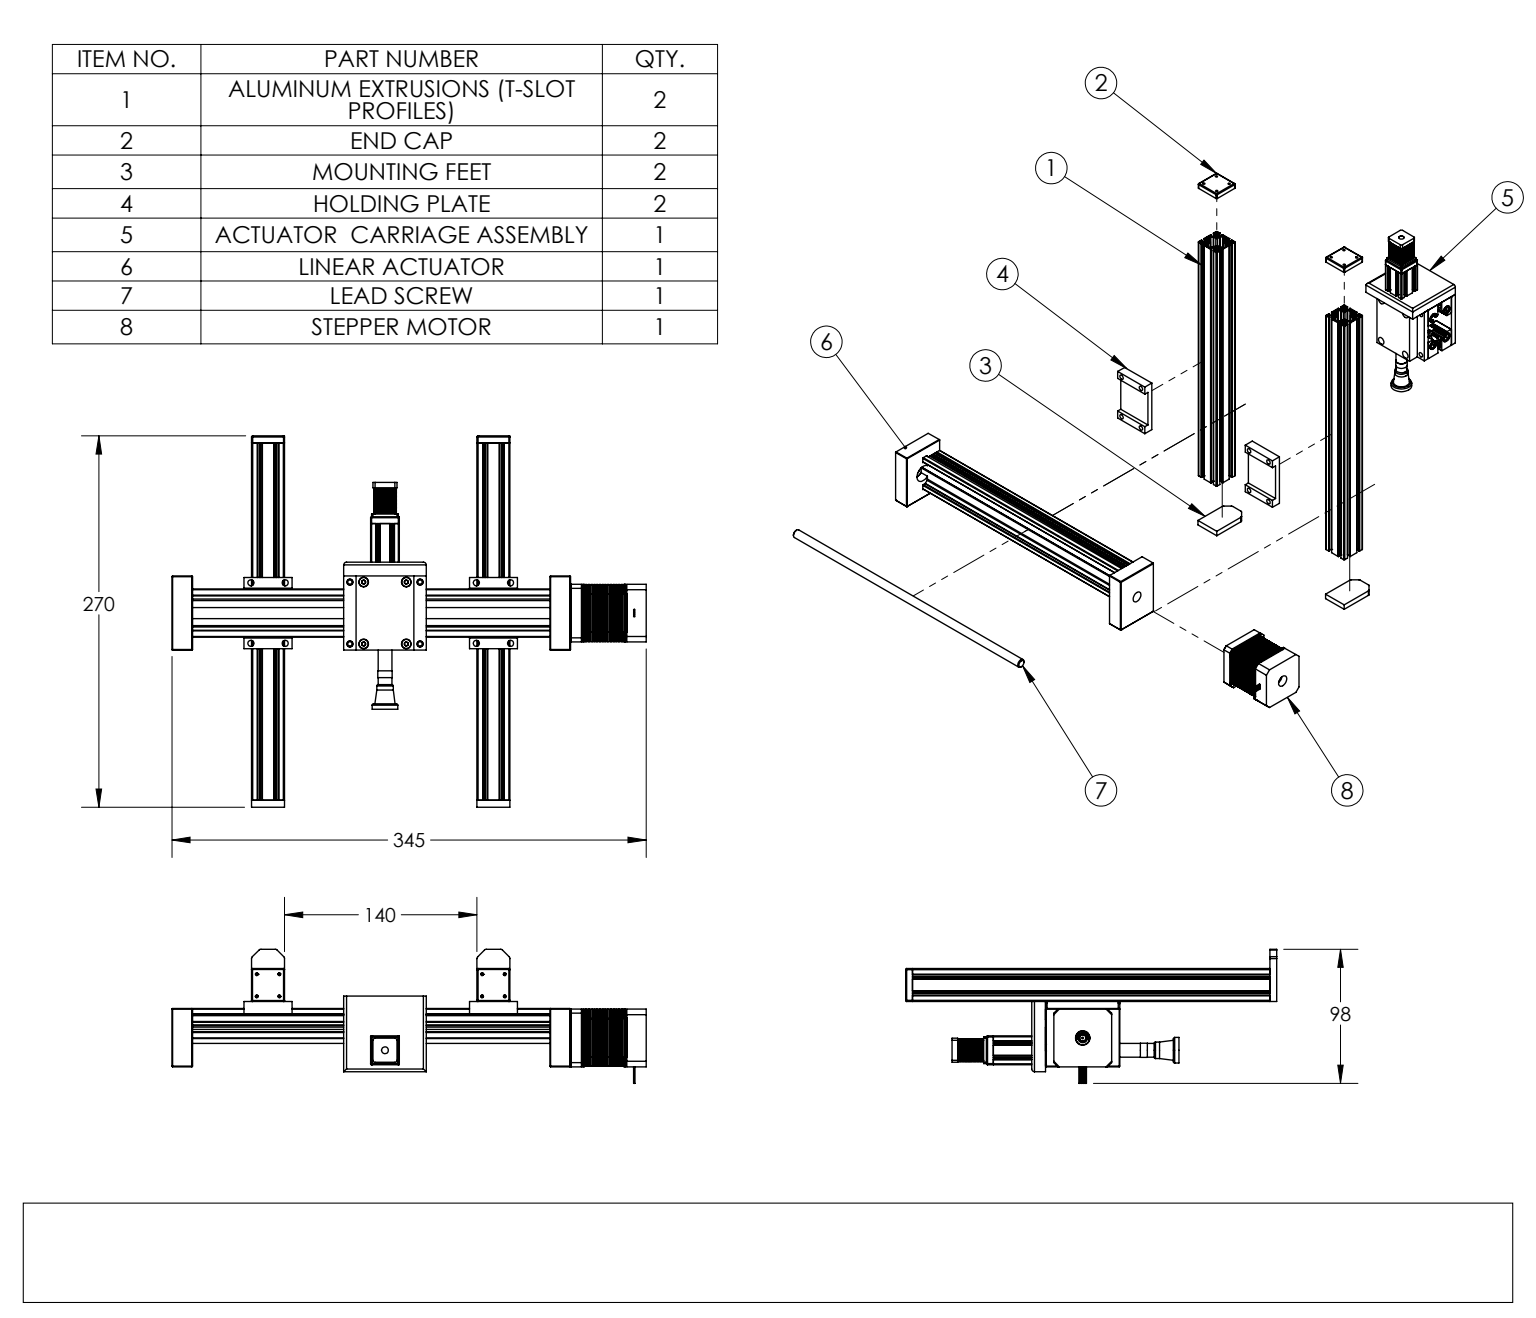
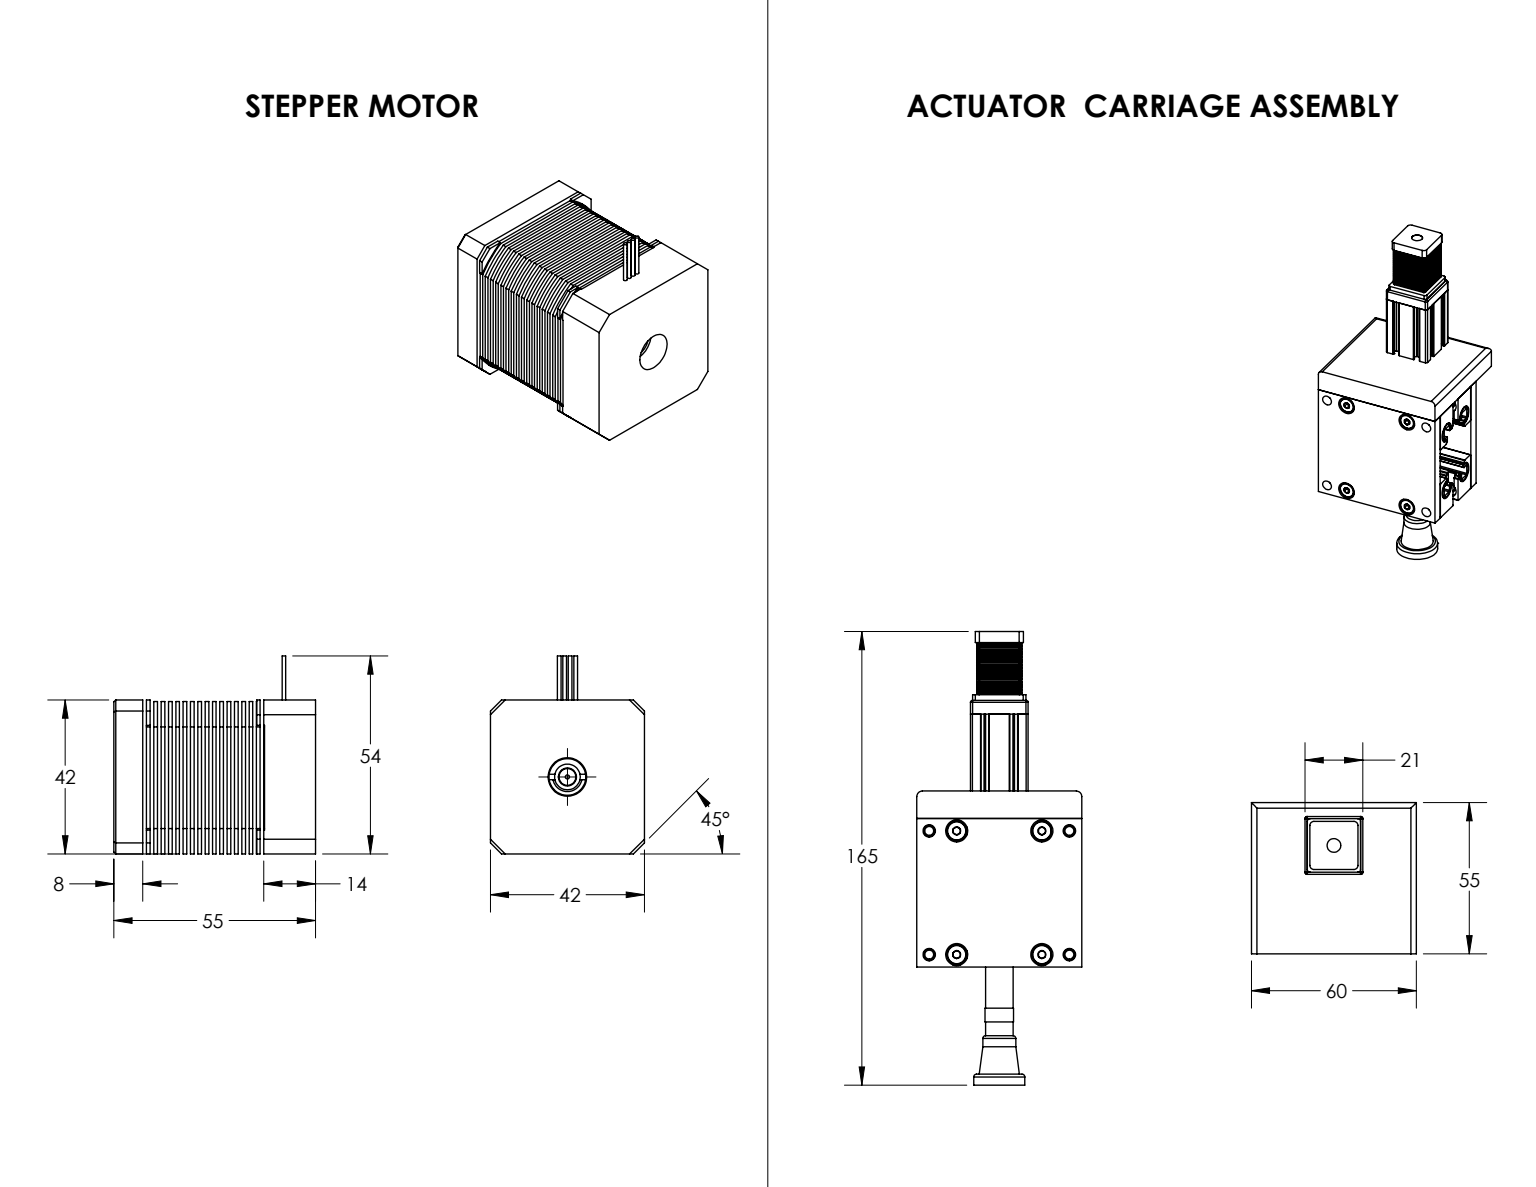
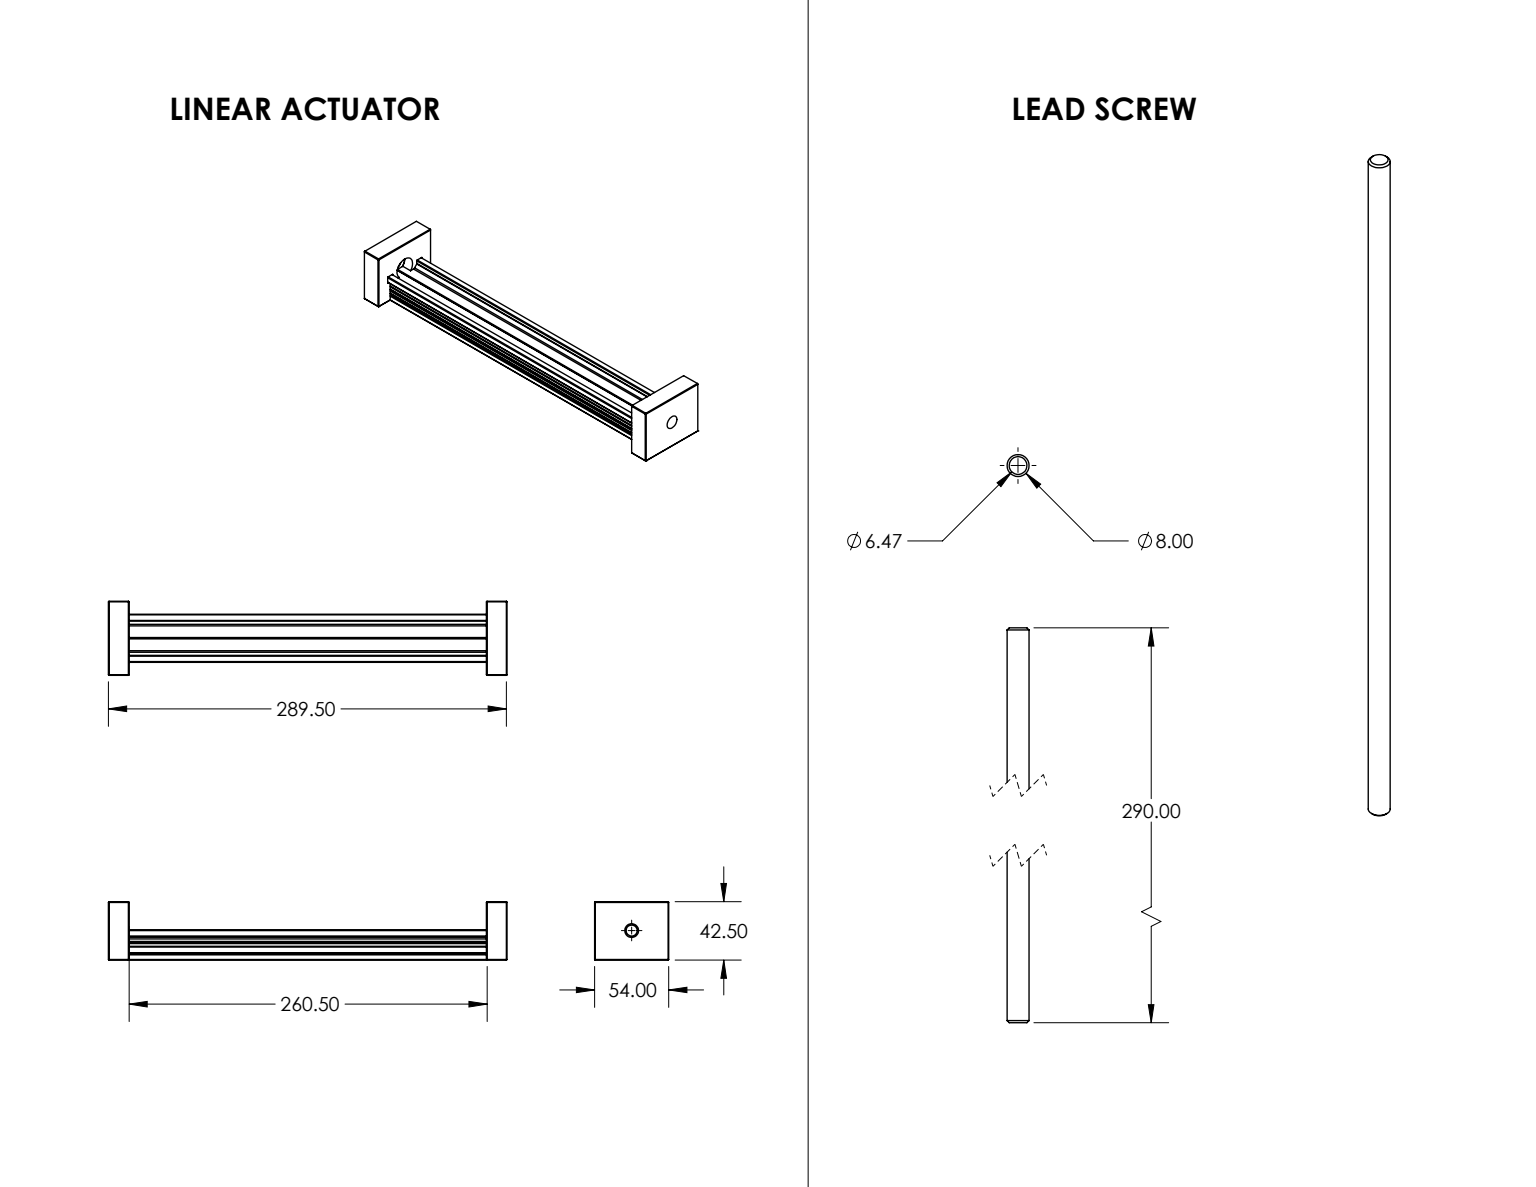
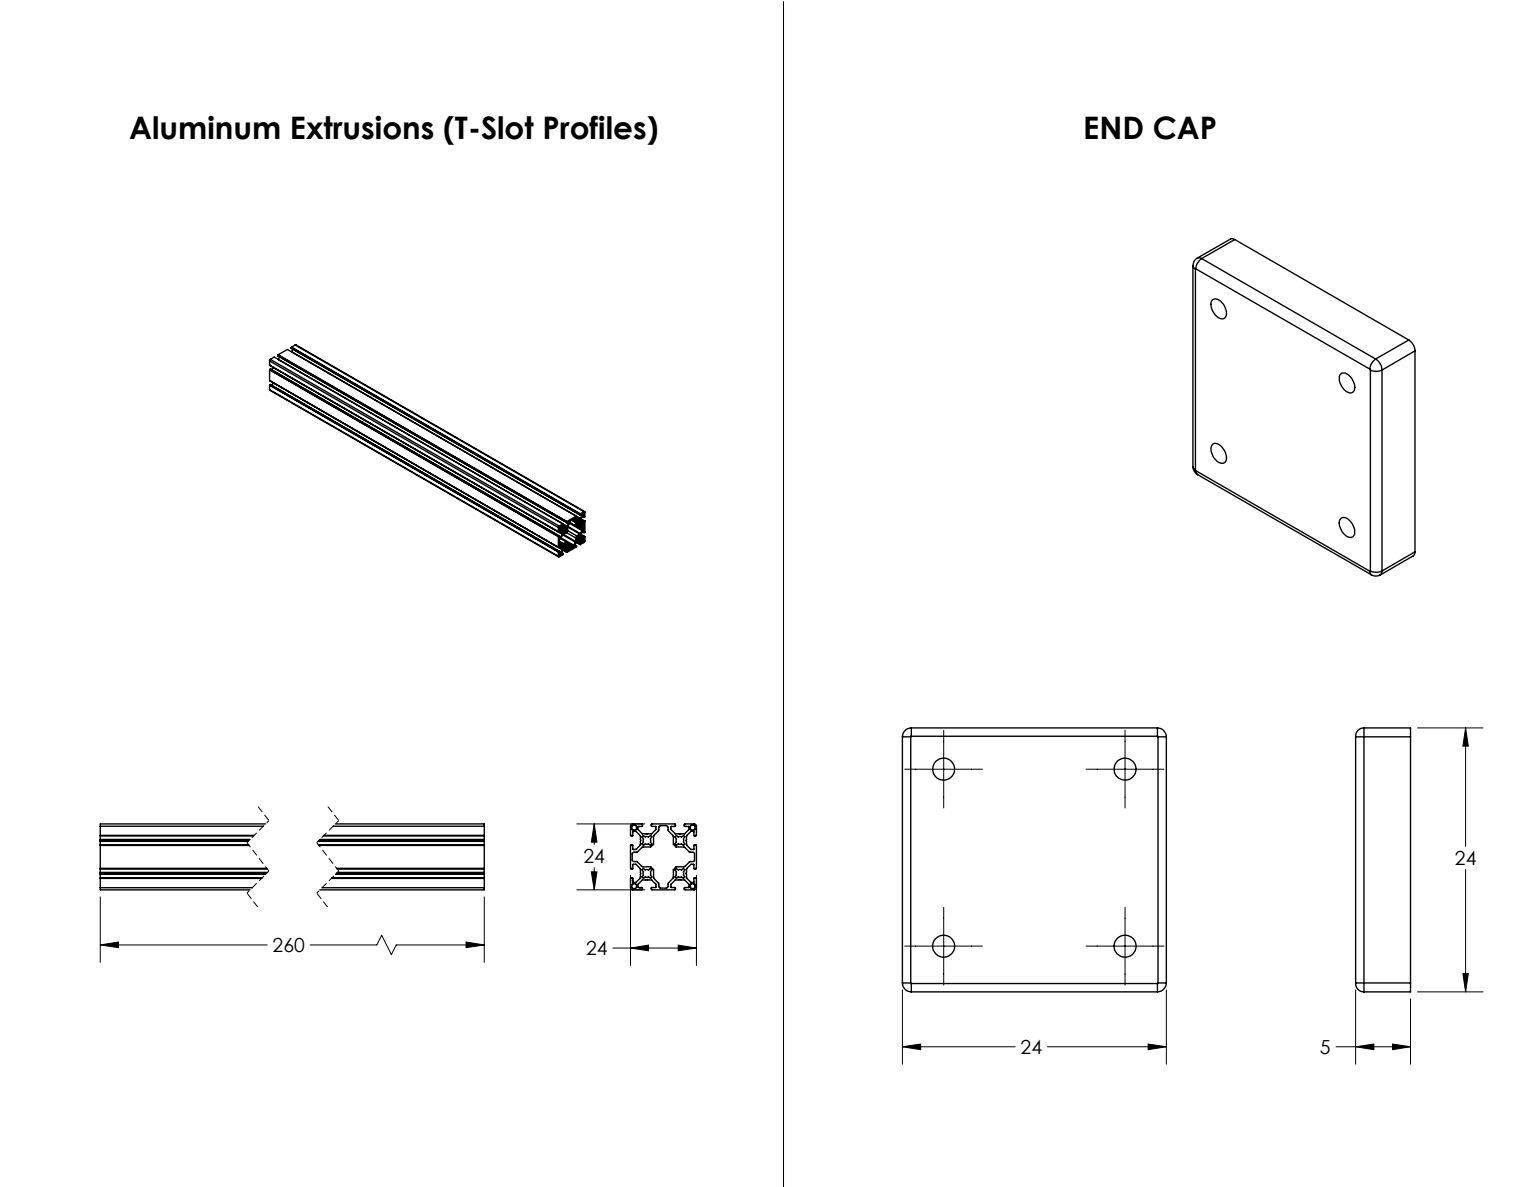
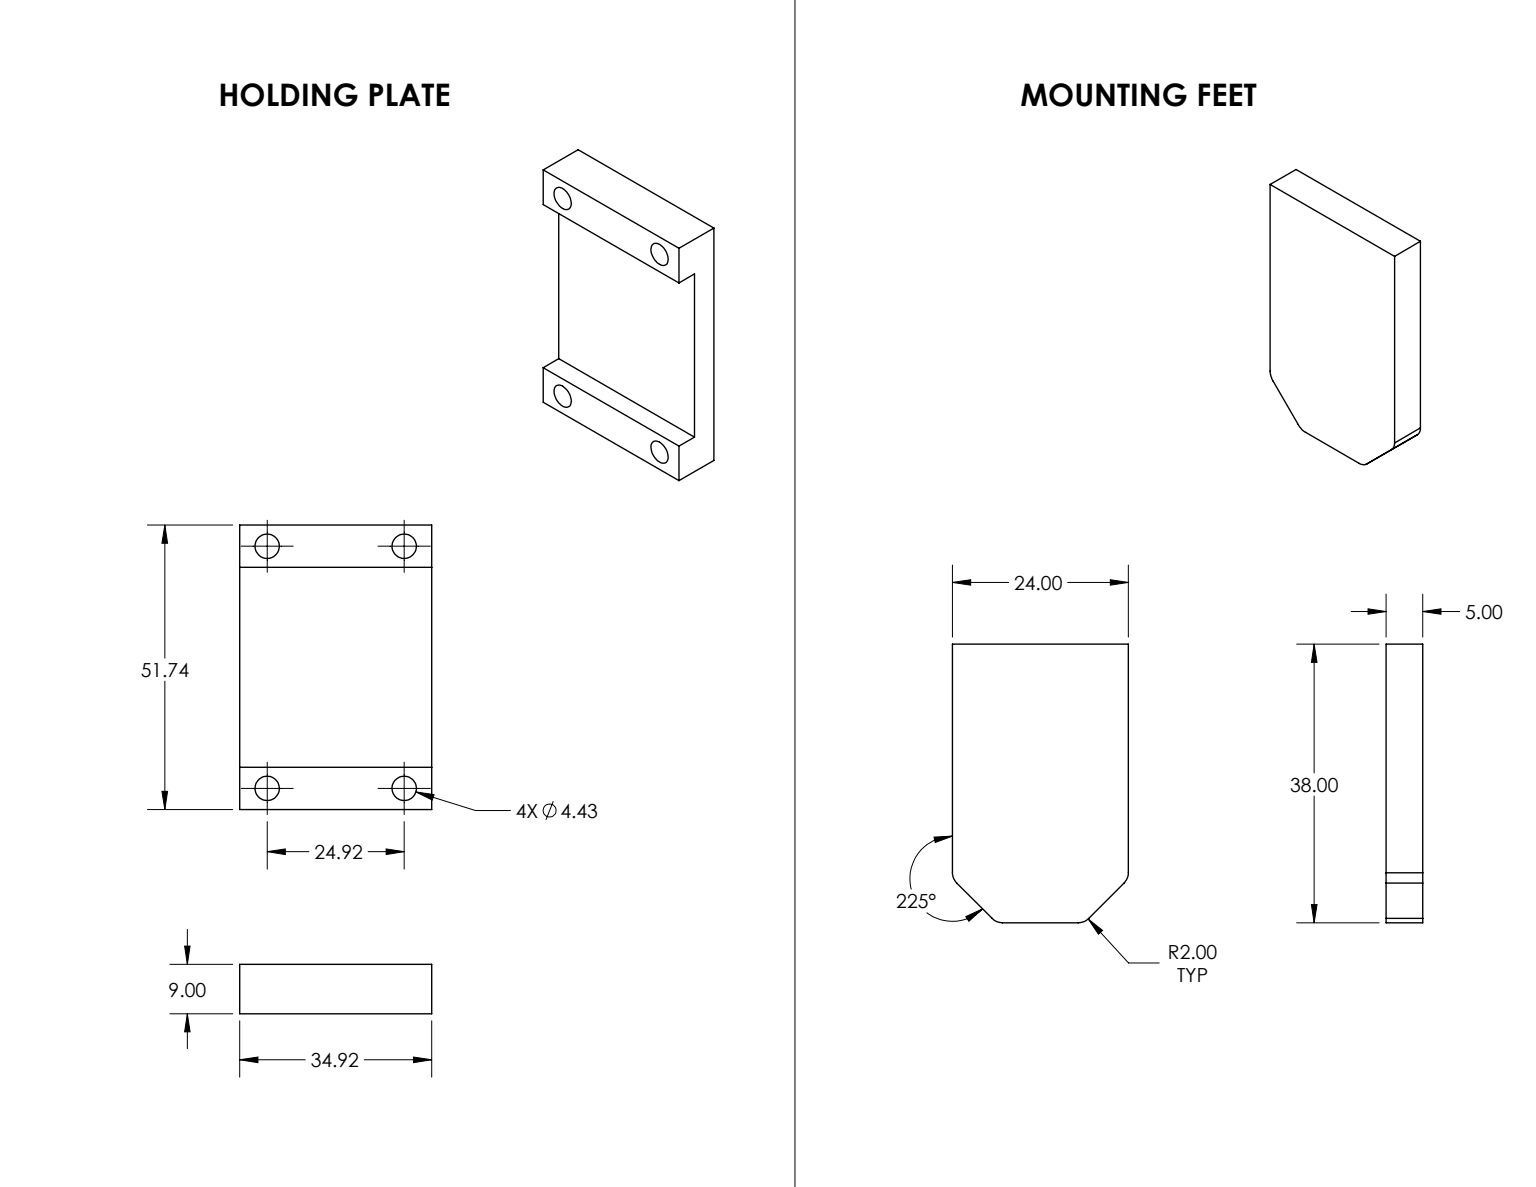
ISO-10303-21;
HEADER;
FILE_DESCRIPTION (('STEP AP214'),
    '1' );
FILE_NAME ('BR-Y-111',
    '2026-10-09T16:01:55',
    ( '' ),
    ( '' ),
    'SwSTEP 2.0',
    'SolidWorks 2024',
    '' );
FILE_SCHEMA (( 'AUTOMOTIVE_DESIGN' ));
ENDSEC;

DATA;
#1 = DIRECTION ( 'NONE',  ( 1.836970198721029934E-16, 1.836970198721010706E-16, -1.000000000000000000 ) ) ;
#3 = PLANE ( 'NONE',  #28714 ) ;
#2 = AXIS2_PLACEMENT_3D ( 'NONE', #65024, #57963, #9532 ) ;
#4 = ORIENTED_EDGE ( 'NONE', *, *, #679, .F. ) ;
#5 = CIRCLE ( 'NONE', #64414, 24.99999999998794920 ) ;
#6 = DIRECTION ( 'NONE',  ( -1.000000000000000000, 0.000000000000000000, 0.000000000000000000 ) ) ;
#8 = LINE ( 'NONE', #43125, #47900 ) ;
#7 = DIRECTION ( 'NONE',  ( 0.7071067811865422437, -0.7071067811865527908, 0.000000000000000000 ) ) ;
#9 = ORIENTED_EDGE ( 'NONE', *, *, #69803, .T. ) ;
#10 = VERTEX_POINT ( 'NONE', #4255 ) ;
#12 = VERTEX_POINT ( 'NONE', #25817 ) ;
#11 = LINE ( 'NONE', #65402, #38696 ) ;
#13 = ORIENTED_EDGE ( 'NONE', *, *, #42356, .F. ) ;
#14 = AXIS2_PLACEMENT_3D ( 'NONE', #25100, #35689, #34989 ) ;
#15 = ADVANCED_FACE ( 'NONE', ( #41711 ), #19784, .T. ) ;
#17 = AXIS2_PLACEMENT_3D ( 'NONE', #56008, #906, #7566 ) ;
#16 = FACE_OUTER_BOUND ( 'NONE', #57290, .T. ) ;
#18 = CIRCLE ( 'NONE', #40620, 8.300000000000002487 ) ;
#19 = ADVANCED_FACE ( 'NONE', ( #47367 ), #45971, .F. ) ;
#20 = CARTESIAN_POINT ( 'NONE',  ( 7.000000000000000000, -26.50000000000000000, 9.080000000000000071 ) ) ;
#21 = ORIENTED_EDGE ( 'NONE', *, *, #32727, .F. ) ;
#22 = EDGE_CURVE ( 'NONE', #35164, #51205, #22753, .T. ) ;
#23 = AXIS2_PLACEMENT_3D ( 'NONE', #22038, #43598, #28713 ) ;
#24 = VECTOR ( 'NONE', #20692, 1000.000000000000000 ) ;
#25 = FACE_OUTER_BOUND ( 'NONE', #67171, .T. ) ;
#26 = EDGE_CURVE ( 'NONE', #33489, #6963, #35337, .T. ) ;
#27 = DIRECTION ( 'NONE',  ( -1.000000000000000000, 1.794541526872559352E-16, 0.000000000000000000 ) ) ;
#28 = VERTEX_POINT ( 'NONE', #47018 ) ;
#29 = ORIENTED_EDGE ( 'NONE', *, *, #35649, .T. ) ;
#30 = PLANE ( 'NONE',  #1467 ) ;
#31 = LINE ( 'NONE', #62705, #60565 ) ;
#32 = ADVANCED_FACE ( 'NONE', ( #68598 ), #51631, .F. ) ;
#33 = CARTESIAN_POINT ( 'NONE',  ( 32.89999999999999858, -21.00000000000001421, -13.86939075806900945 ) ) ;
#34 = ORIENTED_EDGE ( 'NONE', *, *, #62391, .F. ) ;
#35 = SHAPE_REPRESENTATION ( 'Aluminum Extrusions (T-Slot Profiles)_5537T808', ( #45918 ), #47199 ) ;
#36 = CARTESIAN_POINT ( 'NONE',  ( -11.99351654964679526, -7.826483450353362237, 455.0000000000000568 ) ) ;
#37 = FACE_OUTER_BOUND ( 'NONE', #4535, .T. ) ;
#39 = ORIENTED_EDGE ( 'NONE', *, *, #40166, .F. ) ;
#38 = CARTESIAN_POINT ( 'NONE',  ( 4.201500623656003519, -4.740315990920191069, 195.0000000000000284 ) ) ;
#41 = ORIENTED_EDGE ( 'NONE', *, *, #17643, .F. ) ;
#40 = CARTESIAN_POINT ( 'NONE',  ( -12.00000000000000000, -11.18999999999999950, -4.250000000000000000 ) ) ;
#42 = EDGE_CURVE ( 'NONE', #51075, #15946, #66798, .T. ) ;
#43 = FACE_OUTER_BOUND ( 'NONE', #36731, .T. ) ;
#44 = DIRECTION ( 'NONE',  ( -1.000000000000000000, 0.000000000000000000, 0.000000000000000000 ) ) ;
#45 = CARTESIAN_POINT ( 'NONE',  ( 6.006483450353353959, 5.993516549646629166, 195.0000000000000284 ) ) ;
#46 = LINE ( 'NONE', #38894, #69673 ) ;
#47 = ADVANCED_FACE ( 'NONE', ( #64337 ), #37812, .F. ) ;
#48 = CARTESIAN_POINT ( 'NONE',  ( 11.08848345035334404, -11.08848345035339733, 195.0000000000000284 ) ) ;
#49 = FACE_OUTER_BOUND ( 'NONE', #48947, .T. ) ;
#50 = VERTEX_POINT ( 'NONE', #59375 ) ;
#51 = DIRECTION ( 'NONE',  ( 1.000000000000000000, 0.000000000000000000, 0.000000000000000000 ) ) ;
#52 = VECTOR ( 'NONE', #54469, 1000.000000000000000 ) ;
#54 = ORIENTED_EDGE ( 'NONE', *, *, #29068, .T. ) ;
#53 = DIRECTION ( 'NONE',  ( 0.000000000000000000, -1.000000000000000000, 0.000000000000000000 ) ) ;
#56 = ORIENTED_EDGE ( 'NONE', *, *, #20714, .T. ) ;
#55 = LINE ( 'NONE', #58414, #51365 ) ;
#57 = CIRCLE ( 'NONE', #62089, 0.3999999999999993006 ) ;
#58 = DIRECTION ( 'NONE',  ( 0.000000000000000000, 0.7096009616570518874, -0.7046037717862339012 ) ) ;
#59 = DIRECTION ( 'NONE',  ( -0.000000000000000000, -0.000000000000000000, -1.000000000000000000 ) ) ;
#60 = VECTOR ( 'NONE', #58581, 1000.000000000000000 ) ;
#61 = ORIENTED_EDGE ( 'NONE', *, *, #49040, .T. ) ;
#62 = CARTESIAN_POINT ( 'NONE',  ( 30.00000000000000000, -14.04000000000000092, 17.04524521594300523 ) ) ;
#63 = CARTESIAN_POINT ( 'NONE',  ( -7.605476262117258024, 9.722976262117178692, 54.00000000000000711 ) ) ;
#64 = VERTEX_POINT ( 'NONE', #42415 ) ;
#65 = VECTOR ( 'NONE', #47625, 1000.000000000000114 ) ;
#66 = DIRECTION ( 'NONE',  ( -1.000000000000000000, 0.000000000000000000, 0.000000000000000000 ) ) ;
#67 = DIRECTION ( 'NONE',  ( 2.478176394252584099E-15, 1.000000000000000000, 0.000000000000000000 ) ) ;
#68 =( LENGTH_UNIT ( ) NAMED_UNIT ( * ) SI_UNIT ( .MILLI., .METRE. ) );
#69 = AXIS2_PLACEMENT_3D ( 'NONE', #9677, #37599, #64471 ) ;
#70 = EDGE_CURVE ( 'NONE', #46124, #11076, #48766, .T. ) ;
#71 = ADVANCED_FACE ( 'NONE', ( #55074 ), #31476, .T. ) ;
#72 = ORIENTED_EDGE ( 'NONE', *, *, #39303, .F. ) ;
#73 = DIRECTION ( 'NONE',  ( 0.000000000000000000, 0.000000000000000000, 1.000000000000000000 ) ) ;
#74 = ORIENTED_EDGE ( 'NONE', *, *, #13941, .F. ) ;
#75 = ORIENTED_EDGE ( 'NONE', *, *, #18728, .F. ) ;
#76 = CARTESIAN_POINT ( 'NONE',  ( 11.00000000000000000, -17.14999999999900027, 26.64999999999900027 ) ) ;
#77 = AXIS2_PLACEMENT_3D ( 'NONE', #40976, #13759, #8096 ) ;
#78 = CARTESIAN_POINT ( 'NONE',  ( 11.48848345035341900, 10.19191654964656202, 455.0000000000000568 ) ) ;
#79 = VECTOR ( 'NONE', #901, 1000.000000000000000 ) ;
#80 = PLANE ( 'NONE',  #21958 ) ;
#81 = PLANE ( 'NONE',  #14890 ) ;
#82 = EDGE_LOOP ( 'NONE', ( #52627, #35376, #11266, #26532 ) ) ;
#83 = ORIENTED_EDGE ( 'NONE', *, *, #7597, .F. ) ;
#85 = ORIENTED_EDGE ( 'NONE', *, *, #57080, .T. ) ;
#84 = CARTESIAN_POINT ( 'NONE',  ( 30.00000000000000000, -5.599999999999999645, -9.400000000000000355 ) ) ;
#86 = VERTEX_POINT ( 'NONE', #37468 ) ;
#87 = DIRECTION ( 'NONE',  ( 0.000000000000000000, -3.673940397442059868E-16, 1.000000000000000000 ) ) ;
#88 = PLANE ( 'NONE',  #65914 ) ;
#89 = CARTESIAN_POINT ( 'NONE',  ( 6.006483450353353959, 5.993516549646629166, 195.0000000000000284 ) ) ;
#90 = LINE ( 'NONE', #39288, #28849 ) ;
#92 = FACE_OUTER_BOUND ( 'NONE', #31226, .T. ) ;
#91 = DIRECTION ( 'NONE',  ( 0.000000000000000000, -0.9938079899998859545, 0.1111111111112941946 ) ) ;
#93 = ORIENTED_EDGE ( 'NONE', *, *, #1630, .F. ) ;
#95 = ORIENTED_EDGE ( 'NONE', *, *, #37069, .T. ) ;
#94 = LINE ( 'NONE', #53844, #47687 ) ;
#96 = VERTEX_POINT ( 'NONE', #36776 ) ;
#97 = VERTEX_POINT ( 'NONE', #64001 ) ;
#98 = CARTESIAN_POINT ( 'NONE',  ( 275.0000000000000000, -0.5000000000000000000, -26.50000000000000000 ) ) ;
#99 = LINE ( 'NONE', #17046, #62617 ) ;
#100 = AXIS2_PLACEMENT_3D ( 'NONE', #13229, #2981, #46110 ) ;
#101 = DIRECTION ( 'NONE',  ( 1.000000000000000000, 0.000000000000000000, 0.000000000000000000 ) ) ;
#102 = EDGE_CURVE ( 'NONE', #33046, #57965, #58906, .T. ) ;
#103 = CARTESIAN_POINT ( 'NONE',  ( 0.000000000000000000, -8.249999999999998224, -13.50000000000000178 ) ) ;
#104 = EDGE_LOOP ( 'NONE', ( #32156, #26137, #19889, #8846 ) ) ;
#105 = ORIENTED_EDGE ( 'NONE', *, *, #55339, .T. ) ;
#106 = ORIENTED_EDGE ( 'NONE', *, *, #31966, .F. ) ;
#108 = ADVANCED_FACE ( 'NONE', ( #69649 ), #9907, .T. ) ;
#107 = VECTOR ( 'NONE', #53809, 1000.000000000000000 ) ;
#109 = CARTESIAN_POINT ( 'NONE',  ( 11.00000000000000000, -17.00000000000000000, 15.70499999999969809 ) ) ;
#110 = CARTESIAN_POINT ( 'NONE',  ( 14.89999999999999680, 13.66939075806899240, -20.79999999999999361 ) ) ;
#111 = EDGE_CURVE ( 'NONE', #61998, #6695, #11268, .T. ) ;
#112 = CARTESIAN_POINT ( 'NONE',  ( 8.249999999999996447, -7.848062532927998269, 0.000000000000000000 ) ) ;
#113 = EDGE_CURVE ( 'NONE', #43177, #7725, #15895, .T. ) ;
#114 = VERTEX_POINT ( 'NONE', #53041 ) ;
#115 = CIRCLE ( 'NONE', #62160, 1.620999999999997332 ) ;
#116 = VECTOR ( 'NONE', #2061, 1000.000000000000000 ) ;
#117 = ORIENTED_EDGE ( 'NONE', *, *, #12680, .F. ) ;
#118 = DIRECTION ( 'NONE',  ( -1.836970198721029934E-16, 1.836970198721036344E-16, -1.000000000000000000 ) ) ;
#119 = ADVANCED_FACE ( 'NONE', ( #37125 ), #15567, .T. ) ;
#120 = EDGE_CURVE ( 'NONE', #5167, #67654, #58950, .T. ) ;
#121 = FACE_OUTER_BOUND ( 'NONE', #43409, .T. ) ;
#122 = VERTEX_POINT ( 'NONE', #47717 ) ;
#123 = AXIS2_PLACEMENT_3D ( 'NONE', #35895, #68773, #47212 ) ;
#124 = EDGE_CURVE ( 'NONE', #2059, #46953, #44248, .T. ) ;
#125 = CARTESIAN_POINT ( 'NONE',  ( -11.00000000000000000, -9.200000000000120082, 17.64999999999993108 ) ) ;
#127 = VERTEX_POINT ( 'NONE', #32847 ) ;
#126 = LINE ( 'NONE', #53521, #21596 ) ;
#128 = ORIENTED_EDGE ( 'NONE', *, *, #65488, .T. ) ;
#130 = CARTESIAN_POINT ( 'NONE',  ( -7.793516549646827940, -11.12648345035340647, 455.0000000000000568 ) ) ;
#129 = AXIS2_PLACEMENT_3D ( 'NONE', #11576, #55092, #50108 ) ;
#131 = DIRECTION ( 'NONE',  ( 0.8660254037844482555, 0.000000000000000000, -0.4999999999999831801 ) ) ;
#132 = DIRECTION ( 'NONE',  ( 0.000000000000000000, 0.000000000000000000, 1.000000000000000000 ) ) ;
#133 = CARTESIAN_POINT ( 'NONE',  ( 1.480523737882788238, -9.404523737882794165, 54.00000000000000711 ) ) ;
#134 = DIRECTION ( 'NONE',  ( 0.000000000000000000, 0.000000000000000000, 1.000000000000000000 ) ) ;
#135 = VERTEX_POINT ( 'NONE', #54425 ) ;
#136 = DIRECTION ( 'NONE',  ( -1.836970198721029934E-16, 1.836970198721036344E-16, -1.000000000000000000 ) ) ;
#137 = ORIENTED_EDGE ( 'NONE', *, *, #53122, .T. ) ;
#138 = DIRECTION ( 'NONE',  ( 1.000000000000000000, -0.000000000000000000, -0.000000000000000000 ) ) ;
#139 = CARTESIAN_POINT ( 'NONE',  ( 29.50000000000000355, -12.00000000000000000, 10.69999999999999929 ) ) ;
#140 = VECTOR ( 'NONE', #32792, 1000.000000000000000 ) ;
#141 = CARTESIAN_POINT ( 'NONE',  ( 275.0000000000000000, -21.00000000000000000, 12.50000000000000000 ) ) ;
#142 = DIRECTION ( 'NONE',  ( 1.836970198721029934E-16, 1.836970198721010706E-16, -1.000000000000000000 ) ) ;
#143 = DIRECTION ( 'NONE',  ( 1.047444401652939849E-14, 1.000000000000000000, 1.836970198721029934E-16 ) ) ;
#144 = VERTEX_POINT ( 'NONE', #43447 ) ;
#145 = DIRECTION ( 'NONE',  ( 1.000000000000000000, 0.000000000000000000, 0.000000000000000000 ) ) ;
#146 = CIRCLE ( 'NONE', #27251, 2.000000000000001776 ) ;
#147 = DIRECTION ( 'NONE',  ( 1.000000000000000000, 0.000000000000000000, 0.000000000000000000 ) ) ;
#148 = EDGE_CURVE ( 'NONE', #32098, #68514, #65034, .T. ) ;
#149 = VECTOR ( 'NONE', #1157, 1000.000000000000000 ) ;
#150 = EDGE_LOOP ( 'NONE', ( #65077, #13580, #38197, #52160, #31394, #37304, #41041, #48083 ) ) ;
#151 = DIRECTION ( 'NONE',  ( 1.000000000000000000, 0.000000000000000000, 0.000000000000000000 ) ) ;
#152 = CARTESIAN_POINT ( 'NONE',  ( 47.00000000000000000, 0.000000000000000000, 0.000000000000000000 ) ) ;
#153 = ADVANCED_FACE ( 'NONE', ( #5637 ), #10243, .T. ) ;
#154 = AXIS2_PLACEMENT_3D ( 'NONE', #15103, #20746, #47621 ) ;
#155 = ORIENTED_EDGE ( 'NONE', *, *, #10566, .T. ) ;
#156 = EDGE_CURVE ( 'NONE', #48024, #52249, #59027, .T. ) ;
#157 = DIRECTION ( 'NONE',  ( 1.000000000000000000, 0.000000000000000000, 0.000000000000000000 ) ) ;
#158 = CARTESIAN_POINT ( 'NONE',  ( 31.89999999999999858, -0.2000000000089119934, -8.913009219568841313E-12 ) ) ;
#159 = ORIENTED_EDGE ( 'NONE', *, *, #8792, .F. ) ;
#160 = CARTESIAN_POINT ( 'NONE',  ( 12.00648345035338060, -7.826483450353491023, 455.0000000000000568 ) ) ;
#161 = DIRECTION ( 'NONE',  ( -1.000000000000000000, 4.121462285523434458E-16, 1.514200678731842937E-31 ) ) ;
#162 = EDGE_CURVE ( 'NONE', #51028, #19307, #65708, .T. ) ;
#163 = CIRCLE ( 'NONE', #63398, 0.1999999999999987899 ) ;
#164 = VECTOR ( 'NONE', #31402, 1000.000000000000000 ) ;
#165 = LINE ( 'NONE', #32674, #35413 ) ;
#166 = CARTESIAN_POINT ( 'NONE',  ( 275.2500000000000000, -42.25000000000000000, 26.75000000000000000 ) ) ;
#167 = VERTEX_POINT ( 'NONE', #1968 ) ;
#169 = EDGE_LOOP ( 'NONE', ( #39486, #29430, #2363, #22947 ) ) ;
#168 = DIRECTION ( 'NONE',  ( 1.000000000000000000, -0.000000000000000000, 0.000000000000000000 ) ) ;
#170 = AXIS2_PLACEMENT_3D ( 'NONE', #9286, #3635, #67983 ) ;
#171 = CIRCLE ( 'NONE', #58872, 0.4999999999991850963 ) ;
#172 = DIRECTION ( 'NONE',  ( 1.356437060717831815E-15, 1.000000000000000000, 0.000000000000000000 ) ) ;
#173 = CYLINDRICAL_SURFACE ( 'NONE', #39140, 3.499999999999850342 ) ;
#174 = LINE ( 'NONE', #65556, #3686 ) ;
#175 = ORIENTED_EDGE ( 'NONE', *, *, #63248, .F. ) ;
#176 = AXIS2_PLACEMENT_3D ( 'NONE', #44626, #60208, #34021 ) ;
#177 = PLANE ( 'NONE',  #17503 ) ;
#178 = CARTESIAN_POINT ( 'NONE',  ( -7.250000000000000888, 7.250000000000001776, -18.00000000000000000 ) ) ;
#179 = ORIENTED_EDGE ( 'NONE', *, *, #39700, .T. ) ;
#180 = ORIENTED_EDGE ( 'NONE', *, *, #26893, .F. ) ;
#181 = ORIENTED_EDGE ( 'NONE', *, *, #42792, .T. ) ;
#182 = DIRECTION ( 'NONE',  ( -0.000000000000000000, 3.673940397442059868E-16, -1.000000000000000000 ) ) ;
#183 = CARTESIAN_POINT ( 'NONE',  ( 11.50000000000000000, -11.50000000000100009, -10.50000000000065903 ) ) ;
#184 =( LENGTH_UNIT ( ) NAMED_UNIT ( * ) SI_UNIT ( .MILLI., .METRE. ) );
#185 = EDGE_CURVE ( 'NONE', #36958, #12401, #20004, .T. ) ;
#186 = ORIENTED_EDGE ( 'NONE', *, *, #14388, .F. ) ;
#187 = VERTEX_POINT ( 'NONE', #23532 ) ;
#188 = ORIENTED_EDGE ( 'NONE', *, *, #41288, .T. ) ;
#189 = DIRECTION ( 'NONE',  ( -1.813998472013049506E-14, -1.000000000000000000, -1.836970198721043986E-16 ) ) ;
#190 = VERTEX_POINT ( 'NONE', #61701 ) ;
#191 = VERTEX_POINT ( 'NONE', #61342 ) ;
#192 = ORIENTED_EDGE ( 'NONE', *, *, #64535, .T. ) ;
#193 = ORIENTED_EDGE ( 'NONE', *, *, #5564, .T. ) ;
#194 = DIRECTION ( 'NONE',  ( 1.000000000000000000, 0.000000000000000000, 0.000000000000000000 ) ) ;
#195 = EDGE_CURVE ( 'NONE', #57192, #24019, #50407, .T. ) ;
#196 = EDGE_CURVE ( 'NONE', #13160, #36733, #7955, .T. ) ;
#197 = CIRCLE ( 'NONE', #57770, 2.204799999999999205 ) ;
#199 = ORIENTED_EDGE ( 'NONE', *, *, #12386, .F. ) ;
#198 = DIRECTION ( 'NONE',  ( 1.000000000000000000, 0.000000000000000000, 0.000000000000000000 ) ) ;
#200 = CARTESIAN_POINT ( 'NONE',  ( 7.000000000000000000, -42.00000000000000000, -7.000000000000000000 ) ) ;
#201 = AXIS2_PLACEMENT_3D ( 'NONE', #59073, #10628, #38219 ) ;
#202 = DIRECTION ( 'NONE',  ( -0.7071067811865480168, -0.7071067811865470176, 0.000000000000000000 ) ) ;
#203 = EDGE_CURVE ( 'NONE', #26279, #24611, #49905, .T. ) ;
#204 = CARTESIAN_POINT ( 'NONE',  ( 7.000000000000000000, -26.50000000000000000, -0.5000000000000000000 ) ) ;
#205 = ORIENTED_EDGE ( 'NONE', *, *, #6943, .T. ) ;
#206 = VECTOR ( 'NONE', #26081, 1000.000000000000000 ) ;
#207 = AXIS2_PLACEMENT_3D ( 'NONE', #51978, #16234, #48423 ) ;
#208 = DIRECTION ( 'NONE',  ( -1.000000000000000000, 3.491481338843133355E-15, 1.836970198721036344E-16 ) ) ;
#209 = CARTESIAN_POINT ( 'NONE',  ( -7.450000000000001954, 0.000000000000000000, -18.00000000000000000 ) ) ;
#210 = ORIENTED_EDGE ( 'NONE', *, *, #15362, .F. ) ;
#211 = AXIS2_PLACEMENT_3D ( 'NONE', #34304, #7442, #6750 ) ;
#212 = DIRECTION ( 'NONE',  ( 0.000000000000000000, -0.1249999999999996531, -0.9921567416492215186 ) ) ;
#213 = CARTESIAN_POINT ( 'NONE',  ( 32.89999999999999858, 20.60000000000000142, 13.86939075806900057 ) ) ;
#214 = LINE ( 'NONE', #16474, #66351 ) ;
#215 = ORIENTED_EDGE ( 'NONE', *, *, #61304, .T. ) ;
#216 = DIRECTION ( 'NONE',  ( 0.000000000000000000, -0.7071067811865474617, -0.7071067811865474617 ) ) ;
#217 = DIRECTION ( 'NONE',  ( -1.047444401652940164E-14, -1.000000000000000000, -1.836970198721030181E-16 ) ) ;
#218 = DIRECTION ( 'NONE',  ( 0.000000000000000000, 0.000000000000000000, 1.000000000000000000 ) ) ;
#219 = DIRECTION ( 'NONE',  ( 0.000000000000000000, 0.000000000000000000, -1.000000000000000000 ) ) ;
#220 = PLANE ( 'NONE',  #66350 ) ;
#221 = LINE ( 'NONE', #21784, #62152 ) ;
#222 = DIRECTION ( 'NONE',  ( -0.000000000000000000, -0.000000000000000000, -1.000000000000000000 ) ) ;
#223 = PLANE ( 'NONE',  #58243 ) ;
#224 = ORIENTED_EDGE ( 'NONE', *, *, #41153, .T. ) ;
#225 = CARTESIAN_POINT ( 'NONE',  ( -29.50000000000000355, -15.46862696659690073, 14.50000000000000000 ) ) ;
#226 = LINE ( 'NONE', #22825, #12692 ) ;
#227 = EDGE_CURVE ( 'NONE', #15964, #12532, #53311, .T. ) ;
#228 = ADVANCED_FACE ( 'NONE', ( #56750 ), #13963, .T. ) ;
#229 = EDGE_CURVE ( 'NONE', #49648, #8082, #14853, .T. ) ;
#230 = DIRECTION ( 'NONE',  ( 0.000000000000000000, 0.000000000000000000, -1.000000000000000000 ) ) ;
#231 = CARTESIAN_POINT ( 'NONE',  ( 0.000000000000000000, -42.00000000000000000, 26.50000000000000000 ) ) ;
#232 = ORIENTED_EDGE ( 'NONE', *, *, #38318, .F. ) ;
#233 = CARTESIAN_POINT ( 'NONE',  ( 30.00000000000000000, -5.599999999999999645, 9.400000000000000355 ) ) ;
#234 = DIRECTION ( 'NONE',  ( -1.000000000000000000, 0.000000000000000000, 0.000000000000000000 ) ) ;
#235 = AXIS2_PLACEMENT_3D ( 'NONE', #32460, #32097, #54031 ) ;
#236 = LINE ( 'NONE', #68848, #62717 ) ;
#237 = ADVANCED_FACE ( 'NONE', ( #40838 ), #18219, .F. ) ;
#238 = CARTESIAN_POINT ( 'NONE',  ( -11.00000000000000000, -9.199999999999999289, -12.34999999999989839 ) ) ;
#239 = LINE ( 'NONE', #1275, #59908 ) ;
#240 = VECTOR ( 'NONE', #33249, 1000.000000000000000 ) ;
#241 = ORIENTED_EDGE ( 'NONE', *, *, #54639, .T. ) ;
#242 = ORIENTED_EDGE ( 'NONE', *, *, #68755, .F. ) ;
#243 = FACE_OUTER_BOUND ( 'NONE', #8510, .T. ) ;
#244 = CARTESIAN_POINT ( 'NONE',  ( 7.450000000000004619, -1.336933437520057563E-15, -23.00000000000000000 ) ) ;
#245 = VERTEX_POINT ( 'NONE', #54763 ) ;
#246 = CARTESIAN_POINT ( 'NONE',  ( 7.250000000000005329, -8.249999999999998224, -20.00000000000000000 ) ) ;
#247 = DIRECTION ( 'NONE',  ( 0.000000000000000000, 0.000000000000000000, -1.000000000000000000 ) ) ;
#248 = ORIENTED_EDGE ( 'NONE', *, *, #20850, .F. ) ;
#249 = AXIS2_PLACEMENT_3D ( 'NONE', #24240, #50751, #62765 ) ;
#250 = ADVANCED_FACE ( 'NONE', ( #56401 ), #28821, .T. ) ;
#251 = CARTESIAN_POINT ( 'NONE',  ( -11.00000000000000000, -11.50000000000000000, -11.00000000000000000 ) ) ;
#252 = ORIENTED_EDGE ( 'NONE', *, *, #3134, .T. ) ;
#253 = ORIENTED_EDGE ( 'NONE', *, *, #15197, .T. ) ;
#254 = CARTESIAN_POINT ( 'NONE',  ( -6.775514141871385121, 7.394232575409538377, 26.00000000000000711 ) ) ;
#255 = ORIENTED_EDGE ( 'NONE', *, *, #43723, .F. ) ;
#256 = CIRCLE ( 'NONE', #3484, 0.3499999999999996447 ) ;
#257 = DIRECTION ( 'NONE',  ( -1.836970198721029934E-16, 1.836970198721036590E-16, -1.000000000000000000 ) ) ;
#258 = DIRECTION ( 'NONE',  ( 0.000000000000000000, 0.000000000000000000, -1.000000000000000000 ) ) ;
#259 = DIRECTION ( 'NONE',  ( -0.000000000000000000, -0.7071067811865474617, 0.7071067811865474617 ) ) ;
#260 = VECTOR ( 'NONE', #28913, 1000.000000000000000 ) ;
#261 = ORIENTED_EDGE ( 'NONE', *, *, #56801, .T. ) ;
#262 = ORIENTED_EDGE ( 'NONE', *, *, #61325, .F. ) ;
#263 = DIRECTION ( 'NONE',  ( 0.000000000000000000, 0.000000000000000000, -1.000000000000000000 ) ) ;
#265 = DIRECTION ( 'NONE',  ( -1.000000000000000000, 0.000000000000000000, 0.000000000000000000 ) ) ;
#264 = CARTESIAN_POINT ( 'NONE',  ( 8.711985858128686644, 8.079219948824833963, 54.00000000000000711 ) ) ;
#266 = ORIENTED_EDGE ( 'NONE', *, *, #48155, .T. ) ;
#267 = EDGE_LOOP ( 'NONE', ( #46441, #3343, #16944, #35181, #20767, #32717, #56095, #39421 ) ) ;
#268 = VERTEX_POINT ( 'NONE', #57103 ) ;
#269 = LINE ( 'NONE', #54368, #39000 ) ;
#271 = EDGE_LOOP ( 'NONE', ( #35321, #22155, #8372, #56356 ) ) ;
#270 = FACE_OUTER_BOUND ( 'NONE', #3892, .T. ) ;
#272 = ADVANCED_FACE ( 'NONE', ( #34467 ), #50744, .F. ) ;
#273 = FACE_OUTER_BOUND ( 'NONE', #58305, .T. ) ;
#274 = CARTESIAN_POINT ( 'NONE',  ( -8.593516549646745162, -4.396432944014545541, 455.0000000000000568 ) ) ;
#275 = EDGE_CURVE ( 'NONE', #16443, #31143, #40125, .T. ) ;
#276 = ORIENTED_EDGE ( 'NONE', *, *, #51497, .T. ) ;
#277 = ADVANCED_FACE ( 'NONE', ( #51453 ), #24234, .T. ) ;
#278 = VERTEX_POINT ( 'NONE', #3022 ) ;
#279 = FACE_OUTER_BOUND ( 'NONE', #56428, .T. ) ;
#280 = ADVANCED_FACE ( 'NONE', ( #45792 ), #62049, .F. ) ;
#281 = ORIENTED_EDGE ( 'NONE', *, *, #951, .F. ) ;
#282 = EDGE_CURVE ( 'NONE', #46458, #1557, #680, .T. ) ;
#283 = CARTESIAN_POINT ( 'NONE',  ( -8.000000000000000000, 8.000000000000000000, -1.000000000000000000 ) ) ;
#284 = CARTESIAN_POINT ( 'NONE',  ( -11.33351654964671162, 1.077516549646603483, 455.0000000000000568 ) ) ;
#285 = EDGE_CURVE ( 'NONE', #49229, #23467, #8668, .T. ) ;
#286 = EDGE_CURVE ( 'NONE', #67917, #37432, #33951, .T. ) ;
#287 = VECTOR ( 'NONE', #16206, 1000.000000000000000 ) ;
#288 = VERTEX_POINT ( 'NONE', #14671 ) ;
#289 = EDGE_CURVE ( 'NONE', #31751, #6775, #9008, .T. ) ;
#290 = DIRECTION ( 'NONE',  ( 1.000000000000000000, -0.000000000000000000, 0.000000000000000000 ) ) ;
#291 = CARTESIAN_POINT ( 'NONE',  ( -9.722976262117237312, 7.605476262117214503, 54.00000000000000711 ) ) ;
#293 = ORIENTED_EDGE ( 'NONE', *, *, #42329, .T. ) ;
#292 = FACE_OUTER_BOUND ( 'NONE', #58833, .T. ) ;
#294 = ORIENTED_EDGE ( 'NONE', *, *, #44456, .F. ) ;
#295 = AXIS2_PLACEMENT_3D ( 'NONE', #54190, #47225, #5411 ) ;
#296 = DIRECTION ( 'NONE',  ( 1.000000000000000000, -0.000000000000000000, 0.000000000000000000 ) ) ;
#297 = CARTESIAN_POINT ( 'NONE',  ( -6.651770455163783957, -7.532023737882790115, 54.00000000000000711 ) ) ;
#298 = FACE_OUTER_BOUND ( 'NONE', #42957, .T. ) ;
#299 = DIRECTION ( 'NONE',  ( 0.000000000000000000, -1.000000000000000000, 0.000000000000000000 ) ) ;
#300 = LINE ( 'NONE', #16908, #68047 ) ;
#301 = ORIENTED_EDGE ( 'NONE', *, *, #36059, .F. ) ;
#302 = LINE ( 'NONE', #38144, #67419 ) ;
#303 = CARTESIAN_POINT ( 'NONE',  ( 0.9555237378828163042, 9.390476262117214645, 54.00000000000000711 ) ) ;
#304 = CARTESIAN_POINT ( 'NONE',  ( 11.18999999999999950, 11.25000000000000178, -5.000000000000000000 ) ) ;
#306 = ORIENTED_EDGE ( 'NONE', *, *, #47365, .T. ) ;
#305 = DIRECTION ( 'NONE',  ( -1.000000000000000000, -0.000000000000000000, -0.000000000000000000 ) ) ;
#307 = CYLINDRICAL_SURFACE ( 'NONE', #50491, 0.5000000000079367624 ) ;
#308 = VECTOR ( 'NONE', #40044, 1000.000000000000000 ) ;
#309 = DIRECTION ( 'NONE',  ( 1.000000000000000000, 0.000000000000000000, 0.000000000000000000 ) ) ;
#310 = CARTESIAN_POINT ( 'NONE',  ( -7.250000000000000888, 8.250000000000001776, -19.50000000000000000 ) ) ;
#311 = VECTOR ( 'NONE', #59625, 1000.000000000000000 ) ;
#312 = DIRECTION ( 'NONE',  ( 1.000000000000000000, 0.000000000000000000, 0.000000000000000000 ) ) ;
#313 = AXIS2_PLACEMENT_3D ( 'NONE', #44992, #2555, #62301 ) ;
#314 = ORIENTED_EDGE ( 'NONE', *, *, #49490, .T. ) ;
#315 = CARTESIAN_POINT ( 'NONE',  ( -14.25000000000000000, -0.2038245569916330158, 21.77831216351300014 ) ) ;
#316 = CARTESIAN_POINT ( 'NONE',  ( 5.257023737882819070, -4.032023737882826531, 54.00000000000000711 ) ) ;
#317 = ORIENTED_EDGE ( 'NONE', *, *, #26344, .F. ) ;
#318 = LINE ( 'NONE', #15885, #62736 ) ;
#319 = PLANE ( 'NONE',  #6241 ) ;
#320 = CARTESIAN_POINT ( 'NONE',  ( 8.250000000000005329, -7.249999999999998224, -19.50000000000000000 ) ) ;
#321 = VECTOR ( 'NONE', #3166, 1000.000000000000000 ) ;
#322 = CARTESIAN_POINT ( 'NONE',  ( 4.186483450353422953, 11.77351654964658501, 455.0000000000000568 ) ) ;
#323 = CARTESIAN_POINT ( 'NONE',  ( 275.5000000000000000, -42.50000000000000000, -30.09999999999999787 ) ) ;
#324 = VECTOR ( 'NONE', #38964, 1000.000000000000000 ) ;
#325 = VERTEX_POINT ( 'NONE', #15027 ) ;
#326 = ORIENTED_EDGE ( 'NONE', *, *, #36665, .T. ) ;
#327 = CARTESIAN_POINT ( 'NONE',  ( -9.689999999999999503, -9.750000000000001776, -5.000000000000000000 ) ) ;
#328 = ORIENTED_EDGE ( 'NONE', *, *, #56971, .F. ) ;
#329 = CYLINDRICAL_SURFACE ( 'NONE', #52589, 2.458500000000000796 ) ;
#330 = VERTEX_POINT ( 'NONE', #52509 ) ;
#331 = DIRECTION ( 'NONE',  ( 0.000000000000000000, 0.000000000000000000, 1.000000000000000000 ) ) ;
#332 = EDGE_CURVE ( 'NONE', #67879, #12341, #4078, .T. ) ;
#333 = DIRECTION ( 'NONE',  ( -1.836970198721029934E-16, -1.836970198721010706E-16, 1.000000000000000000 ) ) ;
#334 = EDGE_CURVE ( 'NONE', #43309, #34406, #4773, .T. ) ;
#335 = PLANE ( 'NONE',  #53647 ) ;
#336 = ORIENTED_EDGE ( 'NONE', *, *, #64829, .F. ) ;
#337 = EDGE_LOOP ( 'NONE', ( #22411, #3438, #18951, #7458 ) ) ;
#338 = VECTOR ( 'NONE', #2632, 1000.000000000000000 ) ;
#339 = CARTESIAN_POINT ( 'NONE',  ( -6.331612867284244217, -8.406483450353421816, 455.0000000000000568 ) ) ;
#340 = ORIENTED_EDGE ( 'NONE', *, *, #61679, .T. ) ;
#341 = VERTEX_POINT ( 'NONE', #10421 ) ;
#342 = CARTESIAN_POINT ( 'NONE',  ( 11.75000000000000000, -5.000000000000000000, 23.89194109070750471 ) ) ;
#343 = LINE ( 'NONE', #58702, #21159 ) ;
#344 = CARTESIAN_POINT ( 'NONE',  ( 7.000000000000000000, -28.94999999999999929, -13.50000000000000000 ) ) ;
#345 = EDGE_CURVE ( 'NONE', #14752, #26669, #26112, .T. ) ;
#346 = ORIENTED_EDGE ( 'NONE', *, *, #49780, .F. ) ;
#347 = AXIS2_PLACEMENT_3D ( 'NONE', #37839, #1052, #32875 ) ;
#348 = DIRECTION ( 'NONE',  ( -0.000000000000000000, 3.673940397442059868E-16, -1.000000000000000000 ) ) ;
#350 = DIRECTION ( 'NONE',  ( -1.000000000000000000, 0.000000000000000000, 0.000000000000000000 ) ) ;
#349 = DIRECTION ( 'NONE',  ( -0.000000000000000000, 0.000000000000000000, -1.000000000000000000 ) ) ;
#351 = ORIENTED_EDGE ( 'NONE', *, *, #10046, .F. ) ;
#352 = ORIENTED_EDGE ( 'NONE', *, *, #34899, .F. ) ;
#354 = VERTEX_POINT ( 'NONE', #52877 ) ;
#353 = DIRECTION ( 'NONE',  ( 1.047444401652940007E-14, 1.000000000000000000, 1.836970198721029934E-16 ) ) ;
#355 = VERTEX_POINT ( 'NONE', #24929 ) ;
#356 = EDGE_CURVE ( 'NONE', #64205, #63555, #57452, .T. ) ;
#357 = PLANE ( 'NONE',  #20890 ) ;
#358 = VECTOR ( 'NONE', #51370, 1000.000000000000000 ) ;
#359 = ADVANCED_FACE ( 'NONE', ( #19615 ), #63466, .F. ) ;
#360 = ORIENTED_EDGE ( 'NONE', *, *, #15360, .T. ) ;
#361 = VERTEX_POINT ( 'NONE', #69466 ) ;
#362 = AXIS2_PLACEMENT_3D ( 'NONE', #29002, #49877, #27973 ) ;
#364 = CARTESIAN_POINT ( 'NONE',  ( 3.682023737882785586, -9.912023737882801555, 26.00000000000000000 ) ) ;
#363 = VECTOR ( 'NONE', #30317, 1000.000000000000000 ) ;
#365 = CARTESIAN_POINT ( 'NONE',  ( 39.00000000000000000, -21.00000000000000000, -16.96999999999999886 ) ) ;
#366 = ORIENTED_EDGE ( 'NONE', *, *, #51811, .T. ) ;
#367 = CARTESIAN_POINT ( 'NONE',  ( 39.00000000000000000, 4.286263797015736595E-16, -3.500000000000000000 ) ) ;
#368 = CARTESIAN_POINT ( 'NONE',  ( 8.612468434717177601, 1.466476262117168972, 26.00000000000000711 ) ) ;
#369 = VECTOR ( 'NONE', #9157, 1000.000000000000000 ) ;
#370 = AXIS2_PLACEMENT_3D ( 'NONE', #47263, #51866, #52935 ) ;
#371 = EDGE_CURVE ( 'NONE', #42134, #10117, #15730, .T. ) ;
#372 = LINE ( 'NONE', #65080, #9063 ) ;
#373 = VERTEX_POINT ( 'NONE', #52152 ) ;
#374 = EDGE_CURVE ( 'NONE', #1632, #1811, #9368, .T. ) ;
#375 = AXIS2_PLACEMENT_3D ( 'NONE', #48813, #22962, #60097 ) ;
#376 = FACE_OUTER_BOUND ( 'NONE', #48764, .T. ) ;
#377 = CARTESIAN_POINT ( 'NONE',  ( 25.90000000000000213, 13.66939075806899240, 20.79999999999999361 ) ) ;
#379 = ORIENTED_EDGE ( 'NONE', *, *, #51031, .F. ) ;
#378 = DIRECTION ( 'NONE',  ( -1.000000000000000000, 0.000000000000000000, 0.000000000000000000 ) ) ;
#381 = VERTEX_POINT ( 'NONE', #68418 ) ;
#380 = CARTESIAN_POINT ( 'NONE',  ( 6.500000000000000888, -6.500000000000002665, -1.000000000000000000 ) ) ;
#382 = FACE_OUTER_BOUND ( 'NONE', #42466, .T. ) ;
#383 = CARTESIAN_POINT ( 'NONE',  ( -4.141586236041100655, 5.779227145995200488, 26.00000000000000711 ) ) ;
#384 = AXIS2_PLACEMENT_3D ( 'NONE', #58436, #19880, #25191 ) ;
#385 = EDGE_CURVE ( 'NONE', #21656, #53653, #49808, .T. ) ;
#386 = PLANE ( 'NONE',  #21114 ) ;
#387 = CARTESIAN_POINT ( 'NONE',  ( 7.811466277050736373, -4.740315990920159095, 195.0000000000000284 ) ) ;
#388 = DIRECTION ( 'NONE',  ( 1.836970198721029934E-16, 1.836970198721010706E-16, -1.000000000000000000 ) ) ;
#389 = PLANE ( 'NONE',  #20249 ) ;
#390 = CIRCLE ( 'NONE', #36469, 1.224999999999998757 ) ;
#391 = VERTEX_POINT ( 'NONE', #36234 ) ;
#392 = CARTESIAN_POINT ( 'NONE',  ( 7.000000000000000000, -20.40000000000000213, 12.40000000000000213 ) ) ;
#394 = ORIENTED_EDGE ( 'NONE', *, *, #68255, .T. ) ;
#393 = LINE ( 'NONE', #21950, #33380 ) ;
#396 = ORIENTED_EDGE ( 'NONE', *, *, #62344, .F. ) ;
#395 = DIRECTION ( 'NONE',  ( 0.5001543609659999667, 1.060466075314215496E-16, 0.8659362650950080953 ) ) ;
#397 =( LENGTH_UNIT ( ) NAMED_UNIT ( * ) SI_UNIT ( .MILLI., .METRE. ) );
#398 = FACE_OUTER_BOUND ( 'NONE', #65165, .T. ) ;
#399 = ORIENTED_EDGE ( 'NONE', *, *, #14387, .F. ) ;
#400 = CARTESIAN_POINT ( 'NONE',  ( 0.000000000000000000, -17.79289321881345032, 20.50000000000000000 ) ) ;
#401 = CARTESIAN_POINT ( 'NONE',  ( -11.00000000000000000, -12.00000000000000000, -12.20000000000000107 ) ) ;
#402 = ORIENTED_EDGE ( 'NONE', *, *, #57864, .T. ) ;
#403 = ADVANCED_FACE ( 'NONE', ( #57802 ), #20668, .T. ) ;
#404 = CARTESIAN_POINT ( 'NONE',  ( -11.00000000000000000, -17.14999999999999858, -27.00000000000000000 ) ) ;
#405 = DIRECTION ( 'NONE',  ( -0.000000000000000000, -0.000000000000000000, -1.000000000000000000 ) ) ;
#406 = CARTESIAN_POINT ( 'NONE',  ( -11.50000000000000000, -11.50000000000100009, 15.00000000000084910 ) ) ;
#407 = EDGE_CURVE ( 'NONE', #41205, #12761, #63817, .T. ) ;
#408 = CIRCLE ( 'NONE', #10596, 6.000000000000005329 ) ;
#409 = AXIS2_PLACEMENT_3D ( 'NONE', #62583, #37393, #19457 ) ;
#410 = ORIENTED_EDGE ( 'NONE', *, *, #40798, .T. ) ;
#411 = CYLINDRICAL_SURFACE ( 'NONE', #53076, 0.1999999999999987899 ) ;
#412 = ORIENTED_EDGE ( 'NONE', *, *, #18461, .T. ) ;
#413 = EDGE_CURVE ( 'NONE', #57464, #29889, #25280, .T. ) ;
#414 = VERTEX_POINT ( 'NONE', #10075 ) ;
#415 = VECTOR ( 'NONE', #51891, 1000.000000000000000 ) ;
#416 = PLANE ( 'NONE',  #61814 ) ;
#417 = CARTESIAN_POINT ( 'NONE',  ( 18.89999999999999858, -21.00000000000001421, -13.86939075806900945 ) ) ;
#418 = VECTOR ( 'NONE', #29526, 1000.000000000000000 ) ;
#419 = VECTOR ( 'NONE', #6445, 1000.000000000000000 ) ;
#420 = EDGE_CURVE ( 'NONE', #60080, #69579, #58869, .T. ) ;
#421 = PLANE ( 'NONE',  #68238 ) ;
#422 = VECTOR ( 'NONE', #20592, 1000.000000000000000 ) ;
#423 = VECTOR ( 'NONE', #48895, 1000.000000000000000 ) ;
#424 = EDGE_CURVE ( 'NONE', #60302, #2392, #26333, .T. ) ;
#425 = PLANE ( 'NONE',  #31811 ) ;
#426 = ORIENTED_EDGE ( 'NONE', *, *, #27573, .F. ) ;
#427 = VERTEX_POINT ( 'NONE', #21020 ) ;
#429 = ORIENTED_EDGE ( 'NONE', *, *, #55499, .F. ) ;
#428 = LINE ( 'NONE', #32247, #49859 ) ;
#430 = ORIENTED_EDGE ( 'NONE', *, *, #65625, .F. ) ;
#431 = DIRECTION ( 'NONE',  ( 1.901462112903059913E-14, 1.000000000000000000, 1.836970198721045958E-16 ) ) ;
#432 = DIRECTION ( 'NONE',  ( 8.673617379884068604E-15, 1.000000000000000000, 0.000000000000000000 ) ) ;
#433 = CARTESIAN_POINT ( 'NONE',  ( -2.993516549646791258, -7.428221114745081621, 455.0000000000000568 ) ) ;
#434 = EDGE_CURVE ( 'NONE', #62987, #48159, #64181, .T. ) ;
#435 = ADVANCED_FACE ( 'NONE', ( #60581 ), #22758, .F. ) ;
#436 = DIRECTION ( 'NONE',  ( 1.000000000000000000, 0.000000000000000000, 0.000000000000000000 ) ) ;
#438 = PLANE ( 'NONE',  #6363 ) ;
#437 = DIRECTION ( 'NONE',  ( -1.000000000000000000, 0.000000000000000000, -0.000000000000000000 ) ) ;
#439 = EDGE_LOOP ( 'NONE', ( #63217, #45203, #8235, #44713 ) ) ;
#441 = ORIENTED_EDGE ( 'NONE', *, *, #10741, .T. ) ;
#440 = CARTESIAN_POINT ( 'NONE',  ( 9.404523737882817258, -1.480523737882825985, 54.00000000000000711 ) ) ;
#442 = EDGE_LOOP ( 'NONE', ( #22286, #68727, #54112, #64195 ) ) ;
#443 = EDGE_LOOP ( 'NONE', ( #42999, #49146, #19104, #67733 ) ) ;
#444 = EDGE_CURVE ( 'NONE', #43479, #36887, #64517, .T. ) ;
#445 = EDGE_CURVE ( 'NONE', #15497, #55902, #11786, .T. ) ;
#446 = DIRECTION ( 'NONE',  ( 0.000000000000000000, -0.7046037717859445770, 0.7096009616573392131 ) ) ;
#447 = CARTESIAN_POINT ( 'NONE',  ( 7.450000000000006395, 7.250000000000000888, -13.00000000000000178 ) ) ;
#448 = EDGE_CURVE ( 'NONE', #36079, #28576, #31997, .T. ) ;
#449 = FACE_OUTER_BOUND ( 'NONE', #18243, .T. ) ;
#450 = ORIENTED_EDGE ( 'NONE', *, *, #43002, .T. ) ;
#451 = ORIENTED_EDGE ( 'NONE', *, *, #36674, .F. ) ;
#452 = ORIENTED_EDGE ( 'NONE', *, *, #12447, .F. ) ;
#453 = VECTOR ( 'NONE', #50729, 1000.000000000000000 ) ;
#454 = CARTESIAN_POINT ( 'NONE',  ( 8.250000000000005329, -8.249999999999998224, -26.00000000000001066 ) ) ;
#455 = DIRECTION ( 'NONE',  ( -1.000000000000000000, 0.000000000000000000, 0.000000000000000000 ) ) ;
#456 = DIRECTION ( 'NONE',  ( 0.000000000000000000, 0.000000000000000000, -1.000000000000000000 ) ) ;
#457 = ORIENTED_EDGE ( 'NONE', *, *, #46961, .T. ) ;
#458 = ORIENTED_EDGE ( 'NONE', *, *, #13082, .T. ) ;
#459 = CARTESIAN_POINT ( 'NONE',  ( 39.00000000000000000, -0.2000000000000000111, 0.000000000000000000 ) ) ;
#460 = ADVANCED_FACE ( 'NONE', ( #5816 ), #59558, .F. ) ;
#461 = DIRECTION ( 'NONE',  ( 1.836970198721029934E-16, -1.836970198721036344E-16, 1.000000000000000000 ) ) ;
#462 = ORIENTED_EDGE ( 'NONE', *, *, #49079, .T. ) ;
#463 = EDGE_CURVE ( 'NONE', #56608, #65774, #59207, .T. ) ;
#464 = AXIS2_PLACEMENT_3D ( 'NONE', #42051, #41699, #8826 ) ;
#465 = AXIS2_PLACEMENT_3D ( 'NONE', #49320, #22091, #59913 ) ;
#466 = DIRECTION ( 'NONE',  ( 0.000000000000000000, 0.000000000000000000, 1.000000000000000000 ) ) ;
#468 = ORIENTED_EDGE ( 'NONE', *, *, #39229, .F. ) ;
#467 = DIRECTION ( 'NONE',  ( 0.000000000000000000, 0.000000000000000000, -1.000000000000000000 ) ) ;
#469 = ORIENTED_EDGE ( 'NONE', *, *, #18723, .T. ) ;
#470 = CARTESIAN_POINT ( 'NONE',  ( -9.093516549646711411, 11.11351654964659730, 195.0000000000000284 ) ) ;
#471 = CARTESIAN_POINT ( 'NONE',  ( -8.250000000000001776, 7.250000000000000888, -18.50000000000000000 ) ) ;
#472 = VECTOR ( 'NONE', #25072, 1000.000000000000000 ) ;
#473 = LINE ( 'NONE', #6118, #22739 ) ;
#474 = DIRECTION ( 'NONE',  ( -0.6414496315691494699, -0.7671651518153064231, -0.000000000000000000 ) ) ;
#475 = DIRECTION ( 'NONE',  ( 0.000000000000000000, -0.8188976377952758012, -0.5739395950910839428 ) ) ;
#476 = VECTOR ( 'NONE', #4566, 1000.000000000000000 ) ;
#477 = VECTOR ( 'NONE', #26958, 1000.000000000000000 ) ;
#478 = ORIENTED_EDGE ( 'NONE', *, *, #7168, .T. ) ;
#479 = LINE ( 'NONE', #69082, #25901 ) ;
#480 = ORIENTED_EDGE ( 'NONE', *, *, #45337, .T. ) ;
#481 = CARTESIAN_POINT ( 'NONE',  ( -9.093516549646711411, 10.08346604330776941, 195.0000000000000284 ) ) ;
#482 = FACE_OUTER_BOUND ( 'NONE', #63046, .T. ) ;
#483 = CARTESIAN_POINT ( 'NONE',  ( -8.198316549646712303, 5.993516549646603409, 455.0000000000000568 ) ) ;
#484 = CIRCLE ( 'NONE', #15171, 0.1999999999999996503 ) ;
#485 = DIRECTION ( 'NONE',  ( 0.8660254037844435926, 0.4999999999999913958, 2.509347957447859069E-16 ) ) ;
#486 = FACE_OUTER_BOUND ( 'NONE', #18940, .T. ) ;
#487 = ORIENTED_EDGE ( 'NONE', *, *, #5618, .F. ) ;
#488 = CARTESIAN_POINT ( 'NONE',  ( 5.668387132715918320, -8.406483450353393394, 195.0000000000000284 ) ) ;
#489 = CARTESIAN_POINT ( 'NONE',  ( 283.0000000000000568, -23.70411739045900390, 12.50000000000000000 ) ) ;
#490 = EDGE_CURVE ( 'NONE', #33868, #48285, #12497, .T. ) ;
#491 = ORIENTED_EDGE ( 'NONE', *, *, #68790, .F. ) ;
#492 = DIRECTION ( 'NONE',  ( -0.000000000000000000, 3.673940397442059868E-16, -1.000000000000000000 ) ) ;
#493 = DIRECTION ( 'NONE',  ( -1.000000000000000000, 0.000000000000000000, 0.000000000000000000 ) ) ;
#494 = AXIS2_PLACEMENT_3D ( 'NONE', #5103, #65205, #17093 ) ;
#495 = EDGE_CURVE ( 'NONE', #42963, #28954, #53915, .T. ) ;
#496 = ORIENTED_EDGE ( 'NONE', *, *, #56762, .T. ) ;
#497 = CARTESIAN_POINT ( 'NONE',  ( 8.250000000000005329, -8.249999999999998224, -26.00000000000001066 ) ) ;
#498 = LINE ( 'NONE', #1194, #5981 ) ;
#499 = ORIENTED_EDGE ( 'NONE', *, *, #54883, .F. ) ;
#500 = DIRECTION ( 'NONE',  ( 0.000000000000000000, 0.000000000000000000, -1.000000000000000000 ) ) ;
#501 = EDGE_CURVE ( 'NONE', #12761, #21320, #43973, .T. ) ;
#502 = VECTOR ( 'NONE', #16926, 1000.000000000000000 ) ;
#503 = LINE ( 'NONE', #22069, #24410 ) ;
#504 = CARTESIAN_POINT ( 'NONE',  ( -4.173516549646792306, -12.00648345035339837, 195.0000000000000284 ) ) ;
#505 = EDGE_CURVE ( 'NONE', #35470, #13557, #53561, .T. ) ;
#506 = DIRECTION ( 'NONE',  ( 0.000000000000000000, 1.000000000000000000, 0.000000000000000000 ) ) ;
#507 = ADVANCED_FACE ( 'NONE', ( #26684, #69821 ), #37996, .T. ) ;
#508 = ORIENTED_EDGE ( 'NONE', *, *, #1282, .F. ) ;
#510 = ORIENTED_EDGE ( 'NONE', *, *, #6735, .F. ) ;
#509 = FACE_OUTER_BOUND ( 'NONE', #40006, .T. ) ;
#511 = VECTOR ( 'NONE', #43350, 1000.000000000000000 ) ;
#512 = CIRCLE ( 'NONE', #39986, 0.3999999999993817390 ) ;
#513 = DIRECTION ( 'NONE',  ( 0.000000000000000000, 0.000000000000000000, -1.000000000000000000 ) ) ;
#514 = CARTESIAN_POINT ( 'NONE',  ( 10.92648345035336277, 2.893516549646527825, 455.0000000000000568 ) ) ;
#515 = CARTESIAN_POINT ( 'NONE',  ( -9.689726262117227762, 9.689726262117183353, 54.00000000000000711 ) ) ;
#516 = ORIENTED_EDGE ( 'NONE', *, *, #65064, .F. ) ;
#517 = CARTESIAN_POINT ( 'NONE',  ( 11.50000000000000000, -11.50000000000100009, 19.50000000000103739 ) ) ;
#518 = CARTESIAN_POINT ( 'NONE',  ( -11.11351654964671098, 4.193516549646605363, 455.0000000000000568 ) ) ;
#519 = VECTOR ( 'NONE', #50986, 1000.000000000000000 ) ;
#520 = VERTEX_POINT ( 'NONE', #38678 ) ;
#521 = EDGE_LOOP ( 'NONE', ( #59602, #68123, #42949, #33400 ) ) ;
#523 = VERTEX_POINT ( 'NONE', #48252 ) ;
#522 = AXIS2_PLACEMENT_3D ( 'NONE', #27556, #699, #37140 ) ;
#524 = CARTESIAN_POINT ( 'NONE',  ( -18.85410196625000268, -17.50000000000000000, -21.50000000000000000 ) ) ;
#525 = DIRECTION ( 'NONE',  ( 0.000000000000000000, -3.673940397442059868E-16, 1.000000000000000000 ) ) ;
#526 = ORIENTED_EDGE ( 'NONE', *, *, #44380, .T. ) ;
#527 = VERTEX_POINT ( 'NONE', #49303 ) ;
#528 = ORIENTED_EDGE ( 'NONE', *, *, #49827, .F. ) ;
#529 = VECTOR ( 'NONE', #27230, 1000.000000000000000 ) ;
#530 = CARTESIAN_POINT ( 'NONE',  ( -8.250000000000001776, 0.000000000000000000, -24.00000000000000000 ) ) ;
#531 = ORIENTED_EDGE ( 'NONE', *, *, #58938, .T. ) ;
#532 = ORIENTED_EDGE ( 'NONE', *, *, #12088, .T. ) ;
#533 = ORIENTED_EDGE ( 'NONE', *, *, #46307, .T. ) ;
#534 = ORIENTED_EDGE ( 'NONE', *, *, #35078, .T. ) ;
#535 = LINE ( 'NONE', #21059, #41754 ) ;
#536 = UNCERTAINTY_MEASURE_WITH_UNIT (LENGTH_MEASURE( 1.000000000000000082E-05 ), #15361, 'distance_accuracy_value', 'NONE');
#537 = ADVANCED_FACE ( 'NONE', ( #5475 ), #48597, .T. ) ;
#539 = ORIENTED_EDGE ( 'NONE', *, *, #11824, .T. ) ;
#538 = CYLINDRICAL_SURFACE ( 'NONE', #54810, 0.2000000000000005107 ) ;
#540 = CARTESIAN_POINT ( 'NONE',  ( -7.342976262117259623, 4.947141984184421304, 26.00000000000000711 ) ) ;
#541 = EDGE_CURVE ( 'NONE', #27734, #10730, #30589, .T. ) ;
#542 = CARTESIAN_POINT ( 'NONE',  ( -7.394232575409614761, 3.710438382363058896, 26.00000000000000711 ) ) ;
#543 = FACE_OUTER_BOUND ( 'NONE', #55140, .T. ) ;
#544 = CIRCLE ( 'NONE', #20825, 0.5000000000001357803 ) ;
#545 = EDGE_CURVE ( 'NONE', #32184, #13431, #27723, .T. ) ;
#546 = ORIENTED_EDGE ( 'NONE', *, *, #54338, .T. ) ;
#547 = AXIS2_PLACEMENT_3D ( 'NONE', #67792, #14039, #9095 ) ;
#548 = CARTESIAN_POINT ( 'NONE',  ( 3.724485858128685045, 7.394232575409559693, 54.00000000000000711 ) ) ;
#549 = ORIENTED_EDGE ( 'NONE', *, *, #26936, .F. ) ;
#550 = DIRECTION ( 'NONE',  ( -1.261617073437657735E-14, -1.000000000000000000, 0.000000000000000000 ) ) ;
#551 = AXIS2_PLACEMENT_3D ( 'NONE', #51333, #46036, #67608 ) ;
#553 = CARTESIAN_POINT ( 'NONE',  ( 36.90000000000000568, 20.60000000000000142, -13.86939075806900057 ) ) ;
#552 = VECTOR ( 'NONE', #39215, 1000.000000000000000 ) ;
#554 = PLANE ( 'NONE',  #7433 ) ;
#555 = LINE ( 'NONE', #43330, #59554 ) ;
#556 = ADVANCED_FACE ( 'NONE', ( #509 ), #65220, .T. ) ;
#557 = ORIENTED_EDGE ( 'NONE', *, *, #21564, .T. ) ;
#558 = DIRECTION ( 'NONE',  ( -1.000000000000000000, 0.000000000000000000, 0.000000000000000000 ) ) ;
#559 = COLOUR_RGB ( '', 0.08235294, 0.09019608, 0.10196078) ;
#560 = CARTESIAN_POINT ( 'NONE',  ( 39.00000000000000000, -21.00000000000000000, -14.57806571531352091 ) ) ;
#561 = DIRECTION ( 'NONE',  ( -1.000000000000000000, 0.000000000000000000, 0.000000000000000000 ) ) ;
#562 = CIRCLE ( 'NONE', #40052, 2.458500000000000796 ) ;
#563 = CARTESIAN_POINT ( 'NONE',  ( 11.00000000000000000, -11.70000000000000284, 12.50000000000000000 ) ) ;
#564 = DIRECTION ( 'NONE',  ( 1.000000000000000000, -0.000000000000000000, 0.000000000000000000 ) ) ;
#565 = DIRECTION ( 'NONE',  ( 0.000000000000000000, 0.000000000000000000, 1.000000000000000000 ) ) ;
#566 = DIRECTION ( 'NONE',  ( 0.000000000000000000, -1.000000000000000000, 0.000000000000000000 ) ) ;
#567 = PLANE ( 'NONE',  #57123 ) ;
#568 = EDGE_CURVE ( 'NONE', #4457, #43741, #22425, .T. ) ;
#569 = AXIS2_PLACEMENT_3D ( 'NONE', #12617, #13330, #56464 ) ;
#570 = EDGE_LOOP ( 'NONE', ( #1915, #32078, #8129, #192 ) ) ;
#571 = CARTESIAN_POINT ( 'NONE',  ( 13.00000000000000178, -17.50000000000000000, -20.05051025721700242 ) ) ;
#572 = DIRECTION ( 'NONE',  ( -4.956352788505168198E-15, -1.000000000000000000, 0.000000000000000000 ) ) ;
#573 = AXIS2_PLACEMENT_3D ( 'NONE', #21075, #15076, #32996 ) ;
#574 = LINE ( 'NONE', #22144, #58360 ) ;
#575 = FACE_OUTER_BOUND ( 'NONE', #39075, .T. ) ;
#576 = ORIENTED_EDGE ( 'NONE', *, *, #13666, .T. ) ;
#577 = DIRECTION ( 'NONE',  ( -2.439149994343049068E-15, -1.000000000000000000, 0.000000000000000000 ) ) ;
#578 = DIRECTION ( 'NONE',  ( 0.000000000000000000, 0.000000000000000000, 1.000000000000000000 ) ) ;
#579 = ADVANCED_FACE ( 'NONE', ( #13181 ), #1883, .F. ) ;
#580 = EDGE_CURVE ( 'NONE', #24182, #41169, #23453, .T. ) ;
#581 = CYLINDRICAL_SURFACE ( 'NONE', #36803, 8.000000000000000000 ) ;
#582 = LINE ( 'NONE', #16497, #34375 ) ;
#583 = CARTESIAN_POINT ( 'NONE',  ( -7.517976262117294084, -6.665817930929260449, 54.00000000000000711 ) ) ;
#584 = EDGE_CURVE ( 'NONE', #17555, #46156, #6828, .T. ) ;
#585 = DIRECTION ( 'NONE',  ( 1.000000000000000000, -0.000000000000000000, 0.000000000000000000 ) ) ;
#586 = EDGE_CURVE ( 'NONE', #18944, #24350, #18136, .T. ) ;
#587 = VERTEX_POINT ( 'NONE', #66922 ) ;
#588 = AXIS2_PLACEMENT_3D ( 'NONE', #30987, #41594, #37012 ) ;
#589 = ORIENTED_EDGE ( 'NONE', *, *, #57565, .F. ) ;
#590 = ADVANCED_FACE ( 'NONE', ( #7529 ), #61257, .F. ) ;
#591 = PLANE ( 'NONE',  #55308 ) ;
#592 = DIRECTION ( 'NONE',  ( -1.000000000000000000, 1.794541526872559352E-16, 0.000000000000000000 ) ) ;
#593 = ORIENTED_EDGE ( 'NONE', *, *, #855, .F. ) ;
#594 = DIRECTION ( 'NONE',  ( 0.000000000000000000, 1.000000000000000000, 0.000000000000000000 ) ) ;
#595 = VECTOR ( 'NONE', #44304, 1000.000000000000000 ) ;
#596 = VERTEX_POINT ( 'NONE', #12818 ) ;
#597 = CIRCLE ( 'NONE', #14164, 1.224999999999998757 ) ;
#598 = CARTESIAN_POINT ( 'NONE',  ( 7.000000000000000000, -42.50000000000000000, 9.950000000000001066 ) ) ;
#599 = ORIENTED_EDGE ( 'NONE', *, *, #39611, .F. ) ;
#600 = ORIENTED_EDGE ( 'NONE', *, *, #16363, .T. ) ;
#601 = CARTESIAN_POINT ( 'NONE',  ( 16.75000000000000000, -2.500000000000000000, -23.22168783648699986 ) ) ;
#602 = ORIENTED_EDGE ( 'NONE', *, *, #62615, .F. ) ;
#603 = FACE_OUTER_BOUND ( 'NONE', #10615, .T. ) ;
#604 = FACE_OUTER_BOUND ( 'NONE', #11488, .T. ) ;
#605 = CARTESIAN_POINT ( 'NONE',  ( 14.50000000000000000, -42.50000000000000000, 26.50000000000000000 ) ) ;
#606 = AXIS2_PLACEMENT_3D ( 'NONE', #28514, #56090, #7641 ) ;
#607 = VECTOR ( 'NONE', #2459, 1000.000000000000000 ) ;
#608 = AXIS2_PLACEMENT_3D ( 'NONE', #9316, #63413, #57045 ) ;
#609 = AXIS2_PLACEMENT_3D ( 'NONE', #20518, #59049, #32541 ) ;
#610 = ORIENTED_EDGE ( 'NONE', *, *, #34222, .F. ) ;
#611 = VERTEX_POINT ( 'NONE', #40036 ) ;
#612 = DIRECTION ( 'NONE',  ( 1.000000000000000000, -0.000000000000000000, 0.000000000000000000 ) ) ;
#613 = LINE ( 'NONE', #38777, #60397 ) ;
#614 = VECTOR ( 'NONE', #18317, 1000.000000000000000 ) ;
#615 =( GEOMETRIC_REPRESENTATION_CONTEXT ( 3 ) GLOBAL_UNCERTAINTY_ASSIGNED_CONTEXT ( ( #42268 ) ) GLOBAL_UNIT_ASSIGNED_CONTEXT ( ( #31322, #48608, #68779 ) ) REPRESENTATION_CONTEXT ( 'NONE', 'WORKASPACE' ) );
#616 = ORIENTED_EDGE ( 'NONE', *, *, #25208, .T. ) ;
#617 = ORIENTED_EDGE ( 'NONE', *, *, #68183, .T. ) ;
#619 = ORIENTED_EDGE ( 'NONE', *, *, #21968, .F. ) ;
#618 = CONTEXT_DEPENDENT_SHAPE_REPRESENTATION ( #6956, #1924 ) ;
#620 = AXIS2_PLACEMENT_3D ( 'NONE', #69047, #10357, #8942 ) ;
#621 = CARTESIAN_POINT ( 'NONE',  ( 40.90000000000000568, 21.00000000000000355, -13.98999642601812354 ) ) ;
#623 = ORIENTED_EDGE ( 'NONE', *, *, #59248, .F. ) ;
#622 = CARTESIAN_POINT ( 'NONE',  ( 14.89999999999999680, 20.60000000000000142, -13.86939075806900057 ) ) ;
#624 = DIRECTION ( 'NONE',  ( -0.000000000000000000, -0.000000000000000000, -1.000000000000000000 ) ) ;
#625 = VECTOR ( 'NONE', #3696, 1000.000000000000000 ) ;
#626 = CARTESIAN_POINT ( 'NONE',  ( 8.250000000000005329, -7.249999999999998224, -15.50000000000000000 ) ) ;
#627 = ORIENTED_EDGE ( 'NONE', *, *, #34864, .F. ) ;
#628 = ORIENTED_EDGE ( 'NONE', *, *, #33674, .F. ) ;
#629 = ADVANCED_FACE ( 'NONE', ( #34381 ), #67286, .F. ) ;
#630 = CIRCLE ( 'NONE', #40114, 1.000000000000000000 ) ;
#631 = EDGE_CURVE ( 'NONE', #59475, #32917, #18840, .T. ) ;
#632 = EDGE_LOOP ( 'NONE', ( #12732, #36531, #57400, #6391 ) ) ;
#633 = EDGE_CURVE ( 'NONE', #54560, #21685, #40408, .T. ) ;
#634 = DIRECTION ( 'NONE',  ( 0.000000000000000000, 0.000000000000000000, -1.000000000000000000 ) ) ;
#635 = DIRECTION ( 'NONE',  ( 1.836970198721029934E-16, 1.836970198721010706E-16, -1.000000000000000000 ) ) ;
#636 = EDGE_LOOP ( 'NONE', ( #49737, #64125, #34092, #53225 ) ) ;
#637 = SURFACE_STYLE_FILL_AREA ( #1652 ) ;
#638 = PLANE ( 'NONE',  #53910 ) ;
#640 = ORIENTED_EDGE ( 'NONE', *, *, #69472, .F. ) ;
#639 = LINE ( 'NONE', #27506, #3790 ) ;
#641 = ORIENTED_EDGE ( 'NONE', *, *, #13313, .T. ) ;
#642 = CARTESIAN_POINT ( 'NONE',  ( -7.593516549646838421, -11.78648345035340839, 455.0000000000000568 ) ) ;
#643 = CARTESIAN_POINT ( 'NONE',  ( 7.250000000000005329, 7.250000000000000888, -7.000000000000000000 ) ) ;
#644 = PLANE ( 'NONE',  #32533 ) ;
#645 = FACE_OUTER_BOUND ( 'NONE', #22768, .T. ) ;
#646 = AXIS2_PLACEMENT_3D ( 'NONE', #65623, #39094, #23527 ) ;
#647 = CARTESIAN_POINT ( 'NONE',  ( 7.450000000000004619, -1.336933437520057563E-15, -19.50000000000000000 ) ) ;
#648 = ORIENTED_EDGE ( 'NONE', *, *, #3440, .F. ) ;
#649 = CARTESIAN_POINT ( 'NONE',  ( -10.49297626211726175, 3.650476262117184234, 54.00000000000000711 ) ) ;
#650 = DIRECTION ( 'NONE',  ( -1.185108578570163244E-14, -1.000000000000000000, -1.836970198721014650E-16 ) ) ;
#651 = DIRECTION ( 'NONE',  ( -1.836970198721029934E-16, 1.836970198721036344E-16, -1.000000000000000000 ) ) ;
#653 = EDGE_LOOP ( 'NONE', ( #42784, #54327, #4173, #68157 ) ) ;
#652 = DIRECTION ( 'NONE',  ( 0.000000000000000000, 1.000000000000000000, 0.000000000000000000 ) ) ;
#654 = VECTOR ( 'NONE', #47837, 1000.000000000000000 ) ;
#655 = AXIS2_PLACEMENT_3D ( 'NONE', #12198, #65284, #6575 ) ;
#656 = VECTOR ( 'NONE', #33989, 1000.000000000000000 ) ;
#657 = DIRECTION ( 'NONE',  ( -1.000000000000000000, 0.000000000000000000, 0.000000000000000000 ) ) ;
#658 = DIRECTION ( 'NONE',  ( 0.7671651518152939886, -0.6414496315691644579, -2.587583378555133721E-16 ) ) ;
#659 = CARTESIAN_POINT ( 'NONE',  ( 10.31452373788281562, -6.849523737882823760, 54.00000000000000711 ) ) ;
#660 = AXIS2_PLACEMENT_3D ( 'NONE', #3330, #61305, #29143 ) ;
#661 = CIRCLE ( 'NONE', #35613, 0.1749999999999993783 ) ;
#662 = CIRCLE ( 'NONE', #5214, 0.2000000000000005107 ) ;
#663 = DIRECTION ( 'NONE',  ( -0.000000000000000000, 3.673940397442059868E-16, -1.000000000000000000 ) ) ;
#664 = ORIENTED_EDGE ( 'NONE', *, *, #67900, .F. ) ;
#665 = CARTESIAN_POINT ( 'NONE',  ( -8.697938382363103571, -2.420780051175099423, 54.00000000000000711 ) ) ;
#666 = DIRECTION ( 'NONE',  ( 1.000000000000000000, 0.000000000000000000, 0.000000000000000000 ) ) ;
#667 = ORIENTED_EDGE ( 'NONE', *, *, #3824, .T. ) ;
#668 = CARTESIAN_POINT ( 'NONE',  ( 7.250000000000005329, -7.249999999999998224, -15.50000000000000000 ) ) ;
#669 = LINE ( 'NONE', #60052, #57064 ) ;
#670 = VECTOR ( 'NONE', #11222, 1000.000000000000000 ) ;
#671 = CARTESIAN_POINT ( 'NONE',  ( 7.250000000000005329, -7.249999999999998224, -11.00000000000000000 ) ) ;
#672 = CARTESIAN_POINT ( 'NONE',  ( -7.259684009079930611, 7.798499376343971612, 195.0000000000000284 ) ) ;
#673 = PLANE ( 'NONE',  #54224 ) ;
#674 = EDGE_CURVE ( 'NONE', #5423, #64032, #46062, .T. ) ;
#675 = ADVANCED_FACE ( 'NONE', ( #1525 ), #23797, .F. ) ;
#676 = DIRECTION ( 'NONE',  ( 0.000000000000000000, -0.1249999999999996531, -0.9921567416492215186 ) ) ;
#677 = AXIS2_PLACEMENT_3D ( 'NONE', #17605, #24303, #7681 ) ;
#678 = ORIENTED_EDGE ( 'NONE', *, *, #57075, .T. ) ;
#679 = EDGE_CURVE ( 'NONE', #53653, #2028, #29441, .T. ) ;
#680 = LINE ( 'NONE', #46143, #37362 ) ;
#681 = CARTESIAN_POINT ( 'NONE',  ( 7.000000000000000000, -30.80000000000000071, -12.20000000000000107 ) ) ;
#682 = EDGE_CURVE ( 'NONE', #36598, #40990, #13532, .T. ) ;
#683 = ORIENTED_EDGE ( 'NONE', *, *, #53543, .T. ) ;
#684 = MECHANICAL_DESIGN_GEOMETRIC_PRESENTATION_REPRESENTATION (  '', ( #62800 ), #8420 ) ;
#685 = DIRECTION ( 'NONE',  ( -1.000000000000000000, 7.304098846218132892E-15, -0.000000000000000000 ) ) ;
#686 = PRODUCT_RELATED_PRODUCT_CATEGORY ( 'part', '', ( #67289 ) ) ;
#687 = CARTESIAN_POINT ( 'NONE',  ( -16.75000000000000000, -0.2038245569916330158, 21.77831216351300014 ) ) ;
#688 = FACE_OUTER_BOUND ( 'NONE', #35087, .T. ) ;
#689 = ORIENTED_EDGE ( 'NONE', *, *, #63377, .F. ) ;
#690 =( REPRESENTATION_RELATIONSHIP ('NONE','NONE', #33057, #60228 ) REPRESENTATION_RELATIONSHIP_WITH_TRANSFORMATION ( #16532 )SHAPE_REPRESENTATION_RELATIONSHIP( ) );
#691 = EDGE_CURVE ( 'NONE', #33692, #7966, #2577, .T. ) ;
#692 = ORIENTED_EDGE ( 'NONE', *, *, #38279, .T. ) ;
#693 = DIRECTION ( 'NONE',  ( -0.4999999999999913958, 0.8660254037844437036, 6.723777587268537869E-17 ) ) ;
#695 = ORIENTED_EDGE ( 'NONE', *, *, #12685, .F. ) ;
#694 = EDGE_CURVE ( 'NONE', #60836, #46781, #44152, .T. ) ;
#696 = EDGE_LOOP ( 'NONE', ( #30041, #28566, #64326, #7292 ) ) ;
#697 = CARTESIAN_POINT ( 'NONE',  ( 1.634292677759874302, 8.227189898828697778, 54.00000000000000711 ) ) ;
#698 = LINE ( 'NONE', #23621, #5377 ) ;
#699 = DIRECTION ( 'NONE',  ( 0.000000000000000000, -1.000000000000000000, 0.000000000000000000 ) ) ;
#700 = AXIS2_PLACEMENT_3D ( 'NONE', #18899, #62020, #12531 ) ;
#701 = VERTEX_POINT ( 'NONE', #45700 ) ;
#702 = DIRECTION ( 'NONE',  ( 0.000000000000000000, 1.000000000000000000, 0.000000000000000000 ) ) ;
#704 = DIRECTION ( 'NONE',  ( 8.359604446858500663E-15, 1.000000000000000000, 3.673940397442059868E-16 ) ) ;
#703 = DIRECTION ( 'NONE',  ( 0.000000000000000000, 1.000000000000000000, 0.000000000000000000 ) ) ;
#705 = VERTEX_POINT ( 'NONE', #39361 ) ;
#706 = ORIENTED_EDGE ( 'NONE', *, *, #9650, .T. ) ;
#708 = ORIENTED_EDGE ( 'NONE', *, *, #57409, .F. ) ;
#707 = LINE ( 'NONE', #53756, #64695 ) ;
#709 = VECTOR ( 'NONE', #25731, 1000.000000000000000 ) ;
#710 = ORIENTED_EDGE ( 'NONE', *, *, #11155, .T. ) ;
#711 = VECTOR ( 'NONE', #11442, 1000.000000000000000 ) ;
#712 = LINE ( 'NONE', #9935, #52492 ) ;
#713 = VECTOR ( 'NONE', #29747, 1000.000000000000000 ) ;
#714 = AXIS2_PLACEMENT_3D ( 'NONE', #11350, #11017, #4670 ) ;
#715 = VECTOR ( 'NONE', #34605, 1000.000000000000000 ) ;
#716 = DIRECTION ( 'NONE',  ( 0.000000000000000000, 0.000000000000000000, 1.000000000000000000 ) ) ;
#717 = EDGE_LOOP ( 'NONE', ( #1969, #50627, #51311, #41125, #30322, #8766, #47543, #54269 ) ) ;
#718 = ORIENTED_EDGE ( 'NONE', *, *, #64493, .F. ) ;
#719 = AXIS2_PLACEMENT_3D ( 'NONE', #53529, #25960, #46803 ) ;
#720 = AXIS2_PLACEMENT_3D ( 'NONE', #47472, #10687, #69040 ) ;
#721 = AXIS2_PLACEMENT_3D ( 'NONE', #41997, #30342, #9477 ) ;
#722 = CARTESIAN_POINT ( 'NONE',  ( -9.093516549646711411, 10.91351654964659978, 455.0000000000000568 ) ) ;
#723 = LINE ( 'NONE', #42453, #25543 ) ;
#724 = ORIENTED_EDGE ( 'NONE', *, *, #43067, .T. ) ;
#725 = EDGE_CURVE ( 'NONE', #13178, #7022, #29794, .T. ) ;
#726 = DIRECTION ( 'NONE',  ( -1.000000000000000000, 0.000000000000000000, 0.000000000000000000 ) ) ;
#728 = AXIS2_PLACEMENT_3D ( 'NONE', #36991, #31684, #58558 ) ;
#727 = CARTESIAN_POINT ( 'NONE',  ( -9.690000000000001279, 10.50000000000000178, -4.250000000000000000 ) ) ;
#729 = CARTESIAN_POINT ( 'NONE',  ( 41.09999999999999432, 13.66939075806899950, 20.80000000000000426 ) ) ;
#730 = ORIENTED_EDGE ( 'NONE', *, *, #44793, .F. ) ;
#731 = VECTOR ( 'NONE', #46911, 1000.000000000000000 ) ;
#732 = LINE ( 'NONE', #43847, #65115 ) ;
#733 = LINE ( 'NONE', #60793, #54302 ) ;
#735 = ORIENTED_EDGE ( 'NONE', *, *, #49732, .T. ) ;
#734 = DIRECTION ( 'NONE',  ( 0.000000000000000000, 0.000000000000000000, -1.000000000000000000 ) ) ;
#737 = ORIENTED_EDGE ( 'NONE', *, *, #66754, .F. ) ;
#736 = CYLINDRICAL_SURFACE ( 'NONE', #763, 4.000000000000000000 ) ;
#738 = FACE_OUTER_BOUND ( 'NONE', #41918, .T. ) ;
#739 = EDGE_CURVE ( 'NONE', #268, #19808, #12478, .T. ) ;
#740 = DIRECTION ( 'NONE',  ( 0.000000000000000000, 0.000000000000000000, 1.000000000000000000 ) ) ;
#741 = CYLINDRICAL_SURFACE ( 'NONE', #16577, 1.000000000000000000 ) ;
#742 = DIRECTION ( 'NONE',  ( -1.000000000000000000, 0.000000000000000000, 0.000000000000000000 ) ) ;
#743 = DIRECTION ( 'NONE',  ( 0.000000000000000000, 0.000000000000000000, -1.000000000000000000 ) ) ;
#744 = EDGE_CURVE ( 'NONE', #11392, #21475, #55291, .T. ) ;
#745 = LINE ( 'NONE', #59085, #36041 ) ;
#746 = ORIENTED_EDGE ( 'NONE', *, *, #15039, .F. ) ;
#747 = CARTESIAN_POINT ( 'NONE',  ( 15.00000000000000000, -20.40000000000000213, -12.40000000000000213 ) ) ;
#749 = VERTEX_POINT ( 'NONE', #42155 ) ;
#748 = DIRECTION ( 'NONE',  ( 0.000000000000000000, 0.000000000000000000, -1.000000000000000000 ) ) ;
#751 = ORIENTED_EDGE ( 'NONE', *, *, #28929, .T. ) ;
#750 = CARTESIAN_POINT ( 'NONE',  ( 24.00000000000000000, -15.50000000000000000, -14.50000000000000000 ) ) ;
#752 = CARTESIAN_POINT ( 'NONE',  ( 7.250000000000005329, -7.249999999999998224, -13.50000000000000178 ) ) ;
#753 = VECTOR ( 'NONE', #10732, 1000.000000000000114 ) ;
#754 = DIRECTION ( 'NONE',  ( 0.000000000000000000, 0.000000000000000000, 1.000000000000000000 ) ) ;
#755 = VECTOR ( 'NONE', #5820, 1000.000000000000000 ) ;
#756 = ORIENTED_EDGE ( 'NONE', *, *, #15619, .T. ) ;
#757 = DIRECTION ( 'NONE',  ( -1.836970198721029934E-16, 1.836970198721036344E-16, -1.000000000000000000 ) ) ;
#758 = CARTESIAN_POINT ( 'NONE',  ( 7.250000000000005329, 7.250000000000000888, -13.50000000000000178 ) ) ;
#759 = EDGE_CURVE ( 'NONE', #64942, #41138, #44198, .T. ) ;
#760 = EDGE_LOOP ( 'NONE', ( #11877, #61842, #65585, #14010, #43398, #6520 ) ) ;
#761 = CARTESIAN_POINT ( 'NONE',  ( -8.593516549646793123, -7.616533956692233431, 455.0000000000000568 ) ) ;
#762 = CARTESIAN_POINT ( 'NONE',  ( 275.5000000000000000, 50.00000000000000000, 27.00000000000000000 ) ) ;
#763 = AXIS2_PLACEMENT_3D ( 'NONE', #55845, #33245, #1748 ) ;
#764 = AXIS2_PLACEMENT_3D ( 'NONE', #53431, #27254, #16981 ) ;
#765 = LINE ( 'NONE', #44212, #31442 ) ;
#766 = CARTESIAN_POINT ( 'NONE',  ( 7.357023737882797398, 5.538810540049960984, 26.00000000000000711 ) ) ;
#767 = AXIS2_PLACEMENT_3D ( 'NONE', #45596, #44915, #2470 ) ;
#768 = AXIS2_PLACEMENT_3D ( 'NONE', #55446, #39511, #6988 ) ;
#770 = LINE ( 'NONE', #25982, #22956 ) ;
#769 = VECTOR ( 'NONE', #43138, 1000.000000000000000 ) ;
#771 = ORIENTED_EDGE ( 'NONE', *, *, #36456, .T. ) ;
#772 = ADVANCED_FACE ( 'NONE', ( #63030, #46754 ), #4686, .T. ) ;
#773 = FACE_OUTER_BOUND ( 'NONE', #49623, .T. ) ;
#774 = ORIENTED_EDGE ( 'NONE', *, *, #17721, .F. ) ;
#775 = ADVANCED_FACE ( 'NONE', ( #62666 ), #31566, .T. ) ;
#776 = ORIENTED_EDGE ( 'NONE', *, *, #46433, .T. ) ;
#777 = CARTESIAN_POINT ( 'NONE',  ( 33.89999999999999858, -0.000000000000000000, 20.80000000000000426 ) ) ;
#779 = CARTESIAN_POINT ( 'NONE',  ( 4.149127210878726046, 6.822336235477391320, 54.00000000000000711 ) ) ;
#778 = VECTOR ( 'NONE', #33252, 1000.000000000000000 ) ;
#780 = AXIS2_PLACEMENT_3D ( 'NONE', #16871, #22182, #10518 ) ;
#781 = ADVANCED_FACE ( 'NONE', ( #68330 ), #9995, .F. ) ;
#782 = VECTOR ( 'NONE', #26904, 1000.000000000000000 ) ;
#783 = FACE_OUTER_BOUND ( 'NONE', #23681, .T. ) ;
#784 = CARTESIAN_POINT ( 'NONE',  ( 46.39999999999999858, 21.00000000000000000, -0.2500000000000000000 ) ) ;
#785 = ORIENTED_EDGE ( 'NONE', *, *, #39572, .T. ) ;
#786 = EDGE_CURVE ( 'NONE', #9283, #69426, #58073, .T. ) ;
#787 = ORIENTED_EDGE ( 'NONE', *, *, #45856, .F. ) ;
#789 = ORIENTED_EDGE ( 'NONE', *, *, #32438, .F. ) ;
#788 = DIRECTION ( 'NONE',  ( 1.000000000000000000, 0.000000000000000000, 0.000000000000000000 ) ) ;
#791 = ORIENTED_EDGE ( 'NONE', *, *, #7025, .T. ) ;
#790 = EDGE_CURVE ( 'NONE', #45723, #45427, #9640, .T. ) ;
#792 = VECTOR ( 'NONE', #20280, 1000.000000000000000 ) ;
#793 = CYLINDRICAL_SURFACE ( 'NONE', #25893, 1.929199999999997139 ) ;
#794 = DIRECTION ( 'NONE',  ( 0.000000000000000000, 0.000000000000000000, 1.000000000000000000 ) ) ;
#795 = DIRECTION ( 'NONE',  ( 0.000000000000000000, 1.000000000000000000, 0.000000000000000000 ) ) ;
#796 = DIRECTION ( 'NONE',  ( 0.000000000000000000, -1.000000000000000000, 0.000000000000000000 ) ) ;
#798 = CARTESIAN_POINT ( 'NONE',  ( -4.242044687070611886, -8.465062094116088787, 195.0000000000000284 ) ) ;
#797 = DIRECTION ( 'NONE',  ( 0.000000000000000000, 0.000000000000000000, -1.000000000000000000 ) ) ;
#799 = ORIENTED_EDGE ( 'NONE', *, *, #48308, .T. ) ;
#801 = ORIENTED_EDGE ( 'NONE', *, *, #31729, .T. ) ;
#800 = CARTESIAN_POINT ( 'NONE',  ( -7.450000000000001954, -7.249999999999998224, -21.50000000000000000 ) ) ;
#802 = ORIENTED_EDGE ( 'NONE', *, *, #11052, .F. ) ;
#803 = VERTEX_POINT ( 'NONE', #53143 ) ;
#804 = CARTESIAN_POINT ( 'NONE',  ( 39.90000000000000568, -21.00000000000000000, 14.57806571531351914 ) ) ;
#805 = PLANE ( 'NONE',  #55812 ) ;
#806 = DIRECTION ( 'NONE',  ( 0.000000000000000000, 0.000000000000000000, -1.000000000000000000 ) ) ;
#807 = DIRECTION ( 'NONE',  ( 3.540251991789405856E-15, 1.000000000000000000, 0.000000000000000000 ) ) ;
#808 = ADVANCED_FACE ( 'NONE', ( #69379 ), #15961, .T. ) ;
#809 = EDGE_LOOP ( 'NONE', ( #4041, #12322, #25517, #67082 ) ) ;
#810 = AXIS2_PLACEMENT_3D ( 'NONE', #56558, #8104, #44904 ) ;
#811 = ORIENTED_EDGE ( 'NONE', *, *, #65786, .F. ) ;
#812 = CARTESIAN_POINT ( 'NONE',  ( 7.806483450353418618, 11.11351654964657421, 455.0000000000000568 ) ) ;
#813 = CARTESIAN_POINT ( 'NONE',  ( 32.89999999999999858, 0.000000000000000000, 0.000000000000000000 ) ) ;
#814 = ORIENTED_EDGE ( 'NONE', *, *, #16232, .F. ) ;
#815 = EDGE_CURVE ( 'NONE', #68276, #10103, #58910, .T. ) ;
#816 = ORIENTED_EDGE ( 'NONE', *, *, #61457, .T. ) ;
#817 = CIRCLE ( 'NONE', #40302, 0.1749999999999998224 ) ;
#819 = CARTESIAN_POINT ( 'NONE',  ( 8.406483450353404052, 6.331612867284015955, 455.0000000000000568 ) ) ;
#818 = VECTOR ( 'NONE', #43071, 1000.000000000000000 ) ;
#820 = FACE_OUTER_BOUND ( 'NONE', #25377, .T. ) ;
#821 = ORIENTED_EDGE ( 'NONE', *, *, #16313, .T. ) ;
#822 = ADVANCED_FACE ( 'NONE', ( #57369 ), #66756, .F. ) ;
#823 = CIRCLE ( 'NONE', #22260, 0.1999999999999987899 ) ;
#824 = VECTOR ( 'NONE', #5850, 1000.000000000000000 ) ;
#825 =( GEOMETRIC_REPRESENTATION_CONTEXT ( 3 ) GLOBAL_UNCERTAINTY_ASSIGNED_CONTEXT ( ( #21060 ) ) GLOBAL_UNIT_ASSIGNED_CONTEXT ( ( #4006, #36892, #47144 ) ) REPRESENTATION_CONTEXT ( 'NONE', 'WORKASPACE' ) );
#826 = DIRECTION ( 'NONE',  ( 1.000000000000000000, 0.000000000000000000, 0.000000000000000000 ) ) ;
#827 = EDGE_CURVE ( 'NONE', #44516, #18842, #55470, .T. ) ;
#829 = VERTEX_POINT ( 'NONE', #69030 ) ;
#828 = CARTESIAN_POINT ( 'NONE',  ( 7.250000000000005329, 7.250000000000000888, -15.50000000000000000 ) ) ;
#830 = ORIENTED_EDGE ( 'NONE', *, *, #51327, .T. ) ;
#831 = FACE_OUTER_BOUND ( 'NONE', #58240, .T. ) ;
#832 = AXIS2_PLACEMENT_3D ( 'NONE', #15080, #68822, #58575 ) ;
#833 = CARTESIAN_POINT ( 'NONE',  ( 8.250000000000005329, -7.249999999999998224, -20.50000000000000000 ) ) ;
#834 = VECTOR ( 'NONE', #69668, 1000.000000000000000 ) ;
#835 = PLANE ( 'NONE',  #56604 ) ;
#836 = CARTESIAN_POINT ( 'NONE',  ( 16.75000000000000000, -0.2038245569916320166, 23.22168783648699986 ) ) ;
#837 = LINE ( 'NONE', #29752, #22571 ) ;
#838 = AXIS2_PLACEMENT_3D ( 'NONE', #32473, #4555, #64989 ) ;
#839 = ADVANCED_FACE ( 'NONE', ( #26252 ), #63738, .T. ) ;
#840 = EDGE_LOOP ( 'NONE', ( #34414, #10179, #35438, #60528 ) ) ;
#841 = CARTESIAN_POINT ( 'NONE',  ( 277.1811023147819810, -20.65270074880750428, -17.15270074880750784 ) ) ;
#843 = ORIENTED_EDGE ( 'NONE', *, *, #23067, .F. ) ;
#842 = LINE ( 'NONE', #42642, #9618 ) ;
#844 = VECTOR ( 'NONE', #58657, 1000.000000000000000 ) ;
#845 = LINE ( 'NONE', #43946, #45658 ) ;
#846 = DIRECTION ( 'NONE',  ( 0.000000000000000000, 1.000000000000000000, 0.000000000000000000 ) ) ;
#847 = EDGE_CURVE ( 'NONE', #21320, #24963, #58871, .T. ) ;
#848 = LINE ( 'NONE', #483, #11059 ) ;
#849 = ADVANCED_FACE ( 'NONE', ( #36875 ), #67886, .F. ) ;
#850 = LINE ( 'NONE', #43258, #19324 ) ;
#851 = CARTESIAN_POINT ( 'NONE',  ( 30.00000000000000000, -16.28999999999710369, -15.00000000000794920 ) ) ;
#852 = EDGE_CURVE ( 'NONE', #48338, #31486, #54371, .T. ) ;
#853 = ORIENTED_EDGE ( 'NONE', *, *, #17034, .T. ) ;
#854 = EDGE_CURVE ( 'NONE', #18488, #28131, #47123, .T. ) ;
#855 = EDGE_CURVE ( 'NONE', #46179, #68965, #3278, .T. ) ;
#856 = VERTEX_POINT ( 'NONE', #64779 ) ;
#857 = PLANE ( 'NONE',  #53952 ) ;
#858 = CARTESIAN_POINT ( 'NONE',  ( 6.358413763958946419, 4.706725378239151603, 54.00000000000000711 ) ) ;
#859 = EDGE_CURVE ( 'NONE', #63319, #31475, #10678, .T. ) ;
#860 = ORIENTED_EDGE ( 'NONE', *, *, #23793, .F. ) ;
#861 = EDGE_CURVE ( 'NONE', #40609, #24879, #59816, .T. ) ;
#862 = DIRECTION ( 'NONE',  ( 0.000000000000000000, 0.000000000000000000, 1.000000000000000000 ) ) ;
#863 = CARTESIAN_POINT ( 'NONE',  ( -9.249999999999998224, 8.250000000000001776, 5.000000000000000000 ) ) ;
#864 = AXIS2_PLACEMENT_3D ( 'NONE', #67353, #65696, #3001 ) ;
#865 = EDGE_LOOP ( 'NONE', ( #51644, #64448, #69573, #67536 ) ) ;
#866 = FACE_OUTER_BOUND ( 'NONE', #3479, .T. ) ;
#867 = CARTESIAN_POINT ( 'NONE',  ( -7.955476262117259445, 9.547976262117179758, 26.00000000000000711 ) ) ;
#868 = VERTEX_POINT ( 'NONE', #37910 ) ;
#869 = LINE ( 'NONE', #32332, #41210 ) ;
#870 = CARTESIAN_POINT ( 'NONE',  ( 30.00000000000000000, -9.454754784057099570, -17.53999999999999915 ) ) ;
#871 = VECTOR ( 'NONE', #27780, 1000.000000000000000 ) ;
#872 = CIRCLE ( 'NONE', #32458, 0.5999999999999989786 ) ;
#873 = DIRECTION ( 'NONE',  ( -1.000000000000000000, 0.000000000000000000, 0.000000000000000000 ) ) ;
#874 = CARTESIAN_POINT ( 'NONE',  ( 15.50000000000000000, -2.500000000000000000, -21.05662432702600029 ) ) ;
#875 = EDGE_CURVE ( 'NONE', #38341, #57811, #5399, .T. ) ;
#876 = EDGE_LOOP ( 'NONE', ( #22779, #36516, #11658, #58619 ) ) ;
#878 = ORIENTED_EDGE ( 'NONE', *, *, #43600, .T. ) ;
#877 = DIRECTION ( 'NONE',  ( 1.000000000000000000, 0.000000000000000000, 0.000000000000000000 ) ) ;
#879 = EDGE_CURVE ( 'NONE', #24754, #25574, #42511, .T. ) ;
#880 = CIRCLE ( 'NONE', #44900, 1.929199999999998028 ) ;
#881 = AXIS2_PLACEMENT_3D ( 'NONE', #32979, #11408, #38971 ) ;
#882 = CARTESIAN_POINT ( 'NONE',  ( -4.734785091273957747, 6.606374702650051667, 455.0000000000000568 ) ) ;
#883 = PRODUCT_DEFINITION_FORMATION_WITH_SPECIFIED_SOURCE ( 'ANY', '', #35679, .NOT_KNOWN. ) ;
#884 = DIRECTION ( 'NONE',  ( 0.000000000000000000, -1.000000000000000000, 0.000000000000000000 ) ) ;
#885 = FACE_OUTER_BOUND ( 'NONE', #64182, .T. ) ;
#886 = ORIENTED_EDGE ( 'NONE', *, *, #67563, .F. ) ;
#887 = AXIS2_PLACEMENT_3D ( 'NONE', #13239, #40098, #8984 ) ;
#889 = DIRECTION ( 'NONE',  ( 3.491481338843132961E-15, 1.000000000000000000, 0.000000000000000000 ) ) ;
#888 = CIRCLE ( 'NONE', #18921, 1.000000000000000000 ) ;
#890 = DIRECTION ( 'NONE',  ( -0.000000000000000000, 3.673940397442059868E-16, -1.000000000000000000 ) ) ;
#891 = ORIENTED_EDGE ( 'NONE', *, *, #39004, .T. ) ;
#892 = ADVANCED_FACE ( 'NONE', ( #48172 ), #42853, .T. ) ;
#893 = ORIENTED_EDGE ( 'NONE', *, *, #55404, .T. ) ;
#894 = EDGE_LOOP ( 'NONE', ( #48430, #3497, #17008, #60516 ) ) ;
#895 = CARTESIAN_POINT ( 'NONE',  ( 5.393625297349890602, 7.252248008019372527, 195.0000000000000284 ) ) ;
#896 = FACE_OUTER_BOUND ( 'NONE', #41303, .T. ) ;
#897 = LINE ( 'NONE', #65568, #43887 ) ;
#898 = ORIENTED_EDGE ( 'NONE', *, *, #30137, .F. ) ;
#899 = ORIENTED_EDGE ( 'NONE', *, *, #69732, .T. ) ;
#900 = ORIENTED_EDGE ( 'NONE', *, *, #47319, .T. ) ;
#901 = DIRECTION ( 'NONE',  ( -1.000000000000000000, 0.000000000000000000, 0.000000000000000000 ) ) ;
#902 = VERTEX_POINT ( 'NONE', #65471 ) ;
#903 = VERTEX_POINT ( 'NONE', #11031 ) ;
#904 = ORIENTED_EDGE ( 'NONE', *, *, #11775, .T. ) ;
#905 = EDGE_LOOP ( 'NONE', ( #8696, #17992, #23017, #20153 ) ) ;
#906 = DIRECTION ( 'NONE',  ( 0.000000000000000000, 0.000000000000000000, 1.000000000000000000 ) ) ;
#908 = EDGE_LOOP ( 'NONE', ( #65645, #15970, #35262, #63312 ) ) ;
#907 = DIRECTION ( 'NONE',  ( -0.000000000000000000, 3.673940397442059868E-16, -1.000000000000000000 ) ) ;
#909 = EDGE_CURVE ( 'NONE', #50899, #60848, #15648, .T. ) ;
#910 = CARTESIAN_POINT ( 'NONE',  ( 30.00000000000000000, -16.64230188589299786, -14.64519951917100116 ) ) ;
#911 = FACE_OUTER_BOUND ( 'NONE', #18961, .T. ) ;
#912 = CARTESIAN_POINT ( 'NONE',  ( -7.261609891743268541, -8.000000000000000000, 5.000000000000000000 ) ) ;
#913 = AXIS2_PLACEMENT_3D ( 'NONE', #51344, #30135, #56304 ) ;
#914 = ADVANCED_FACE ( 'NONE', ( #64433 ), #11706, .F. ) ;
#915 = EDGE_LOOP ( 'NONE', ( #60259, #42478, #33687, #25586 ) ) ;
#916 = EDGE_CURVE ( 'NONE', #53994, #5435, #428, .T. ) ;
#917 = CARTESIAN_POINT ( 'NONE',  ( -10.30047626211725742, 3.842976262117182351, 54.00000000000000711 ) ) ;
#918 = CARTESIAN_POINT ( 'NONE',  ( 6.665817930929288870, 7.342976262117195674, 54.00000000000000711 ) ) ;
#919 = ADVANCED_FACE ( 'NONE', ( #58782 ), #22348, .F. ) ;
#920 = ORIENTED_EDGE ( 'NONE', *, *, #10649, .T. ) ;
#921 = LINE ( 'NONE', #10807, #30327 ) ;
#922 = AXIS2_PLACEMENT_3D ( 'NONE', #63291, #58689, #9198 ) ;
#923 = DIRECTION ( 'NONE',  ( 0.000000000000000000, 0.000000000000000000, -1.000000000000000000 ) ) ;
#924 = PLANE ( 'NONE',  #11913 ) ;
#925 = ORIENTED_EDGE ( 'NONE', *, *, #48482, .F. ) ;
#926 = CARTESIAN_POINT ( 'NONE',  ( 275.5000000000000000, -42.50000000000000000, 26.50000000000000000 ) ) ;
#927 = AXIS2_PLACEMENT_3D ( 'NONE', #15351, #36558, #36936 ) ;
#928 = VECTOR ( 'NONE', #4450, 1000.000000000000000 ) ;
#929 = DIRECTION ( 'NONE',  ( -0.000000000000000000, 3.673940397442059868E-16, -1.000000000000000000 ) ) ;
#930 = DIRECTION ( 'NONE',  ( 9.912705577010344285E-15, 1.000000000000000000, 0.000000000000000000 ) ) ;
#931 = EDGE_CURVE ( 'NONE', #9404, #31249, #5735, .T. ) ;
#932 = CARTESIAN_POINT ( 'NONE',  ( 5.257023737882801306, 5.242976262117200470, 54.00000000000000711 ) ) ;
#933 = DIRECTION ( 'NONE',  ( -1.836970198721029934E-16, 1.836970198721036344E-16, -1.000000000000000000 ) ) ;
#934 = CARTESIAN_POINT ( 'NONE',  ( -9.404046420174067222, -1.866219381641389674, 195.0000000000000284 ) ) ;
#935 = DIRECTION ( 'NONE',  ( -1.000000000000000000, 0.000000000000000000, 0.000000000000000000 ) ) ;
#936 = LINE ( 'NONE', #5876, #27757 ) ;
#937 = VECTOR ( 'NONE', #53202, 1000.000000000000114 ) ;
#938 = VERTEX_POINT ( 'NONE', #16694 ) ;
#939 = CARTESIAN_POINT ( 'NONE',  ( 158.8349105750994568, -35.83962462487175316, 5.000000000000000000 ) ) ;
#940 = PLANE ( 'NONE',  #55617 ) ;
#941 = CARTESIAN_POINT ( 'NONE',  ( 9.737023737882783081, 3.667976262117152775, 54.00000000000000711 ) ) ;
#942 = CARTESIAN_POINT ( 'NONE',  ( 9.690000000000001279, 9.690000000000001279, -4.250000000000000000 ) ) ;
#943 = ORIENTED_EDGE ( 'NONE', *, *, #45066, .T. ) ;
#944 = CARTESIAN_POINT ( 'NONE',  ( 28.90000000000000213, -0.1999999999911430404, -8.864436962241481021E-12 ) ) ;
#945 = FACE_OUTER_BOUND ( 'NONE', #29269, .T. ) ;
#946 = PLANE ( 'NONE',  #16450 ) ;
#947 = DIRECTION ( 'NONE',  ( 0.000000000000000000, 0.000000000000000000, 1.000000000000000000 ) ) ;
#948 = CARTESIAN_POINT ( 'NONE',  ( -23.75054448485400016, -15.50000000000000000, -25.53140320652400064 ) ) ;
#949 = ADVANCED_FACE ( 'NONE', ( #38260 ), #49211, .F. ) ;
#950 = ORIENTED_EDGE ( 'NONE', *, *, #46963, .T. ) ;
#951 = EDGE_CURVE ( 'NONE', #35648, #2273, #6897, .T. ) ;
#952 = ORIENTED_EDGE ( 'NONE', *, *, #56490, .T. ) ;
#953 = CARTESIAN_POINT ( 'NONE',  ( 3.006483450353407250, 7.415254214038215608, 455.0000000000000568 ) ) ;
#954 = LINE ( 'NONE', #38420, #18746 ) ;
#955 = VECTOR ( 'NONE', #42136, 1000.000000000000000 ) ;
#956 = ORIENTED_EDGE ( 'NONE', *, *, #21730, .F. ) ;
#957 = DIRECTION ( 'NONE',  ( 1.047444401652940007E-14, 1.000000000000000000, 1.836970198721029934E-16 ) ) ;
#958 = ORIENTED_EDGE ( 'NONE', *, *, #875, .F. ) ;
#959 = LINE ( 'NONE', #22850, #22115 ) ;
#960 = ORIENTED_EDGE ( 'NONE', *, *, #2716, .F. ) ;
#961 = VERTEX_POINT ( 'NONE', #49550 ) ;
#962 = PLANE ( 'NONE',  #48707 ) ;
#963 = ORIENTED_EDGE ( 'NONE', *, *, #20143, .F. ) ;
#964 = DIRECTION ( 'NONE',  ( -7.665540703601096574E-15, -1.000000000000000000, -3.673940397442059868E-16 ) ) ;
#965 = VECTOR ( 'NONE', #30411, 1000.000000000000000 ) ;
#966 = FACE_OUTER_BOUND ( 'NONE', #3399, .T. ) ;
#967 = PLANE ( 'NONE',  #5428 ) ;
#968 = ORIENTED_EDGE ( 'NONE', *, *, #62086, .T. ) ;
#969 = ORIENTED_EDGE ( 'NONE', *, *, #8252, .F. ) ;
#970 = LINE ( 'NONE', #38776, #59466 ) ;
#971 = VECTOR ( 'NONE', #50877, 1000.000000000000000 ) ;
#972 = CARTESIAN_POINT ( 'NONE',  ( 15.50000000000000000, -1.037157890325000054, -19.00000000000000000 ) ) ;
#973 = ORIENTED_EDGE ( 'NONE', *, *, #16758, .F. ) ;
#974 = VERTEX_POINT ( 'NONE', #43892 ) ;
#975 = ORIENTED_EDGE ( 'NONE', *, *, #64139, .T. ) ;
#976 = DIRECTION ( 'NONE',  ( 0.000000000000000000, 0.000000000000000000, 1.000000000000000000 ) ) ;
#978 = ORIENTED_EDGE ( 'NONE', *, *, #3877, .F. ) ;
#977 = DIRECTION ( 'NONE',  ( 0.000000000000000000, 0.000000000000000000, 1.000000000000000000 ) ) ;
#979 = AXIS2_PLACEMENT_3D ( 'NONE', #1671, #6642, #49087 ) ;
#980 = EDGE_CURVE ( 'NONE', #40956, #37986, #10339, .T. ) ;
#981 = LINE ( 'NONE', #11554, #670 ) ;
#982 = DIRECTION ( 'NONE',  ( -0.000000000000000000, 1.000000000000000000, -0.000000000000000000 ) ) ;
#983 = ORIENTED_EDGE ( 'NONE', *, *, #34081, .F. ) ;
#984 = ORIENTED_EDGE ( 'NONE', *, *, #42876, .T. ) ;
#985 = EDGE_CURVE ( 'NONE', #67402, #14886, #60148, .T. ) ;
#986 = EDGE_CURVE ( 'NONE', #22607, #46315, #61093, .T. ) ;
#987 = EDGE_CURVE ( 'NONE', #52737, #4257, #6425, .T. ) ;
#988 = DIRECTION ( 'NONE',  ( 0.000000000000000000, 1.000000000000000000, 1.880440247955360336E-12 ) ) ;
#989 = CARTESIAN_POINT ( 'NONE',  ( 8.835729544836338434, -8.144523737882822800, 54.00000000000000711 ) ) ;
#990 = EDGE_CURVE ( 'NONE', #32081, #28477, #18203, .T. ) ;
#991 = EDGE_CURVE ( 'NONE', #24393, #37044, #28320, .T. ) ;
#992 = VERTEX_POINT ( 'NONE', #55548 ) ;
#993 = EDGE_CURVE ( 'NONE', #54687, #42154, #12053, .T. ) ;
#994 = DIRECTION ( 'NONE',  ( -1.053224967557348291E-14, -1.000000000000000000, 0.000000000000000000 ) ) ;
#995 = LINE ( 'NONE', #67059, #3067 ) ;
#997 = VERTEX_POINT ( 'NONE', #28668 ) ;
#996 = CYLINDRICAL_SURFACE ( 'NONE', #17307, 3.499999999999853895 ) ;
#998 = ORIENTED_EDGE ( 'NONE', *, *, #30275, .F. ) ;
#999 = LINE ( 'NONE', #23231, #47913 ) ;
#1000 = DIRECTION ( 'NONE',  ( 1.000000000000000000, -5.981805089575194965E-17, 0.000000000000000000 ) ) ;
#1001 = LINE ( 'NONE', #11920, #10971 ) ;
#1002 = PLANE ( 'NONE',  #36242 ) ;
#1003 = AXIS2_PLACEMENT_3D ( 'NONE', #69133, #46856, #24949 ) ;
#1004 = CARTESIAN_POINT ( 'NONE',  ( -9.293516549646827940, -10.92648345035338764, 455.0000000000000568 ) ) ;
#1005 = VERTEX_POINT ( 'NONE', #2144 ) ;
#1006 = DIRECTION ( 'NONE',  ( 1.000000000000000000, -2.135044278125299371E-15, -7.844025423732059533E-31 ) ) ;
#1007 = PLANE ( 'NONE',  #27095 ) ;
#1008 = SURFACE_STYLE_USAGE ( .BOTH. , #66721 ) ;
#1009 = VECTOR ( 'NONE', #69897, 1000.000000000000114 ) ;
#1010 = DIRECTION ( 'NONE',  ( -0.000000000000000000, -0.000000000000000000, -1.000000000000000000 ) ) ;
#1011 = LINE ( 'NONE', #46125, #12079 ) ;
#1012 = DIRECTION ( 'NONE',  ( 1.000000000000000000, -0.000000000000000000, -0.000000000000000000 ) ) ;
#1013 = LINE ( 'NONE', #60730, #37520 ) ;
#1014 = AXIS2_PLACEMENT_3D ( 'NONE', #63250, #5857, #48299 ) ;
#1015 = DIRECTION ( 'NONE',  ( -1.000000000000000000, 0.000000000000000000, 0.000000000000000000 ) ) ;
#1016 = ORIENTED_EDGE ( 'NONE', *, *, #15929, .T. ) ;
#1017 = CARTESIAN_POINT ( 'NONE',  ( -11.19000000000000128, -11.25000000000000000, -5.000000000000000000 ) ) ;
#1018 = LINE ( 'NONE', #27529, #5657 ) ;
#1019 = ORIENTED_EDGE ( 'NONE', *, *, #9468, .F. ) ;
#1020 = DIRECTION ( 'NONE',  ( 1.000000000000000000, -0.000000000000000000, -0.000000000000000000 ) ) ;
#1021 = LINE ( 'NONE', #7329, #52709 ) ;
#1022 = CIRCLE ( 'NONE', #10201, 1.999999999999315436 ) ;
#1023 = LINE ( 'NONE', #53727, #59201 ) ;
#1024 = CARTESIAN_POINT ( 'NONE',  ( 52.83090410532631864, 61.65740854044500452, 0.000000000000000000 ) ) ;
#1025 = CARTESIAN_POINT ( 'NONE',  ( -30.00000000000000000, -9.487228132326899654, 12.50000000000000000 ) ) ;
#1026 = AXIS2_PLACEMENT_3D ( 'NONE', #14029, #61406, #51523 ) ;
#1027 = FACE_OUTER_BOUND ( 'NONE', #62770, .T. ) ;
#1028 = EDGE_CURVE ( 'NONE', #14072, #47780, #49890, .T. ) ;
#1029 = VERTEX_POINT ( 'NONE', #12734 ) ;
#1030 = CARTESIAN_POINT ( 'NONE',  ( -4.135079735113203370, -3.677663764522608236, 26.00000000000000711 ) ) ;
#1031 = VERTEX_POINT ( 'NONE', #18051 ) ;
#1032 = ADVANCED_FACE ( 'NONE', ( #60837 ), #45267, .T. ) ;
#1033 = LINE ( 'NONE', #33190, #57372 ) ;
#1034 = ADVANCED_FACE ( 'NONE', ( #33964 ), #61177, .T. ) ;
#1035 = AXIS2_PLACEMENT_3D ( 'NONE', #17679, #56207, #51240 ) ;
#1036 = ADVANCED_FACE ( 'NONE', ( #67193 ), #22806, .F. ) ;
#1037 = DIRECTION ( 'NONE',  ( 0.000000000000000000, -1.000000000000000000, 0.000000000000000000 ) ) ;
#1038 = DIRECTION ( 'NONE',  ( 0.000000000000000000, 0.000000000000000000, 1.000000000000000000 ) ) ;
#1039 = ORIENTED_EDGE ( 'NONE', *, *, #61435, .F. ) ;
#1040 = VERTEX_POINT ( 'NONE', #39957 ) ;
#1041 = CARTESIAN_POINT ( 'NONE',  ( -7.813516549646711162, 11.77351654964660277, 455.0000000000000568 ) ) ;
#1042 = ORIENTED_EDGE ( 'NONE', *, *, #49305, .F. ) ;
#1043 = VERTEX_POINT ( 'NONE', #33633 ) ;
#1044 = PLANE ( 'NONE',  #51872 ) ;
#1045 = DIRECTION ( 'NONE',  ( -0.000000000000000000, 1.000000000000000000, -0.000000000000000000 ) ) ;
#1046 = FACE_OUTER_BOUND ( 'NONE', #30946, .T. ) ;
#1047 = VERTEX_POINT ( 'NONE', #12389 ) ;
#1048 = CARTESIAN_POINT ( 'NONE',  ( 283.0000000000000568, -39.80000000000000426, -8.400000000000000355 ) ) ;
#1050 = LINE ( 'NONE', #38193, #15255 ) ;
#1049 = CARTESIAN_POINT ( 'NONE',  ( -10.03972626211731978, -8.930623737882752877, 54.00000000000000711 ) ) ;
#1051 = ORIENTED_EDGE ( 'NONE', *, *, #66369, .F. ) ;
#1053 = ORIENTED_EDGE ( 'NONE', *, *, #19173, .F. ) ;
#1052 = DIRECTION ( 'NONE',  ( -1.836970198721029934E-16, -1.836970198721010706E-16, 1.000000000000000000 ) ) ;
#1054 = ORIENTED_EDGE ( 'NONE', *, *, #39987, .F. ) ;
#1055 = AXIS2_PLACEMENT_3D ( 'NONE', #65789, #64755, #5720 ) ;
#1056 = CARTESIAN_POINT ( 'NONE',  ( -11.00000000000000000, -11.50000000000100009, -15.00000000000084910 ) ) ;
#1057 = EDGE_CURVE ( 'NONE', #68976, #11076, #69099, .T. ) ;
#1058 = DIRECTION ( 'NONE',  ( 0.000000000000000000, 3.673940397442059868E-16, -1.000000000000000000 ) ) ;
#1059 = ORIENTED_EDGE ( 'NONE', *, *, #53222, .F. ) ;
#1060 = ORIENTED_EDGE ( 'NONE', *, *, #2553, .T. ) ;
#1061 = AXIS2_PLACEMENT_3D ( 'NONE', #24470, #41423, #61936 ) ;
#1062 = DIRECTION ( 'NONE',  ( -0.000000000000000000, 1.000000000000000000, -0.000000000000000000 ) ) ;
#1063 = CARTESIAN_POINT ( 'NONE',  ( 15.50000000000000000, -0.1999999999999999556, -22.50000000000000000 ) ) ;
#1064 = ORIENTED_EDGE ( 'NONE', *, *, #26942, .F. ) ;
#1065 = AXIS2_PLACEMENT_3D ( 'NONE', #21415, #31694, #15767 ) ;
#1066 = DIRECTION ( 'NONE',  ( -1.836970198721029934E-16, 1.836970198721036344E-16, -1.000000000000000000 ) ) ;
#1067 = DIRECTION ( 'NONE',  ( 1.000000000000000000, 0.000000000000000000, 0.000000000000000000 ) ) ;
#1068 = FACE_OUTER_BOUND ( 'NONE', #61139, .T. ) ;
#1069 = ADVANCED_FACE ( 'NONE', ( #44930 ), #23709, .F. ) ;
#1070 = ORIENTED_EDGE ( 'NONE', *, *, #5352, .T. ) ;
#1071 = AXIS2_PLACEMENT_3D ( 'NONE', #24574, #15367, #42221 ) ;
#1072 = EDGE_CURVE ( 'NONE', #28664, #4772, #40327, .T. ) ;
#1073 = CARTESIAN_POINT ( 'NONE',  ( -8.250000000000000000, 7.250000000000001776, -18.00000000000000000 ) ) ;
#1074 = DIRECTION ( 'NONE',  ( 1.000000000000000000, -0.000000000000000000, 0.000000000000000000 ) ) ;
#1076 = ORIENTED_EDGE ( 'NONE', *, *, #25942, .T. ) ;
#1075 = CARTESIAN_POINT ( 'NONE',  ( -7.450000000000001954, 0.000000000000000000, -19.50000000000000000 ) ) ;
#1078 = ORIENTED_EDGE ( 'NONE', *, *, #7206, .F. ) ;
#1077 = CARTESIAN_POINT ( 'NONE',  ( 48.83288643746762148, -0.7500000000000002220, 3.758927509733821726 ) ) ;
#1079 = CARTESIAN_POINT ( 'NONE',  ( 41.09999999999999432, -14.06939075806900163, 20.80000000000000426 ) ) ;
#1080 = AXIS2_PLACEMENT_3D ( 'NONE', #28442, #50013, #34091 ) ;
#1081 = DIRECTION ( 'NONE',  ( -1.000000000000000000, 0.000000000000000000, 0.000000000000000000 ) ) ;
#1082 = DIRECTION ( 'NONE',  ( 0.000000000000000000, 0.000000000000000000, 1.000000000000000000 ) ) ;
#1083 = DIRECTION ( 'NONE',  ( -1.000000000000000000, 0.000000000000000000, 0.000000000000000000 ) ) ;
#1084 = DIRECTION ( 'NONE',  ( 0.000000000000000000, 0.000000000000000000, -1.000000000000000000 ) ) ;
#1085 = FACE_BOUND ( 'NONE', #67725, .T. ) ;
#1086 = ORIENTED_EDGE ( 'NONE', *, *, #68428, .T. ) ;
#1087 = FACE_OUTER_BOUND ( 'NONE', #44944, .T. ) ;
#1089 = ORIENTED_EDGE ( 'NONE', *, *, #21994, .T. ) ;
#1088 = LINE ( 'NONE', #64406, #5175 ) ;
#1091 = ORIENTED_EDGE ( 'NONE', *, *, #28712, .T. ) ;
#1090 = PLANE ( 'NONE',  #16351 ) ;
#1092 = CARTESIAN_POINT ( 'NONE',  ( 29.25000000000000000, -5.200000000000001066, -11.75000000000000000 ) ) ;
#1093 = CARTESIAN_POINT ( 'NONE',  ( 29.50000000000000355, -11.70000000000000284, 11.00000000000000000 ) ) ;
#1094 = ORIENTED_EDGE ( 'NONE', *, *, #27274, .F. ) ;
#1095 = LINE ( 'NONE', #62, #16198 ) ;
#1096 = CARTESIAN_POINT ( 'NONE',  ( 283.0000000000000568, -23.70411739045900390, 12.50000000000000000 ) ) ;
#1097 = ORIENTED_EDGE ( 'NONE', *, *, #7601, .T. ) ;
#1098 = DIRECTION ( 'NONE',  ( 1.836970198721029934E-16, 1.836970198721010706E-16, -1.000000000000000000 ) ) ;
#1099 = DIRECTION ( 'NONE',  ( 0.000000000000000000, 0.000000000000000000, 1.000000000000000000 ) ) ;
#1100 = CYLINDRICAL_SURFACE ( 'NONE', #41565, 0.1999999999999987899 ) ;
#1101 = LINE ( 'NONE', #28304, #13515 ) ;
#1102 = AXIS2_PLACEMENT_3D ( 'NONE', #7957, #29532, #3368 ) ;
#1103 = AXIS2_PLACEMENT_3D ( 'NONE', #34668, #8490, #13452 ) ;
#1104 = DIRECTION ( 'NONE',  ( 1.836970198721029934E-16, 1.836970198721010706E-16, -1.000000000000000000 ) ) ;
#1105 = EDGE_LOOP ( 'NONE', ( #737, #1051, #33722, #17043 ) ) ;
#1106 = DIRECTION ( 'NONE',  ( 0.000000000000000000, 0.000000000000000000, -1.000000000000000000 ) ) ;
#1107 = EDGE_LOOP ( 'NONE', ( #6092, #33644, #51229, #28813 ) ) ;
#1108 = ORIENTED_EDGE ( 'NONE', *, *, #21032, .T. ) ;
#1109 = ADVANCED_FACE ( 'NONE', ( #55890 ), #39281, .F. ) ;
#1110 = CIRCLE ( 'NONE', #40610, 1.224999999999999423 ) ;
#1111 = CARTESIAN_POINT ( 'NONE',  ( 283.0000000000000568, -42.50000000000000000, -7.500000000000000000 ) ) ;
#1112 = CARTESIAN_POINT ( 'NONE',  ( 8.250000000000005329, -7.249999999999998224, -26.00000000000001066 ) ) ;
#1113 = EDGE_CURVE ( 'NONE', #62633, #46357, #23019, .T. ) ;
#1114 = VECTOR ( 'NONE', #19093, 1000.000000000000000 ) ;
#1115 = CARTESIAN_POINT ( 'NONE',  ( 10.05377373788281581, 8.916576262117182239, 54.00000000000000711 ) ) ;
#1116 = CARTESIAN_POINT ( 'NONE',  ( -1.620245201994373385, -8.241237374594328813, 54.00000000000000711 ) ) ;
#1117 = ORIENTED_EDGE ( 'NONE', *, *, #195, .F. ) ;
#1118 = ORIENTED_EDGE ( 'NONE', *, *, #34633, .F. ) ;
#1120 = ORIENTED_EDGE ( 'NONE', *, *, #57494, .F. ) ;
#1119 = CARTESIAN_POINT ( 'NONE',  ( -10.91351654964670637, 9.293516549646604119, 455.0000000000000568 ) ) ;
#1121 = VERTEX_POINT ( 'NONE', #61523 ) ;
#1122 = VECTOR ( 'NONE', #20226, 1000.000000000000000 ) ;
#1123 = DIRECTION ( 'NONE',  ( 0.000000000000000000, 0.000000000000000000, 1.000000000000000000 ) ) ;
#1124 = CARTESIAN_POINT ( 'NONE',  ( 11.50000000000000000, -11.50000000000100009, -15.00000000000084910 ) ) ;
#1125 = DIRECTION ( 'NONE',  ( -1.836970198721029934E-16, 1.836970198721036344E-16, -1.000000000000000000 ) ) ;
#1126 = DIRECTION ( 'NONE',  ( -0.000000000000000000, 1.000000000000000000, -0.000000000000000000 ) ) ;
#1127 = AXIS2_PLACEMENT_3D ( 'NONE', #13585, #57769, #40806 ) ;
#1129 = CARTESIAN_POINT ( 'NONE',  ( 0.000000000000000000, 17.79289321881347163, -20.50000000000002487 ) ) ;
#1128 = CARTESIAN_POINT ( 'NONE',  ( 10.92648345035337343, -9.306483450353493225, 455.0000000000000568 ) ) ;
#1130 = ORIENTED_EDGE ( 'NONE', *, *, #66026, .F. ) ;
#1132 = ORIENTED_EDGE ( 'NONE', *, *, #68198, .T. ) ;
#1131 = CARTESIAN_POINT ( 'NONE',  ( 41.09999999999999432, 13.66939075806899950, 20.80000000000000426 ) ) ;
#1133 = ORIENTED_EDGE ( 'NONE', *, *, #46290, .F. ) ;
#1134 = ORIENTED_EDGE ( 'NONE', *, *, #62305, .F. ) ;
#1135 = ADVANCED_FACE ( 'NONE', ( #13447 ), #29017, .T. ) ;
#1136 = CARTESIAN_POINT ( 'NONE',  ( 27.90000000000000213, -21.00000000000001421, -13.86939075806900945 ) ) ;
#1137 = DIRECTION ( 'NONE',  ( -1.000000000000000000, 0.000000000000000000, 0.000000000000000000 ) ) ;
#1138 = CARTESIAN_POINT ( 'NONE',  ( 6.501044194225443995, 2.617976262117186703, 54.00000000000000711 ) ) ;
#1139 = CIRCLE ( 'NONE', #58734, 9.300000000000002487 ) ;
#1140 = DIRECTION ( 'NONE',  ( 0.000000000000000000, -1.000000000000000000, 0.000000000000000000 ) ) ;
#1141 = VERTEX_POINT ( 'NONE', #34665 ) ;
#1142 = EDGE_LOOP ( 'NONE', ( #69661, #33730, #30512, #11876 ) ) ;
#1143 = CARTESIAN_POINT ( 'NONE',  ( -11.75000000000000000, -5.000000000000000000, 21.10805890929250239 ) ) ;
#1144 = DIRECTION ( 'NONE',  ( 0.000000000000000000, 0.000000000000000000, 1.000000000000000000 ) ) ;
#1145 = ORIENTED_EDGE ( 'NONE', *, *, #54162, .T. ) ;
#1146 = ORIENTED_EDGE ( 'NONE', *, *, #32037, .F. ) ;
#1147 = CARTESIAN_POINT ( 'NONE',  ( 14.50000000000000000, -0.5000000000000000000, -27.00000000000000000 ) ) ;
#1148 = CARTESIAN_POINT ( 'NONE',  ( -11.50000000000000000, -11.50000000000100009, -19.50000000000103739 ) ) ;
#1149 = AXIS2_PLACEMENT_3D ( 'NONE', #2658, #12561, #19280 ) ;
#1150 = VERTEX_POINT ( 'NONE', #35007 ) ;
#1151 = AXIS2_PLACEMENT_3D ( 'NONE', #37394, #52971, #63572 ) ;
#1152 = EDGE_CURVE ( 'NONE', #49918, #39966, #56583, .T. ) ;
#1153 = AXIS2_PLACEMENT_3D ( 'NONE', #46137, #13612, #29873 ) ;
#1154 = ADVANCED_FACE ( 'NONE', ( #29703 ), #30772, .T. ) ;
#1155 = CARTESIAN_POINT ( 'NONE',  ( -6.350872789121313922, -3.677663764522584255, 26.00000000000000711 ) ) ;
#1156 = EDGE_CURVE ( 'NONE', #55902, #66560, #52704, .T. ) ;
#1158 = VERTEX_POINT ( 'NONE', #31132 ) ;
#1157 = DIRECTION ( 'NONE',  ( 0.000000000000000000, 0.000000000000000000, 1.000000000000000000 ) ) ;
#1159 = ORIENTED_EDGE ( 'NONE', *, *, #22456, .T. ) ;
#1160 = VECTOR ( 'NONE', #55772, 1000.000000000000000 ) ;
#1161 = PLANE ( 'NONE',  #26470 ) ;
#1162 = FACE_OUTER_BOUND ( 'NONE', #57497, .T. ) ;
#1163 = EDGE_CURVE ( 'NONE', #46897, #43093, #9208, .T. ) ;
#1164 = CARTESIAN_POINT ( 'NONE',  ( 5.393625297349950110, 4.734785091273829849, 455.0000000000000568 ) ) ;
#1165 = CARTESIAN_POINT ( 'NONE',  ( -11.00000000000000000, -17.35230188589299871, 15.35019951917099945 ) ) ;
#1166 = PRODUCT_DEFINITION ( 'UNKNOWN', '', #16619, #28930 ) ;
#1167 = DIRECTION ( 'NONE',  ( 0.000000000000000000, -1.000000000000000000, 0.000000000000000000 ) ) ;
#1168 = ADVANCED_FACE ( 'NONE', ( #63657 ), #9917, .T. ) ;
#1169 = VECTOR ( 'NONE', #44683, 1000.000000000000000 ) ;
#1170 = ORIENTED_EDGE ( 'NONE', *, *, #7468, .F. ) ;
#1171 = LINE ( 'NONE', #44978, #64259 ) ;
#1172 = ADVANCED_FACE ( 'NONE', ( #68609 ), #20162, .F. ) ;
#1173 = VECTOR ( 'NONE', #30051, 1000.000000000000000 ) ;
#1175 = ORIENTED_EDGE ( 'NONE', *, *, #22784, .F. ) ;
#1174 = CARTESIAN_POINT ( 'NONE',  ( 10.62249899919920004, -53.81370849898476649, -17.50000000000000000 ) ) ;
#1176 = LINE ( 'NONE', #22729, #65952 ) ;
#1177 = CARTESIAN_POINT ( 'NONE',  ( -11.77351654964669336, -4.186483450353275515, 195.0000000000000284 ) ) ;
#1178 = CYLINDRICAL_SURFACE ( 'NONE', #52866, 0.1999999999999987899 ) ;
#1179 = CARTESIAN_POINT ( 'NONE',  ( 0.000000000000000000, -8.249999999999998224, -8.000000000000000000 ) ) ;
#1180 = AXIS2_PLACEMENT_3D ( 'NONE', #39575, #65093, #55169 ) ;
#1181 = VECTOR ( 'NONE', #42615, 1000.000000000000000 ) ;
#1182 = DIRECTION ( 'NONE',  ( -1.000000000000000000, 0.000000000000000000, 0.000000000000000000 ) ) ;
#1183 = ORIENTED_EDGE ( 'NONE', *, *, #37699, .F. ) ;
#1184 = ORIENTED_EDGE ( 'NONE', *, *, #68443, .T. ) ;
#1185 = CARTESIAN_POINT ( 'NONE',  ( 24.00000000000000000, -16.28999999999999915, 14.50000000000000000 ) ) ;
#1186 = CARTESIAN_POINT ( 'NONE',  ( 2.544523737882815162, 8.821682069070730492, 54.00000000000000711 ) ) ;
#1187 = ORIENTED_EDGE ( 'NONE', *, *, #58222, .F. ) ;
#1188 = VECTOR ( 'NONE', #4712, 1000.000000000000000 ) ;
#1189 = DIRECTION ( 'NONE',  ( 1.000000000000000000, -0.000000000000000000, 0.000000000000000000 ) ) ;
#1190 = EDGE_CURVE ( 'NONE', #3757, #43775, #51019, .T. ) ;
#1191 = VERTEX_POINT ( 'NONE', #4266 ) ;
#1192 = ORIENTED_EDGE ( 'NONE', *, *, #19802, .F. ) ;
#1193 = CARTESIAN_POINT ( 'NONE',  ( 23.48000000000000043, -15.50000000000000000, -26.00000000000000355 ) ) ;
#1194 = CARTESIAN_POINT ( 'NONE',  ( -17.00000000000000000, -16.64230188589299786, -14.64519951917100116 ) ) ;
#1195 = EDGE_LOOP ( 'NONE', ( #63285, #14361, #64812, #8946 ) ) ;
#1196 = DIRECTION ( 'NONE',  ( -0.000000000000000000, -0.000000000000000000, 1.000000000000000000 ) ) ;
#1197 = DIRECTION ( 'NONE',  ( 1.000000000000000000, 0.000000000000000000, 0.000000000000000000 ) ) ;
#1198 = DIRECTION ( 'NONE',  ( 0.000000000000000000, 1.000000000000000000, 0.000000000000000000 ) ) ;
#1199 = PLANE ( 'NONE',  #2400 ) ;
#1200 = VERTEX_POINT ( 'NONE', #41012 ) ;
#1201 = CIRCLE ( 'NONE', #29390, 3.499999999999041655 ) ;
#1203 = ORIENTED_EDGE ( 'NONE', *, *, #20044, .F. ) ;
#1202 = DIRECTION ( 'NONE',  ( 1.000000000000000000, -0.000000000000000000, -0.000000000000000000 ) ) ;
#1204 = CIRCLE ( 'NONE', #27204, 1.449999999999999956 ) ;
#1205 = DIRECTION ( 'NONE',  ( 0.000000000000000000, -1.000000000000000000, 0.000000000000000000 ) ) ;
#1206 = CARTESIAN_POINT ( 'NONE',  ( -6.822336235477489019, -6.364920264886855250, 54.00000000000000711 ) ) ;
#1207 = CARTESIAN_POINT ( 'NONE',  ( -29.50000000000000355, -11.50000000000000000, 19.00000000000000000 ) ) ;
#1208 = VERTEX_POINT ( 'NONE', #63300 ) ;
#1209 = AXIS2_PLACEMENT_3D ( 'NONE', #21962, #6056, #53118 ) ;
#1210 = LINE ( 'NONE', #30507, #44645 ) ;
#1211 = CARTESIAN_POINT ( 'NONE',  ( 290.0000000000000000, 0.000000000000000000, 3.232999999999965901 ) ) ;
#1212 = ORIENTED_EDGE ( 'NONE', *, *, #35563, .T. ) ;
#1213 = ORIENTED_EDGE ( 'NONE', *, *, #68292, .T. ) ;
#1214 = AXIS2_PLACEMENT_3D ( 'NONE', #27801, #65298, #22835 ) ;
#1215 = ORIENTED_EDGE ( 'NONE', *, *, #57311, .T. ) ;
#1216 = ADVANCED_FACE ( 'NONE', ( #51993 ), #13796, .T. ) ;
#1217 = LINE ( 'NONE', #22771, #19721 ) ;
#1218 = CARTESIAN_POINT ( 'NONE',  ( 13.00000000000000178, -15.50000000000000000, -20.05051025721700242 ) ) ;
#1219 = CARTESIAN_POINT ( 'NONE',  ( -7.250000000000000888, 7.250000000000001776, -22.50000000000000000 ) ) ;
#1220 = ORIENTED_EDGE ( 'NONE', *, *, #37017, .T. ) ;
#1222 = EDGE_CURVE ( 'NONE', #22220, #53770, #14862, .T. ) ;
#1221 = ORIENTED_EDGE ( 'NONE', *, *, #59660, .F. ) ;
#1223 = ORIENTED_EDGE ( 'NONE', *, *, #46884, .T. ) ;
#1225 = LINE ( 'NONE', #48975, #63309 ) ;
#1224 = VECTOR ( 'NONE', #7831, 1000.000000000000000 ) ;
#1226 = ORIENTED_EDGE ( 'NONE', *, *, #66324, .T. ) ;
#1227 = ADVANCED_FACE ( 'NONE', ( #14507 ), #58357, .T. ) ;
#1228 = ORIENTED_EDGE ( 'NONE', *, *, #64048, .T. ) ;
#1229 = EDGE_CURVE ( 'NONE', #15828, #25947, #67557, .T. ) ;
#1230 = ORIENTED_EDGE ( 'NONE', *, *, #3922, .F. ) ;
#1231 = VERTEX_POINT ( 'NONE', #56925 ) ;
#1232 = PLANE ( 'NONE',  #35006 ) ;
#1234 = ORIENTED_EDGE ( 'NONE', *, *, #63821, .T. ) ;
#1233 = CARTESIAN_POINT ( 'NONE',  ( 5.552858015815581361, -7.357023737882814274, 26.00000000000000000 ) ) ;
#1235 = CARTESIAN_POINT ( 'NONE',  ( -11.00000000000000000, -9.454754784057099570, -17.53999999999999915 ) ) ;
#1236 = DIRECTION ( 'NONE',  ( 0.000000000000000000, 0.000000000000000000, -1.000000000000000000 ) ) ;
#1237 = AXIS2_PLACEMENT_3D ( 'NONE', #42013, #69594, #37075 ) ;
#1238 = EDGE_CURVE ( 'NONE', #64203, #14678, #3587, .T. ) ;
#1239 = DIRECTION ( 'NONE',  ( 1.000000000000000000, -1.883404846338789915E-14, 1.836970198720995421E-16 ) ) ;
#1240 = EDGE_LOOP ( 'NONE', ( #28286, #25016, #26977, #63500 ) ) ;
#1241 = FACE_BOUND ( 'NONE', #47229, .T. ) ;
#1242 = LINE ( 'NONE', #22803, #31158 ) ;
#1243 = CARTESIAN_POINT ( 'NONE',  ( 10.00000000000000000, 18.00000000000000355, 21.00000000000000000 ) ) ;
#1244 = EDGE_CURVE ( 'NONE', #17331, #9620, #3201, .T. ) ;
#1245 = VERTEX_POINT ( 'NONE', #46323 ) ;
#1246 = PLANE ( 'NONE',  #58564 ) ;
#1247 = ADVANCED_FACE ( 'NONE', ( #67899 ), #19451, .F. ) ;
#1248 = DIRECTION ( 'NONE',  ( 0.000000000000000000, 0.000000000000000000, -1.000000000000000000 ) ) ;
#1249 = VECTOR ( 'NONE', #13838, 1000.000000000000114 ) ;
#1250 = DIRECTION ( 'NONE',  ( -0.000000000000000000, -0.000000000000000000, 1.000000000000000000 ) ) ;
#1251 = ORIENTED_EDGE ( 'NONE', *, *, #54904, .F. ) ;
#1253 = DIRECTION ( 'NONE',  ( 0.000000000000000000, -1.000000000000000000, -0.000000000000000000 ) ) ;
#1252 = VECTOR ( 'NONE', #4585, 1000.000000000000000 ) ;
#1254 = LINE ( 'NONE', #34102, #2536 ) ;
#1255 = CARTESIAN_POINT ( 'NONE',  ( -8.250000000000001776, 7.250000000000000888, -15.50000000000000000 ) ) ;
#1256 = VECTOR ( 'NONE', #44307, 1000.000000000000000 ) ;
#1257 = CIRCLE ( 'NONE', #52086, 1.000000000000000000 ) ;
#1258 = CARTESIAN_POINT ( 'NONE',  ( 47.00000000000000000, -0.7500000000000000000, 3.418698582794335028 ) ) ;
#1259 = CARTESIAN_POINT ( 'NONE',  ( 10.31452373788281562, -6.657023737882815873, 26.00000000000000000 ) ) ;
#1260 = DIRECTION ( 'NONE',  ( -0.000000000000000000, -1.000000000000000000, -0.000000000000000000 ) ) ;
#1261 = DIRECTION ( 'NONE',  ( -1.000000000000000000, 0.000000000000000000, 0.000000000000000000 ) ) ;
#1262 = DIRECTION ( 'NONE',  ( 0.000000000000000000, 0.7071067811865496822, 0.7071067811865454633 ) ) ;
#1263 = ORIENTED_EDGE ( 'NONE', *, *, #54330, .F. ) ;
#1264 = CARTESIAN_POINT ( 'NONE',  ( 7.250000000000005329, -7.249999999999998224, -22.50000000000000000 ) ) ;
#1265 = CARTESIAN_POINT ( 'NONE',  ( -7.250000000000001776, -7.249999999999998224, -15.50000000000000000 ) ) ;
#1266 = CIRCLE ( 'NONE', #20449, 0.5999999999999998668 ) ;
#1267 = DIRECTION ( 'NONE',  ( 0.000000000000000000, 0.000000000000000000, 1.000000000000000000 ) ) ;
#1268 = DIRECTION ( 'NONE',  ( -1.000000000000000000, 0.000000000000000000, 0.000000000000000000 ) ) ;
#1269 = ORIENTED_EDGE ( 'NONE', *, *, #4748, .T. ) ;
#1270 = DIRECTION ( 'NONE',  ( 1.000000000000000000, 0.000000000000000000, 0.000000000000000000 ) ) ;
#1271 = CYLINDRICAL_SURFACE ( 'NONE', #15837, 1.000000000000000000 ) ;
#1272 = DIRECTION ( 'NONE',  ( 1.000000000000000000, 0.000000000000000000, 0.000000000000000000 ) ) ;
#1273 = ADVANCED_FACE ( 'NONE', ( #25114 ), #46671, .T. ) ;
#1274 = LINE ( 'NONE', #5889, #51165 ) ;
#1275 = CARTESIAN_POINT ( 'NONE',  ( 2.706483450353419862, 10.91351654964658735, 455.0000000000000568 ) ) ;
#1276 = VERTEX_POINT ( 'NONE', #3906 ) ;
#1277 = EDGE_CURVE ( 'NONE', #59384, #6050, #25467, .T. ) ;
#1278 = DIRECTION ( 'NONE',  ( -1.000000000000000000, 0.000000000000000000, 0.000000000000000000 ) ) ;
#1279 = CIRCLE ( 'NONE', #3559, 0.5000000000009372503 ) ;
#1280 = DIRECTION ( 'NONE',  ( 0.000000000000000000, 0.000000000000000000, -1.000000000000000000 ) ) ;
#1281 = ORIENTED_EDGE ( 'NONE', *, *, #66042, .F. ) ;
#1282 = EDGE_CURVE ( 'NONE', #69741, #32938, #44251, .T. ) ;
#1283 = FACE_OUTER_BOUND ( 'NONE', #43184, .T. ) ;
#1284 = EDGE_CURVE ( 'NONE', #48776, #37166, #15907, .T. ) ;
#1285 = ORIENTED_EDGE ( 'NONE', *, *, #38363, .T. ) ;
#1286 = PLANE ( 'NONE',  #15354 ) ;
#1287 = ORIENTED_EDGE ( 'NONE', *, *, #46603, .T. ) ;
#1288 = EDGE_CURVE ( 'NONE', #48269, #20561, #46522, .T. ) ;
#1289 = ORIENTED_EDGE ( 'NONE', *, *, #15089, .F. ) ;
#1290 = DIRECTION ( 'NONE',  ( -1.000000000000000000, 0.000000000000000000, 0.000000000000000000 ) ) ;
#1291 = AXIS2_PLACEMENT_3D ( 'NONE', #46802, #14634, #58493 ) ;
#1292 = DIRECTION ( 'NONE',  ( 0.000000000000000000, 0.000000000000000000, -1.000000000000000000 ) ) ;
#1293 = FACE_OUTER_BOUND ( 'NONE', #53167, .T. ) ;
#1294 = DIRECTION ( 'NONE',  ( 0.000000000000000000, -1.000000000000000000, 0.000000000000000000 ) ) ;
#1295 = AXIS2_PLACEMENT_3D ( 'NONE', #68288, #9243, #30806 ) ;
#1296 = ORIENTED_EDGE ( 'NONE', *, *, #4827, .F. ) ;
#1297 = ADVANCED_FACE ( 'NONE', ( #32859 ), #64347, .F. ) ;
#1298 = VERTEX_POINT ( 'NONE', #54091 ) ;
#1299 = FACE_OUTER_BOUND ( 'NONE', #3983, .T. ) ;
#1300 = EDGE_CURVE ( 'NONE', #9609, #39844, #5648, .T. ) ;
#1301 = CARTESIAN_POINT ( 'NONE',  ( 4.206483450353343478, -11.12648345035337982, 195.0000000000000284 ) ) ;
#1302 = VERTEX_POINT ( 'NONE', #27959 ) ;
#1303 = ORIENTED_EDGE ( 'NONE', *, *, #34868, .T. ) ;
#1305 = ADVANCED_FACE ( 'NONE', ( #59733 ), #11279, .F. ) ;
#1304 = CIRCLE ( 'NONE', #61135, 0.5249999999999994671 ) ;
#1306 = ADVANCED_FACE ( 'NONE', ( #32167 ), #15577, .T. ) ;
#1307 = VERTEX_POINT ( 'NONE', #10946 ) ;
#1308 = DIRECTION ( 'NONE',  ( 0.000000000000000000, -0.7075259945833242137, 0.7066873191085842887 ) ) ;
#1309 = DIRECTION ( 'NONE',  ( 0.000000000000000000, 0.000000000000000000, 1.000000000000000000 ) ) ;
#1311 = VERTEX_POINT ( 'NONE', #21555 ) ;
#1310 = CARTESIAN_POINT ( 'NONE',  ( 283.0000000000000568, -25.60000000000000142, 15.10000000000000142 ) ) ;
#1312 = VECTOR ( 'NONE', #19189, 1000.000000000000000 ) ;
#1313 = EDGE_CURVE ( 'NONE', #1245, #29373, #256, .T. ) ;
#1314 = DIRECTION ( 'NONE',  ( -1.000000000000000000, 0.000000000000000000, 0.000000000000000000 ) ) ;
#1315 = DIRECTION ( 'NONE',  ( 1.000000000000000000, -0.000000000000000000, -0.000000000000000000 ) ) ;
#1316 = EDGE_LOOP ( 'NONE', ( #1706, #48717, #10061, #39619 ) ) ;
#1317 = ORIENTED_EDGE ( 'NONE', *, *, #31913, .T. ) ;
#1318 = ORIENTED_EDGE ( 'NONE', *, *, #5140, .F. ) ;
#1319 = CIRCLE ( 'NONE', #46434, 0.1749999999999989342 ) ;
#1320 = DIRECTION ( 'NONE',  ( 1.000000000000000000, -0.000000000000000000, 0.000000000000000000 ) ) ;
#1321 = DIRECTION ( 'NONE',  ( -1.053224967557348291E-14, -1.000000000000000000, 0.000000000000000000 ) ) ;
#1322 = EDGE_CURVE ( 'NONE', #33439, #58687, #16057, .T. ) ;
#1323 = CARTESIAN_POINT ( 'NONE',  ( 7.606483450353376696, 11.77351654964662053, 195.0000000000000284 ) ) ;
#1324 = EDGE_CURVE ( 'NONE', #31007, #4729, #59948, .T. ) ;
#1325 = DIRECTION ( 'NONE',  ( 0.000000000000000000, 0.000000000000000000, 1.000000000000000000 ) ) ;
#1326 = CARTESIAN_POINT ( 'NONE',  ( 6.344579767990823349, -8.406483450353396947, 195.0000000000000284 ) ) ;
#1327 = VECTOR ( 'NONE', #17482, 1000.000000000000000 ) ;
#1329 = ORIENTED_EDGE ( 'NONE', *, *, #11998, .F. ) ;
#1328 = FACE_OUTER_BOUND ( 'NONE', #32846, .T. ) ;
#1330 = ORIENTED_EDGE ( 'NONE', *, *, #63237, .T. ) ;
#1331 = CARTESIAN_POINT ( 'NONE',  ( 39.90000000000000568, 14.08845687959340154, -20.99999999999999645 ) ) ;
#1332 = CARTESIAN_POINT ( 'NONE',  ( 6.344579767990823349, -8.406483450353491094, 455.0000000000000568 ) ) ;
#1333 = CARTESIAN_POINT ( 'NONE',  ( 17.24945551514599984, -17.50000000000000000, 25.53140320652400064 ) ) ;
#1334 = DIRECTION ( 'NONE',  ( -1.084202172485501594E-14, -1.000000000000000000, 0.000000000000000000 ) ) ;
#1335 = CARTESIAN_POINT ( 'NONE',  ( 7.250000000000005329, 7.250000000000000888, -25.00000000000000000 ) ) ;
#1336 = VERTEX_POINT ( 'NONE', #22257 ) ;
#1337 = CARTESIAN_POINT ( 'NONE',  ( -7.250000000000000888, 7.250000000000001776, -12.00000000000000000 ) ) ;
#1338 = CARTESIAN_POINT ( 'NONE',  ( 6.657023737882818537, -9.912023737882819319, 54.00000000000000711 ) ) ;
#1339 = AXIS2_PLACEMENT_3D ( 'NONE', #35757, #36831, #19845 ) ;
#1340 = SURFACE_STYLE_FILL_AREA ( #17933 ) ;
#1341 = DIRECTION ( 'NONE',  ( -0.000000000000000000, 3.673940397442059868E-16, -1.000000000000000000 ) ) ;
#1342 = PRODUCT_DEFINITION_SHAPE ( 'NONE', 'NONE',  #69984 ) ;
#1343 = CIRCLE ( 'NONE', #12574, 4.000000000000000000 ) ;
#1344 = CARTESIAN_POINT ( 'NONE',  ( 7.000000000000000000, -21.00000000000000000, 0.000000000000000000 ) ) ;
#1345 = CARTESIAN_POINT ( 'NONE',  ( 14.25000000000000000, -0.2038245569916330158, 21.77831216351300014 ) ) ;
#1346 = CARTESIAN_POINT ( 'NONE',  ( 283.0000000000000568, -42.50000000000000000, -15.10000000000000142 ) ) ;
#1347 = ORIENTED_EDGE ( 'NONE', *, *, #34902, .T. ) ;
#1348 = CARTESIAN_POINT ( 'NONE',  ( -14.66242688423474227, -0.3152598339554810170, 21.54019739087905094 ) ) ;
#1349 = DIRECTION ( 'NONE',  ( 0.000000000000000000, -1.000000000000000000, -3.673940397442059868E-16 ) ) ;
#1350 = ORIENTED_EDGE ( 'NONE', *, *, #6171, .F. ) ;
#1351 = CARTESIAN_POINT ( 'NONE',  ( -6.467976262117274722, -5.257023737882803083, 26.00000000000000711 ) ) ;
#1352 = CIRCLE ( 'NONE', #39742, 25.39999999999999858 ) ;
#1353 = FACE_OUTER_BOUND ( 'NONE', #2216, .T. ) ;
#1354 = DIRECTION ( 'NONE',  ( 0.000000000000000000, 0.000000000000000000, 1.000000000000000000 ) ) ;
#1355 = CARTESIAN_POINT ( 'NONE',  ( -7.793516549646712477, 11.11351654964660085, 455.0000000000000568 ) ) ;
#1356 = LINE ( 'NONE', #38501, #62102 ) ;
#1357 = AXIS2_PLACEMENT_3D ( 'NONE', #2836, #24414, #25826 ) ;
#1358 = ADVANCED_FACE ( 'NONE', ( #58696 ), #48778, .F. ) ;
#1359 = CARTESIAN_POINT ( 'NONE',  ( 25.90000000000000213, 20.60000000000000142, 1.939442395502021001E-15 ) ) ;
#1360 = ORIENTED_EDGE ( 'NONE', *, *, #2181, .F. ) ;
#1361 = CARTESIAN_POINT ( 'NONE',  ( 49.00000000000000000, -0.1999999999911430404, -8.864436962241481021E-12 ) ) ;
#1362 = VERTEX_POINT ( 'NONE', #43461 ) ;
#1363 = EDGE_CURVE ( 'NONE', #17706, #30714, #5313, .T. ) ;
#1364 = LINE ( 'NONE', #33536, #69805 ) ;
#1365 = AXIS2_PLACEMENT_3D ( 'NONE', #30474, #52049, #14558 ) ;
#1366 = EDGE_CURVE ( 'NONE', #22769, #43177, #26876, .T. ) ;
#1367 = ADVANCED_FACE ( 'NONE', ( #38517 ), #10253, .T. ) ;
#1368 = FACE_OUTER_BOUND ( 'NONE', #6690, .T. ) ;
#1369 = VERTEX_POINT ( 'NONE', #53398 ) ;
#1370 = EDGE_CURVE ( 'NONE', #16386, #66031, #4950, .T. ) ;
#1371 = VERTEX_POINT ( 'NONE', #69662 ) ;
#1372 = EDGE_CURVE ( 'NONE', #67636, #34438, #55125, .T. ) ;
#1373 = DIRECTION ( 'NONE',  ( 0.000000000000000000, -0.7046037717806115097, 0.7096009616626348659 ) ) ;
#1374 = ORIENTED_EDGE ( 'NONE', *, *, #51278, .F. ) ;
#1375 = VERTEX_POINT ( 'NONE', #50147 ) ;
#1376 = DIRECTION ( 'NONE',  ( 0.7071067811865486830, 0.7071067811865464625, 0.000000000000000000 ) ) ;
#1377 = LINE ( 'NONE', #60762, #24532 ) ;
#1378 = CARTESIAN_POINT ( 'NONE',  ( -5.242976262117259978, 5.242976262117182706, 54.00000000000000711 ) ) ;
#1379 = ORIENTED_EDGE ( 'NONE', *, *, #7734, .F. ) ;
#1380 = LINE ( 'NONE', #33209, #39108 ) ;
#1382 = FACE_BOUND ( 'NONE', #14584, .T. ) ;
#1381 = CARTESIAN_POINT ( 'NONE',  ( 7.900000000000000355, -18.00000000000000355, 21.00000000000000000 ) ) ;
#1383 = ORIENTED_EDGE ( 'NONE', *, *, #19821, .T. ) ;
#1385 = VERTEX_POINT ( 'NONE', #50502 ) ;
#1384 = LINE ( 'NONE', #45543, #33091 ) ;
#1386 = VECTOR ( 'NONE', #23590, 1000.000000000000000 ) ;
#1387 = VERTEX_POINT ( 'NONE', #28925 ) ;
#1388 = PLANE ( 'NONE',  #58139 ) ;
#1389 = AXIS2_PLACEMENT_3D ( 'NONE', #27171, #64642, #64999 ) ;
#1390 = DIRECTION ( 'NONE',  ( 1.000000000000000000, 0.000000000000000000, 0.000000000000000000 ) ) ;
#1391 = VERTEX_POINT ( 'NONE', #22592 ) ;
#1392 = ORIENTED_EDGE ( 'NONE', *, *, #32157, .F. ) ;
#1393 = DIRECTION ( 'NONE',  ( -1.000000000000000000, 0.000000000000000000, 0.000000000000000000 ) ) ;
#1394 = DIRECTION ( 'NONE',  ( 0.000000000000000000, 1.000000000000000000, 0.000000000000000000 ) ) ;
#1395 = VECTOR ( 'NONE', #65892, 1000.000000000000000 ) ;
#1396 = ORIENTED_EDGE ( 'NONE', *, *, #50921, .T. ) ;
#1397 = DIRECTION ( 'NONE',  ( -0.000000000000000000, 0.000000000000000000, 1.000000000000000000 ) ) ;
#1398 = DIRECTION ( 'NONE',  ( -1.000000000000000000, 0.000000000000000000, 0.000000000000000000 ) ) ;
#1399 = LINE ( 'NONE', #17309, #22646 ) ;
#1400 = EDGE_LOOP ( 'NONE', ( #29351, #65718, #23483, #8254 ) ) ;
#1401 = EDGE_CURVE ( 'NONE', #2837, #64033, #17624, .T. ) ;
#1402 = VECTOR ( 'NONE', #11116, 1000.000000000000000 ) ;
#1403 = FACE_OUTER_BOUND ( 'NONE', #19703, .T. ) ;
#1404 = DIRECTION ( 'NONE',  ( 0.000000000000000000, 0.000000000000000000, -1.000000000000000000 ) ) ;
#1406 = VERTEX_POINT ( 'NONE', #39528 ) ;
#1405 = EDGE_CURVE ( 'NONE', #49901, #24890, #6667, .T. ) ;
#1408 = ORIENTED_EDGE ( 'NONE', *, *, #33147, .F. ) ;
#1407 = FACE_OUTER_BOUND ( 'NONE', #53741, .T. ) ;
#1410 = CARTESIAN_POINT ( 'NONE',  ( -11.18071654964681372, -11.19368345035335821, 455.0000000000000568 ) ) ;
#1409 = VECTOR ( 'NONE', #51524, 1000.000000000000000 ) ;
#1411 = CARTESIAN_POINT ( 'NONE',  ( 7.000000000000000000, -32.45000000000000995, 15.00000000000000000 ) ) ;
#1412 = DIRECTION ( 'NONE',  ( 1.836970198721029934E-16, -1.836970198721036344E-16, 1.000000000000000000 ) ) ;
#1413 = DIRECTION ( 'NONE',  ( 0.000000000000000000, 1.000000000000000000, 0.000000000000000000 ) ) ;
#1414 = LINE ( 'NONE', #22305, #61005 ) ;
#1415 = DIRECTION ( 'NONE',  ( 0.000000000000000000, 0.000000000000000000, -1.000000000000000000 ) ) ;
#1416 = ORIENTED_EDGE ( 'NONE', *, *, #51944, .F. ) ;
#1417 = CARTESIAN_POINT ( 'NONE',  ( -14.25000000000000000, -2.500000000000000000, -23.22168783648699986 ) ) ;
#1418 = DIRECTION ( 'NONE',  ( 0.000000000000000000, 0.000000000000000000, 1.000000000000000000 ) ) ;
#1420 = ORIENTED_EDGE ( 'NONE', *, *, #47528, .F. ) ;
#1419 = DIRECTION ( 'NONE',  ( 1.000000000000000000, -3.491481338843133355E-15, -1.836970198721036344E-16 ) ) ;
#1421 = DIRECTION ( 'NONE',  ( 1.836970198721029934E-16, -1.836970198721036344E-16, 1.000000000000000000 ) ) ;
#1422 = CARTESIAN_POINT ( 'NONE',  ( -7.798499376344109280, -4.740315990920159095, 455.0000000000000568 ) ) ;
#1423 = ORIENTED_EDGE ( 'NONE', *, *, #47757, .F. ) ;
#1424 = DIRECTION ( 'NONE',  ( -1.000000000000000000, 0.000000000000000000, 0.000000000000000000 ) ) ;
#1425 = PLANE ( 'NONE',  #32851 ) ;
#1426 = AXIS2_PLACEMENT_3D ( 'NONE', #25719, #57522, #15457 ) ;
#1427 = EDGE_LOOP ( 'NONE', ( #23899, #9021, #40035, #61175, #33660, #14173, #23433, #811, #34516, #4708, #47273, #5222, #68139, #6145, #12426, #39969, #23820 ) ) ;
#1428 = DIRECTION ( 'NONE',  ( -0.000000000000000000, -0.000000000000000000, 1.000000000000000000 ) ) ;
#1429 = CARTESIAN_POINT ( 'NONE',  ( 7.000000000000000000, -20.40000000000000213, 16.03137303340311348 ) ) ;
#1430 = PLANE ( 'NONE',  #63020 ) ;
#1431 = VECTOR ( 'NONE', #21426, 1000.000000000000000 ) ;
#1432 = PLANE ( 'NONE',  #65466 ) ;
#1433 = EDGE_CURVE ( 'NONE', #8412, #16770, #34213, .T. ) ;
#1434 = CARTESIAN_POINT ( 'NONE',  ( 10.90000000000000036, -21.00000000000001421, -13.86939075806900945 ) ) ;
#1435 = VERTEX_POINT ( 'NONE', #49472 ) ;
#1436 = CARTESIAN_POINT ( 'NONE',  ( 22.14589803375000088, -15.50000000000000000, -21.50000000000000000 ) ) ;
#1437 = ORIENTED_EDGE ( 'NONE', *, *, #39757, .F. ) ;
#1438 = ORIENTED_EDGE ( 'NONE', *, *, #37753, .F. ) ;
#1439 = FACE_OUTER_BOUND ( 'NONE', #15747, .T. ) ;
#1440 = CARTESIAN_POINT ( 'NONE',  ( -8.566576262117260754, 8.916576262117214213, 54.00000000000000711 ) ) ;
#1441 = EDGE_CURVE ( 'NONE', #56939, #1406, #61091, .T. ) ;
#1442 = CARTESIAN_POINT ( 'NONE',  ( 8.250000000000005329, -8.249999999999998224, -26.00000000000001066 ) ) ;
#1443 = LINE ( 'NONE', #23016, #34040 ) ;
#1444 = ORIENTED_EDGE ( 'NONE', *, *, #39819, .T. ) ;
#1445 = EDGE_CURVE ( 'NONE', #59664, #10161, #34093, .T. ) ;
#1446 = ORIENTED_EDGE ( 'NONE', *, *, #33690, .T. ) ;
#1447 = EDGE_CURVE ( 'NONE', #37532, #3798, #20437, .T. ) ;
#1448 = CARTESIAN_POINT ( 'NONE',  ( 30.00000000000000000, -16.64230188589299786, -14.64519951917100116 ) ) ;
#1449 = ORIENTED_EDGE ( 'NONE', *, *, #1893, .F. ) ;
#1450 = DIRECTION ( 'NONE',  ( -1.000000000000000000, 0.000000000000000000, 0.000000000000000000 ) ) ;
#1451 = CIRCLE ( 'NONE', #53416, 0.9999999999999991118 ) ;
#1452 = DIRECTION ( 'NONE',  ( -0.000000000000000000, 3.673940397442059868E-16, -1.000000000000000000 ) ) ;
#1453 = ADVANCED_FACE ( 'NONE', ( #33197 ), #12649, .F. ) ;
#1454 = CARTESIAN_POINT ( 'NONE',  ( -6.651770455163739548, 7.342976262117183239, 54.00000000000000711 ) ) ;
#1455 = VECTOR ( 'NONE', #11168, 1000.000000000000000 ) ;
#1457 = DIRECTION ( 'NONE',  ( -0.000000000000000000, -0.000000000000000000, 1.000000000000000000 ) ) ;
#1456 = CARTESIAN_POINT ( 'NONE',  ( -1.991476262117235274, 8.598420958951582094, 54.00000000000000711 ) ) ;
#1458 = COLOUR_RGB ( '', 0.09019608, 0.27058824, 0.51372549) ;
#1459 = VERTEX_POINT ( 'NONE', #28236 ) ;
#1461 = ORIENTED_EDGE ( 'NONE', *, *, #25428, .F. ) ;
#1460 = DIRECTION ( 'NONE',  ( -0.000000000000000000, -0.000000000000000000, -1.000000000000000000 ) ) ;
#1462 = VERTEX_POINT ( 'NONE', #49806 ) ;
#1463 = ORIENTED_EDGE ( 'NONE', *, *, #22319, .T. ) ;
#1464 = AXIS2_PLACEMENT_3D ( 'NONE', #40636, #35310, #45228 ) ;
#1465 = CARTESIAN_POINT ( 'NONE',  ( -28.00000000000000000, -16.28999999999999915, -14.50000000000000000 ) ) ;
#1466 = CARTESIAN_POINT ( 'NONE',  ( 7.000000000000000000, -38.65000000000095781, -14.49999999999903899 ) ) ;
#1467 = AXIS2_PLACEMENT_3D ( 'NONE', #20534, #63686, #37508 ) ;
#1468 = FACE_OUTER_BOUND ( 'NONE', #19907, .T. ) ;
#1469 = ORIENTED_EDGE ( 'NONE', *, *, #10867, .T. ) ;
#1470 = ORIENTED_EDGE ( 'NONE', *, *, #29362, .T. ) ;
#1471 = FACE_OUTER_BOUND ( 'NONE', #21863, .T. ) ;
#1472 = CARTESIAN_POINT ( 'NONE',  ( -11.00000000000000000, -14.33999999999999986, 14.50000000000000000 ) ) ;
#1473 = VECTOR ( 'NONE', #43632, 1000.000000000000000 ) ;
#1474 = ORIENTED_EDGE ( 'NONE', *, *, #23405, .F. ) ;
#1475 = VERTEX_POINT ( 'NONE', #56160 ) ;
#1476 = DIRECTION ( 'NONE',  ( 0.000000000000000000, 0.000000000000000000, -1.000000000000000000 ) ) ;
#1477 = VECTOR ( 'NONE', #52633, 1000.000000000000000 ) ;
#1478 = CARTESIAN_POINT ( 'NONE',  ( -14.10805890929250062, -5.000000000000000000, 26.25000000000000000 ) ) ;
#1479 = EDGE_LOOP ( 'NONE', ( #65688, #31155, #2228, #38780 ) ) ;
#1480 = CARTESIAN_POINT ( 'NONE',  ( 7.250000000000005329, -7.249999999999998224, -24.00000000000000000 ) ) ;
#1481 = VECTOR ( 'NONE', #33559, 1000.000000000000000 ) ;
#1484 = EDGE_LOOP ( 'NONE', ( #51385, #66092, #32923, #69891 ) ) ;
#1483 = EDGE_CURVE ( 'NONE', #14490, #54337, #29462, .T. ) ;
#1482 =( LENGTH_UNIT ( ) NAMED_UNIT ( * ) SI_UNIT ( .MILLI., .METRE. ) );
#1485 = ORIENTED_EDGE ( 'NONE', *, *, #31305, .T. ) ;
#1486 = EDGE_CURVE ( 'NONE', #22030, #7056, #55806, .T. ) ;
#1487 = EDGE_CURVE ( 'NONE', #16822, #52439, #21549, .T. ) ;
#1488 = CARTESIAN_POINT ( 'NONE',  ( 4.149127210878725158, 6.822336235477391320, 54.00000000000000711 ) ) ;
#1489 = CARTESIAN_POINT ( 'NONE',  ( 16.89999999999999858, -21.00000000000000000, 13.86939075806900057 ) ) ;
#1490 = LINE ( 'NONE', #29402, #14826 ) ;
#1491 = FACE_OUTER_BOUND ( 'NONE', #7855, .T. ) ;
#1492 = CARTESIAN_POINT ( 'NONE',  ( -6.331612867284154511, 8.393516549646601987, 195.0000000000000284 ) ) ;
#1493 = EDGE_CURVE ( 'NONE', #44134, #53260, #54471, .T. ) ;
#1494 = LINE ( 'NONE', #28367, #26018 ) ;
#1495 = ORIENTED_EDGE ( 'NONE', *, *, #61365, .T. ) ;
#1496 = CARTESIAN_POINT ( 'NONE',  ( -8.393516549646712122, 6.331612867284047041, 455.0000000000000568 ) ) ;
#1498 = ORIENTED_EDGE ( 'NONE', *, *, #56858, .T. ) ;
#1497 = DIRECTION ( 'NONE',  ( 1.000000000000000000, -1.813998472013049822E-14, 0.000000000000000000 ) ) ;
#1499 = FACE_OUTER_BOUND ( 'NONE', #3883, .T. ) ;
#1500 = AXIS2_PLACEMENT_3D ( 'NONE', #56590, #57295, #62959 ) ;
#1501 = CARTESIAN_POINT ( 'NONE',  ( 39.90000000000000568, 20.60000000000000142, 13.86939075806899702 ) ) ;
#1502 = DIRECTION ( 'NONE',  ( 0.000000000000000000, -1.000000000000000000, 0.000000000000000000 ) ) ;
#1504 = CARTESIAN_POINT ( 'NONE',  ( 9.306483450353418618, 10.91351654964656426, 455.0000000000000568 ) ) ;
#1503 = VECTOR ( 'NONE', #29338, 1000.000000000000000 ) ;
#1505 = AXIS2_PLACEMENT_3D ( 'NONE', #583, #23529, #38412 ) ;
#1506 = DIRECTION ( 'NONE',  ( 0.000000000000000000, 0.000000000000000000, 1.000000000000000000 ) ) ;
#1507 = CIRCLE ( 'NONE', #18452, 0.5000000000009459100 ) ;
#1508 = ORIENTED_EDGE ( 'NONE', *, *, #11975, .T. ) ;
#1509 = ORIENTED_EDGE ( 'NONE', *, *, #62192, .F. ) ;
#1510 = AXIS2_PLACEMENT_3D ( 'NONE', #36370, #14100, #8806 ) ;
#1511 = LINE ( 'NONE', #22738, #3157 ) ;
#1512 =( NAMED_UNIT ( * ) PLANE_ANGLE_UNIT ( ) SI_UNIT ( $, .RADIAN. ) );
#1513 = ORIENTED_EDGE ( 'NONE', *, *, #6208, .T. ) ;
#1514 = CARTESIAN_POINT ( 'NONE',  ( 6.836383711242970840, 4.135079735113107446, 26.00000000000000711 ) ) ;
#1515 = EDGE_LOOP ( 'NONE', ( #52071, #22197, #20017, #42552 ) ) ;
#1516 = ORIENTED_EDGE ( 'NONE', *, *, #68122, .F. ) ;
#1517 = DIRECTION ( 'NONE',  ( -1.000000000000000000, 0.000000000000000000, 0.000000000000000000 ) ) ;
#1518 = DIRECTION ( 'NONE',  ( 0.000000000000000000, -0.7071067811865875408, -0.7071067811865076047 ) ) ;
#1519 = ORIENTED_EDGE ( 'NONE', *, *, #31973, .T. ) ;
#1520 = FACE_OUTER_BOUND ( 'NONE', #17280, .T. ) ;
#1521 = DIRECTION ( 'NONE',  ( 0.000000000000000000, 0.000000000000000000, 1.000000000000000000 ) ) ;
#1522 = LINE ( 'NONE', #33370, #9492 ) ;
#1523 = DIRECTION ( 'NONE',  ( 0.000000000000000000, 1.000000000000000000, 0.000000000000000000 ) ) ;
#1524 = ORIENTED_EDGE ( 'NONE', *, *, #59667, .T. ) ;
#1526 = ORIENTED_EDGE ( 'NONE', *, *, #42730, .F. ) ;
#1525 = FACE_OUTER_BOUND ( 'NONE', #31691, .T. ) ;
#1527 = EDGE_CURVE ( 'NONE', #3937, #22000, #44835, .T. ) ;
#1528 = DIRECTION ( 'NONE',  ( 0.000000000000000000, -1.000000000000000000, 0.000000000000000000 ) ) ;
#1529 = DIRECTION ( 'NONE',  ( -0.000000000000000000, 3.673940397442059868E-16, -1.000000000000000000 ) ) ;
#1530 = EDGE_CURVE ( 'NONE', #24780, #41832, #39594, .T. ) ;
#1531 = DIRECTION ( 'NONE',  ( 0.7071067811865463515, 0.7071067811865487940, 0.000000000000000000 ) ) ;
#1532 = DIRECTION ( 'NONE',  ( 0.000000000000000000, -1.000000000000000000, 0.000000000000000000 ) ) ;
#1533 = EDGE_LOOP ( 'NONE', ( #21122, #40347, #45235, #65247 ) ) ;
#1534 = EDGE_CURVE ( 'NONE', #42678, #52964, #27904, .T. ) ;
#1535 = CARTESIAN_POINT ( 'NONE',  ( 277.3542486889354564, -20.50000000000000000, 17.00000000000000000 ) ) ;
#1536 = CARTESIAN_POINT ( 'NONE',  ( 52.83090410532631864, 5.657408540445001854, 0.000000000000000000 ) ) ;
#1537 = EDGE_CURVE ( 'NONE', #32087, #62810, #57683, .T. ) ;
#1538 = ORIENTED_EDGE ( 'NONE', *, *, #59245, .T. ) ;
#1539 = ORIENTED_EDGE ( 'NONE', *, *, #26792, .T. ) ;
#1540 = PRODUCT_RELATED_PRODUCT_CATEGORY ( 'part', '', ( #57140 ) ) ;
#1541 = ORIENTED_EDGE ( 'NONE', *, *, #827, .F. ) ;
#1542 = CARTESIAN_POINT ( 'NONE',  ( 7.250000000000005329, -8.249999999999998224, -19.50000000000000000 ) ) ;
#1543 = EDGE_CURVE ( 'NONE', #33912, #33774, #60405, .T. ) ;
#1544 = DIRECTION ( 'NONE',  ( 0.000000000000000000, 1.000000000000000000, 0.000000000000000000 ) ) ;
#1545 = EDGE_CURVE ( 'NONE', #54090, #69297, #66417, .T. ) ;
#1546 = CARTESIAN_POINT ( 'NONE',  ( 49.49873889023718476, 0.7500000000000000000, 4.436432704656454895 ) ) ;
#1547 = AXIS2_PLACEMENT_3D ( 'NONE', #61946, #34725, #13513 ) ;
#1548 = CIRCLE ( 'NONE', #10597, 1.399999999999998579 ) ;
#1549 = CARTESIAN_POINT ( 'NONE',  ( -10.30047626211729472, -6.849523737882750929, 54.00000000000000711 ) ) ;
#1550 = EDGE_LOOP ( 'NONE', ( #4888, #5831, #20049, #32762 ) ) ;
#1551 = ORIENTED_EDGE ( 'NONE', *, *, #30265, .T. ) ;
#1552 = ORIENTED_EDGE ( 'NONE', *, *, #17669, .F. ) ;
#1553 = LINE ( 'NONE', #46089, #36194 ) ;
#1554 = ORIENTED_EDGE ( 'NONE', *, *, #19391, .T. ) ;
#1555 = VECTOR ( 'NONE', #67629, 1000.000000000000000 ) ;
#1556 = AXIS2_PLACEMENT_3D ( 'NONE', #57071, #35142, #8635 ) ;
#1557 = VERTEX_POINT ( 'NONE', #19704 ) ;
#1558 = EDGE_LOOP ( 'NONE', ( #62226, #31483, #47154, #67223 ) ) ;
#1559 = ORIENTED_EDGE ( 'NONE', *, *, #13351, .F. ) ;
#1560 = CARTESIAN_POINT ( 'NONE',  ( -9.690000000000001279, 10.50000000000000178, -5.000000000000000000 ) ) ;
#1561 = AXIS2_PLACEMENT_3D ( 'NONE', #7094, #24422, #50240 ) ;
#1562 = VECTOR ( 'NONE', #37245, 1000.000000000000000 ) ;
#1564 = ORIENTED_EDGE ( 'NONE', *, *, #25883, .T. ) ;
#1563 = CARTESIAN_POINT ( 'NONE',  ( -7.450000000000001954, 0.000000000000000000, -21.00000000000000000 ) ) ;
#1565 = DIRECTION ( 'NONE',  ( 3.491481338843132961E-15, 1.000000000000000000, 0.000000000000000000 ) ) ;
#1566 = CARTESIAN_POINT ( 'NONE',  ( 275.0000000000000000, -0.5000000000000000000, 50.00000000000000000 ) ) ;
#1567 = LINE ( 'NONE', #65589, #38121 ) ;
#1569 = ORIENTED_EDGE ( 'NONE', *, *, #60453, .F. ) ;
#1568 = LINE ( 'NONE', #18175, #59424 ) ;
#1570 = FACE_OUTER_BOUND ( 'NONE', #29203, .T. ) ;
#1571 = CARTESIAN_POINT ( 'NONE',  ( -7.250000000000000888, -8.249999999999998224, -26.00000000000001066 ) ) ;
#1572 = EDGE_CURVE ( 'NONE', #5389, #36022, #29616, .T. ) ;
#1573 = DIRECTION ( 'NONE',  ( 0.000000000000000000, 0.000000000000000000, 1.000000000000000000 ) ) ;
#1574 = VERTEX_POINT ( 'NONE', #62486 ) ;
#1575 = DIRECTION ( 'NONE',  ( -1.000000000000000000, 0.000000000000000000, 0.000000000000000000 ) ) ;
#1576 = CARTESIAN_POINT ( 'NONE',  ( -9.722976262117294155, -6.832023737882757963, 54.00000000000000711 ) ) ;
#1577 = FACE_OUTER_BOUND ( 'NONE', #60002, .T. ) ;
#1578 = ORIENTED_EDGE ( 'NONE', *, *, #61062, .F. ) ;
#1579 = CARTESIAN_POINT ( 'NONE',  ( -9.689726262117325462, -9.703773737882725570, 54.00000000000000711 ) ) ;
#1580 = EDGE_CURVE ( 'NONE', #38637, #12098, #57900, .T. ) ;
#1581 = DIRECTION ( 'NONE',  ( -1.836970198721029934E-16, 1.836970198721036344E-16, -1.000000000000000000 ) ) ;
#1582 = CARTESIAN_POINT ( 'NONE',  ( 283.0000000000000568, -31.30000000000045191, 8.900000000000430234 ) ) ;
#1583 = VECTOR ( 'NONE', #66399, 1000.000000000000114 ) ;
#1584 = ORIENTED_EDGE ( 'NONE', *, *, #53447, .F. ) ;
#1585 = EDGE_CURVE ( 'NONE', #26989, #55919, #9467, .T. ) ;
#1586 = LINE ( 'NONE', #17861, #34253 ) ;
#1587 = FACE_OUTER_BOUND ( 'NONE', #30596, .T. ) ;
#1588 = DIRECTION ( 'NONE',  ( 0.000000000000000000, 1.000000000000000000, 0.000000000000000000 ) ) ;
#1589 = CARTESIAN_POINT ( 'NONE',  ( -11.75000000000000000, -5.000000000000000000, 23.89194109070750471 ) ) ;
#1590 = AXIS2_PLACEMENT_3D ( 'NONE', #35235, #23946, #51530 ) ;
#1591 = AXIS2_PLACEMENT_3D ( 'NONE', #14961, #30871, #52446 ) ;
#1592 = VERTEX_POINT ( 'NONE', #14426 ) ;
#1593 = FACE_OUTER_BOUND ( 'NONE', #63694, .T. ) ;
#1594 = FACE_OUTER_BOUND ( 'NONE', #55076, .T. ) ;
#1595 = DIRECTION ( 'NONE',  ( -1.000000000000000000, 0.000000000000000000, 0.000000000000000000 ) ) ;
#1596 = CARTESIAN_POINT ( 'NONE',  ( 8.900000000000005684, -14.06939075806900163, -20.80000000000000426 ) ) ;
#1597 = DIRECTION ( 'NONE',  ( 0.000000000000000000, 0.000000000000000000, -1.000000000000000000 ) ) ;
#1598 = VECTOR ( 'NONE', #19788, 1000.000000000000000 ) ;
#1599 = VERTEX_POINT ( 'NONE', #35984 ) ;
#1600 = DIRECTION ( 'NONE',  ( 0.000000000000000000, 0.000000000000000000, -1.000000000000000000 ) ) ;
#1601 = DIRECTION ( 'NONE',  ( -0.6414496315691617934, -0.7671651518152962090, -2.818519042763987834E-16 ) ) ;
#1602 = EDGE_CURVE ( 'NONE', #22867, #61212, #51553, .T. ) ;
#1603 = CARTESIAN_POINT ( 'NONE',  ( 11.12648345035337982, -4.206483450353492692, 455.0000000000000568 ) ) ;
#1604 = VECTOR ( 'NONE', #54096, 1000.000000000000000 ) ;
#1605 = CARTESIAN_POINT ( 'NONE',  ( 289.2330000000000041, 4.898587196589412829E-16, -4.000000000000000000 ) ) ;
#1606 = DIRECTION ( 'NONE',  ( 0.000000000000000000, 0.000000000000000000, -1.000000000000000000 ) ) ;
#1607 = ORIENTED_EDGE ( 'NONE', *, *, #69112, .T. ) ;
#1608 = ORIENTED_EDGE ( 'NONE', *, *, #4024, .F. ) ;
#1609 = DIRECTION ( 'NONE',  ( 3.614007241618349165E-15, 1.000000000000000000, 0.000000000000000000 ) ) ;
#1610 = ADVANCED_FACE ( 'NONE', ( #40929 ), #46582, .T. ) ;
#1611 = FACE_OUTER_BOUND ( 'NONE', #65405, .T. ) ;
#1612 = ORIENTED_EDGE ( 'NONE', *, *, #7995, .T. ) ;
#1613 = AXIS2_PLACEMENT_3D ( 'NONE', #62679, #69039, #20597 ) ;
#1614 = CARTESIAN_POINT ( 'NONE',  ( 11.00000000000000000, -13.54524521594299991, 17.53999999999999915 ) ) ;
#1615 = ORIENTED_EDGE ( 'NONE', *, *, #28816, .F. ) ;
#1616 = CARTESIAN_POINT ( 'NONE',  ( -14.25000000000000178, -0.2714405302574905976, -22.98746066354537732 ) ) ;
#1617 = ORIENTED_EDGE ( 'NONE', *, *, #28712, .F. ) ;
#1618 = ORIENTED_EDGE ( 'NONE', *, *, #42670, .T. ) ;
#1620 = EDGE_CURVE ( 'NONE', #61917, #27668, #9116, .T. ) ;
#1619 = CARTESIAN_POINT ( 'NONE',  ( -1.077516549646670541, 11.33351654964656596, 455.0000000000000568 ) ) ;
#1621 = DIRECTION ( 'NONE',  ( -1.000000000000000000, 1.671920889371702854E-15, 6.142537696789956391E-31 ) ) ;
#1622 = ADVANCED_FACE ( 'NONE', ( #8046 ), #52613, .F. ) ;
#1623 = CARTESIAN_POINT ( 'NONE',  ( 25.50000000000000355, -17.50000000000000000, -25.99999999999985434 ) ) ;
#1624 = CARTESIAN_POINT ( 'NONE',  ( 32.89999999999999858, 20.60000000000000142, -13.86939075806900057 ) ) ;
#1625 = ORIENTED_EDGE ( 'NONE', *, *, #63006, .T. ) ;
#1626 = ORIENTED_EDGE ( 'NONE', *, *, #18494, .T. ) ;
#1627 = DIRECTION ( 'NONE',  ( -0.4999999999999832356, 0.000000000000000000, 0.8660254037844483666 ) ) ;
#1628 = LINE ( 'NONE', #972, #56470 ) ;
#1629 = ORIENTED_EDGE ( 'NONE', *, *, #51776, .T. ) ;
#1630 = EDGE_CURVE ( 'NONE', #15321, #39690, #52252, .T. ) ;
#1631 = VECTOR ( 'NONE', #48674, 1000.000000000000000 ) ;
#1632 = VERTEX_POINT ( 'NONE', #4175 ) ;
#1633 = ORIENTED_EDGE ( 'NONE', *, *, #51084, .F. ) ;
#1634 = DIRECTION ( 'NONE',  ( -0.7071067811865486830, -0.7071067811865464625, -2.597868168706476160E-16 ) ) ;
#1635 = CARTESIAN_POINT ( 'NONE',  ( -7.450000000000001954, 0.000000000000000000, -12.50000000000000000 ) ) ;
#1637 = EDGE_LOOP ( 'NONE', ( #57088, #33379, #39872, #24268 ) ) ;
#1636 = CARTESIAN_POINT ( 'NONE',  ( 6.358413763958968623, -5.793274621760859944, 54.00000000000000711 ) ) ;
#1638 = CARTESIAN_POINT ( 'NONE',  ( -3.842976262117224984, 9.897976262117168744, 26.00000000000000711 ) ) ;
#1639 = AXIS2_PLACEMENT_3D ( 'NONE', #45428, #66654, #67362 ) ;
#1640 = AXIS2_PLACEMENT_3D ( 'NONE', #8943, #8593, #25581 ) ;
#1641 = CYLINDRICAL_SURFACE ( 'NONE', #38486, 0.3499999999999996447 ) ;
#1642 = ORIENTED_EDGE ( 'NONE', *, *, #69015, .T. ) ;
#1643 = ORIENTED_EDGE ( 'NONE', *, *, #28455, .T. ) ;
#1644 = VECTOR ( 'NONE', #60064, 1000.000000000000000 ) ;
#1645 = ADVANCED_FACE ( 'NONE', ( #67474 ), #19022, .F. ) ;
#1646 = CARTESIAN_POINT ( 'NONE',  ( -8.250000000000000000, 7.250000000000001776, -11.00000000000000000 ) ) ;
#1647 = DIRECTION ( 'NONE',  ( 3.491481338843133355E-15, 1.000000000000000000, 1.836970198721029934E-16 ) ) ;
#1648 = CIRCLE ( 'NONE', #34395, 0.1999999999999987899 ) ;
#1649 = CARTESIAN_POINT ( 'NONE',  ( -4.727349090213463612, 7.798499376343949407, 455.0000000000000568 ) ) ;
#1650 = EDGE_CURVE ( 'NONE', #57266, #62681, #23812, .T. ) ;
#1651 = PRESENTATION_LAYER_ASSIGNMENT (  '', '', ( #38970 ) ) ;
#1652 = FILL_AREA_STYLE ('',( #61043 ) ) ;
#1653 = DIRECTION ( 'NONE',  ( 0.000000000000000000, 0.000000000000000000, 1.000000000000000000 ) ) ;
#1655 = ORIENTED_EDGE ( 'NONE', *, *, #59855, .T. ) ;
#1654 = DIRECTION ( 'NONE',  ( 0.000000000000000000, 0.000000000000000000, 1.000000000000000000 ) ) ;
#1656 = ORIENTED_EDGE ( 'NONE', *, *, #67381, .T. ) ;
#1657 = EDGE_CURVE ( 'NONE', #57888, #27734, #62142, .T. ) ;
#1658 = AXIS2_PLACEMENT_3D ( 'NONE', #22273, #7, #53407 ) ;
#1659 = DIRECTION ( 'NONE',  ( 1.000000000000000000, 0.000000000000000000, 0.000000000000000000 ) ) ;
#1660 = PLANE ( 'NONE',  #56748 ) ;
#1661 = EDGE_CURVE ( 'NONE', #3520, #47586, #3115, .T. ) ;
#1662 = FACE_OUTER_BOUND ( 'NONE', #48471, .T. ) ;
#1663 = DIRECTION ( 'NONE',  ( 1.000000000000000000, -0.000000000000000000, -0.000000000000000000 ) ) ;
#1664 = EDGE_CURVE ( 'NONE', #31939, #11916, #24681, .T. ) ;
#1665 = LINE ( 'NONE', #45144, #10556 ) ;
#1666 = EDGE_LOOP ( 'NONE', ( #15251, #59650 ) ) ;
#1667 = CARTESIAN_POINT ( 'NONE',  ( -4.188533722949374649, -7.272650909786617213, 195.0000000000000284 ) ) ;
#1668 = CARTESIAN_POINT ( 'NONE',  ( 181.4833316329832940, 9.000000000000001776, 284.4801873289890182 ) ) ;
#1669 = CARTESIAN_POINT ( 'NONE',  ( -8.566576262117358453, -9.703773737882738004, 54.00000000000000711 ) ) ;
#1670 = CARTESIAN_POINT ( 'NONE',  ( -7.450000000000001954, 0.000000000000000000, -21.50000000000000000 ) ) ;
#1671 = CARTESIAN_POINT ( 'NONE',  ( 25.49999999999869971, -15.50000000000000000, -22.50000000000000000 ) ) ;
#1672 = EDGE_CURVE ( 'NONE', #26901, #3811, #20074, .T. ) ;
#1673 = AXIS2_PLACEMENT_3D ( 'NONE', #16608, #16241, #66054 ) ;
#1674 = LINE ( 'NONE', #32828, #36392 ) ;
#1675 = EDGE_CURVE ( 'NONE', #14837, #20832, #52186, .T. ) ;
#1676 = LINE ( 'NONE', #66391, #8125 ) ;
#1677 = ORIENTED_EDGE ( 'NONE', *, *, #36142, .F. ) ;
#1678 = PLANE ( 'NONE',  #59210 ) ;
#1679 = FACE_OUTER_BOUND ( 'NONE', #12903, .T. ) ;
#1680 = EDGE_CURVE ( 'NONE', #55748, #40253, #35619, .T. ) ;
#1681 = VECTOR ( 'NONE', #12130, 1000.000000000000000 ) ;
#1682 = VERTEX_POINT ( 'NONE', #25740 ) ;
#1683 = CARTESIAN_POINT ( 'NONE',  ( 6.872275254348426010, -3.003254798005762449, 54.00000000000000711 ) ) ;
#1684 = ADVANCED_FACE ( 'NONE', ( #30332, #51905 ), #47297, .F. ) ;
#1685 = EDGE_CURVE ( 'NONE', #67031, #20195, #1257, .T. ) ;
#1686 = DIRECTION ( 'NONE',  ( 0.000000000000000000, 0.000000000000000000, -1.000000000000000000 ) ) ;
#1687 = CARTESIAN_POINT ( 'NONE',  ( -15.50000000000000000, -2.500000000000000000, -21.05662432702600029 ) ) ;
#1688 = DIRECTION ( 'NONE',  ( 0.000000000000000000, 0.000000000000000000, -1.000000000000000000 ) ) ;
#1689 = DIRECTION ( 'NONE',  ( -1.000000000000000000, 0.000000000000000000, 0.000000000000000000 ) ) ;
#1690 = VERTEX_POINT ( 'NONE', #16519 ) ;
#1691 = ADVANCED_FACE ( 'NONE', ( #48690 ), #32440, .F. ) ;
#1692 = CARTESIAN_POINT ( 'NONE',  ( -9.689726262117325462, -10.05377373788272166, 26.00000000000000000 ) ) ;
#1693 = AXIS2_PLACEMENT_3D ( 'NONE', #11004, #37878, #59442 ) ;
#1694 = VECTOR ( 'NONE', #14522, 1000.000000000000114 ) ;
#1695 = ORIENTED_EDGE ( 'NONE', *, *, #58865, .T. ) ;
#1696 = EDGE_CURVE ( 'NONE', #66712, #58124, #15482, .T. ) ;
#1697 = DIRECTION ( 'NONE',  ( 1.000000000000000000, 0.000000000000000000, 0.000000000000000000 ) ) ;
#1698 = ORIENTED_EDGE ( 'NONE', *, *, #19092, .T. ) ;
#1699 = DIRECTION ( 'NONE',  ( 0.000000000000000000, 0.000000000000000000, -1.000000000000000000 ) ) ;
#1700 = EDGE_CURVE ( 'NONE', #65232, #34832, #54010, .T. ) ;
#1701 = VECTOR ( 'NONE', #44410, 1000.000000000000000 ) ;
#1702 = CIRCLE ( 'NONE', #54821, 0.3999999999999993006 ) ;
#1703 = CARTESIAN_POINT ( 'NONE',  ( 11.78648345035335865, 7.813516549646607245, 195.0000000000000284 ) ) ;
#1704 = AXIS2_PLACEMENT_3D ( 'NONE', #52680, #4582, #31107 ) ;
#1705 = DIRECTION ( 'NONE',  ( -1.000000000000000000, -0.000000000000000000, -0.000000000000000000 ) ) ;
#1706 = ORIENTED_EDGE ( 'NONE', *, *, #12925, .T. ) ;
#1707 = VERTEX_POINT ( 'NONE', #15127 ) ;
#1709 = ADVANCED_FACE ( 'NONE', ( #36689 ), #15817, .F. ) ;
#1708 = CARTESIAN_POINT ( 'NONE',  ( 17.00000000000000000, -17.00000000000000000, -15.70499999999969809 ) ) ;
#1710 = ORIENTED_EDGE ( 'NONE', *, *, #124, .F. ) ;
#1711 = ORIENTED_EDGE ( 'NONE', *, *, #61698, .F. ) ;
#1712 = EDGE_CURVE ( 'NONE', #65266, #65838, #58954, .T. ) ;
#1713 = PLANE ( 'NONE',  #57515 ) ;
#1714 = CARTESIAN_POINT ( 'NONE',  ( -11.77351654964669514, -4.406483450353273490, 195.0000000000000284 ) ) ;
#1715 = CARTESIAN_POINT ( 'NONE',  ( 75.42576880091934299, 0.000000000000000000, 327.4830310981788557 ) ) ;
#1716 = ORIENTED_EDGE ( 'NONE', *, *, #5157, .T. ) ;
#1717 = VECTOR ( 'NONE', #40181, 1000.000000000000000 ) ;
#1718 = FACE_OUTER_BOUND ( 'NONE', #696, .T. ) ;
#1720 = DIRECTION ( 'NONE',  ( -1.000000000000000000, 0.000000000000000000, 0.000000000000000000 ) ) ;
#1719 = PLANE ( 'NONE',  #23120 ) ;
#1721 = VERTEX_POINT ( 'NONE', #254 ) ;
#1723 = ORIENTED_EDGE ( 'NONE', *, *, #14236, .F. ) ;
#1722 = DIRECTION ( 'NONE',  ( 0.000000000000000000, 0.7071067811865474617, -0.7071067811865474617 ) ) ;
#1724 = ORIENTED_EDGE ( 'NONE', *, *, #43985, .T. ) ;
#1725 = DIRECTION ( 'NONE',  ( 0.000000000000000000, 1.000000000000000000, 0.000000000000000000 ) ) ;
#1726 = ORIENTED_EDGE ( 'NONE', *, *, #4024, .T. ) ;
#1727 = DIRECTION ( 'NONE',  ( -1.000000000000000000, 0.000000000000000000, 0.000000000000000000 ) ) ;
#1728 = DIRECTION ( 'NONE',  ( 1.000000000000000000, -0.000000000000000000, 0.000000000000000000 ) ) ;
#1729 = VERTEX_POINT ( 'NONE', #54348 ) ;
#1730 = ORIENTED_EDGE ( 'NONE', *, *, #55564, .T. ) ;
#1731 = LINE ( 'NONE', #29290, #24476 ) ;
#1732 = DIRECTION ( 'NONE',  ( -1.000000000000000000, 1.214636490590110115E-14, -1.836970198721007501E-16 ) ) ;
#1733 = VECTOR ( 'NONE', #60060, 1000.000000000000000 ) ;
#1734 = ORIENTED_EDGE ( 'NONE', *, *, #15533, .T. ) ;
#1735 = DIRECTION ( 'NONE',  ( -1.000000000000000000, 0.000000000000000000, 0.000000000000000000 ) ) ;
#1736 = FACE_BOUND ( 'NONE', #15930, .T. ) ;
#1737 = VECTOR ( 'NONE', #21797, 1000.000000000000000 ) ;
#1738 = CARTESIAN_POINT ( 'NONE',  ( 283.0000000000000568, -20.50000000000000000, -17.00000000000000000 ) ) ;
#1739 = EDGE_LOOP ( 'NONE', ( #36567, #1625, #38351, #20773 ) ) ;
#1740 = EDGE_CURVE ( 'NONE', #48692, #36045, #21815, .T. ) ;
#1741 = VECTOR ( 'NONE', #56009, 1000.000000000000000 ) ;
#1742 = CIRCLE ( 'NONE', #37914, 0.1999999999999987899 ) ;
#1743 = VECTOR ( 'NONE', #55400, 1000.000000000000114 ) ;
#1744 = CARTESIAN_POINT ( 'NONE',  ( 17.00000000000000000, -17.50000000000000000, -15.70500000000000007 ) ) ;
#1745 = CARTESIAN_POINT ( 'NONE',  ( 11.00000000000000000, -14.04000000000000092, 14.80000000000000071 ) ) ;
#1747 = ORIENTED_EDGE ( 'NONE', *, *, #16600, .F. ) ;
#1746 = PRESENTATION_STYLE_ASSIGNMENT (( #18704 ) ) ;
#1749 = ORIENTED_EDGE ( 'NONE', *, *, #28904, .F. ) ;
#1748 = DIRECTION ( 'NONE',  ( 0.000000000000000000, 0.000000000000000000, -1.000000000000000000 ) ) ;
#1750 = EDGE_CURVE ( 'NONE', #68268, #288, #69045, .T. ) ;
#1751 = CARTESIAN_POINT ( 'NONE',  ( 7.000000000000000000, -40.30000000000000426, 8.900000000000000355 ) ) ;
#1752 = CIRCLE ( 'NONE', #14234, 24.99999999998784972 ) ;
#1753 = FACE_OUTER_BOUND ( 'NONE', #60046, .T. ) ;
#1754 = ADVANCED_FACE ( 'NONE', ( #26086 ), #10508, .F. ) ;
#1755 = CARTESIAN_POINT ( 'NONE',  ( 33.89999999999999858, 0.000000000000000000, 2.801416793502919355E-15 ) ) ;
#1756 = FACE_OUTER_BOUND ( 'NONE', #63411, .T. ) ;
#1757 = B_SPLINE_CURVE_WITH_KNOTS ( 'NONE', 3,
 ( #31440, #33830, #65342, #6623, #44781, #66373 ),
 .UNSPECIFIED., .F., .F.,
 ( 4, 2, 4 ),
 ( 1.820537833122031657, 2.555393473688636341, 3.290249114255240581 ),
 .UNSPECIFIED. ) ;
#1758 = EDGE_CURVE ( 'NONE', #28928, #18073, #29509, .T. ) ;
#1759 = DIRECTION ( 'NONE',  ( 0.000000000000000000, 1.000000000000000000, 0.000000000000000000 ) ) ;
#1760 = VERTEX_POINT ( 'NONE', #69905 ) ;
#1761 = DIRECTION ( 'NONE',  ( -0.000000000000000000, 1.000000000000000000, 0.000000000000000000 ) ) ;
#1762 = CARTESIAN_POINT ( 'NONE',  ( 7.250000000000005329, 7.250000000000000888, -26.00000000000001066 ) ) ;
#1763 = DIRECTION ( 'NONE',  ( -0.6414496315691617934, -0.7671651518152962090, -2.818519042763987834E-16 ) ) ;
#1765 = EDGE_LOOP ( 'NONE', ( #69753, #46852, #22162, #36717 ) ) ;
#1764 = CARTESIAN_POINT ( 'NONE',  ( 8.250000000000005329, 0.000000000000000000, -22.50000000000000000 ) ) ;
#1766 = AXIS2_PLACEMENT_3D ( 'NONE', #18824, #40392, #23778 ) ;
#1767 = CARTESIAN_POINT ( 'NONE',  ( 30.00000000000000000, -5.000000000000000000, 27.00000000000000000 ) ) ;
#1768 = AXIS2_PLACEMENT_3D ( 'NONE', #6717, #60465, #33930 ) ;
#1769 = CARTESIAN_POINT ( 'NONE',  ( -7.447976262117260049, 9.880476262117177555, 54.00000000000000711 ) ) ;
#1770 = ORIENTED_EDGE ( 'NONE', *, *, #65264, .F. ) ;
#1771 = FACE_OUTER_BOUND ( 'NONE', #49422, .T. ) ;
#1772 = DIRECTION ( 'NONE',  ( 0.000000000000000000, 0.000000000000000000, 1.000000000000000000 ) ) ;
#1773 = ORIENTED_EDGE ( 'NONE', *, *, #26359, .F. ) ;
#1774 = ADVANCED_FACE ( 'NONE', ( #16166 ), #10162, .T. ) ;
#1775 = FACE_OUTER_BOUND ( 'NONE', #49116, .T. ) ;
#1776 = DIRECTION ( 'NONE',  ( 0.000000000000000000, 0.7071067811865474617, 0.7071067811865474617 ) ) ;
#1777 = DIRECTION ( 'NONE',  ( 0.000000000000000000, 0.000000000000000000, -1.000000000000000000 ) ) ;
#1778 = LINE ( 'NONE', #766, #55320 ) ;
#1779 = FACE_OUTER_BOUND ( 'NONE', #3037, .T. ) ;
#1780 = EDGE_LOOP ( 'NONE', ( #11033, #31500, #64794, #15896 ) ) ;
#1781 = CARTESIAN_POINT ( 'NONE',  ( -7.250000000000001776, -7.249999999999998224, -21.50000000000000000 ) ) ;
#1782 = VERTEX_POINT ( 'NONE', #58259 ) ;
#1783 = CIRCLE ( 'NONE', #16488, 4.000000000000001776 ) ;
#1784 = ORIENTED_EDGE ( 'NONE', *, *, #54013, .T. ) ;
#1785 = CARTESIAN_POINT ( 'NONE',  ( 7.000000000000000000, -23.50007830495750127, -12.28007262201345995 ) ) ;
#1786 = AXIS2_PLACEMENT_3D ( 'NONE', #9014, #47217, #36238 ) ;
#1787 = CARTESIAN_POINT ( 'NONE',  ( 158.0064834503532722, -35.83962462487175316, 0.000000000000000000 ) ) ;
#1788 = VECTOR ( 'NONE', #25866, 1000.000000000000000 ) ;
#1789 = CARTESIAN_POINT ( 'NONE',  ( 8.930623737882843471, 8.566576262117187923, 54.00000000000000711 ) ) ;
#1790 = EDGE_LOOP ( 'NONE', ( #57606, #59148, #46088, #2843 ) ) ;
#1791 = ORIENTED_EDGE ( 'NONE', *, *, #45815, .F. ) ;
#1793 = EDGE_CURVE ( 'NONE', #34056, #15308, #39643, .T. ) ;
#1792 = DIRECTION ( 'NONE',  ( 1.000000000000000000, 0.000000000000000000, 0.000000000000000000 ) ) ;
#1794 = ORIENTED_EDGE ( 'NONE', *, *, #6856, .F. ) ;
#1795 = EDGE_CURVE ( 'NONE', #57965, #33976, #20768, .T. ) ;
#1796 = AXIS2_PLACEMENT_3D ( 'NONE', #20618, #52462, #63772 ) ;
#1797 = VECTOR ( 'NONE', #20042, 1000.000000000000000 ) ;
#1798 = VECTOR ( 'NONE', #69775, 1000.000000000000000 ) ;
#1799 = CARTESIAN_POINT ( 'NONE',  ( 283.0000000000000568, -25.56180396883900130, 14.25872597390799967 ) ) ;
#1800 = DIRECTION ( 'NONE',  ( 0.000000000000000000, 0.000000000000000000, -1.000000000000000000 ) ) ;
#1801 = DIRECTION ( 'NONE',  ( 0.000000000000000000, -1.000000000000000000, 0.000000000000000000 ) ) ;
#1802 = EDGE_CURVE ( 'NONE', #23208, #33832, #4865, .T. ) ;
#1803 = CARTESIAN_POINT ( 'NONE',  ( 9.737023737882804397, 6.817976262117185549, 54.00000000000000711 ) ) ;
#1804 = VECTOR ( 'NONE', #62363, 1000.000000000000000 ) ;
#1805 = AXIS2_PLACEMENT_3D ( 'NONE', #44579, #17373, #38942 ) ;
#1806 = AXIS2_PLACEMENT_3D ( 'NONE', #11968, #43123, #33553 ) ;
#1808 = CARTESIAN_POINT ( 'NONE',  ( -8.227189898828745740, 1.620245201994245043, 54.00000000000000711 ) ) ;
#1807 = DIRECTION ( 'NONE',  ( -3.540251991789403884E-15, -1.000000000000000000, 0.000000000000000000 ) ) ;
#1809 = ORIENTED_EDGE ( 'NONE', *, *, #53810, .T. ) ;
#1811 = VERTEX_POINT ( 'NONE', #49039 ) ;
#1810 = DIRECTION ( 'NONE',  ( 1.000000000000000000, 0.000000000000000000, 0.000000000000000000 ) ) ;
#1812 = EDGE_LOOP ( 'NONE', ( #21750, #12453, #4821, #46142 ) ) ;
#1813 = ORIENTED_EDGE ( 'NONE', *, *, #23355, .F. ) ;
#1814 = CIRCLE ( 'NONE', #10853, 0.2000000000000005107 ) ;
#1815 = CARTESIAN_POINT ( 'NONE',  ( 9.247904806590725002, 9.942044687070426434, 455.0000000000000568 ) ) ;
#1816 = AXIS2_PLACEMENT_3D ( 'NONE', #7213, #50703, #50008 ) ;
#1817 = LINE ( 'NONE', #28008, #25247 ) ;
#1818 = CARTESIAN_POINT ( 'NONE',  ( 7.250000000000005329, -7.249999999999998224, -8.500000000000000000 ) ) ;
#1819 = VERTEX_POINT ( 'NONE', #21126 ) ;
#1820 = ORIENTED_EDGE ( 'NONE', *, *, #43998, .T. ) ;
#1821 = AXIS2_PLACEMENT_3D ( 'NONE', #4575, #30737, #41337 ) ;
#1822 = DIRECTION ( 'NONE',  ( 0.000000000000000000, 0.000000000000000000, -1.000000000000000000 ) ) ;
#1823 = LINE ( 'NONE', #12759, #9699 ) ;
#1824 = ORIENTED_EDGE ( 'NONE', *, *, #1545, .T. ) ;
#1825 = VERTEX_POINT ( 'NONE', #32082 ) ;
#1826 = DIRECTION ( 'NONE',  ( -4.745709458399858621E-16, -1.000000000000000000, 0.000000000000000000 ) ) ;
#1827 = DIRECTION ( 'NONE',  ( 0.000000000000000000, 0.000000000000000000, 1.000000000000000000 ) ) ;
#1828 = ORIENTED_EDGE ( 'NONE', *, *, #60940, .F. ) ;
#1829 = EDGE_CURVE ( 'NONE', #20348, #7353, #5223, .T. ) ;
#1830 = DIRECTION ( 'NONE',  ( -1.000000000000000000, 0.000000000000000000, 0.000000000000000000 ) ) ;
#1831 = CIRCLE ( 'NONE', #69596, 0.2000000000000005107 ) ;
#1833 = ORIENTED_EDGE ( 'NONE', *, *, #58480, .T. ) ;
#1832 = CARTESIAN_POINT ( 'NONE',  ( 6.364920264886885448, -3.677663764522618450, 26.00000000000000711 ) ) ;
#1834 = ORIENTED_EDGE ( 'NONE', *, *, #11388, .T. ) ;
#1835 = EDGE_CURVE ( 'NONE', #47486, #64753, #4652, .T. ) ;
#1836 = DIRECTION ( 'NONE',  ( 2.478176394252584099E-15, 1.000000000000000000, 0.000000000000000000 ) ) ;
#1837 = CARTESIAN_POINT ( 'NONE',  ( 11.12648345035337627, -2.906483450353491094, 455.0000000000000568 ) ) ;
#1838 = CIRCLE ( 'NONE', #28942, 3.499999999999040323 ) ;
#1839 = DIRECTION ( 'NONE',  ( -1.000000000000000000, 0.000000000000000000, 0.000000000000000000 ) ) ;
#1840 = EDGE_CURVE ( 'NONE', #19166, #11369, #36282, .T. ) ;
#1841 = CARTESIAN_POINT ( 'NONE',  ( 39.00000000000000000, 0.000000000000000000, 0.000000000000000000 ) ) ;
#1842 = EDGE_CURVE ( 'NONE', #49731, #2475, #63399, .T. ) ;
#1843 = DIRECTION ( 'NONE',  ( 0.000000000000000000, 0.000000000000000000, 1.000000000000000000 ) ) ;
#1844 = LINE ( 'NONE', #39329, #18059 ) ;
#1845 = AXIS2_PLACEMENT_3D ( 'NONE', #32567, #54131, #58738 ) ;
#1846 = AXIS2_PLACEMENT_3D ( 'NONE', #17312, #69696, #65759 ) ;
#1847 = EDGE_CURVE ( 'NONE', #52946, #36081, #39115, .T. ) ;
#1848 = EDGE_CURVE ( 'NONE', #62579, #21671, #44749, .T. ) ;
#1849 = FACE_OUTER_BOUND ( 'NONE', #5558, .T. ) ;
#1850 = ORIENTED_EDGE ( 'NONE', *, *, #6567, .T. ) ;
#1851 = LINE ( 'NONE', #23424, #50706 ) ;
#1853 = ORIENTED_EDGE ( 'NONE', *, *, #28054, .F. ) ;
#1852 = DIRECTION ( 'NONE',  ( 1.000000000000000000, -0.000000000000000000, 0.000000000000000000 ) ) ;
#1854 = VECTOR ( 'NONE', #50629, 1000.000000000000000 ) ;
#1855 = VECTOR ( 'NONE', #51255, 1000.000000000000000 ) ;
#1857 = PLANE ( 'NONE',  #30991 ) ;
#1856 = VECTOR ( 'NONE', #60431, 1000.000000000000114 ) ;
#1858 = FACE_OUTER_BOUND ( 'NONE', #31054, .T. ) ;
#1859 = ADVANCED_FACE ( 'NONE', ( #61358 ), #3533, .F. ) ;
#1860 = DIRECTION ( 'NONE',  ( -1.047444401652940007E-14, -1.000000000000000000, -1.836970198721029934E-16 ) ) ;
#1861 = LINE ( 'NONE', #28377, #65672 ) ;
#1862 = VECTOR ( 'NONE', #59394, 1000.000000000000000 ) ;
#1863 = CARTESIAN_POINT ( 'NONE',  ( 3.157023737882804770, 6.486996718459879574, 54.00000000000000711 ) ) ;
#1864 = ORIENTED_EDGE ( 'NONE', *, *, #57969, .T. ) ;
#1865 = ORIENTED_EDGE ( 'NONE', *, *, #69497, .F. ) ;
#1866 = VECTOR ( 'NONE', #43487, 1000.000000000000000 ) ;
#1867 = DIRECTION ( 'NONE',  ( 0.000000000000000000, 1.000000000000000000, 0.000000000000000000 ) ) ;
#1868 =( LENGTH_UNIT ( ) NAMED_UNIT ( * ) SI_UNIT ( .MILLI., .METRE. ) );
#1869 =( BOUNDED_CURVE ( )  B_SPLINE_CURVE ( 3, ( #40623, #13401, #30014, #8805 ),
 .UNSPECIFIED., .F., .F. ) 
 B_SPLINE_CURVE_WITH_KNOTS ( ( 4, 4 ),
 ( 0.7227342478134164416, 0.8480620789814840021 ),
 .UNSPECIFIED. ) 
 CURVE ( )  GEOMETRIC_REPRESENTATION_ITEM ( )  RATIONAL_B_SPLINE_CURVE ( ( 1.000000000000000000, 0.9986915061577686936, 0.9986915061577686936, 1.000000000000000000 ) ) 
 REPRESENTATION_ITEM ( '' )  );
#1870 = CIRCLE ( 'NONE', #41394, 1.000000000000000888 ) ;
#1871 = CARTESIAN_POINT ( 'NONE',  ( 17.51999999999999957, -15.50000000000000000, -26.00000000000000355 ) ) ;
#1872 = ORIENTED_EDGE ( 'NONE', *, *, #54165, .T. ) ;
#1873 = CARTESIAN_POINT ( 'NONE',  ( 7.450000000000006395, 7.250000000000000888, -20.50000000000000000 ) ) ;
#1874 = ORIENTED_EDGE ( 'NONE', *, *, #23682, .T. ) ;
#1875 = EDGE_LOOP ( 'NONE', ( #69414, #54797, #47049, #6618 ) ) ;
#1876 = FACE_OUTER_BOUND ( 'NONE', #61635, .T. ) ;
#1877 = DIRECTION ( 'NONE',  ( 0.000000000000000000, 1.000000000000000000, 0.000000000000000000 ) ) ;
#1878 = ORIENTED_EDGE ( 'NONE', *, *, #36967, .F. ) ;
#1879 = CARTESIAN_POINT ( 'NONE',  ( -2.752095193409509033, -9.955011587777317317, 455.0000000000000568 ) ) ;
#1880 = CARTESIAN_POINT ( 'NONE',  ( 1.866219381641426533, -9.417013320880872840, 455.0000000000000568 ) ) ;
#1881 = DIRECTION ( 'NONE',  ( -1.836970198721029934E-16, 1.836970198721036344E-16, -1.000000000000000000 ) ) ;
#1882 = ORIENTED_EDGE ( 'NONE', *, *, #8487, .T. ) ;
#1884 = ORIENTED_EDGE ( 'NONE', *, *, #34073, .T. ) ;
#1883 = PLANE ( 'NONE',  #41894 ) ;
#1885 = ADVANCED_FACE ( 'NONE', ( #16862 ), #962, .F. ) ;
#1886 = ADVANCED_FACE ( 'NONE', ( #56075 ), #49723, .T. ) ;
#1887 = CARTESIAN_POINT ( 'NONE',  ( 7.000000000000000000, -38.09999999999885034, 7.900000000002049383 ) ) ;
#1888 = CARTESIAN_POINT ( 'NONE',  ( 7.900000000000000355, -18.00000000000000355, 21.00000000000000000 ) ) ;
#1889 = CARTESIAN_POINT ( 'NONE',  ( 8.250000000000005329, 8.250000000000001776, -26.00000000000001066 ) ) ;
#1890 = DIRECTION ( 'NONE',  ( 0.8660254037844482555, 0.000000000000000000, 0.4999999999999831801 ) ) ;
#1891 = AXIS2_PLACEMENT_3D ( 'NONE', #9973, #30120, #31539 ) ;
#1892 = ADVANCED_FACE ( 'NONE', ( #11878 ), #54694, .F. ) ;
#1893 = EDGE_CURVE ( 'NONE', #37032, #63752, #50757, .T. ) ;
#1894 = CARTESIAN_POINT ( 'NONE',  ( 4.201500623656003519, -4.740315990920286104, 455.0000000000000568 ) ) ;
#1895 = CYLINDRICAL_SURFACE ( 'NONE', #21751, 0.5999999999999989786 ) ;
#1896 = PRESENTATION_LAYER_ASSIGNMENT (  '', '', ( #52752 ) ) ;
#1897 = ORIENTED_EDGE ( 'NONE', *, *, #9600, .T. ) ;
#1898 = ORIENTED_EDGE ( 'NONE', *, *, #64918, .F. ) ;
#1899 = EDGE_CURVE ( 'NONE', #27192, #49549, #59981, .T. ) ;
#1900 = VECTOR ( 'NONE', #62542, 1000.000000000000000 ) ;
#1901 = AXIS2_PLACEMENT_3D ( 'NONE', #24715, #9154, #14811 ) ;
#1902 = ORIENTED_EDGE ( 'NONE', *, *, #52669, .F. ) ;
#1903 = DIRECTION ( 'NONE',  ( 0.000000000000000000, 0.7096009616570518874, 0.7046037717862339012 ) ) ;
#1904 = FACE_OUTER_BOUND ( 'NONE', #24343, .T. ) ;
#1905 = DIRECTION ( 'NONE',  ( 0.000000000000000000, 0.000000000000000000, -1.000000000000000000 ) ) ;
#1906 = VECTOR ( 'NONE', #11858, 1000.000000000000000 ) ;
#1907 = VECTOR ( 'NONE', #23645, 1000.000000000000000 ) ;
#1908 = PRODUCT_DEFINITION_FORMATION_WITH_SPECIFIED_SOURCE ( 'ANY', '', #62794, .NOT_KNOWN. ) ;
#1909 = ORIENTED_EDGE ( 'NONE', *, *, #6875, .T. ) ;
#1910 = VERTEX_POINT ( 'NONE', #50068 ) ;
#1911 = VERTEX_POINT ( 'NONE', #55727 ) ;
#1912 = CARTESIAN_POINT ( 'NONE',  ( 30.90000000000000213, -14.06939075806900874, 20.80000000000001137 ) ) ;
#1913 = VECTOR ( 'NONE', #20902, 1000.000000000000000 ) ;
#1914 = AXIS2_PLACEMENT_3D ( 'NONE', #5914, #612, #6257 ) ;
#1915 = ORIENTED_EDGE ( 'NONE', *, *, #64017, .T. ) ;
#1916 = ORIENTED_EDGE ( 'NONE', *, *, #29294, .F. ) ;
#1917 = ORIENTED_EDGE ( 'NONE', *, *, #3301, .F. ) ;
#1918 = ORIENTED_EDGE ( 'NONE', *, *, #23000, .F. ) ;
#1919 = VECTOR ( 'NONE', #20110, 1000.000000000000000 ) ;
#1920 = CARTESIAN_POINT ( 'NONE',  ( -7.250000000000001776, -7.249999999999998224, -24.50000000000000000 ) ) ;
#1922 = ORIENTED_EDGE ( 'NONE', *, *, #30216, .F. ) ;
#1921 = DIRECTION ( 'NONE',  ( 0.000000000000000000, 1.000000000000000000, 0.000000000000000000 ) ) ;
#1923 = DIRECTION ( 'NONE',  ( 1.000000000000000000, 0.000000000000000000, 0.000000000000000000 ) ) ;
#1924 = PRODUCT_DEFINITION_SHAPE ( 'NONE', 'NONE',  #69999 ) ;
#1925 = VECTOR ( 'NONE', #33922, 1000.000000000000000 ) ;
#1926 = DIRECTION ( 'NONE',  ( 0.000000000000000000, 0.000000000000000000, 1.000000000000000000 ) ) ;
#1927 = PLANE ( 'NONE',  #35705 ) ;
#1929 = ORIENTED_EDGE ( 'NONE', *, *, #68682, .F. ) ;
#1928 = CARTESIAN_POINT ( 'NONE',  ( 3.003254798005744242, -6.872275254348403806, 26.00000000000000000 ) ) ;
#1930 = EDGE_LOOP ( 'NONE', ( #25395, #45905, #27603, #50848, #50229, #47234 ) ) ;
#1931 = CARTESIAN_POINT ( 'NONE',  ( -11.77351654964670935, 4.173516549646604901, 455.0000000000000568 ) ) ;
#1932 = DIRECTION ( 'NONE',  ( 1.000000000000000000, 0.000000000000000000, 0.000000000000000000 ) ) ;
#1933 = CARTESIAN_POINT ( 'NONE',  ( -11.77351654964679284, -7.826483450353365789, 455.0000000000000568 ) ) ;
#1934 = EDGE_CURVE ( 'NONE', #57421, #59763, #7269, .T. ) ;
#1935 = ORIENTED_EDGE ( 'NONE', *, *, #52374, .T. ) ;
#1936 = CARTESIAN_POINT ( 'NONE',  ( 37.90000000000000568, 0.000000000000000000, 0.000000000000000000 ) ) ;
#1937 = FACE_OUTER_BOUND ( 'NONE', #59015, .T. ) ;
#1938 = DIRECTION ( 'NONE',  ( 0.000000000000000000, 1.000000000000000000, 0.000000000000000000 ) ) ;
#1939 = EDGE_CURVE ( 'NONE', #21232, #11735, #66678, .T. ) ;
#1940 = VECTOR ( 'NONE', #64322, 1000.000000000000114 ) ;
#1941 = VERTEX_POINT ( 'NONE', #2327 ) ;
#1942 = DIRECTION ( 'NONE',  ( -1.836970198721029934E-16, -1.836970198721010706E-16, 1.000000000000000000 ) ) ;
#1943 = CARTESIAN_POINT ( 'NONE',  ( 283.0000000000000568, -27.13000000000000611, 13.50000000000000000 ) ) ;
#1944 = LINE ( 'NONE', #55684, #9971 ) ;
#1945 = ORIENTED_EDGE ( 'NONE', *, *, #17552, .T. ) ;
#1946 = VECTOR ( 'NONE', #44801, 1000.000000000000000 ) ;
#1947 = FACE_OUTER_BOUND ( 'NONE', #15735, .T. ) ;
#1948 = DIRECTION ( 'NONE',  ( -1.836970198721029934E-16, 1.836970198721036590E-16, -1.000000000000000000 ) ) ;
#1949 = EDGE_CURVE ( 'NONE', #587, #58549, #27821, .T. ) ;
#1950 = CARTESIAN_POINT ( 'NONE',  ( 9.562023737882761054, 2.530476262117158370, 26.00000000000000711 ) ) ;
#1951 = AXIS2_PLACEMENT_3D ( 'NONE', #12127, #12468, #60222 ) ;
#1952 = AXIS2_PLACEMENT_3D ( 'NONE', #45923, #56869, #26031 ) ;
#1953 = VERTEX_POINT ( 'NONE', #23194 ) ;
#1954 = CARTESIAN_POINT ( 'NONE',  ( 30.00000000000000000, -16.28999999999710369, 15.00000000000794920 ) ) ;
#1955 = CYLINDRICAL_SURFACE ( 'NONE', #9476, 0.1999999999999987899 ) ;
#1956 = DIRECTION ( 'NONE',  ( 0.000000000000000000, 1.000000000000000000, 0.000000000000000000 ) ) ;
#1957 = AXIS2_PLACEMENT_3D ( 'NONE', #1579, #1942, #23149 ) ;
#1958 = CARTESIAN_POINT ( 'NONE',  ( -15.50000000000000000, -0.4000000000000000222, -25.99999999999999645 ) ) ;
#1959 = VECTOR ( 'NONE', #10259, 1000.000000000000000 ) ;
#1960 = CARTESIAN_POINT ( 'NONE',  ( 3.664523737882781518, -10.31452373788279964, 26.00000000000000000 ) ) ;
#1961 = ORIENTED_EDGE ( 'NONE', *, *, #27199, .F. ) ;
#1962 = CARTESIAN_POINT ( 'NONE',  ( -15.29686605391142606, -0.2715358723588626733, -21.17390376548178210 ) ) ;
#1963 = DIRECTION ( 'NONE',  ( -0.000000000000000000, -0.000000000000000000, -1.000000000000000000 ) ) ;
#1964 = DIRECTION ( 'NONE',  ( -0.000000000000000000, -0.000000000000000000, -1.000000000000000000 ) ) ;
#1965 = CARTESIAN_POINT ( 'NONE',  ( -11.11351654964674118, -4.206483450353336373, 455.0000000000000568 ) ) ;
#1966 = DIRECTION ( 'NONE',  ( 1.000000000000000000, 0.000000000000000000, 0.000000000000000000 ) ) ;
#1967 = ORIENTED_EDGE ( 'NONE', *, *, #37147, .T. ) ;
#1969 = ORIENTED_EDGE ( 'NONE', *, *, #48362, .F. ) ;
#1968 = CARTESIAN_POINT ( 'NONE',  ( 8.144523737882806813, 8.821682069070714505, 26.00000000000000711 ) ) ;
#1970 = CIRCLE ( 'NONE', #27972, 4.000000000000000888 ) ;
#1971 = CARTESIAN_POINT ( 'NONE',  ( 17.51999999999999957, -17.50000000000000000, -26.00000000000000355 ) ) ;
#1972 = CARTESIAN_POINT ( 'NONE',  ( 106.4257688009193430, 10.00000000000000000, 334.4830310981789694 ) ) ;
#1973 = ORIENTED_EDGE ( 'NONE', *, *, #63608, .T. ) ;
#1974 = CARTESIAN_POINT ( 'NONE',  ( -10.73351654964669599, -1.690483450353341910, 455.0000000000000568 ) ) ;
#1975 = ORIENTED_EDGE ( 'NONE', *, *, #6677, .T. ) ;
#1976 = ADVANCED_FACE ( 'NONE', ( #38768 ), #60322, .F. ) ;
#1977 = CARTESIAN_POINT ( 'NONE',  ( -4.727349090213461835, 4.188533722949259186, 455.0000000000000568 ) ) ;
#1978 = VERTEX_POINT ( 'NONE', #60680 ) ;
#1979 = ORIENTED_EDGE ( 'NONE', *, *, #51944, .T. ) ;
#1980 = CARTESIAN_POINT ( 'NONE',  ( 7.250000000000005329, 7.250000000000000888, -23.50000000000000000 ) ) ;
#1981 = DIRECTION ( 'NONE',  ( 0.000000000000000000, 1.000000000000000000, 0.000000000000000000 ) ) ;
#1982 = CYLINDRICAL_SURFACE ( 'NONE', #24707, 0.1999999999999987899 ) ;
#1983 = DIRECTION ( 'NONE',  ( -1.836970198721029934E-16, 1.836970198721036344E-16, -1.000000000000000000 ) ) ;
#1984 = AXIS2_PLACEMENT_3D ( 'NONE', #44989, #1867, #2552 ) ;
#1985 = ORIENTED_EDGE ( 'NONE', *, *, #4293, .F. ) ;
#1986 = ORIENTED_EDGE ( 'NONE', *, *, #3138, .T. ) ;
#1987 = DIRECTION ( 'NONE',  ( -0.000000000000000000, 3.673940397442059868E-16, -1.000000000000000000 ) ) ;
#1988 = CARTESIAN_POINT ( 'NONE',  ( 16.89999999999999858, -14.06939075806902117, -20.80000000000000426 ) ) ;
#1989 = EDGE_CURVE ( 'NONE', #56362, #44739, #47548, .T. ) ;
#1990 = ORIENTED_EDGE ( 'NONE', *, *, #49365, .F. ) ;
#1991 = ORIENTED_EDGE ( 'NONE', *, *, #21479, .T. ) ;
#1993 = VERTEX_POINT ( 'NONE', #12227 ) ;
#1992 = ITEM_DEFINED_TRANSFORMATION ( 'NONE', 'NONE', #29004,  #45918 ) ;
#1994 = VECTOR ( 'NONE', #25777, 1000.000000000000000 ) ;
#1995 = SHAPE_REPRESENTATION ( 'LEAD SCREW', ( #45918 ), #52770 ) ;
#1996 = EDGE_CURVE ( 'NONE', #37495, #25592, #19996, .T. ) ;
#1997 = DIRECTION ( 'NONE',  ( 0.000000000000000000, -0.1249999999999996531, 0.9921567416492215186 ) ) ;
#1999 = ORIENTED_EDGE ( 'NONE', *, *, #40865, .T. ) ;
#1998 = DIRECTION ( 'NONE',  ( 0.000000000000000000, 0.000000000000000000, -1.000000000000000000 ) ) ;
#2000 = AXIS2_PLACEMENT_3D ( 'NONE', #65464, #17351, #33284 ) ;
#2001 = AXIS2_PLACEMENT_3D ( 'NONE', #69068, #14987, #42194 ) ;
#2002 = CARTESIAN_POINT ( 'NONE',  ( -4.609516549646713202, 3.593516549646603941, 455.0000000000000568 ) ) ;
#2003 = LINE ( 'NONE', #24627, #50876 ) ;
#2004 = CIRCLE ( 'NONE', #41532, 0.8128000000000145109 ) ;
#2005 = EDGE_LOOP ( 'NONE', ( #28923, #44760, #13918, #33372 ) ) ;
#2006 = ORIENTED_EDGE ( 'NONE', *, *, #4750, .T. ) ;
#2007 = CIRCLE ( 'NONE', #27961, 0.1999999999999996503 ) ;
#2008 = DIRECTION ( 'NONE',  ( 0.000000000000000000, 1.000000000000000000, 0.000000000000000000 ) ) ;
#2009 = CARTESIAN_POINT ( 'NONE',  ( 11.00000000000000000, -14.33999999999999986, -14.50000000000000000 ) ) ;
#2010 = APPLICATION_CONTEXT ( 'automotive_design' ) ;
#2011 = DIRECTION ( 'NONE',  ( 0.000000000000000000, 0.000000000000000000, -1.000000000000000000 ) ) ;
#2012 = EDGE_CURVE ( 'NONE', #55425, #68679, #66748, .T. ) ;
#2013 = AXIS2_PLACEMENT_3D ( 'NONE', #32729, #6565, #218 ) ;
#2014 = FACE_OUTER_BOUND ( 'NONE', #23892, .T. ) ;
#2015 = FACE_OUTER_BOUND ( 'NONE', #59268, .T. ) ;
#2016 = EDGE_CURVE ( 'NONE', #55203, #57776, #46157, .T. ) ;
#2017 = ADVANCED_FACE ( 'NONE', ( #30601 ), #13631, .F. ) ;
#2019 = ORIENTED_EDGE ( 'NONE', *, *, #43767, .T. ) ;
#2018 = DIRECTION ( 'NONE',  ( -1.000000000000000000, 0.000000000000000000, 0.000000000000000000 ) ) ;
#2020 = ORIENTED_EDGE ( 'NONE', *, *, #22789, .F. ) ;
#2021 = CARTESIAN_POINT ( 'NONE',  ( 13.90000000000000213, 20.60000000000000142, 13.86939075806899702 ) ) ;
#2022 = CARTESIAN_POINT ( 'NONE',  ( 33.89999999999999858, 0.000000000000000000, 2.458500000000000796 ) ) ;
#2023 = EDGE_CURVE ( 'NONE', #26897, #48692, #25302, .T. ) ;
#2024 = CYLINDRICAL_SURFACE ( 'NONE', #64138, 0.2000000000000005107 ) ;
#2025 = EDGE_CURVE ( 'NONE', #10730, #59143, #35908, .T. ) ;
#2026 = CARTESIAN_POINT ( 'NONE',  ( -7.793516549646712477, 11.11351654964660085, 455.0000000000000568 ) ) ;
#2027 = ADVANCED_FACE ( 'NONE', ( #51819 ), #8321, .T. ) ;
#2028 = VERTEX_POINT ( 'NONE', #46853 ) ;
#2029 = FACE_OUTER_BOUND ( 'NONE', #16923, .T. ) ;
#2030 = DIRECTION ( 'NONE',  ( 0.000000000000000000, 0.000000000000000000, 1.000000000000000000 ) ) ;
#2032 = EDGE_CURVE ( 'NONE', #14101, #50592, #23855, .T. ) ;
#2031 = DIRECTION ( 'NONE',  ( -0.8660254037844482555, 0.000000000000000000, 0.4999999999999831801 ) ) ;
#2033 = CARTESIAN_POINT ( 'NONE',  ( -11.77351654964674132, -4.186483450353323477, 455.0000000000000568 ) ) ;
#2034 = AXIS2_PLACEMENT_3D ( 'NONE', #68676, #52055, #52410 ) ;
#2035 = PLANE ( 'NONE',  #64269 ) ;
#2036 = DIRECTION ( 'NONE',  ( 0.000000000000000000, 0.000000000000000000, -1.000000000000000000 ) ) ;
#2037 = CARTESIAN_POINT ( 'NONE',  ( 275.0000000000000000, -21.00000000000000000, -5.000000000000000000 ) ) ;
#2038 = ORIENTED_EDGE ( 'NONE', *, *, #28352, .T. ) ;
#2039 = DIRECTION ( 'NONE',  ( -1.000000000000000000, 1.819560449471430698E-15, 1.836970198721033385E-16 ) ) ;
#2040 = CARTESIAN_POINT ( 'NONE',  ( 12.00648345035338060, -7.826483450353491023, 455.0000000000000568 ) ) ;
#2041 = VERTEX_POINT ( 'NONE', #35183 ) ;
#2042 = CARTESIAN_POINT ( 'NONE',  ( -30.00000000000000000, -12.00000000000000000, 11.03137303340310282 ) ) ;
#2043 = LINE ( 'NONE', #11941, #38994 ) ;
#2044 = CARTESIAN_POINT ( 'NONE',  ( 9.750000000000000000, -9.690000000000001279, -4.250000000000000000 ) ) ;
#2045 = CARTESIAN_POINT ( 'NONE',  ( -7.250000000000000888, 7.250000000000001776, -14.00000000000000000 ) ) ;
#2046 = CARTESIAN_POINT ( 'NONE',  ( 9.106483450353371367, 10.91351654964661222, 195.0000000000000284 ) ) ;
#2047 = ORIENTED_EDGE ( 'NONE', *, *, #25845, .T. ) ;
#2048 = CIRCLE ( 'NONE', #7689, 0.2000000000005261458 ) ;
#2049 = DIRECTION ( 'NONE',  ( 1.000000000000000000, 0.000000000000000000, 0.000000000000000000 ) ) ;
#2050 = VERTEX_POINT ( 'NONE', #29891 ) ;
#2051 = CARTESIAN_POINT ( 'NONE',  ( 283.0000000000000568, -39.79999999999905214, 12.19999999999906315 ) ) ;
#2052 = ADVANCED_FACE ( 'NONE', ( #14687 ), #51466, .F. ) ;
#2053 = ORIENTED_EDGE ( 'NONE', *, *, #14448, .F. ) ;
#2054 = LINE ( 'NONE', #20067, #3220 ) ;
#2055 = CIRCLE ( 'NONE', #65322, 0.3500000000002719824 ) ;
#2056 = EDGE_CURVE ( 'NONE', #59501, #58190, #49801, .T. ) ;
#2057 = SURFACE_STYLE_FILL_AREA ( #7000 ) ;
#2058 = DIRECTION ( 'NONE',  ( -1.000000000000000000, 1.088659024508174415E-14, 0.000000000000000000 ) ) ;
#2059 = VERTEX_POINT ( 'NONE', #36250 ) ;
#2060 = ORIENTED_EDGE ( 'NONE', *, *, #64688, .F. ) ;
#2061 = DIRECTION ( 'NONE',  ( -1.000000000000000000, 0.000000000000000000, 0.000000000000000000 ) ) ;
#2062 = ORIENTED_EDGE ( 'NONE', *, *, #67652, .T. ) ;
#2063 = VERTEX_POINT ( 'NONE', #63126 ) ;
#2064 = VECTOR ( 'NONE', #49003, 1000.000000000000000 ) ;
#2065 = PRODUCT_DEFINITION_CONTEXT ( 'detailed design', #64814, 'design' ) ;
#2066 = CYLINDRICAL_SURFACE ( 'NONE', #48548, 0.3499999999999996447 ) ;
#2067 = CARTESIAN_POINT ( 'NONE',  ( -10.30047626211725742, 6.642976262117184838, 54.00000000000000711 ) ) ;
#2068 = DIRECTION ( 'NONE',  ( 0.000000000000000000, 0.000000000000000000, 1.000000000000000000 ) ) ;
#2069 = ORIENTED_EDGE ( 'NONE', *, *, #10123, .F. ) ;
#2070 = CARTESIAN_POINT ( 'NONE',  ( 19.90000000000000213, 20.60000000000000142, -13.86939075806900057 ) ) ;
#2072 = DIRECTION ( 'NONE',  ( 1.000000000000000000, -0.000000000000000000, -0.000000000000000000 ) ) ;
#2071 = CARTESIAN_POINT ( 'NONE',  ( 7.000000000000000000, -31.30000000000000071, 12.69999999999999929 ) ) ;
#2073 = EDGE_LOOP ( 'NONE', ( #13908, #1608 ) ) ;
#2075 = ORIENTED_EDGE ( 'NONE', *, *, #44533, .F. ) ;
#2074 = CARTESIAN_POINT ( 'NONE',  ( -7.793516549646781755, -11.12648345035335851, 195.0000000000000284 ) ) ;
#2076 = ORIENTED_EDGE ( 'NONE', *, *, #56977, .F. ) ;
#2077 = DIRECTION ( 'NONE',  ( 1.000000000000000000, 0.000000000000000000, 0.000000000000000000 ) ) ;
#2078 = EDGE_CURVE ( 'NONE', #5855, #17298, #46421, .T. ) ;
#2079 = CARTESIAN_POINT ( 'NONE',  ( -7.450000000000001954, -7.249999999999998224, -15.00000000000000000 ) ) ;
#2080 = VERTEX_POINT ( 'NONE', #40142 ) ;
#2081 = CARTESIAN_POINT ( 'NONE',  ( -7.450000000000001954, -7.249999999999998224, -15.50000000000000000 ) ) ;
#2082 = DIRECTION ( 'NONE',  ( 0.000000000000000000, -0.000000000000000000, 1.000000000000000000 ) ) ;
#2083 = ORIENTED_EDGE ( 'NONE', *, *, #62101, .F. ) ;
#2084 = EDGE_CURVE ( 'NONE', #36374, #24688, #14347, .T. ) ;
#2085 = EDGE_LOOP ( 'NONE', ( #62596, #47715, #4125, #262 ) ) ;
#2086 = EDGE_CURVE ( 'NONE', #68211, #36802, #45805, .T. ) ;
#2087 = DIRECTION ( 'NONE',  ( 0.000000000000000000, -0.000000000000000000, -1.000000000000000000 ) ) ;
#2088 = CARTESIAN_POINT ( 'NONE',  ( 7.250000000000005329, 7.250000000000000888, -17.00000000000000000 ) ) ;
#2089 = ADVANCED_FACE ( 'NONE', ( #61721 ), #13282, .F. ) ;
#2090 = EDGE_CURVE ( 'NONE', #55737, #53865, #67391, .T. ) ;
#2091 = ADVANCED_FACE ( 'NONE', ( #57116, #8684 ), #30257, .F. ) ;
#2092 = EDGE_LOOP ( 'NONE', ( #50879, #11296, #52153, #39882 ) ) ;
#2093 = CARTESIAN_POINT ( 'NONE',  ( -6.642976262117260333, 9.897976262117179402, 26.00000000000000711 ) ) ;
#2094 = CARTESIAN_POINT ( 'NONE',  ( 9.703773737882810835, 9.689726262117158484, 26.00000000000000711 ) ) ;
#2095 = DIRECTION ( 'NONE',  ( -0.000000000000000000, -0.000000000000000000, -1.000000000000000000 ) ) ;
#2096 = ORIENTED_EDGE ( 'NONE', *, *, #38243, .F. ) ;
#2097 = EDGE_CURVE ( 'NONE', #45523, #65979, #94, .T. ) ;
#2098 = CIRCLE ( 'NONE', #54057, 4.000000000000000888 ) ;
#2099 = CARTESIAN_POINT ( 'NONE',  ( -7.250000000000000888, 7.250000000000001776, -18.00000000000000000 ) ) ;
#2100 = EDGE_CURVE ( 'NONE', #59106, #61047, #48858, .T. ) ;
#2101 = CARTESIAN_POINT ( 'NONE',  ( 9.562023737882814345, -2.544523737882825820, 54.00000000000000711 ) ) ;
#2103 = ORIENTED_EDGE ( 'NONE', *, *, #44517, .T. ) ;
#2102 = CARTESIAN_POINT ( 'NONE',  ( 9.737023737882783081, 3.667976262117152775, 54.00000000000000711 ) ) ;
#2105 = ORIENTED_EDGE ( 'NONE', *, *, #10566, .F. ) ;
#2104 = CARTESIAN_POINT ( 'NONE',  ( 48.66606140682858239, -0.7499999999999964473, 3.588709161325267516 ) ) ;
#2106 = EDGE_CURVE ( 'NONE', #66978, #54625, #43214, .T. ) ;
#2107 = CARTESIAN_POINT ( 'NONE',  ( -7.250000000000000888, 7.450000000000003730, -12.50000000000000000 ) ) ;
#2108 = CARTESIAN_POINT ( 'NONE',  ( 9.562023737882812569, -2.369523737882825998, 54.00000000000000711 ) ) ;
#2109 = DIRECTION ( 'NONE',  ( 0.000000000000000000, 0.000000000000000000, -1.000000000000000000 ) ) ;
#2110 = FACE_OUTER_BOUND ( 'NONE', #47645, .T. ) ;
#2111 = CARTESIAN_POINT ( 'NONE',  ( 7.250000000000005329, 8.250000000000001776, -19.00000000000000000 ) ) ;
#2112 = EDGE_CURVE ( 'NONE', #6054, #21483, #22689, .T. ) ;
#2113 = ORIENTED_EDGE ( 'NONE', *, *, #32730, .T. ) ;
#2114 = DIRECTION ( 'NONE',  ( 1.000000000000000000, 0.000000000000000000, 0.000000000000000000 ) ) ;
#2115 = DIRECTION ( 'NONE',  ( -1.000000000000000000, 0.000000000000000000, 0.000000000000000000 ) ) ;
#2117 = EDGE_CURVE ( 'NONE', #12465, #8340, #16094, .T. ) ;
#2116 = CARTESIAN_POINT ( 'NONE',  ( -4.031976262117253462, -3.157023737882814096, 26.00000000000000711 ) ) ;
#2118 = CIRCLE ( 'NONE', #41639, 0.2999999999998732569 ) ;
#2120 = ORIENTED_EDGE ( 'NONE', *, *, #67768, .T. ) ;
#2119 = CARTESIAN_POINT ( 'NONE',  ( 30.00000000000000000, -17.50000000000000000, -15.70500000000000007 ) ) ;
#2121 = CARTESIAN_POINT ( 'NONE',  ( -15.50000000000129852, -15.50000000000000000, -22.50000000000000000 ) ) ;
#2122 = DIRECTION ( 'NONE',  ( -1.000000000000000000, 0.000000000000000000, 0.000000000000000000 ) ) ;
#2123 = VERTEX_POINT ( 'NONE', #5748 ) ;
#2124 = DIRECTION ( 'NONE',  ( -0.7071067811865422437, 0.7071067811865529018, 2.597868168706500319E-16 ) ) ;
#2125 = LINE ( 'NONE', #45243, #38508 ) ;
#2126 = ORIENTED_EDGE ( 'NONE', *, *, #11507, .T. ) ;
#2127 = CARTESIAN_POINT ( 'NONE',  ( 15.00000000000000000, -25.60000000000000142, -15.10000000000000142 ) ) ;
#2128 = DIRECTION ( 'NONE',  ( 1.000000000000000000, 0.000000000000000000, 0.000000000000000000 ) ) ;
#2129 = FACE_BOUND ( 'NONE', #68189, .T. ) ;
#2130 = CARTESIAN_POINT ( 'NONE',  ( 14.75000000000000355, -0.2500000000000096589, 26.74999999999999289 ) ) ;
#2131 = FACE_OUTER_BOUND ( 'NONE', #52391, .T. ) ;
#2132 = VERTEX_POINT ( 'NONE', #28000 ) ;
#2133 = DIRECTION ( 'NONE',  ( -0.7071067811865503483, 0.7071067811865446862, 0.000000000000000000 ) ) ;
#2134 = ORIENTED_EDGE ( 'NONE', *, *, #60821, .F. ) ;
#2135 = ORIENTED_EDGE ( 'NONE', *, *, #36829, .T. ) ;
#2136 = LINE ( 'NONE', #46317, #42637 ) ;
#2137 = TOROIDAL_SURFACE ( 'NONE', #1003, 8.300000000000006040, 1.000000000000000000 ) ;
#2138 = EDGE_CURVE ( 'NONE', #5502, #8082, #32955, .T. ) ;
#2139 = CARTESIAN_POINT ( 'NONE',  ( 25.50000000000000355, 0.000000000000000000, -22.50000000000000000 ) ) ;
#2141 = LINE ( 'NONE', #23705, #51303 ) ;
#2140 = CARTESIAN_POINT ( 'NONE',  ( -10.49297626211726175, 6.835476262117182955, 26.00000000000000711 ) ) ;
#2142 = ORIENTED_EDGE ( 'NONE', *, *, #64189, .T. ) ;
#2143 = ORIENTED_EDGE ( 'NONE', *, *, #36742, .F. ) ;
#2144 = CARTESIAN_POINT ( 'NONE',  ( 275.5000000000000000, -42.50000000000000000, -26.50000000000000000 ) ) ;
#2145 = VERTEX_POINT ( 'NONE', #800 ) ;
#2146 = CIRCLE ( 'NONE', #17934, 0.1749999999999980738 ) ;
#2147 = ADVANCED_FACE ( 'NONE', ( #44243 ), #32619, .F. ) ;
#2148 = CARTESIAN_POINT ( 'NONE',  ( 3.848229544836323512, -7.357023737882812497, 54.00000000000000711 ) ) ;
#2149 = DIRECTION ( 'NONE',  ( -1.000000000000000000, 2.602085213965213008E-15, 0.000000000000000000 ) ) ;
#2150 = DIRECTION ( 'NONE',  ( -0.000000000000000000, -0.000000000000000000, -1.000000000000000000 ) ) ;
#2151 = EDGE_CURVE ( 'NONE', #52459, #69392, #22359, .T. ) ;
#2152 = CIRCLE ( 'NONE', #66502, 2.215251240775983899 ) ;
#2153 = LINE ( 'NONE', #61900, #46929 ) ;
#2155 = CARTESIAN_POINT ( 'NONE',  ( 28.00000000000000000, -15.50000000000000000, 20.05051025721700242 ) ) ;
#2154 = LINE ( 'NONE', #13808, #20810 ) ;
#2156 = VERTEX_POINT ( 'NONE', #54534 ) ;
#2157 = EDGE_CURVE ( 'NONE', #40956, #50486, #12673, .T. ) ;
#2159 = ORIENTED_EDGE ( 'NONE', *, *, #34968, .T. ) ;
#2158 = CYLINDRICAL_SURFACE ( 'NONE', #17188, 0.1999999999999987899 ) ;
#2160 = ORIENTED_EDGE ( 'NONE', *, *, #21520, .T. ) ;
#2161 = EDGE_LOOP ( 'NONE', ( #1446, #41553, #21929, #49721 ) ) ;
#2162 = AXIS2_PLACEMENT_3D ( 'NONE', #53607, #42635, #58908 ) ;
#2163 = ADVANCED_FACE ( 'NONE', ( #21658 ), #21999, .F. ) ;
#2164 = DIRECTION ( 'NONE',  ( -0.000000000000000000, -0.000000000000000000, 1.000000000000000000 ) ) ;
#2166 = AXIS2_PLACEMENT_3D ( 'NONE', #23921, #45474, #57146 ) ;
#2165 = VECTOR ( 'NONE', #62454, 1000.000000000000000 ) ;
#2167 = DIRECTION ( 'NONE',  ( 0.000000000000000000, -1.000000000000000000, 0.000000000000000000 ) ) ;
#2168 = EDGE_LOOP ( 'NONE', ( #23384, #4521, #24581, #34063 ) ) ;
#2169 = ORIENTED_EDGE ( 'NONE', *, *, #43684, .T. ) ;
#2170 = EDGE_CURVE ( 'NONE', #54089, #37232, #43561, .T. ) ;
#2171 = AXIS2_PLACEMENT_3D ( 'NONE', #40725, #66546, #67248 ) ;
#2172 = DIRECTION ( 'NONE',  ( 0.5000000000000018874, 0.8660254037844374864, 0.000000000000000000 ) ) ;
#2173 = CARTESIAN_POINT ( 'NONE',  ( 25.57999999999999829, 0.000000000000000000, 0.000000000000000000 ) ) ;
#2174 = ORIENTED_EDGE ( 'NONE', *, *, #51095, .F. ) ;
#2175 = EDGE_CURVE ( 'NONE', #18730, #21397, #26965, .T. ) ;
#2176 = EDGE_CURVE ( 'NONE', #69782, #34171, #6089, .T. ) ;
#2177 = VERTEX_POINT ( 'NONE', #48527 ) ;
#2178 = PLANE ( 'NONE',  #57907 ) ;
#2179 = CARTESIAN_POINT ( 'NONE',  ( 11.00000000000000000, -5.200000000000001066, -9.400000000000000355 ) ) ;
#2180 = ORIENTED_EDGE ( 'NONE', *, *, #29330, .T. ) ;
#2181 = EDGE_CURVE ( 'NONE', #66583, #36010, #60164, .T. ) ;
#2182 = CARTESIAN_POINT ( 'NONE',  ( 10.20488345035338185, -9.804883450353433005, 195.0000000000000284 ) ) ;
#2183 = VECTOR ( 'NONE', #64370, 1000.000000000000000 ) ;
#2184 = LINE ( 'NONE', #29742, #62149 ) ;
#2186 = ORIENTED_EDGE ( 'NONE', *, *, #24408, .T. ) ;
#2185 = CARTESIAN_POINT ( 'NONE',  ( 40.90000000000000568, -16.96999999999999886, 21.00000000000000000 ) ) ;
#2187 = EDGE_LOOP ( 'NONE', ( #7754, #52608, #38102, #50654 ) ) ;
#2188 = DIRECTION ( 'NONE',  ( -1.000000000000000000, -2.135044278125301343E-15, 0.000000000000000000 ) ) ;
#2189 = LINE ( 'NONE', #18090, #57170 ) ;
#2190 = CARTESIAN_POINT ( 'NONE',  ( -8.250000000000001776, -7.249999999999998224, -21.00000000000000000 ) ) ;
#2191 = CARTESIAN_POINT ( 'NONE',  ( 8.406483450353379183, -7.616533956692230767, 195.0000000000000284 ) ) ;
#2192 = DIRECTION ( 'NONE',  ( 1.000000000000000000, 0.000000000000000000, 0.000000000000000000 ) ) ;
#2193 = LINE ( 'NONE', #23761, #7915 ) ;
#2194 = FACE_OUTER_BOUND ( 'NONE', #18891, .T. ) ;
#2195 = EDGE_CURVE ( 'NONE', #66560, #16506, #36375, .T. ) ;
#2196 = EDGE_LOOP ( 'NONE', ( #38925, #20069, #46346, #38174 ) ) ;
#2197 = DIRECTION ( 'NONE',  ( -1.000000000000000000, -1.084202172485504434E-16, 0.000000000000000000 ) ) ;
#2198 = VECTOR ( 'NONE', #62489, 1000.000000000000000 ) ;
#2201 = ORIENTED_EDGE ( 'NONE', *, *, #56952, .T. ) ;
#2200 = EDGE_CURVE ( 'NONE', #37027, #7815, #6437, .T. ) ;
#2199 = CARTESIAN_POINT ( 'NONE',  ( -9.390476262117209316, -1.480523737882732060, 54.00000000000000711 ) ) ;
#2202 = PLANE ( 'NONE',  #24225 ) ;
#2203 = PLANE ( 'NONE',  #61687 ) ;
#2204 = CARTESIAN_POINT ( 'NONE',  ( 10.20488345035338007, -11.48848345035349361, 455.0000000000000568 ) ) ;
#2205 = DIRECTION ( 'NONE',  ( -5.163402228214836012E-15, -1.000000000000000000, -1.836970198721026976E-16 ) ) ;
#2206 = CARTESIAN_POINT ( 'NONE',  ( 283.0000000000000568, -27.13000000000000611, -13.50000000000000000 ) ) ;
#2207 = ORIENTED_EDGE ( 'NONE', *, *, #13982, .F. ) ;
#2208 = ORIENTED_EDGE ( 'NONE', *, *, #34444, .F. ) ;
#2209 = VECTOR ( 'NONE', #42059, 1000.000000000000114 ) ;
#2210 = CARTESIAN_POINT ( 'NONE',  ( -7.250000000000000888, 7.450000000000003730, -18.00000000000000000 ) ) ;
#2211 = CARTESIAN_POINT ( 'NONE',  ( 7.250000000000005329, -7.249999999999998224, -20.50000000000000000 ) ) ;
#2212 = VECTOR ( 'NONE', #34453, 1000.000000000000000 ) ;
#2213 = FACE_BOUND ( 'NONE', #64525, .T. ) ;
#2214 = ORIENTED_EDGE ( 'NONE', *, *, #35787, .F. ) ;
#2215 = DIRECTION ( 'NONE',  ( 1.000000000000000000, -0.000000000000000000, -0.000000000000000000 ) ) ;
#2216 = EDGE_LOOP ( 'NONE', ( #62847, #12809, #40061, #13416 ) ) ;
#2217 = VERTEX_POINT ( 'NONE', #12067 ) ;
#2218 = DIRECTION ( 'NONE',  ( 0.000000000000000000, -1.000000000000000000, 0.000000000000000000 ) ) ;
#2219 = VECTOR ( 'NONE', #7218, 1000.000000000000000 ) ;
#2220 = LINE ( 'NONE', #9989, #10523 ) ;
#2221 = ORIENTED_EDGE ( 'NONE', *, *, #37349, .F. ) ;
#2222 = DIRECTION ( 'NONE',  ( 0.000000000000000000, 0.000000000000000000, 1.000000000000000000 ) ) ;
#2223 = LINE ( 'NONE', #1880, #6116 ) ;
#2224 = CARTESIAN_POINT ( 'NONE',  ( -6.350872789121327244, 6.822336235477381550, 54.00000000000000711 ) ) ;
#2225 = ORIENTED_EDGE ( 'NONE', *, *, #20728, .F. ) ;
#2226 = ORIENTED_EDGE ( 'NONE', *, *, #54155, .F. ) ;
#2228 = ORIENTED_EDGE ( 'NONE', *, *, #52293, .F. ) ;
#2227 = CARTESIAN_POINT ( 'NONE',  ( 2.906483450353342324, -11.12648345035346331, 455.0000000000000568 ) ) ;
#2229 = EDGE_LOOP ( 'NONE', ( #30375, #8867, #7920, #42250 ) ) ;
#2230 = EDGE_CURVE ( 'NONE', #2766, #7775, #69754, .T. ) ;
#2231 = DIRECTION ( 'NONE',  ( -1.000000000000000000, 0.000000000000000000, 0.000000000000000000 ) ) ;
#2232 = DIRECTION ( 'NONE',  ( 0.000000000000000000, 0.000000000000000000, 1.000000000000000000 ) ) ;
#2233 = CARTESIAN_POINT ( 'NONE',  ( 49.00000000000000000, -0.1999999999911795112, 8.826273045769999343E-12 ) ) ;
#2234 = AXIS2_PLACEMENT_3D ( 'NONE', #48982, #69493, #59234 ) ;
#2235 = DIRECTION ( 'NONE',  ( -1.000000000000000000, 0.000000000000000000, 0.000000000000000000 ) ) ;
#2236 = EDGE_CURVE ( 'NONE', #61067, #1462, #21311, .T. ) ;
#2237 = LINE ( 'NONE', #34390, #32211 ) ;
#2238 = LINE ( 'NONE', #51027, #30787 ) ;
#2239 = ADVANCED_FACE ( 'NONE', ( #28329 ), #19119, .T. ) ;
#2240 = ORIENTED_EDGE ( 'NONE', *, *, #46153, .F. ) ;
#2241 = ORIENTED_EDGE ( 'NONE', *, *, #59283, .T. ) ;
#2242 = ADVANCED_FACE ( 'NONE', ( #40688 ), #17732, .F. ) ;
#2243 = ORIENTED_EDGE ( 'NONE', *, *, #19085, .T. ) ;
#2244 = ORIENTED_EDGE ( 'NONE', *, *, #66501, .F. ) ;
#2245 = DIRECTION ( 'NONE',  ( 0.000000000000000000, 0.000000000000000000, -1.000000000000000000 ) ) ;
#2246 = ADVANCED_FACE ( 'NONE', ( #50246 ), #39627, .F. ) ;
#2247 = EDGE_CURVE ( 'NONE', #11267, #58003, #18402, .T. ) ;
#2248 = DIRECTION ( 'NONE',  ( 3.540573132209560831E-15, 1.000000000000000000, 0.000000000000000000 ) ) ;
#2249 = AXIS2_PLACEMENT_3D ( 'NONE', #19984, #47557, #41895 ) ;
#2250 = AXIS2_PLACEMENT_3D ( 'NONE', #26432, #6601, #27824 ) ;
#2251 = CARTESIAN_POINT ( 'NONE',  ( -7.450000000000001954, -7.249999999999998224, -9.000000000000001776 ) ) ;
#2252 = DIRECTION ( 'NONE',  ( 0.000000000000000000, 0.000000000000000000, 1.000000000000000000 ) ) ;
#2253 = AXIS2_PLACEMENT_3D ( 'NONE', #30312, #18636, #24657 ) ;
#2254 = ADVANCED_FACE ( 'NONE', ( #7457 ), #66166, .T. ) ;
#2255 = ORIENTED_EDGE ( 'NONE', *, *, #31102, .F. ) ;
#2256 = ORIENTED_EDGE ( 'NONE', *, *, #22911, .T. ) ;
#2257 = VERTEX_POINT ( 'NONE', #23382 ) ;
#2258 = AXIS2_PLACEMENT_3D ( 'NONE', #60030, #16573, #11580 ) ;
#2259 = DIRECTION ( 'NONE',  ( 0.000000000000000000, 1.000000000000000000, 0.000000000000000000 ) ) ;
#2260 = ORIENTED_EDGE ( 'NONE', *, *, #66512, .F. ) ;
#2261 = VERTEX_POINT ( 'NONE', #39292 ) ;
#2262 = ORIENTED_EDGE ( 'NONE', *, *, #11342, .F. ) ;
#2263 = AXIS2_PLACEMENT_3D ( 'NONE', #34558, #40913, #24663 ) ;
#2264 = ORIENTED_EDGE ( 'NONE', *, *, #25922, .T. ) ;
#2265 = DIRECTION ( 'NONE',  ( 0.000000000000000000, 0.000000000000000000, 1.000000000000000000 ) ) ;
#2267 = ORIENTED_EDGE ( 'NONE', *, *, #16073, .F. ) ;
#2266 = CARTESIAN_POINT ( 'NONE',  ( -7.250000000000000888, 7.450000000000003730, -25.50000000000000355 ) ) ;
#2268 = AXIS2_PLACEMENT_3D ( 'NONE', #16757, #38326, #64167 ) ;
#2269 = PLANE ( 'NONE',  #43619 ) ;
#2270 = CARTESIAN_POINT ( 'NONE',  ( -7.250000000000000888, 7.450000000000003730, -7.500000000000000000 ) ) ;
#2271 = DIRECTION ( 'NONE',  ( 7.457533623526253657E-15, 1.000000000000000000, 0.000000000000000000 ) ) ;
#2273 = VERTEX_POINT ( 'NONE', #34675 ) ;
#2272 = CARTESIAN_POINT ( 'NONE',  ( -7.250000000000000888, 7.250000000000001776, -16.50000000000000000 ) ) ;
#2274 = ORIENTED_EDGE ( 'NONE', *, *, #51239, .T. ) ;
#2275 = AXIS2_PLACEMENT_3D ( 'NONE', #4400, #54225, #27350 ) ;
#2276 = AXIS2_PLACEMENT_3D ( 'NONE', #31674, #47232, #14698 ) ;
#2277 = LINE ( 'NONE', #66968, #53206 ) ;
#2278 = DIRECTION ( 'NONE',  ( 2.135044278125299371E-15, 1.000000000000000000, 0.000000000000000000 ) ) ;
#2279 = DIRECTION ( 'NONE',  ( 0.000000000000000000, 0.000000000000000000, 1.000000000000000000 ) ) ;
#2280 = EDGE_LOOP ( 'NONE', ( #11523, #12923, #40662, #61638 ) ) ;
#2281 = DIRECTION ( 'NONE',  ( 1.000000000000000000, -1.261617073437657577E-14, 0.000000000000000000 ) ) ;
#2282 = EDGE_CURVE ( 'NONE', #18722, #29792, #61186, .T. ) ;
#2283 = PLANE ( 'NONE',  #26407 ) ;
#2284 = LINE ( 'NONE', #8636, #61637 ) ;
#2285 = CIRCLE ( 'NONE', #12462, 0.5000000000023407942 ) ;
#2286 = ORIENTED_EDGE ( 'NONE', *, *, #28874, .T. ) ;
#2287 = EDGE_CURVE ( 'NONE', #34666, #20953, #4792, .T. ) ;
#2288 = CYLINDRICAL_SURFACE ( 'NONE', #68602, 4.500000000000188294 ) ;
#2289 = FACE_BOUND ( 'NONE', #31446, .T. ) ;
#2290 = LINE ( 'NONE', #34443, #44964 ) ;
#2291 = ADVANCED_FACE ( 'NONE', ( #2502 ), #55217, .T. ) ;
#2292 = ADVANCED_FACE ( 'NONE', ( #44943 ), #34314, .F. ) ;
#2293 = ORIENTED_EDGE ( 'NONE', *, *, #51053, .T. ) ;
#2294 = CARTESIAN_POINT ( 'NONE',  ( -11.50000000000000000, -12.00000000000000000, 10.52786404500095863 ) ) ;
#2295 = PLANE ( 'NONE',  #37676 ) ;
#2296 = AXIS2_PLACEMENT_3D ( 'NONE', #68979, #62266, #46706 ) ;
#2297 = CARTESIAN_POINT ( 'NONE',  ( 11.18999999999999950, 11.25000000000000178, -4.250000000000000000 ) ) ;
#2298 = DIRECTION ( 'NONE',  ( 0.000000000000000000, 0.000000000000000000, 1.000000000000000000 ) ) ;
#2299 = EDGE_LOOP ( 'NONE', ( #3724, #49032, #30876, #8902, #49888, #43618, #33137, #12672, #4862, #55127, #14124, #28234, #69378, #2404, #30624, #11403 ) ) ;
#2300 = FACE_OUTER_BOUND ( 'NONE', #60861, .T. ) ;
#2301 = CARTESIAN_POINT ( 'NONE',  ( 10.31452373788280674, 6.835476262117182067, 54.00000000000000711 ) ) ;
#2302 = DIRECTION ( 'NONE',  ( -1.000000000000000000, 0.000000000000000000, 0.000000000000000000 ) ) ;
#2303 = AXIS2_PLACEMENT_3D ( 'NONE', #67615, #35779, #39417 ) ;
#2304 = CARTESIAN_POINT ( 'NONE',  ( 0.000000000000000000, -8.249999999999998224, -21.50000000000000000 ) ) ;
#2305 = CARTESIAN_POINT ( 'NONE',  ( -10.91351654964670637, 2.693516549646604030, 195.0000000000000284 ) ) ;
#2306 = ORIENTED_EDGE ( 'NONE', *, *, #38956, .T. ) ;
#2307 = CARTESIAN_POINT ( 'NONE',  ( -12.00854180281611328, 7.798491296477224388, 195.0000000000000284 ) ) ;
#2308 = LINE ( 'NONE', #23872, #13602 ) ;
#2309 = DIRECTION ( 'NONE',  ( -5.981805089575196197E-17, -1.000000000000000000, 0.000000000000000000 ) ) ;
#2310 = VECTOR ( 'NONE', #48676, 1000.000000000000000 ) ;
#2311 = DIRECTION ( 'NONE',  ( 1.000000000000000000, 0.000000000000000000, 0.000000000000000000 ) ) ;
#2312 = AXIS2_PLACEMENT_3D ( 'NONE', #15326, #32283, #31597 ) ;
#2313 = ORIENTED_EDGE ( 'NONE', *, *, #68299, .F. ) ;
#2315 = ORIENTED_EDGE ( 'NONE', *, *, #9003, .T. ) ;
#2314 = CARTESIAN_POINT ( 'NONE',  ( 8.250000000000005329, -8.249999999999998224, -26.00000000000001066 ) ) ;
#2316 = EDGE_CURVE ( 'NONE', #59292, #38183, #38654, .T. ) ;
#2317 = DIRECTION ( 'NONE',  ( -0.000000000000000000, -0.000000000000000000, -1.000000000000000000 ) ) ;
#2318 = DIRECTION ( 'NONE',  ( 0.000000000000000000, 1.000000000000000000, 0.000000000000000000 ) ) ;
#2319 = VERTEX_POINT ( 'NONE', #55558 ) ;
#2320 = VECTOR ( 'NONE', #388, 1000.000000000000000 ) ;
#2321 = AXIS2_PLACEMENT_3D ( 'NONE', #18503, #61639, #13210 ) ;
#2322 = FACE_OUTER_BOUND ( 'NONE', #4311, .T. ) ;
#2323 = ORIENTED_EDGE ( 'NONE', *, *, #16232, .T. ) ;
#2324 = CARTESIAN_POINT ( 'NONE',  ( -14.25000000000000000, -0.2038245569916330158, -23.22168783648699986 ) ) ;
#2325 = ORIENTED_EDGE ( 'NONE', *, *, #64520, .T. ) ;
#2326 = VERTEX_POINT ( 'NONE', #55901 ) ;
#2327 = CARTESIAN_POINT ( 'NONE',  ( -15.50000000000000000, -17.50000000000000000, -25.99999999999985079 ) ) ;
#2328 = ADVANCED_FACE ( 'NONE', ( #56254 ), #29031, .F. ) ;
#2329 = ADVANCED_FACE ( 'NONE', ( #50601 ), #2158, .T. ) ;
#2330 = LINE ( 'NONE', #18232, #35409 ) ;
#2331 = CARTESIAN_POINT ( 'NONE',  ( 30.00000000000000000, -9.199999999999999289, 12.69999999999986073 ) ) ;
#2332 = CYLINDRICAL_SURFACE ( 'NONE', #39309, 24.99999999998794920 ) ;
#2333 = EDGE_CURVE ( 'NONE', #25742, #5708, #39967, .T. ) ;
#2334 = VECTOR ( 'NONE', #12590, 1000.000000000000000 ) ;
#2335 = ORIENTED_EDGE ( 'NONE', *, *, #39615, .F. ) ;
#2336 = ORIENTED_EDGE ( 'NONE', *, *, #65118, .T. ) ;
#2337 = DIRECTION ( 'NONE',  ( -0.4999999999989361843, 0.000000000000000000, 0.8660254037850529940 ) ) ;
#2338 = DIRECTION ( 'NONE',  ( 8.673617379884087537E-15, 1.000000000000000000, 0.000000000000000000 ) ) ;
#2339 = VERTEX_POINT ( 'NONE', #45627 ) ;
#2340 = ORIENTED_EDGE ( 'NONE', *, *, #50487, .T. ) ;
#2341 = ORIENTED_EDGE ( 'NONE', *, *, #2759, .T. ) ;
#2342 = LINE ( 'NONE', #22869, #3348 ) ;
#2343 = AXIS2_PLACEMENT_3D ( 'NONE', #3500, #24710, #19397 ) ;
#2345 = VERTEX_POINT ( 'NONE', #13462 ) ;
#2344 = DIRECTION ( 'NONE',  ( -1.000000000000000000, 0.000000000000000000, 0.000000000000000000 ) ) ;
#2346 = CARTESIAN_POINT ( 'NONE',  ( -8.130476262117316111, -8.835729544836294025, 54.00000000000000711 ) ) ;
#2347 = PRODUCT_DEFINITION_SHAPE ( 'NONE', 'NONE',  #61644 ) ;
#2348 = AXIS2_PLACEMENT_3D ( 'NONE', #68413, #19967, #26326 ) ;
#2349 = LINE ( 'NONE', #29206, #63370 ) ;
#2350 = EDGE_LOOP ( 'NONE', ( #756, #58061, #29808, #46109 ) ) ;
#2351 = AXIS2_PLACEMENT_3D ( 'NONE', #60475, #56222, #34638 ) ;
#2352 = ORIENTED_EDGE ( 'NONE', *, *, #66934, .T. ) ;
#2353 = AXIS2_PLACEMENT_3D ( 'NONE', #35085, #12474, #55625 ) ;
#2354 = AXIS2_PLACEMENT_3D ( 'NONE', #339, #693, #53051 ) ;
#2355 = FACE_OUTER_BOUND ( 'NONE', #33408, .T. ) ;
#2356 = DIRECTION ( 'NONE',  ( 0.000000000000000000, 0.000000000000000000, -1.000000000000000000 ) ) ;
#2357 = DIRECTION ( 'NONE',  ( -1.000000000000000000, 9.799566706031580591E-15, 1.836970198721047683E-16 ) ) ;
#2358 = VECTOR ( 'NONE', #30939, 1000.000000000000000 ) ;
#2359 = CARTESIAN_POINT ( 'NONE',  ( 49.00000000000000000, -14.06939075806900163, -20.80000000000000426 ) ) ;
#2360 = DIRECTION ( 'NONE',  ( 1.000000000000000000, 0.000000000000000000, 0.000000000000000000 ) ) ;
#2362 = ORIENTED_EDGE ( 'NONE', *, *, #6675, .F. ) ;
#2361 = LINE ( 'NONE', #47257, #21860 ) ;
#2363 = ORIENTED_EDGE ( 'NONE', *, *, #27751, .F. ) ;
#2364 = EDGE_CURVE ( 'NONE', #53484, #9595, #62357, .T. ) ;
#2365 = CARTESIAN_POINT ( 'NONE',  ( -8.393516549646712122, 5.655420232009161552, 455.0000000000000568 ) ) ;
#2366 = EDGE_CURVE ( 'NONE', #29539, #17564, #31902, .T. ) ;
#2367 = ADVANCED_FACE ( 'NONE', ( #58002 ), #26186, .F. ) ;
#2368 = CIRCLE ( 'NONE', #48668, 4.000000000000000888 ) ;
#2369 = CARTESIAN_POINT ( 'NONE',  ( -7.450000000000001954, 7.250000000000000000, -17.50000000000000000 ) ) ;
#2370 = CARTESIAN_POINT ( 'NONE',  ( -29.50000000000000355, -11.50000000000000000, 15.00000000000000000 ) ) ;
#2371 = EDGE_CURVE ( 'NONE', #4784, #36435, #56940, .T. ) ;
#2372 = DIRECTION ( 'NONE',  ( 1.000000000000000000, -5.163402228214836012E-15, -1.836970198721039548E-16 ) ) ;
#2373 = ORIENTED_EDGE ( 'NONE', *, *, #47915, .T. ) ;
#2374 = DIRECTION ( 'NONE',  ( -3.491481338843133355E-15, -1.000000000000000000, 0.000000000000000000 ) ) ;
#2375 = PLANE ( 'NONE',  #28245 ) ;
#2376 = LINE ( 'NONE', #23939, #14254 ) ;
#2377 = CYLINDRICAL_SURFACE ( 'NONE', #19870, 0.1749999999999998224 ) ;
#2378 = VECTOR ( 'NONE', #58559, 1000.000000000000000 ) ;
#2379 = CARTESIAN_POINT ( 'NONE',  ( -30.00000000000000000, -17.14999999999999858, -27.00000000000000000 ) ) ;
#2380 = LINE ( 'NONE', #46903, #22864 ) ;
#2381 = CARTESIAN_POINT ( 'NONE',  ( 7.250000000000005329, 7.250000000000000888, -20.00000000000000000 ) ) ;
#2382 = VERTEX_POINT ( 'NONE', #68622 ) ;
#2383 = FACE_OUTER_BOUND ( 'NONE', #44834, .T. ) ;
#2384 = LINE ( 'NONE', #67449, #66601 ) ;
#2385 = ORIENTED_EDGE ( 'NONE', *, *, #45734, .F. ) ;
#2386 = DIRECTION ( 'NONE',  ( 8.673617379884087537E-15, 1.000000000000000000, 0.000000000000000000 ) ) ;
#2387 = DIRECTION ( 'NONE',  ( 0.000000000000000000, 3.673940397442059868E-16, -1.000000000000000000 ) ) ;
#2388 = CARTESIAN_POINT ( 'NONE',  ( 275.0000000000000000, -42.00000000000000000, -26.50000000000000000 ) ) ;
#2389 = LINE ( 'NONE', #8379, #24068 ) ;
#2390 = CARTESIAN_POINT ( 'NONE',  ( 0.000000000000000000, -8.749999999999998224, -26.00000000000001066 ) ) ;
#2391 = VECTOR ( 'NONE', #65517, 1000.000000000000000 ) ;
#2392 = VERTEX_POINT ( 'NONE', #47741 ) ;
#2393 = CARTESIAN_POINT ( 'NONE',  ( 41.09999999999999432, 20.60000000000000142, -13.86939075806900057 ) ) ;
#2394 = VECTOR ( 'NONE', #45651, 1000.000000000000000 ) ;
#2395 = VERTEX_POINT ( 'NONE', #15228 ) ;
#2396 = DIRECTION ( 'NONE',  ( 1.073876437509453175E-14, 1.000000000000000000, 0.000000000000000000 ) ) ;
#2397 = ORIENTED_EDGE ( 'NONE', *, *, #30198, .F. ) ;
#2398 = FACE_OUTER_BOUND ( 'NONE', #46831, .T. ) ;
#2399 = ORIENTED_EDGE ( 'NONE', *, *, #11737, .T. ) ;
#2400 = AXIS2_PLACEMENT_3D ( 'NONE', #42936, #53913, #22423 ) ;
#2401 = AXIS2_PLACEMENT_3D ( 'NONE', #55386, #6924, #28834 ) ;
#2402 = DIRECTION ( 'NONE',  ( 0.000000000000000000, -0.9921567416492215186, 0.1249999999999996531 ) ) ;
#2403 = ORIENTED_EDGE ( 'NONE', *, *, #4156, .T. ) ;
#2404 = ORIENTED_EDGE ( 'NONE', *, *, #34068, .F. ) ;
#2405 = CARTESIAN_POINT ( 'NONE',  ( -13.00000000000000178, -16.28999999999710369, -15.00000000000794920 ) ) ;
#2406 = EDGE_LOOP ( 'NONE', ( #14702, #53614, #42844, #43327 ) ) ;
#2407 = VECTOR ( 'NONE', #5030, 1000.000000000000000 ) ;
#2408 = EDGE_LOOP ( 'NONE', ( #21125, #20626, #64503, #8577 ) ) ;
#2409 = EDGE_CURVE ( 'NONE', #54217, #10955, #51106, .T. ) ;
#2410 = CARTESIAN_POINT ( 'NONE',  ( -10.49297626211729018, -6.849523737882743823, 26.00000000000000000 ) ) ;
#2411 = CARTESIAN_POINT ( 'NONE',  ( 22.90000000000000213, 13.66939075806899240, -20.79999999999999361 ) ) ;
#2412 = CARTESIAN_POINT ( 'NONE',  ( -4.193516549646831848, -11.12648345035344377, 455.0000000000000568 ) ) ;
#2413 = EDGE_CURVE ( 'NONE', #3133, #53573, #22890, .T. ) ;
#2414 = ADVANCED_FACE ( 'NONE', ( #3566 ), #23993, .F. ) ;
#2415 = VERTEX_POINT ( 'NONE', #57652 ) ;
#2416 = CARTESIAN_POINT ( 'NONE',  ( -7.450000000000001954, 7.250000000000000000, -15.50000000000000000 ) ) ;
#2417 = AXIS2_PLACEMENT_3D ( 'NONE', #12115, #45675, #38655 ) ;
#2419 = DIRECTION ( 'NONE',  ( 0.000000000000000000, 0.000000000000000000, -1.000000000000000000 ) ) ;
#2418 = CARTESIAN_POINT ( 'NONE',  ( 275.0000000000000000, -30.80000000000000071, -8.900000000000000355 ) ) ;
#2420 = ORIENTED_EDGE ( 'NONE', *, *, #58009, .T. ) ;
#2423 = ORIENTED_EDGE ( 'NONE', *, *, #68126, .F. ) ;
#2422 = ADVANCED_FACE ( 'NONE', ( #9572 ), #8499, .F. ) ;
#2421 = DIRECTION ( 'NONE',  ( -0.000000000000000000, 3.673940397442059868E-16, -1.000000000000000000 ) ) ;
#2424 = VERTEX_POINT ( 'NONE', #68262 ) ;
#2425 = EDGE_CURVE ( 'NONE', #8140, #23746, #53068, .T. ) ;
#2426 = APPLICATION_PROTOCOL_DEFINITION ( 'draft international standard', 'automotive_design', 1998, #56227 ) ;
#2427 = EDGE_CURVE ( 'NONE', #33149, #36598, #20174, .T. ) ;
#2428 = DIRECTION ( 'NONE',  ( 0.000000000000000000, 0.000000000000000000, 1.000000000000000000 ) ) ;
#2429 = EDGE_CURVE ( 'NONE', #3011, #6950, #52358, .T. ) ;
#2430 = ORIENTED_EDGE ( 'NONE', *, *, #3927, .T. ) ;
#2431 = DIRECTION ( 'NONE',  ( -3.540573132209561620E-15, -1.000000000000000000, 0.000000000000000000 ) ) ;
#2432 = LINE ( 'NONE', #62882, #54244 ) ;
#2433 = ORIENTED_EDGE ( 'NONE', *, *, #27594, .F. ) ;
#2434 = ORIENTED_EDGE ( 'NONE', *, *, #9596, .F. ) ;
#2435 = LINE ( 'NONE', #28605, #32407 ) ;
#2436 = DIRECTION ( 'NONE',  ( 0.000000000000000000, -1.000000000000000000, 0.000000000000000000 ) ) ;
#2437 = ORIENTED_EDGE ( 'NONE', *, *, #36456, .F. ) ;
#2438 = LINE ( 'NONE', #51223, #26802 ) ;
#2439 = FACE_OUTER_BOUND ( 'NONE', #38568, .T. ) ;
#2440 = DIRECTION ( 'NONE',  ( 0.000000000000000000, -1.000000000000000000, -3.673940397442059868E-16 ) ) ;
#2441 = AXIS2_PLACEMENT_3D ( 'NONE', #6036, #10297, #26560 ) ;
#2442 = ORIENTED_EDGE ( 'NONE', *, *, #45546, .T. ) ;
#2443 = LINE ( 'NONE', #17668, #50449 ) ;
#2444 = LINE ( 'NONE', #57241, #10004 ) ;
#2446 = ORIENTED_EDGE ( 'NONE', *, *, #23329, .F. ) ;
#2445 = DIRECTION ( 'NONE',  ( 0.000000000000000000, 0.000000000000000000, -1.000000000000000000 ) ) ;
#2448 = ORIENTED_EDGE ( 'NONE', *, *, #36008, .F. ) ;
#2447 = DIRECTION ( 'NONE',  ( 0.000000000000000000, 1.000000000000000000, 0.000000000000000000 ) ) ;
#2449 = CYLINDRICAL_SURFACE ( 'NONE', #37417, 24.99999999998784972 ) ;
#2450 = DIRECTION ( 'NONE',  ( -0.000000000000000000, 0.000000000000000000, 1.000000000000000000 ) ) ;
#2451 = DIRECTION ( 'NONE',  ( -0.000000000000000000, 1.000000000000000000, -0.000000000000000000 ) ) ;
#2452 = VECTOR ( 'NONE', #50922, 1000.000000000000000 ) ;
#2453 = CLOSED_SHELL ( 'NONE', ( #68580, #27616, #53861, #6340, #58274, #29581 ) ) ;
#2454 = CARTESIAN_POINT ( 'NONE',  ( 7.500000000000000000, -20.40000000000000213, 20.00000000000000000 ) ) ;
#2455 = DIRECTION ( 'NONE',  ( -1.000000000000000000, 0.000000000000000000, 0.000000000000000000 ) ) ;
#2456 = ORIENTED_EDGE ( 'NONE', *, *, #33545, .T. ) ;
#2457 = DIRECTION ( 'NONE',  ( 0.000000000000000000, 0.000000000000000000, 1.000000000000000000 ) ) ;
#2458 = DIRECTION ( 'NONE',  ( 0.000000000000000000, 0.000000000000000000, -1.000000000000000000 ) ) ;
#2460 = EDGE_LOOP ( 'NONE', ( #4758, #41144, #40239, #41807 ) ) ;
#2459 = DIRECTION ( 'NONE',  ( 0.000000000000000000, -1.000000000000000000, 0.000000000000000000 ) ) ;
#2461 = LINE ( 'NONE', #66123, #65157 ) ;
#2462 = LINE ( 'NONE', #24027, #12594 ) ;
#2463 = CIRCLE ( 'NONE', #30697, 0.3999999999999993006 ) ;
#2464 = ADVANCED_FACE ( 'NONE', ( #30079 ), #46338, .T. ) ;
#2465 = VERTEX_POINT ( 'NONE', #63313 ) ;
#2466 = DIRECTION ( 'NONE',  ( 0.000000000000000000, 1.000000000000000000, 0.000000000000000000 ) ) ;
#2467 = DIRECTION ( 'NONE',  ( 0.000000000000000000, -1.000000000000000000, 0.000000000000000000 ) ) ;
#2468 = ORIENTED_EDGE ( 'NONE', *, *, #1113, .F. ) ;
#2469 = DIRECTION ( 'NONE',  ( 0.000000000000000000, 0.000000000000000000, -1.000000000000000000 ) ) ;
#2470 = DIRECTION ( 'NONE',  ( -1.000000000000000000, 0.000000000000000000, 0.000000000000000000 ) ) ;
#2471 = CARTESIAN_POINT ( 'NONE',  ( 7.000000000000000000, -31.30000000000000071, -12.69999999999999929 ) ) ;
#2472 = EDGE_CURVE ( 'NONE', #13751, #1910, #57301, .T. ) ;
#2473 = FACE_OUTER_BOUND ( 'NONE', #43304, .T. ) ;
#2474 = CARTESIAN_POINT ( 'NONE',  ( -11.07551654964667520, 11.07551654964660237, 455.0000000000000568 ) ) ;
#2475 = VERTEX_POINT ( 'NONE', #14875 ) ;
#2476 = DIRECTION ( 'NONE',  ( 0.7071067811865500152, 0.7071067811865451302, -4.361490581750784942E-31 ) ) ;
#2477 = VERTEX_POINT ( 'NONE', #36434 ) ;
#2478 = EDGE_CURVE ( 'NONE', #49993, #10776, #37604, .T. ) ;
#2479 = VERTEX_POINT ( 'NONE', #25839 ) ;
#2480 = DIRECTION ( 'NONE',  ( 0.000000000000000000, -1.000000000000000000, 0.000000000000000000 ) ) ;
#2481 = AXIS2_PLACEMENT_3D ( 'NONE', #21834, #28173, #43392 ) ;
#2482 = EDGE_CURVE ( 'NONE', #57396, #55087, #36799, .T. ) ;
#2483 = LINE ( 'NONE', #13443, #60346 ) ;
#2485 = DIRECTION ( 'NONE',  ( -1.000000000000000000, 0.000000000000000000, 0.000000000000000000 ) ) ;
#2484 = DIRECTION ( 'NONE',  ( 1.836970198721029934E-16, 1.836970198721010706E-16, -1.000000000000000000 ) ) ;
#2486 = VERTEX_POINT ( 'NONE', #3214 ) ;
#2487 = VERTEX_POINT ( 'NONE', #19464 ) ;
#2488 = CIRCLE ( 'NONE', #52211, 0.5999999999999989786 ) ;
#2489 = DIRECTION ( 'NONE',  ( 0.000000000000000000, -1.000000000000000000, 0.000000000000000000 ) ) ;
#2490 = ORIENTED_EDGE ( 'NONE', *, *, #22488, .F. ) ;
#2491 = DIRECTION ( 'NONE',  ( -1.836970198721029934E-16, 1.836970198721036344E-16, -1.000000000000000000 ) ) ;
#2492 = CARTESIAN_POINT ( 'NONE',  ( -9.722976262117249746, -3.682023737882726522, 54.00000000000000711 ) ) ;
#2493 = CARTESIAN_POINT ( 'NONE',  ( 146.5599459900709860, 9.000000000000001776, 328.5239988703752942 ) ) ;
#2494 = EDGE_CURVE ( 'NONE', #38025, #9849, #62592, .T. ) ;
#2495 = FACE_OUTER_BOUND ( 'NONE', #36217, .T. ) ;
#2496 = ORIENTED_EDGE ( 'NONE', *, *, #63798, .T. ) ;
#2497 = VECTOR ( 'NONE', #23027, 1000.000000000000000 ) ;
#2498 = CARTESIAN_POINT ( 'NONE',  ( 4.740315990920131561, -4.201500623656145628, 455.0000000000000568 ) ) ;
#2500 = CARTESIAN_POINT ( 'NONE',  ( 8.406483450353379183, -5.668387132715952959, 195.0000000000000284 ) ) ;
#2499 = LINE ( 'NONE', #61901, #38927 ) ;
#2501 = ORIENTED_EDGE ( 'NONE', *, *, #12826, .T. ) ;
#2503 = VERTEX_POINT ( 'NONE', #5666 ) ;
#2502 = FACE_OUTER_BOUND ( 'NONE', #50544, .T. ) ;
#2504 = VERTEX_POINT ( 'NONE', #33216 ) ;
#2505 = ORIENTED_EDGE ( 'NONE', *, *, #70, .F. ) ;
#2506 = VECTOR ( 'NONE', #69563, 1000.000000000000000 ) ;
#2507 = EDGE_CURVE ( 'NONE', #11767, #61271, #48445, .T. ) ;
#2508 = LINE ( 'NONE', #28006, #21955 ) ;
#2509 = EDGE_CURVE ( 'NONE', #21898, #47065, #43241, .T. ) ;
#2510 = DIRECTION ( 'NONE',  ( -1.000000000000000000, 0.000000000000000000, 0.000000000000000000 ) ) ;
#2511 = AXIS2_PLACEMENT_3D ( 'NONE', #14849, #13782, #36403 ) ;
#2512 = ORIENTED_EDGE ( 'NONE', *, *, #17816, .F. ) ;
#2513 = ORIENTED_EDGE ( 'NONE', *, *, #42294, .T. ) ;
#2514 = CIRCLE ( 'NONE', #56728, 2.458500000000000796 ) ;
#2515 = CARTESIAN_POINT ( 'NONE',  ( 15.00000000000000000, -42.50000000000000000, -27.00000000000000000 ) ) ;
#2516 = DIRECTION ( 'NONE',  ( -0.000000000000000000, 3.673940397442059868E-16, -1.000000000000000000 ) ) ;
#2517 = ORIENTED_EDGE ( 'NONE', *, *, #16738, .F. ) ;
#2518 = VERTEX_POINT ( 'NONE', #54448 ) ;
#2519 = DIRECTION ( 'NONE',  ( 0.000000000000000000, 0.000000000000000000, 1.000000000000000000 ) ) ;
#2520 = DIRECTION ( 'NONE',  ( 0.000000000000000000, 0.000000000000000000, 1.000000000000000000 ) ) ;
#2521 = ORIENTED_EDGE ( 'NONE', *, *, #58516, .F. ) ;
#2522 = DIRECTION ( 'NONE',  ( 1.000000000000000000, 0.000000000000000000, 0.000000000000000000 ) ) ;
#2523 = DIRECTION ( 'NONE',  ( 0.8660254037844358210, -0.5000000000000049960, 0.000000000000000000 ) ) ;
#2525 = ORIENTED_EDGE ( 'NONE', *, *, #35701, .T. ) ;
#2524 = FILL_AREA_STYLE_COLOUR ( '', #18186 ) ;
#2526 = VERTEX_POINT ( 'NONE', #22608 ) ;
#2527 = DIRECTION ( 'NONE',  ( -1.000000000000000000, 0.000000000000000000, 0.000000000000000000 ) ) ;
#2528 = DIRECTION ( 'NONE',  ( -1.000000000000000000, 0.000000000000000000, 0.000000000000000000 ) ) ;
#2529 = LINE ( 'NONE', #13490, #62251 ) ;
#2530 = AXIS2_PLACEMENT_3D ( 'NONE', #65291, #55030, #38406 ) ;
#2531 = CARTESIAN_POINT ( 'NONE',  ( -5.655420232009359616, -8.406483450353428921, 455.0000000000000568 ) ) ;
#2532 = CARTESIAN_POINT ( 'NONE',  ( 11.50000000000000000, -15.97213595500069871, 14.50000000000000000 ) ) ;
#2533 = EDGE_CURVE ( 'NONE', #38911, #55382, #27234, .T. ) ;
#2534 = CARTESIAN_POINT ( 'NONE',  ( 84.77321854994620765, 47.95351654967443977, 26.00000000000000355 ) ) ;
#2535 = CARTESIAN_POINT ( 'NONE',  ( 10.74648345035338082, -1.090483450353491035, 455.0000000000000568 ) ) ;
#2536 = VECTOR ( 'NONE', #33763, 1000.000000000000000 ) ;
#2537 = EDGE_LOOP ( 'NONE', ( #68844, #37953, #46584, #8427 ) ) ;
#2538 = DIRECTION ( 'NONE',  ( -0.000000000000000000, -1.000000000000000000, -0.000000000000000000 ) ) ;
#2539 = EDGE_CURVE ( 'NONE', #47666, #46878, #27441, .T. ) ;
#2541 = ORIENTED_EDGE ( 'NONE', *, *, #2672, .F. ) ;
#2540 = DIRECTION ( 'NONE',  ( -0.7071067811865552333, -0.7071067811865398012, 2.389338318698257180E-30 ) ) ;
#2542 = CARTESIAN_POINT ( 'NONE',  ( 7.250000000000005329, 7.250000000000000888, -18.00000000000000000 ) ) ;
#2543 = CARTESIAN_POINT ( 'NONE',  ( -8.821682069070780230, 8.130476262117182884, 54.00000000000000711 ) ) ;
#2545 = EDGE_CURVE ( 'NONE', #47184, #28252, #707, .T. ) ;
#2544 = DIRECTION ( 'NONE',  ( 0.000000000000000000, -0.9938079899998859545, 0.1111111111112941946 ) ) ;
#2546 = CARTESIAN_POINT ( 'NONE',  ( 49.00000000000000000, -14.06939075806900163, -20.80000000000000426 ) ) ;
#2547 = CARTESIAN_POINT ( 'NONE',  ( 154.0064834503532722, -29.01119750012554732, 5.000000000000000000 ) ) ;
#2548 = EDGE_CURVE ( 'NONE', #55844, #32281, #12724, .T. ) ;
#2549 = ORIENTED_EDGE ( 'NONE', *, *, #41455, .T. ) ;
#2550 = CARTESIAN_POINT ( 'NONE',  ( 37.90000000000000568, 20.60000000000000142, 3.232403992503367940E-15 ) ) ;
#2551 = VERTEX_POINT ( 'NONE', #27566 ) ;
#2552 = DIRECTION ( 'NONE',  ( 0.000000000000000000, 0.000000000000000000, 1.000000000000000000 ) ) ;
#2553 = EDGE_CURVE ( 'NONE', #65808, #53260, #11, .T. ) ;
#2554 = DIRECTION ( 'NONE',  ( 0.000000000000000000, -0.7071067811865474617, 0.7071067811865474617 ) ) ;
#2555 = DIRECTION ( 'NONE',  ( 0.000000000000000000, -1.000000000000000000, -0.000000000000000000 ) ) ;
#2556 = CIRCLE ( 'NONE', #42093, 0.3499999999999996447 ) ;
#2557 = EDGE_LOOP ( 'NONE', ( #44770, #32187, #8325, #48343, #63761, #17815, #62283, #18705 ) ) ;
#2558 = DIRECTION ( 'NONE',  ( 0.000000000000000000, 0.000000000000000000, 1.000000000000000000 ) ) ;
#2559 = ORIENTED_EDGE ( 'NONE', *, *, #20044, .T. ) ;
#2560 = EDGE_CURVE ( 'NONE', #16514, #20589, #58711, .T. ) ;
#2561 = ORIENTED_EDGE ( 'NONE', *, *, #24346, .F. ) ;
#2562 = EDGE_CURVE ( 'NONE', #25048, #26901, #17231, .T. ) ;
#2563 = VECTOR ( 'NONE', #20046, 1000.000000000000000 ) ;
#2564 = CARTESIAN_POINT ( 'NONE',  ( 275.0000000000000000, -26.50000000000000000, -0.5000000000000000000 ) ) ;
#2565 = DIRECTION ( 'NONE',  ( 1.000000000000000000, 0.000000000000000000, 0.000000000000000000 ) ) ;
#2566 = ORIENTED_EDGE ( 'NONE', *, *, #50955, .F. ) ;
#2567 = CARTESIAN_POINT ( 'NONE',  ( -7.250000000000000888, 7.250000000000001776, -20.00000000000000000 ) ) ;
#2568 = AXIS2_PLACEMENT_3D ( 'NONE', #22917, #50483, #12979 ) ;
#2569 = EDGE_CURVE ( 'NONE', #58795, #24609, #48906, .T. ) ;
#2570 = EDGE_CURVE ( 'NONE', #7476, #5949, #50038, .T. ) ;
#2571 = EDGE_CURVE ( 'NONE', #8498, #4905, #5331, .T. ) ;
#2572 = CARTESIAN_POINT ( 'NONE',  ( 8.250000000000005329, 8.250000000000001776, -26.00000000000001066 ) ) ;
#2573 = VECTOR ( 'NONE', #8814, 1000.000000000000000 ) ;
#2574 = DIRECTION ( 'NONE',  ( -1.000000000000000000, 0.000000000000000000, 0.000000000000000000 ) ) ;
#2575 = ORIENTED_EDGE ( 'NONE', *, *, #29145, .T. ) ;
#2576 = ORIENTED_EDGE ( 'NONE', *, *, #11857, .T. ) ;
#2578 = ORIENTED_EDGE ( 'NONE', *, *, #32522, .T. ) ;
#2577 = LINE ( 'NONE', #44651, #35107 ) ;
#2579 = EDGE_CURVE ( 'NONE', #43137, #34664, #26530, .T. ) ;
#2580 = ORIENTED_EDGE ( 'NONE', *, *, #11812, .F. ) ;
#2581 = LINE ( 'NONE', #24151, #30320 ) ;
#2582 = DIRECTION ( 'NONE',  ( 1.000000000000000000, 0.000000000000000000, -0.000000000000000000 ) ) ;
#2583 = DIRECTION ( 'NONE',  ( 0.000000000000000000, 0.000000000000000000, -1.000000000000000000 ) ) ;
#2584 = DIRECTION ( 'NONE',  ( -1.000000000000000000, 0.000000000000000000, 0.000000000000000000 ) ) ;
#2585 = CARTESIAN_POINT ( 'NONE',  ( 7.250000000000005329, 7.250000000000000888, -14.50000000000000000 ) ) ;
#2586 = CIRCLE ( 'NONE', #24031, 24.99999999998784972 ) ;
#2587 = EDGE_LOOP ( 'NONE', ( #29678, #44585, #8119, #42358 ) ) ;
#2588 = ORIENTED_EDGE ( 'NONE', *, *, #65248, .F. ) ;
#2589 = ORIENTED_EDGE ( 'NONE', *, *, #30303, .F. ) ;
#2590 = ORIENTED_EDGE ( 'NONE', *, *, #59099, .F. ) ;
#2591 = LINE ( 'NONE', #45717, #14129 ) ;
#2592 = AXIS2_PLACEMENT_3D ( 'NONE', #41302, #47313, #36000 ) ;
#2593 = EDGE_CURVE ( 'NONE', #22404, #37400, #22277, .T. ) ;
#2594 = DIRECTION ( 'NONE',  ( -1.000000000000000000, 0.000000000000000000, 0.000000000000000000 ) ) ;
#2595 = CARTESIAN_POINT ( 'NONE',  ( -7.250000000000000888, 8.250000000000001776, -26.00000000000001066 ) ) ;
#2596 = EDGE_CURVE ( 'NONE', #28581, #54560, #38196, .T. ) ;
#2597 = DIRECTION ( 'NONE',  ( 0.000000000000000000, -1.000000000000000000, -1.880440247955360336E-12 ) ) ;
#2598 = EDGE_LOOP ( 'NONE', ( #37550, #60580, #10876, #67982 ) ) ;
#2599 = ORIENTED_EDGE ( 'NONE', *, *, #57099, .T. ) ;
#2600 = ORIENTED_EDGE ( 'NONE', *, *, #41043, .T. ) ;
#2601 = LINE ( 'NONE', #35463, #12450 ) ;
#2602 = ORIENTED_EDGE ( 'NONE', *, *, #12840, .T. ) ;
#2603 = EDGE_LOOP ( 'NONE', ( #9284, #22098, #66841, #24413 ) ) ;
#2604 = EDGE_LOOP ( 'NONE', ( #30349, #21481, #8721, #31210 ) ) ;
#2605 = ORIENTED_EDGE ( 'NONE', *, *, #14448, .T. ) ;
#2606 = DIRECTION ( 'NONE',  ( 0.000000000000000000, 0.000000000000000000, -1.000000000000000000 ) ) ;
#2608 = VERTEX_POINT ( 'NONE', #15589 ) ;
#2607 = LINE ( 'NONE', #60952, #2910 ) ;
#2609 = ORIENTED_EDGE ( 'NONE', *, *, #69298, .T. ) ;
#2610 = CARTESIAN_POINT ( 'NONE',  ( 7.826483450353380000, -12.00648345035349251, 455.0000000000000568 ) ) ;
#2611 = EDGE_CURVE ( 'NONE', #34045, #42164, #26339, .T. ) ;
#2613 = DIRECTION ( 'NONE',  ( 0.000000000000000000, 0.000000000000000000, -1.000000000000000000 ) ) ;
#2612 = VECTOR ( 'NONE', #7791, 1000.000000000000000 ) ;
#2614 = DIRECTION ( 'NONE',  ( 1.000000000000000000, -7.457533623526253657E-15, 1.836970198721015882E-16 ) ) ;
#2616 = ORIENTED_EDGE ( 'NONE', *, *, #10169, .F. ) ;
#2615 = LINE ( 'NONE', #28437, #30086 ) ;
#2618 = EDGE_LOOP ( 'NONE', ( #1513, #821, #63105, #9771 ) ) ;
#2617 = AXIS2_PLACEMENT_3D ( 'NONE', #2474, #24038, #67175 ) ;
#2619 = VECTOR ( 'NONE', #5543, 1000.000000000000000 ) ;
#2620 = LINE ( 'NONE', #66626, #26087 ) ;
#2621 = DIRECTION ( 'NONE',  ( 1.000000000000000000, 0.000000000000000000, 0.000000000000000000 ) ) ;
#2622 = CYLINDRICAL_SURFACE ( 'NONE', #48523, 0.3499999999999614531 ) ;
#2623 = VECTOR ( 'NONE', #5180, 1000.000000000000000 ) ;
#2624 = VERTEX_POINT ( 'NONE', #10607 ) ;
#2625 = FACE_OUTER_BOUND ( 'NONE', #43992, .T. ) ;
#2626 = EDGE_CURVE ( 'NONE', #32093, #14268, #47783, .T. ) ;
#2627 = CARTESIAN_POINT ( 'NONE',  ( 8.250000000000005329, -7.249999999999998224, -20.00000000000000000 ) ) ;
#2628 = DIRECTION ( 'NONE',  ( 0.000000000000000000, 1.000000000000000000, 0.000000000000000000 ) ) ;
#2629 = ORIENTED_EDGE ( 'NONE', *, *, #67340, .T. ) ;
#2631 = ADVANCED_FACE ( 'NONE', ( #64363 ), #27919, .F. ) ;
#2630 = CARTESIAN_POINT ( 'NONE',  ( 7.826483450353380000, -12.00648345035339659, 195.0000000000000284 ) ) ;
#2632 = DIRECTION ( 'NONE',  ( -1.000000000000000000, 0.000000000000000000, 0.000000000000000000 ) ) ;
#2633 = CARTESIAN_POINT ( 'NONE',  ( 37.90000000000000568, -14.06939075806902117, -20.80000000000000426 ) ) ;
#2634 = EDGE_CURVE ( 'NONE', #19716, #24845, #7714, .T. ) ;
#2635 = VECTOR ( 'NONE', #63375, 1000.000000000000000 ) ;
#2636 = ORIENTED_EDGE ( 'NONE', *, *, #43110, .T. ) ;
#2637 = SURFACE_SIDE_STYLE ('',( #3344 ) ) ;
#2638 = EDGE_CURVE ( 'NONE', #58346, #66347, #1384, .T. ) ;
#2639 = DIRECTION ( 'NONE',  ( 0.4999999999999695799, -0.8660254037844563602, -6.723777587269172655E-17 ) ) ;
#2640 = ORIENTED_EDGE ( 'NONE', *, *, #46648, .T. ) ;
#2641 = FACE_OUTER_BOUND ( 'NONE', #5074, .T. ) ;
#2642 = DIRECTION ( 'NONE',  ( 0.000000000000000000, -1.000000000000000000, 0.000000000000000000 ) ) ;
#2643 = DIRECTION ( 'NONE',  ( -0.7071067811865486830, -0.7071067811865464625, -2.597868168706476160E-16 ) ) ;
#2644 = CARTESIAN_POINT ( 'NONE',  ( -4.706725378239251967, -4.155633711806651753, 54.00000000000000711 ) ) ;
#2645 = DIRECTION ( 'NONE',  ( -0.000000000000000000, -0.000000000000000000, 1.000000000000000000 ) ) ;
#2646 = VERTEX_POINT ( 'NONE', #6681 ) ;
#2647 = PLANE ( 'NONE',  #1639 ) ;
#2648 = FACE_OUTER_BOUND ( 'NONE', #18794, .T. ) ;
#2649 = DIRECTION ( 'NONE',  ( -1.836970198721029934E-16, 1.836970198721036344E-16, -1.000000000000000000 ) ) ;
#2650 = EDGE_CURVE ( 'NONE', #32206, #61792, #13379, .T. ) ;
#2651 = CARTESIAN_POINT ( 'NONE',  ( -5.993516549646776603, -6.006483450353426790, 455.0000000000000568 ) ) ;
#2652 = LINE ( 'NONE', #62046, #24926 ) ;
#2653 = ORIENTED_EDGE ( 'NONE', *, *, #691, .F. ) ;
#2655 = ORIENTED_EDGE ( 'NONE', *, *, #55583, .F. ) ;
#2654 = CARTESIAN_POINT ( 'NONE',  ( 16.33757311576526305, -0.3152598339554824047, -23.45980260912095616 ) ) ;
#2656 = VECTOR ( 'NONE', #54838, 1000.000000000000000 ) ;
#2657 = TOROIDAL_SURFACE ( 'NONE', #32013, 3.299999999999474909, 0.2000000000005234813 ) ;
#2658 = CARTESIAN_POINT ( 'NONE',  ( 13.00000000000000178, -17.00000000000000000, 15.70499999999969809 ) ) ;
#2659 = DIRECTION ( 'NONE',  ( 0.000000000000000000, -1.000000000000000000, 0.000000000000000000 ) ) ;
#2660 = ORIENTED_EDGE ( 'NONE', *, *, #24158, .F. ) ;
#2661 = AXIS2_PLACEMENT_3D ( 'NONE', #26499, #21210, #27203 ) ;
#2662 = VECTOR ( 'NONE', #46837, 1000.000000000000000 ) ;
#2663 = CARTESIAN_POINT ( 'NONE',  ( -11.00000000000000000, -17.14999999999999858, 27.00000000000000000 ) ) ;
#2664 = VECTOR ( 'NONE', #57739, 1000.000000000000000 ) ;
#2665 = ORIENTED_EDGE ( 'NONE', *, *, #59766, .T. ) ;
#2666 = VECTOR ( 'NONE', #10902, 1000.000000000000000 ) ;
#2667 = LINE ( 'NONE', #45444, #2978 ) ;
#2668 = ORIENTED_EDGE ( 'NONE', *, *, #56721, .T. ) ;
#2669 = AXIS2_PLACEMENT_3D ( 'NONE', #16360, #11061, #48540 ) ;
#2670 = ORIENTED_EDGE ( 'NONE', *, *, #56541, .T. ) ;
#2671 = DIRECTION ( 'NONE',  ( -1.000000000000000000, 0.000000000000000000, 0.000000000000000000 ) ) ;
#2672 = EDGE_CURVE ( 'NONE', #56266, #21095, #65739, .T. ) ;
#2673 = CARTESIAN_POINT ( 'NONE',  ( 7.250000000000005329, -7.449999999999998401, -17.00000000000000000 ) ) ;
#2674 = DIRECTION ( 'NONE',  ( 1.836970198721029934E-16, -1.836970198721036344E-16, 1.000000000000000000 ) ) ;
#2676 = EDGE_CURVE ( 'NONE', #17055, #62668, #23629, .T. ) ;
#2675 = CARTESIAN_POINT ( 'NONE',  ( 10.50702373788281996, -6.849523737882814878, 26.00000000000000000 ) ) ;
#2677 = ORIENTED_EDGE ( 'NONE', *, *, #39393, .T. ) ;
#2679 = EDGE_CURVE ( 'NONE', #44308, #34611, #39211, .T. ) ;
#2678 = ORIENTED_EDGE ( 'NONE', *, *, #28225, .T. ) ;
#2680 = CARTESIAN_POINT ( 'NONE',  ( -15.50000000000000000, -17.50000000000000000, 22.50000000000000000 ) ) ;
#2681 = CARTESIAN_POINT ( 'NONE',  ( 39.00000000000000000, 6.123233995736766282E-16, -5.000000000000000000 ) ) ;
#2682 = ORIENTED_EDGE ( 'NONE', *, *, #6452, .T. ) ;
#2683 = VERTEX_POINT ( 'NONE', #61107 ) ;
#2684 = ORIENTED_EDGE ( 'NONE', *, *, #42449, .F. ) ;
#2685 = DIRECTION ( 'NONE',  ( -1.000000000000000000, 0.000000000000000000, 0.000000000000000000 ) ) ;
#2687 = ORIENTED_EDGE ( 'NONE', *, *, #58098, .T. ) ;
#2686 = PLANE ( 'NONE',  #43491 ) ;
#2688 = DIRECTION ( 'NONE',  ( 0.000000000000000000, 1.000000000000000000, 0.000000000000000000 ) ) ;
#2689 = CARTESIAN_POINT ( 'NONE',  ( 7.250000000000005329, -8.249999999999998224, -23.50000000000000000 ) ) ;
#2690 = ORIENTED_EDGE ( 'NONE', *, *, #67987, .T. ) ;
#2691 = VECTOR ( 'NONE', #48240, 1000.000000000000000 ) ;
#2692 = ORIENTED_EDGE ( 'NONE', *, *, #40418, .F. ) ;
#2693 = CARTESIAN_POINT ( 'NONE',  ( -8.250000000000001776, -7.249999999999998224, -25.00000000000000000 ) ) ;
#2694 = CARTESIAN_POINT ( 'NONE',  ( 1.690483450353371442, 10.73351654964664270, 195.0000000000000284 ) ) ;
#2695 = LINE ( 'NONE', #33825, #39402 ) ;
#2696 = EDGE_CURVE ( 'NONE', #5555, #39293, #38859, .T. ) ;
#2697 = AXIS2_PLACEMENT_3D ( 'NONE', #28551, #66728, #61412 ) ;
#2698 = CARTESIAN_POINT ( 'NONE',  ( 3.857023737882817827, 9.897976262117204271, 54.00000000000000711 ) ) ;
#2699 = LINE ( 'NONE', #47256, #5416 ) ;
#2701 = VERTEX_POINT ( 'NONE', #60419 ) ;
#2700 = LINE ( 'NONE', #24281, #61516 ) ;
#2702 = VERTEX_POINT ( 'NONE', #2765 ) ;
#2703 = CARTESIAN_POINT ( 'NONE',  ( 3.157023737882797665, 4.031976262117209053, 54.00000000000000711 ) ) ;
#2704 = DIRECTION ( 'NONE',  ( 0.000000000000000000, 0.000000000000000000, -1.000000000000000000 ) ) ;
#2705 = AXIS2_PLACEMENT_3D ( 'NONE', #68691, #36871, #20929 ) ;
#2707 = VECTOR ( 'NONE', #68907, 1000.000000000000000 ) ;
#2706 = LINE ( 'NONE', #29578, #12717 ) ;
#2708 = CARTESIAN_POINT ( 'NONE',  ( -10.49297626211726175, 6.835476262117182955, 54.00000000000000711 ) ) ;
#2709 = EDGE_CURVE ( 'NONE', #52538, #3182, #55696, .T. ) ;
#2710 = EDGE_CURVE ( 'NONE', #12955, #45920, #40244, .T. ) ;
#2711 = AXIS2_PLACEMENT_3D ( 'NONE', #13802, #15221, #20864 ) ;
#2712 = DIRECTION ( 'NONE',  ( 1.000000000000000000, 0.000000000000000000, 0.000000000000000000 ) ) ;
#2714 = ORIENTED_EDGE ( 'NONE', *, *, #49535, .F. ) ;
#2713 = EDGE_CURVE ( 'NONE', #42484, #9816, #11972, .T. ) ;
#2715 = CARTESIAN_POINT ( 'NONE',  ( -5.993516549646728642, -6.006483450353378828, 195.0000000000000284 ) ) ;
#2716 = EDGE_CURVE ( 'NONE', #68424, #29039, #34928, .T. ) ;
#2717 = CARTESIAN_POINT ( 'NONE',  ( 13.00000000000000178, -17.50000000000000000, 15.70499999999969809 ) ) ;
#2718 =( NAMED_UNIT ( * ) SI_UNIT ( $, .STERADIAN. ) SOLID_ANGLE_UNIT ( ) );
#2719 = DIRECTION ( 'NONE',  ( 0.000000000000000000, 0.000000000000000000, 1.000000000000000000 ) ) ;
#2720 = ADVANCED_FACE ( 'NONE', ( #28940 ), #45192, .F. ) ;
#2721 = DIRECTION ( 'NONE',  ( -1.000000000000000000, 0.000000000000000000, 0.000000000000000000 ) ) ;
#2722 = CARTESIAN_POINT ( 'NONE',  ( -7.450000000000001954, 0.000000000000000000, -7.000000000000000000 ) ) ;
#2723 = VECTOR ( 'NONE', #11038, 1000.000000000000000 ) ;
#2724 = LINE ( 'NONE', #57178, #51191 ) ;
#2725 = ORIENTED_EDGE ( 'NONE', *, *, #42409, .F. ) ;
#2726 = CARTESIAN_POINT ( 'NONE',  ( 8.144523737882817471, -8.835729544836334881, 26.00000000000000000 ) ) ;
#2727 = LINE ( 'NONE', #3441, #54214 ) ;
#2728 = EDGE_LOOP ( 'NONE', ( #19936, #57321, #24721, #50943 ) ) ;
#2729 = CARTESIAN_POINT ( 'NONE',  ( 7.250000000000005329, 8.250000000000001776, -21.00000000000000000 ) ) ;
#2730 = DIRECTION ( 'NONE',  ( 0.000000000000000000, 0.000000000000000000, 1.000000000000000000 ) ) ;
#2731 = DIRECTION ( 'NONE',  ( 0.000000000000000000, 0.000000000000000000, 1.000000000000000000 ) ) ;
#2732 = DIRECTION ( 'NONE',  ( 0.000000000000000000, -0.9921567416492215186, -0.1249999999999996531 ) ) ;
#2733 = CARTESIAN_POINT ( 'NONE',  ( 30.00000000000000000, -16.28999999999710369, 15.00000000000794920 ) ) ;
#2734 = VERTEX_POINT ( 'NONE', #23982 ) ;
#2735 = DIRECTION ( 'NONE',  ( 1.836970198721029934E-16, 1.836970198721010706E-16, -1.000000000000000000 ) ) ;
#2736 = ORIENTED_EDGE ( 'NONE', *, *, #38625, .F. ) ;
#2737 = DIRECTION ( 'NONE',  ( -9.050731179009442381E-15, -1.000000000000000000, 0.000000000000000000 ) ) ;
#2738 = CARTESIAN_POINT ( 'NONE',  ( -29.50000000000000355, -12.00000000000000000, 10.69999999999999929 ) ) ;
#2739 = ORIENTED_EDGE ( 'NONE', *, *, #17158, .T. ) ;
#2740 = DIRECTION ( 'NONE',  ( 0.4999999999989361843, 0.000000000000000000, -0.8660254037850529940 ) ) ;
#2741 = AXIS2_PLACEMENT_3D ( 'NONE', #64332, #43438, #44128 ) ;
#2742 = EDGE_LOOP ( 'NONE', ( #8520, #22275, #56894, #42174 ) ) ;
#2743 = LINE ( 'NONE', #57809, #15256 ) ;
#2744 = DIRECTION ( 'NONE',  ( 0.000000000000000000, 1.000000000000000000, 0.000000000000000000 ) ) ;
#2745 = ORIENTED_EDGE ( 'NONE', *, *, #58098, .F. ) ;
#2746 = EDGE_LOOP ( 'NONE', ( #41710, #2684, #54465, #30416 ) ) ;
#2747 = DIRECTION ( 'NONE',  ( -1.000000000000000000, 0.000000000000000000, 0.000000000000000000 ) ) ;
#2748 = ORIENTED_EDGE ( 'NONE', *, *, #56140, .F. ) ;
#2749 = ORIENTED_EDGE ( 'NONE', *, *, #59616, .T. ) ;
#2750 = PRODUCT_DEFINITION_CONTEXT ( 'detailed design', #44027, 'design' ) ;
#2751 = CARTESIAN_POINT ( 'NONE',  ( -11.47551654964667733, 11.07551654964660237, 455.0000000000000568 ) ) ;
#2752 = CARTESIAN_POINT ( 'NONE',  ( 6.657023737882821202, 10.30047626211719347, 54.00000000000000711 ) ) ;
#2753 = AXIS2_PLACEMENT_3D ( 'NONE', #233, #6227, #44043 ) ;
#2754 = AXIS2_PLACEMENT_3D ( 'NONE', #13905, #46769, #35456 ) ;
#2755 = CARTESIAN_POINT ( 'NONE',  ( -10.91351654964680584, -9.306483450353375986, 455.0000000000000568 ) ) ;
#2756 = VERTEX_POINT ( 'NONE', #56510 ) ;
#2757 = ADVANCED_FACE ( 'NONE', ( #29631 ), #51204, .F. ) ;
#2758 = CARTESIAN_POINT ( 'NONE',  ( -9.791916549646712653, 11.07551654964660415, 455.0000000000000568 ) ) ;
#2759 = EDGE_CURVE ( 'NONE', #24541, #35101, #55139, .T. ) ;
#2761 = DIRECTION ( 'NONE',  ( 0.000000000000000000, -1.000000000000000000, 3.989863994748342081E-13 ) ) ;
#2760 = CARTESIAN_POINT ( 'NONE',  ( 289.2330000000000041, 4.898587196589412829E-16, 4.000000000000000000 ) ) ;
#2762 = CIRCLE ( 'NONE', #41130, 0.3500000000009988455 ) ;
#2764 = VERTEX_POINT ( 'NONE', #22945 ) ;
#2763 = AXIS2_PLACEMENT_3D ( 'NONE', #55945, #29415, #56294 ) ;
#2766 = VERTEX_POINT ( 'NONE', #44500 ) ;
#2765 = CARTESIAN_POINT ( 'NONE',  ( 11.00000000000000000, -12.00000000000000000, -10.52786404500095863 ) ) ;
#2767 = ORIENTED_EDGE ( 'NONE', *, *, #16069, .T. ) ;
#2768 = EDGE_CURVE ( 'NONE', #44787, #2257, #46665, .T. ) ;
#2769 = PRODUCT_CONTEXT ( 'NONE', #27335, 'mechanical' ) ;
#2770 = VECTOR ( 'NONE', #60601, 1000.000000000000000 ) ;
#2771 = CARTESIAN_POINT ( 'NONE',  ( 4.747751991980625696, -6.619341603356940773, 455.0000000000000568 ) ) ;
#2772 = VERTEX_POINT ( 'NONE', #18319 ) ;
#2773 = DIRECTION ( 'NONE',  ( 0.000000000000000000, 0.000000000000000000, 1.000000000000000000 ) ) ;
#2774 = DIRECTION ( 'NONE',  ( 0.000000000000000000, 0.000000000000000000, 1.000000000000000000 ) ) ;
#2776 = ORIENTED_EDGE ( 'NONE', *, *, #11169, .T. ) ;
#2775 = CIRCLE ( 'NONE', #13550, 1.500000000000000444 ) ;
#2777 = ORIENTED_EDGE ( 'NONE', *, *, #34728, .T. ) ;
#2778 = AXIS2_PLACEMENT_3D ( 'NONE', #65398, #60078, #11625 ) ;
#2779 = DIRECTION ( 'NONE',  ( 0.000000000000000000, -3.673940397442059868E-16, 1.000000000000000000 ) ) ;
#2780 = CYLINDRICAL_SURFACE ( 'NONE', #16505, 0.2000000000000005107 ) ;
#2781 = EDGE_LOOP ( 'NONE', ( #55650, #12350, #23767, #57102 ) ) ;
#2782 = LINE ( 'NONE', #45561, #33592 ) ;
#2783 = CARTESIAN_POINT ( 'NONE',  ( 31.89999999999999858, -0.1999999999911430404, -8.864436962241481021E-12 ) ) ;
#2784 = DIRECTION ( 'NONE',  ( 1.000000000000000000, 0.000000000000000000, 0.000000000000000000 ) ) ;
#2785 = ORIENTED_EDGE ( 'NONE', *, *, #60594, .T. ) ;
#2786 = DIRECTION ( 'NONE',  ( 1.000000000000000000, 0.000000000000000000, 0.000000000000000000 ) ) ;
#2787 = DIRECTION ( 'NONE',  ( 3.016910393003147986E-15, 1.000000000000000000, -0.000000000000000000 ) ) ;
#2788 = AXIS2_PLACEMENT_3D ( 'NONE', #55122, #5644, #37819 ) ;
#2790 = ORIENTED_EDGE ( 'NONE', *, *, #9912, .F. ) ;
#2789 = FACE_OUTER_BOUND ( 'NONE', #50617, .T. ) ;
#2792 = ORIENTED_EDGE ( 'NONE', *, *, #29625, .T. ) ;
#2791 = CARTESIAN_POINT ( 'NONE',  ( 11.00000000000000000, -9.200000000000120082, -17.30000000000000071 ) ) ;
#2793 = CARTESIAN_POINT ( 'NONE',  ( 15.00000000000000000, -25.60000000000000142, -15.10000000000000142 ) ) ;
#2794 = DIRECTION ( 'NONE',  ( 1.000000000000000000, -0.000000000000000000, -0.000000000000000000 ) ) ;
#2795 = VECTOR ( 'NONE', #15106, 1000.000000000000000 ) ;
#2796 = CARTESIAN_POINT ( 'NONE',  ( 6.849523737882817542, -10.50702373788282529, 54.00000000000000711 ) ) ;
#2797 = CARTESIAN_POINT ( 'NONE',  ( -11.50000000000000000, -11.50000000000100009, 15.00000000000084910 ) ) ;
#2798 = CARTESIAN_POINT ( 'NONE',  ( 11.00000000000000000, -5.200000000000001066, -26.59999999999999787 ) ) ;
#2799 = ORIENTED_EDGE ( 'NONE', *, *, #32986, .F. ) ;
#2800 = CARTESIAN_POINT ( 'NONE',  ( 11.00000000000000000, -12.00000000000000000, -11.03137303340310282 ) ) ;
#2801 = EDGE_CURVE ( 'NONE', #44331, #44196, #39883, .T. ) ;
#2802 = CARTESIAN_POINT ( 'NONE',  ( -7.250000000000000888, 7.250000000000001776, -21.50000000000000000 ) ) ;
#2803 = EDGE_CURVE ( 'NONE', #54522, #20164, #29274, .T. ) ;
#2804 = CARTESIAN_POINT ( 'NONE',  ( 4.396432944014527777, -8.406483450353478659, 455.0000000000000568 ) ) ;
#2806 = VERTEX_POINT ( 'NONE', #13725 ) ;
#2805 = DIRECTION ( 'NONE',  ( 0.000000000000000000, -1.000000000000000000, 0.000000000000000000 ) ) ;
#2807 = AXIS2_PLACEMENT_3D ( 'NONE', #9613, #36474, #40383 ) ;
#2808 = VECTOR ( 'NONE', #20875, 1000.000000000000114 ) ;
#2809 = LINE ( 'NONE', #17688, #49351 ) ;
#2810 = EDGE_CURVE ( 'NONE', #40458, #40971, #67490, .T. ) ;
#2811 = EDGE_CURVE ( 'NONE', #35986, #61486, #68533, .T. ) ;
#2812 = CARTESIAN_POINT ( 'NONE',  ( 10.09643294401453417, 2.893516549646536262, 455.0000000000000568 ) ) ;
#2813 = ORIENTED_EDGE ( 'NONE', *, *, #57418, .F. ) ;
#2814 = AXIS2_PLACEMENT_3D ( 'NONE', #25463, #64680, #44144 ) ;
#2815 = VERTEX_POINT ( 'NONE', #40598 ) ;
#2816 = DIRECTION ( 'NONE',  ( 0.000000000000000000, 0.000000000000000000, 1.000000000000000000 ) ) ;
#2817 = DIRECTION ( 'NONE',  ( 4.745709458399858621E-16, 1.000000000000000000, 1.836970198721035604E-16 ) ) ;
#2818 = ORIENTED_EDGE ( 'NONE', *, *, #42486, .F. ) ;
#2819 = CARTESIAN_POINT ( 'NONE',  ( 8.835729544836338434, -2.544523737882825820, 54.00000000000000711 ) ) ;
#2820 = AXIS2_PLACEMENT_3D ( 'NONE', #36517, #36164, #20955 ) ;
#2821 = DIRECTION ( 'NONE',  ( -0.000000000000000000, 0.000000000000000000, -1.000000000000000000 ) ) ;
#2822 = EDGE_CURVE ( 'NONE', #60107, #55424, #18426, .T. ) ;
#2823 = DIRECTION ( 'NONE',  ( 0.000000000000000000, 0.000000000000000000, -1.000000000000000000 ) ) ;
#2824 = ADVANCED_FACE ( 'NONE', ( #19036 ), #35272, .T. ) ;
#2825 = FACE_OUTER_BOUND ( 'NONE', #63781, .T. ) ;
#2826 = MECHANICAL_DESIGN_GEOMETRIC_PRESENTATION_REPRESENTATION (  '', ( #11849 ), #66006 ) ;
#2827 = EDGE_LOOP ( 'NONE', ( #35546, #61651, #61886, #57829, #60828, #10843, #34226, #22448, #53651, #51118, #32783 ) ) ;
#2828 = DIRECTION ( 'NONE',  ( 0.000000000000000000, 3.673940397442059868E-16, -1.000000000000000000 ) ) ;
#2829 = EDGE_LOOP ( 'NONE', ( #50662, #55681 ) ) ;
#2830 = ORIENTED_EDGE ( 'NONE', *, *, #47593, .T. ) ;
#2831 = CIRCLE ( 'NONE', #42365, 24.99999999998789946 ) ;
#2832 = LINE ( 'NONE', #18043, #46014 ) ;
#2833 = DIRECTION ( 'NONE',  ( -1.000000000000000000, 0.000000000000000000, 0.000000000000000000 ) ) ;
#2834 = ORIENTED_EDGE ( 'NONE', *, *, #7554, .F. ) ;
#2835 = ORIENTED_EDGE ( 'NONE', *, *, #43160, .F. ) ;
#2836 = CARTESIAN_POINT ( 'NONE',  ( -7.250000000000000888, 7.250000000000001776, -13.50000000000000178 ) ) ;
#2837 = VERTEX_POINT ( 'NONE', #20090 ) ;
#2838 = ORIENTED_EDGE ( 'NONE', *, *, #50383, .F. ) ;
#2839 = CARTESIAN_POINT ( 'NONE',  ( 9.955011587777235604, -9.247904806590705462, 195.0000000000000284 ) ) ;
#2840 = DIRECTION ( 'NONE',  ( -1.000000000000000000, 1.952517519553884087E-14, 0.000000000000000000 ) ) ;
#2841 = CARTESIAN_POINT ( 'NONE',  ( -7.250000000000000888, 8.250000000000001776, -26.00000000000001066 ) ) ;
#2842 = DIRECTION ( 'NONE',  ( 0.000000000000000000, 1.000000000000000000, 0.000000000000000000 ) ) ;
#2843 = ORIENTED_EDGE ( 'NONE', *, *, #43763, .T. ) ;
#2844 = CARTESIAN_POINT ( 'NONE',  ( -9.690000000000001279, 10.50000000000000000, 0.000000000000000000 ) ) ;
#2846 = CARTESIAN_POINT ( 'NONE',  ( -10.73351654964671020, 1.677516549646604016, 455.0000000000000568 ) ) ;
#2845 = CARTESIAN_POINT ( 'NONE',  ( 5.257023737882801306, 5.242976262117200470, 54.00000000000000711 ) ) ;
#2847 = VERTEX_POINT ( 'NONE', #63218 ) ;
#2849 = VERTEX_POINT ( 'NONE', #56853 ) ;
#2848 = DIRECTION ( 'NONE',  ( 1.836970198721029934E-16, 1.836970198721010706E-16, -1.000000000000000000 ) ) ;
#2850 = AXIS2_PLACEMENT_3D ( 'NONE', #28738, #29095, #2222 ) ;
#2851 = EDGE_LOOP ( 'NONE', ( #17852, #14614, #51041, #19801, #22167, #60121, #33535, #32845 ) ) ;
#2852 = ORIENTED_EDGE ( 'NONE', *, *, #23298, .T. ) ;
#2853 = EDGE_CURVE ( 'NONE', #1375, #17432, #14786, .T. ) ;
#2854 = AXIS2_PLACEMENT_3D ( 'NONE', #30402, #3534, #52322 ) ;
#2855 = DIRECTION ( 'NONE',  ( 1.000000000000000000, 0.000000000000000000, -0.000000000000000000 ) ) ;
#2856 = VECTOR ( 'NONE', #907, 1000.000000000000000 ) ;
#2857 = VECTOR ( 'NONE', #68920, 1000.000000000000000 ) ;
#2859 = CARTESIAN_POINT ( 'NONE',  ( 0.000000000000000000, -7.449999999999998401, -19.00000000000000000 ) ) ;
#2858 = AXIS2_PLACEMENT_3D ( 'NONE', #4019, #31594, #64131 ) ;
#2860 = ORIENTED_EDGE ( 'NONE', *, *, #47589, .F. ) ;
#2861 = ORIENTED_EDGE ( 'NONE', *, *, #54468, .T. ) ;
#2862 = CIRCLE ( 'NONE', #18653, 0.5540281690140901327 ) ;
#2863 = AXIS2_PLACEMENT_3D ( 'NONE', #55635, #22432, #7177 ) ;
#2864 = EDGE_CURVE ( 'NONE', #53691, #10351, #6052, .T. ) ;
#2865 = CYLINDRICAL_SURFACE ( 'NONE', #11702, 1.500000000000000444 ) ;
#2866 = LINE ( 'NONE', #60527, #656 ) ;
#2867 = ORIENTED_EDGE ( 'NONE', *, *, #57305, .F. ) ;
#2868 = ORIENTED_EDGE ( 'NONE', *, *, #14066, .T. ) ;
#2869 = LINE ( 'NONE', #67225, #43226 ) ;
#2870 = VECTOR ( 'NONE', #6616, 1000.000000000000000 ) ;
#2871 = EDGE_CURVE ( 'NONE', #52538, #3728, #14073, .T. ) ;
#2872 = CARTESIAN_POINT ( 'NONE',  ( -15.50000000000000000, -1.037157890325000054, 22.50000000000000000 ) ) ;
#2873 = ORIENTED_EDGE ( 'NONE', *, *, #57385, .F. ) ;
#2874 = AXIS2_PLACEMENT_3D ( 'NONE', #18911, #57436, #30917 ) ;
#2875 = DIRECTION ( 'NONE',  ( 6.308085367188446447E-15, 1.000000000000000000, 3.673940397442059868E-16 ) ) ;
#2876 = CARTESIAN_POINT ( 'NONE',  ( 24.00000000000000000, -15.50000000000000000, 19.33772233983200195 ) ) ;
#2878 = ORIENTED_EDGE ( 'NONE', *, *, #63499, .T. ) ;
#2877 = PRESENTATION_STYLE_ASSIGNMENT (( #39991 ) ) ;
#2879 = VECTOR ( 'NONE', #22312, 1000.000000000000000 ) ;
#2880 = ORIENTED_EDGE ( 'NONE', *, *, #68126, .T. ) ;
#2881 = LINE ( 'NONE', #35754, #18572 ) ;
#2882 = LINE ( 'NONE', #12101, #66209 ) ;
#2883 = DIRECTION ( 'NONE',  ( 1.000000000000000000, -3.491481338843132961E-15, 0.000000000000000000 ) ) ;
#2884 = LINE ( 'NONE', #7829, #35784 ) ;
#2885 = DIRECTION ( 'NONE',  ( 0.000000000000000000, 0.000000000000000000, -1.000000000000000000 ) ) ;
#2886 = DIRECTION ( 'NONE',  ( -1.000000000000000000, 0.000000000000000000, 0.000000000000000000 ) ) ;
#2887 = PLANE ( 'NONE',  #12297 ) ;
#2888 = ORIENTED_EDGE ( 'NONE', *, *, #28482, .F. ) ;
#2889 = FACE_OUTER_BOUND ( 'NONE', #2781, .T. ) ;
#2890 = EDGE_CURVE ( 'NONE', #66424, #5664, #62870, .T. ) ;
#2892 = ORIENTED_EDGE ( 'NONE', *, *, #4662, .T. ) ;
#2891 = FACE_OUTER_BOUND ( 'NONE', #4618, .T. ) ;
#2893 = CARTESIAN_POINT ( 'NONE',  ( 30.00000000000000000, -17.00000000000000000, 15.70499999999969809 ) ) ;
#2894 = DIRECTION ( 'NONE',  ( 0.000000000000000000, 1.000000000000000000, 0.000000000000000000 ) ) ;
#2895 = ADVANCED_FACE ( 'NONE', ( #51565 ), #35995, .F. ) ;
#2896 = EDGE_CURVE ( 'NONE', #62756, #29427, #63595, .T. ) ;
#2897 = AXIS2_PLACEMENT_3D ( 'NONE', #27773, #17851, #11491 ) ;
#2898 = CARTESIAN_POINT ( 'NONE',  ( -7.250000000000000888, 7.250000000000001776, -26.00000000000001066 ) ) ;
#2899 = LINE ( 'NONE', #46040, #19373 ) ;
#2900 = DIRECTION ( 'NONE',  ( 1.836970198721029934E-16, -1.836970198721036344E-16, 1.000000000000000000 ) ) ;
#2901 = EDGE_CURVE ( 'NONE', #59143, #62865, #42125, .T. ) ;
#2902 = VECTOR ( 'NONE', #47633, 1000.000000000000000 ) ;
#2903 = ORIENTED_EDGE ( 'NONE', *, *, #67141, .F. ) ;
#2904 = DIRECTION ( 'NONE',  ( -1.836970198721029934E-16, 1.836970198721036344E-16, -1.000000000000000000 ) ) ;
#2905 = ORIENTED_EDGE ( 'NONE', *, *, #21002, .F. ) ;
#2906 = CIRCLE ( 'NONE', #51463, 0.6000000000000006439 ) ;
#2907 = FACE_OUTER_BOUND ( 'NONE', #45930, .T. ) ;
#2908 = ADVANCED_FACE ( 'NONE', ( #51917, #3480 ), #68171, .T. ) ;
#2909 = EDGE_CURVE ( 'NONE', #17317, #69297, #64806, .T. ) ;
#2910 = VECTOR ( 'NONE', #6862, 1000.000000000000000 ) ;
#2911 = VECTOR ( 'NONE', #12543, 1000.000000000000000 ) ;
#2912 = AXIS2_PLACEMENT_3D ( 'NONE', #12413, #66527, #44957 ) ;
#2913 = CARTESIAN_POINT ( 'NONE',  ( -3.593516549646728286, -6.006483450353403697, 195.0000000000000284 ) ) ;
#2914 = ORIENTED_EDGE ( 'NONE', *, *, #36272, .T. ) ;
#2915 = CARTESIAN_POINT ( 'NONE',  ( -8.250000000000001776, 7.250000000000000888, -22.50000000000000000 ) ) ;
#2916 = VERTEX_POINT ( 'NONE', #40112 ) ;
#2917 = ORIENTED_EDGE ( 'NONE', *, *, #58860, .F. ) ;
#2918 = DIRECTION ( 'NONE',  ( 1.000000000000000000, -7.304098846218132892E-15, 0.000000000000000000 ) ) ;
#2920 = CARTESIAN_POINT ( 'NONE',  ( 13.90000000000000213, -21.00000000000000000, 13.86939075806900057 ) ) ;
#2919 = AXIS2_PLACEMENT_3D ( 'NONE', #37340, #69509, #10456 ) ;
#2921 = VECTOR ( 'NONE', #20071, 1000.000000000000000 ) ;
#2922 = AXIS2_PLACEMENT_3D ( 'NONE', #47814, #26605, #21307 ) ;
#2923 = CARTESIAN_POINT ( 'NONE',  ( 7.250000000000005329, -7.449999999999998401, -16.50000000000000000 ) ) ;
#2924 = VECTOR ( 'NONE', #69150, 1000.000000000000000 ) ;
#2925 = LINE ( 'NONE', #57010, #20793 ) ;
#2926 = CARTESIAN_POINT ( 'NONE',  ( 11.78648345035340661, 7.593516549646560421, 455.0000000000000568 ) ) ;
#2927 = VERTEX_POINT ( 'NONE', #24575 ) ;
#2928 = ORIENTED_EDGE ( 'NONE', *, *, #39145, .F. ) ;
#2930 = ORIENTED_EDGE ( 'NONE', *, *, #13341, .F. ) ;
#2929 = DIRECTION ( 'NONE',  ( -1.794541526872559352E-16, -1.000000000000000000, 0.000000000000000000 ) ) ;
#2931 = VERTEX_POINT ( 'NONE', #17868 ) ;
#2932 = DIRECTION ( 'NONE',  ( 0.000000000000000000, 0.000000000000000000, -1.000000000000000000 ) ) ;
#2933 = DIRECTION ( 'NONE',  ( 1.000000000000000000, 0.000000000000000000, 0.000000000000000000 ) ) ;
#2934 = DIRECTION ( 'NONE',  ( 1.836970198721029934E-16, 1.836970198721010706E-16, -1.000000000000000000 ) ) ;
#2935 = FACE_OUTER_BOUND ( 'NONE', #41692, .T. ) ;
#2936 = PRESENTATION_LAYER_ASSIGNMENT (  '', '', ( #29882 ) ) ;
#2937 = DIRECTION ( 'NONE',  ( 1.000000000000000000, 0.000000000000000000, 0.000000000000000000 ) ) ;
#2938 = DIRECTION ( 'NONE',  ( 0.000000000000000000, 0.6857142857146703019, -0.7278708115914659382 ) ) ;
#2939 = ORIENTED_EDGE ( 'NONE', *, *, #5863, .F. ) ;
#2940 = ORIENTED_EDGE ( 'NONE', *, *, #28231, .T. ) ;
#2941 = ORIENTED_EDGE ( 'NONE', *, *, #46000, .T. ) ;
#2942 = EDGE_CURVE ( 'NONE', #1978, #5458, #18484, .T. ) ;
#2943 = VERTEX_POINT ( 'NONE', #18917 ) ;
#2944 = CARTESIAN_POINT ( 'NONE',  ( 0.000000000000000000, -7.449999999999998401, -21.00000000000000000 ) ) ;
#2945 =( REPRESENTATION_RELATIONSHIP ('NONE','NONE', #33057, #53035 ) REPRESENTATION_RELATIONSHIP_WITH_TRANSFORMATION ( #68883 )SHAPE_REPRESENTATION_RELATIONSHIP( ) );
#2946 = CARTESIAN_POINT ( 'NONE',  ( 7.250000000000005329, -8.249999999999998224, -12.50000000000000000 ) ) ;
#2947 = EDGE_CURVE ( 'NONE', #49494, #4296, #40474, .T. ) ;
#2948 = CARTESIAN_POINT ( 'NONE',  ( 78.77321854994620765, 47.95351654967443977, 26.00000000000000355 ) ) ;
#2949 = ORIENTED_EDGE ( 'NONE', *, *, #50142, .T. ) ;
#2950 = ORIENTED_EDGE ( 'NONE', *, *, #30654, .F. ) ;
#2951 = AXIS2_PLACEMENT_3D ( 'NONE', #45058, #66632, #18187 ) ;
#2952 = ORIENTED_EDGE ( 'NONE', *, *, #27943, .T. ) ;
#2953 = DIRECTION ( 'NONE',  ( -1.000000000000000000, 0.000000000000000000, 0.000000000000000000 ) ) ;
#2954 = ORIENTED_EDGE ( 'NONE', *, *, #51097, .F. ) ;
#2955 = AXIS2_PLACEMENT_3D ( 'NONE', #18935, #33791, #7958 ) ;
#2956 = ORIENTED_EDGE ( 'NONE', *, *, #12121, .T. ) ;
#2957 = CARTESIAN_POINT ( 'NONE',  ( -3.650476262117221093, 10.49297626211717116, 54.00000000000000711 ) ) ;
#2958 = VERTEX_POINT ( 'NONE', #23864 ) ;
#2959 = ORIENTED_EDGE ( 'NONE', *, *, #66910, .F. ) ;
#2960 = VECTOR ( 'NONE', #59887, 1000.000000000000000 ) ;
#2961 = DIRECTION ( 'NONE',  ( 0.000000000000000000, 3.673940397442059868E-16, -1.000000000000000000 ) ) ;
#2962 = ADVANCED_FACE ( 'NONE', ( #34812 ), #24218, .F. ) ;
#2964 = ORIENTED_EDGE ( 'NONE', *, *, #8071, .F. ) ;
#2963 = FACE_OUTER_BOUND ( 'NONE', #3451, .T. ) ;
#2965 = VERTEX_POINT ( 'NONE', #45423 ) ;
#2966 = DIRECTION ( 'NONE',  ( 0.000000000000000000, 0.000000000000000000, -1.000000000000000000 ) ) ;
#2967 = AXIS2_PLACEMENT_3D ( 'NONE', #30549, #9688, #25246 ) ;
#2968 = VECTOR ( 'NONE', #30045, 1000.000000000000000 ) ;
#2969 = VECTOR ( 'NONE', #37503, 1000.000000000000000 ) ;
#2970 = DIRECTION ( 'NONE',  ( 0.000000000000000000, 1.000000000000000000, 0.000000000000000000 ) ) ;
#2971 = CARTESIAN_POINT ( 'NONE',  ( -28.00000000000000000, -15.50000000000000000, 14.50000000000000000 ) ) ;
#2972 = EDGE_CURVE ( 'NONE', #62416, #64892, #20723, .T. ) ;
#2974 = ORIENTED_EDGE ( 'NONE', *, *, #15266, .T. ) ;
#2973 = CARTESIAN_POINT ( 'NONE',  ( 4.740315990920191958, 4.188533722949208560, 455.0000000000000568 ) ) ;
#2975 = ADVANCED_FACE ( 'NONE', ( #51440 ), #29164, .F. ) ;
#2976 = ORIENTED_EDGE ( 'NONE', *, *, #65832, .F. ) ;
#2977 = VECTOR ( 'NONE', #69791, 1000.000000000000000 ) ;
#2978 = VECTOR ( 'NONE', #61353, 1000.000000000000000 ) ;
#2979 = VECTOR ( 'NONE', #44158, 1000.000000000000000 ) ;
#2980 = ADVANCED_FACE ( 'NONE', ( #1594 ), #29865, .F. ) ;
#2981 = DIRECTION ( 'NONE',  ( 1.000000000000000000, 1.084202172485504434E-16, 0.000000000000000000 ) ) ;
#2982 = EDGE_CURVE ( 'NONE', #25281, #14316, #55359, .T. ) ;
#2983 = ADVANCED_FACE ( 'NONE', ( #50387 ), #1955, .F. ) ;
#2984 = DIRECTION ( 'NONE',  ( 1.836970198721029934E-16, 1.836970198721010706E-16, -1.000000000000000000 ) ) ;
#2985 = LINE ( 'NONE', #67338, #6758 ) ;
#2986 = TOROIDAL_SURFACE ( 'NONE', #21058, 0.06000000000000080963, 0.7500000000000000000 ) ;
#2987 = ORIENTED_EDGE ( 'NONE', *, *, #26747, .T. ) ;
#2988 = DIRECTION ( 'NONE',  ( 3.304235192336778667E-15, 1.000000000000000000, 0.000000000000000000 ) ) ;
#2989 = EDGE_CURVE ( 'NONE', #11608, #39751, #45779, .T. ) ;
#2990 = VECTOR ( 'NONE', #61660, 1000.000000000000000 ) ;
#2991 = DIRECTION ( 'NONE',  ( 0.000000000000000000, -1.000000000000000000, 0.000000000000000000 ) ) ;
#2992 = DIRECTION ( 'NONE',  ( 0.000000000000000000, -0.7057491738665943037, -0.7084617869628675457 ) ) ;
#2993 = EDGE_CURVE ( 'NONE', #66919, #61999, #62493, .T. ) ;
#2994 = ORIENTED_EDGE ( 'NONE', *, *, #3222, .T. ) ;
#2995 = CARTESIAN_POINT ( 'NONE',  ( 13.00000000000000178, -16.64230188589299786, -14.64519951917100116 ) ) ;
#2996 = ADVANCED_FACE ( 'NONE', ( #3007 ), #23517, .T. ) ;
#2997 = CARTESIAN_POINT ( 'NONE',  ( 29.50000000000000355, -11.50000000000100009, -15.00000000000084910 ) ) ;
#2998 = DIRECTION ( 'NONE',  ( -1.000000000000000000, 0.000000000000000000, 0.000000000000000000 ) ) ;
#2999 = DIRECTION ( 'NONE',  ( 1.000000000000000000, 0.000000000000000000, 0.000000000000000000 ) ) ;
#3000 = ORIENTED_EDGE ( 'NONE', *, *, #40561, .T. ) ;
#3001 = DIRECTION ( 'NONE',  ( -1.000000000000000000, 0.000000000000000000, 0.000000000000000000 ) ) ;
#3002 = EDGE_CURVE ( 'NONE', #59936, #58981, #21890, .T. ) ;
#3003 = DIRECTION ( 'NONE',  ( -1.000000000000000000, 0.000000000000000000, 0.000000000000000000 ) ) ;
#3004 = EDGE_CURVE ( 'NONE', #54028, #17979, #56044, .T. ) ;
#3005 = EDGE_LOOP ( 'NONE', ( #6232, #45603 ) ) ;
#3006 = DIRECTION ( 'NONE',  ( -1.000000000000000000, 0.000000000000000000, 0.000000000000000000 ) ) ;
#3007 = FACE_OUTER_BOUND ( 'NONE', #21735, .T. ) ;
#3008 = DIRECTION ( 'NONE',  ( -1.000000000000000000, 0.000000000000000000, 0.000000000000000000 ) ) ;
#3009 = CARTESIAN_POINT ( 'NONE',  ( -7.250000000000000888, 7.250000000000001776, -26.00000000000001066 ) ) ;
#3010 = DIRECTION ( 'NONE',  ( 1.836970198721029934E-16, 1.836970198721010706E-16, -1.000000000000000000 ) ) ;
#3011 = VERTEX_POINT ( 'NONE', #7600 ) ;
#3012 = CARTESIAN_POINT ( 'NONE',  ( 11.75000000000000000, -5.200000000000001066, 26.25000000000000000 ) ) ;
#3013 = DIRECTION ( 'NONE',  ( -0.000000000000000000, 3.673940397442059868E-16, -1.000000000000000000 ) ) ;
#3014 = CIRCLE ( 'NONE', #42536, 24.99999999998784972 ) ;
#3015 = EDGE_CURVE ( 'NONE', #1150, #54119, #7240, .T. ) ;
#3016 = DIRECTION ( 'NONE',  ( 0.000000000000000000, 0.000000000000000000, 1.000000000000000000 ) ) ;
#3017 = VECTOR ( 'NONE', #61130, 1000.000000000000000 ) ;
#3018 = AXIS2_PLACEMENT_3D ( 'NONE', #66870, #39988, #18424 ) ;
#3019 = LINE ( 'NONE', #18565, #62458 ) ;
#3020 = LINE ( 'NONE', #24587, #66702 ) ;
#3021 = ORIENTED_EDGE ( 'NONE', *, *, #19474, .F. ) ;
#3023 = ORIENTED_EDGE ( 'NONE', *, *, #12455, .T. ) ;
#3022 = CARTESIAN_POINT ( 'NONE',  ( -24.00000000000000000, -17.50000000000000000, -19.33772233983200195 ) ) ;
#3024 = AXIS2_PLACEMENT_3D ( 'NONE', #51443, #18557, #8655 ) ;
#3025 = VECTOR ( 'NONE', #58679, 1000.000000000000000 ) ;
#3026 = AXIS2_PLACEMENT_3D ( 'NONE', #42452, #64715, #32884 ) ;
#3027 = CARTESIAN_POINT ( 'NONE',  ( 6.006483450353379716, -6.006483450353394815, 195.0000000000000284 ) ) ;
#3028 = AXIS2_PLACEMENT_3D ( 'NONE', #23897, #41203, #13985 ) ;
#3029 = CARTESIAN_POINT ( 'NONE',  ( 11.78648345035337819, -7.606483450353493936, 455.0000000000000568 ) ) ;
#3030 = CYLINDRICAL_SURFACE ( 'NONE', #4850, 0.1749999999999998224 ) ;
#3031 = EDGE_LOOP ( 'NONE', ( #46741, #15515, #66730, #1213 ) ) ;
#3032 = AXIS2_PLACEMENT_3D ( 'NONE', #25521, #62994, #57681 ) ;
#3033 = LINE ( 'NONE', #34475, #62310 ) ;
#3034 = ORIENTED_EDGE ( 'NONE', *, *, #1447, .F. ) ;
#3035 = ADVANCED_FACE ( 'NONE', ( #68053 ), #42222, .F. ) ;
#3036 = CIRCLE ( 'NONE', #42561, 0.5249999999999994671 ) ;
#3037 = EDGE_LOOP ( 'NONE', ( #43907, #36774, #68467, #9501 ) ) ;
#3038 = ORIENTED_EDGE ( 'NONE', *, *, #38237, .T. ) ;
#3039 = CARTESIAN_POINT ( 'NONE',  ( 25.57999999999999829, 0.000000000000000000, 0.000000000000000000 ) ) ;
#3040 = LINE ( 'NONE', #40852, #69302 ) ;
#3041 = ADVANCED_FACE ( 'NONE', ( #53212 ), #19260, .F. ) ;
#3042 = LINE ( 'NONE', #29189, #5541 ) ;
#3043 = DIRECTION ( 'NONE',  ( 0.000000000000000000, 1.000000000000000000, 0.000000000000000000 ) ) ;
#3044 = VECTOR ( 'NONE', #18798, 1000.000000000000000 ) ;
#3045 = ORIENTED_EDGE ( 'NONE', *, *, #7343, .T. ) ;
#3046 = ORIENTED_EDGE ( 'NONE', *, *, #17068, .F. ) ;
#3047 = EDGE_CURVE ( 'NONE', #19854, #10245, #47877, .T. ) ;
#3048 = CARTESIAN_POINT ( 'NONE',  ( -7.450000000000001954, 0.000000000000000000, -20.50000000000000000 ) ) ;
#3049 = CARTESIAN_POINT ( 'NONE',  ( 6.006483450353353959, 5.993516549646629166, 195.0000000000000284 ) ) ;
#3050 = ORIENTED_EDGE ( 'NONE', *, *, #7320, .F. ) ;
#3051 = EDGE_CURVE ( 'NONE', #27113, #13327, #51793, .T. ) ;
#3052 = VERTEX_POINT ( 'NONE', #30923 ) ;
#3053 = ORIENTED_EDGE ( 'NONE', *, *, #52892, .T. ) ;
#3054 = CARTESIAN_POINT ( 'NONE',  ( 15.50000000000000000, -1.037157890325000054, -22.50000000000000000 ) ) ;
#3055 = EDGE_CURVE ( 'NONE', #37912, #38019, #20313, .T. ) ;
#3057 = ORIENTED_EDGE ( 'NONE', *, *, #59190, .T. ) ;
#3056 = CARTESIAN_POINT ( 'NONE',  ( -8.916576262117260399, 8.566576262117216345, 26.00000000000000711 ) ) ;
#3058 = DIRECTION ( 'NONE',  ( 1.000000000000000000, -0.000000000000000000, 0.000000000000000000 ) ) ;
#3059 = CARTESIAN_POINT ( 'NONE',  ( 49.00000000000000000, 20.60000000000000142, -13.86939075806900057 ) ) ;
#3060 = AXIS2_PLACEMENT_3D ( 'NONE', #25438, #30392, #9174 ) ;
#3061 = VERTEX_POINT ( 'NONE', #41533 ) ;
#3062 = ORIENTED_EDGE ( 'NONE', *, *, #53073, .F. ) ;
#3063 = EDGE_CURVE ( 'NONE', #58960, #59292, #40827, .T. ) ;
#3064 = CARTESIAN_POINT ( 'NONE',  ( 8.250000000000005329, -7.249999999999998224, -26.00000000000001066 ) ) ;
#3065 = CARTESIAN_POINT ( 'NONE',  ( 6.665817930929289759, 7.517976262117195496, 54.00000000000000711 ) ) ;
#3066 = CIRCLE ( 'NONE', #35814, 2.250000000000001776 ) ;
#3067 = VECTOR ( 'NONE', #39151, 1000.000000000000000 ) ;
#3068 = CYLINDRICAL_SURFACE ( 'NONE', #45050, 3.500000000000000000 ) ;
#3069 = CONICAL_SURFACE ( 'NONE', #56165, 2.458500000000000796, 1.047019301333029784 ) ;
#3070 = AXIS2_PLACEMENT_3D ( 'NONE', #68809, #35286, #30973 ) ;
#3071 = CARTESIAN_POINT ( 'NONE',  ( -9.722976262117249746, -3.682023737882726522, 54.00000000000000711 ) ) ;
#3073 = CARTESIAN_POINT ( 'NONE',  ( 11.48848345035341900, 10.19191654964656202, 455.0000000000000568 ) ) ;
#3072 = AXIS2_PLACEMENT_3D ( 'NONE', #12664, #7368, #101 ) ;
#3075 = EDGE_LOOP ( 'NONE', ( #56979, #48373, #24959, #46643 ) ) ;
#3074 = CARTESIAN_POINT ( 'NONE',  ( -7.450000000000001954, 0.000000000000000000, -24.50000000000000000 ) ) ;
#3076 = VERTEX_POINT ( 'NONE', #19602 ) ;
#3077 = DIRECTION ( 'NONE',  ( -1.000000000000000000, 0.000000000000000000, -8.480870326997715333E-15 ) ) ;
#3078 = CARTESIAN_POINT ( 'NONE',  ( 39.90000000000000568, 21.00000000000000000, -16.96999999999999886 ) ) ;
#3079 = AXIS2_PLACEMENT_3D ( 'NONE', #18190, #558, #61676 ) ;
#3080 = VECTOR ( 'NONE', #15220, 1000.000000000000000 ) ;
#3081 = DIRECTION ( 'NONE',  ( -1.000000000000000000, 0.000000000000000000, 0.000000000000000000 ) ) ;
#3082 = CARTESIAN_POINT ( 'NONE',  ( 5.257023737882819070, -5.257023737882815517, 26.00000000000000711 ) ) ;
#3083 = CARTESIAN_POINT ( 'NONE',  ( 14.25000000000000000, -2.500000000000000000, 21.77831216351300014 ) ) ;
#3084 = EDGE_LOOP ( 'NONE', ( #28669, #10413, #22405, #32746, #30230, #35069, #12461, #48495 ) ) ;
#3085 = CARTESIAN_POINT ( 'NONE',  ( 7.000000000000000000, -20.49999999999999645, 16.03137303340311348 ) ) ;
#3086 = FACE_OUTER_BOUND ( 'NONE', #51552, .T. ) ;
#3087 = ADVANCED_FACE ( 'NONE', ( #62380 ), #25269, .T. ) ;
#3088 = DIRECTION ( 'NONE',  ( 1.000000000000000000, 0.000000000000000000, 0.000000000000000000 ) ) ;
#3089 = EDGE_CURVE ( 'NONE', #7820, #32087, #63101, .T. ) ;
#3090 = DIRECTION ( 'NONE',  ( -1.000000000000000000, 0.000000000000000000, 0.000000000000000000 ) ) ;
#3091 = FACE_OUTER_BOUND ( 'NONE', #46101, .T. ) ;
#3092 = DIRECTION ( 'NONE',  ( 1.000000000000000000, 0.000000000000000000, 0.000000000000000000 ) ) ;
#3093 = ORIENTED_EDGE ( 'NONE', *, *, #1284, .T. ) ;
#3094 = DIRECTION ( 'NONE',  ( 0.000000000000000000, 0.000000000000000000, 1.000000000000000000 ) ) ;
#3095 = DIRECTION ( 'NONE',  ( -0.000000000000000000, 0.000000000000000000, 1.000000000000000000 ) ) ;
#3096 = VERTEX_POINT ( 'NONE', #4760 ) ;
#3097 = CARTESIAN_POINT ( 'NONE',  ( -7.593516549646838421, -11.78648345035340839, 455.0000000000000568 ) ) ;
#3098 = DIRECTION ( 'NONE',  ( 0.000000000000000000, 0.000000000000000000, -1.000000000000000000 ) ) ;
#3099 = DIRECTION ( 'NONE',  ( 0.7071067811865475727, 0.7071067811865475727, -0.000000000000000000 ) ) ;
#3100 = DIRECTION ( 'NONE',  ( -0.000000000000000000, -0.000000000000000000, 1.000000000000000000 ) ) ;
#3101 = PLANE ( 'NONE',  #2263 ) ;
#3102 = ORIENTED_EDGE ( 'NONE', *, *, #58936, .F. ) ;
#3103 = DIRECTION ( 'NONE',  ( 1.000000000000000000, 0.000000000000000000, 0.000000000000000000 ) ) ;
#3104 = ORIENTED_EDGE ( 'NONE', *, *, #124, .T. ) ;
#3105 = LINE ( 'NONE', #1440, #21392 ) ;
#3106 = DIRECTION ( 'NONE',  ( 1.000000000000000000, -1.047444401652940007E-14, 1.836970198721010706E-16 ) ) ;
#3107 = AXIS2_PLACEMENT_3D ( 'NONE', #38321, #11093, #33353 ) ;
#3108 = ORIENTED_EDGE ( 'NONE', *, *, #3126, .F. ) ;
#3109 = LINE ( 'NONE', #61799, #41579 ) ;
#3110 = ORIENTED_EDGE ( 'NONE', *, *, #59580, .F. ) ;
#3111 = VECTOR ( 'NONE', #58580, 1000.000000000000000 ) ;
#3112 = CARTESIAN_POINT ( 'NONE',  ( -8.393516549646779623, -6.344579767990844665, 455.0000000000000568 ) ) ;
#3113 = ORIENTED_EDGE ( 'NONE', *, *, #40487, .F. ) ;
#3114 = EDGE_LOOP ( 'NONE', ( #58283, #34162, #31033, #23673 ) ) ;
#3115 = LINE ( 'NONE', #25378, #11402 ) ;
#3116 = ORIENTED_EDGE ( 'NONE', *, *, #68278, .T. ) ;
#3117 = VERTEX_POINT ( 'NONE', #15012 ) ;
#3118 = AXIS2_PLACEMENT_3D ( 'NONE', #69373, #63730, #26588 ) ;
#3119 = ADVANCED_FACE ( 'NONE', ( #4419 ), #9716, .T. ) ;
#3120 = AXIS2_PLACEMENT_3D ( 'NONE', #34000, #56960, #1830 ) ;
#3121 = LINE ( 'NONE', #28582, #7836 ) ;
#3122 = DIRECTION ( 'NONE',  ( 0.000000000000000000, 0.000000000000000000, 1.000000000000000000 ) ) ;
#3123 = LINE ( 'NONE', #57553, #11800 ) ;
#3124 = PRODUCT_DEFINITION_FORMATION_WITH_SPECIFIED_SOURCE ( 'ANY', '', #56556, .NOT_KNOWN. ) ;
#3125 = ORIENTED_EDGE ( 'NONE', *, *, #51177, .T. ) ;
#3126 = EDGE_CURVE ( 'NONE', #24433, #9595, #36569, .T. ) ;
#3127 = LINE ( 'NONE', #7014, #41327 ) ;
#3128 = AXIS2_PLACEMENT_3D ( 'NONE', #66980, #46464, #56034 ) ;
#3130 = DIRECTION ( 'NONE',  ( 0.000000000000000000, -0.000000000000000000, 1.000000000000000000 ) ) ;
#3129 = LINE ( 'NONE', #57558, #62023 ) ;
#3131 = ORIENTED_EDGE ( 'NONE', *, *, #65282, .T. ) ;
#3133 = VERTEX_POINT ( 'NONE', #69104 ) ;
#3132 = CARTESIAN_POINT ( 'NONE',  ( 73.77321854994620765, 47.95351654967443977, 15.00000000000000000 ) ) ;
#3134 = EDGE_CURVE ( 'NONE', #29241, #49648, #46477, .T. ) ;
#3135 = ORIENTED_EDGE ( 'NONE', *, *, #23330, .T. ) ;
#3136 = EDGE_CURVE ( 'NONE', #32081, #47780, #15368, .T. ) ;
#3137 = APPLICATION_PROTOCOL_DEFINITION ( 'draft international standard', 'automotive_design', 1998, #23686 ) ;
#3138 = EDGE_CURVE ( 'NONE', #34214, #37466, #14659, .T. ) ;
#3139 = EDGE_CURVE ( 'NONE', #17432, #64, #46824, .T. ) ;
#3140 = PLANE ( 'NONE',  #24314 ) ;
#3142 = EDGE_LOOP ( 'NONE', ( #23809, #13514, #32415, #24549 ) ) ;
#3141 = CARTESIAN_POINT ( 'NONE',  ( 6.006483450353361953, 8.198316549646628815, 195.0000000000000284 ) ) ;
#3143 = VECTOR ( 'NONE', #69172, 999.9999999999998863 ) ;
#3144 = CARTESIAN_POINT ( 'NONE',  ( 6.006483450353353959, 5.993516549646629166, 195.0000000000000284 ) ) ;
#3145 = EDGE_CURVE ( 'NONE', #44522, #21711, #50139, .T. ) ;
#3146 = CARTESIAN_POINT ( 'NONE',  ( -5.380658396643321240, -7.265214908726175480, 455.0000000000000568 ) ) ;
#3147 = EDGE_LOOP ( 'NONE', ( #19987, #516, #19250, #56082 ) ) ;
#3148 = EDGE_LOOP ( 'NONE', ( #533, #30779 ) ) ;
#3149 = DIRECTION ( 'NONE',  ( -0.000000000000000000, -0.000000000000000000, -1.000000000000000000 ) ) ;
#3150 = ORIENTED_EDGE ( 'NONE', *, *, #36264, .T. ) ;
#3151 = PLANE ( 'NONE',  #24566 ) ;
#3152 = CARTESIAN_POINT ( 'NONE',  ( 6.849523737882814878, 10.30047626211719702, 26.00000000000000711 ) ) ;
#3153 = DIRECTION ( 'NONE',  ( -0.7071067811865446862, 0.7071067811865503483, 0.000000000000000000 ) ) ;
#3154 = EDGE_LOOP ( 'NONE', ( #62891, #51251, #14686, #44057 ) ) ;
#3155 = DIRECTION ( 'NONE',  ( -1.000000000000000000, 0.000000000000000000, 0.000000000000000000 ) ) ;
#3156 = PLANE ( 'NONE',  #24630 ) ;
#3157 = VECTOR ( 'NONE', #6137, 1000.000000000000000 ) ;
#3159 = ORIENTED_EDGE ( 'NONE', *, *, #63992, .F. ) ;
#3158 = CYLINDRICAL_SURFACE ( 'NONE', #30849, 0.5000000000000000000 ) ;
#3161 = ORIENTED_EDGE ( 'NONE', *, *, #21418, .T. ) ;
#3160 = LINE ( 'NONE', #24720, #68186 ) ;
#3162 = LINE ( 'NONE', #13407, #24979 ) ;
#3163 = LINE ( 'NONE', #57943, #37545 ) ;
#3164 = DIRECTION ( 'NONE',  ( 1.000000000000000000, 0.000000000000000000, 0.000000000000000000 ) ) ;
#3165 = CARTESIAN_POINT ( 'NONE',  ( 5.793274621760843957, -6.358413763958979281, 54.00000000000000711 ) ) ;
#3166 = DIRECTION ( 'NONE',  ( -0.000000000000000000, -1.000000000000000000, 0.000000000000000000 ) ) ;
#3167 = ORIENTED_EDGE ( 'NONE', *, *, #5781, .T. ) ;
#3168 = LINE ( 'NONE', #58320, #47025 ) ;
#3169 = CARTESIAN_POINT ( 'NONE',  ( 1.690483450353415629, 9.828310488885938057, 455.0000000000000568 ) ) ;
#3170 = LINE ( 'NONE', #40982, #10866 ) ;
#3171 = AXIS2_PLACEMENT_3D ( 'NONE', #4258, #47721, #47022 ) ;
#3173 = ORIENTED_EDGE ( 'NONE', *, *, #6778, .T. ) ;
#3172 = LINE ( 'NONE', #19760, #44587 ) ;
#3174 = EDGE_CURVE ( 'NONE', #32604, #34404, #52863, .T. ) ;
#3175 = DIRECTION ( 'NONE',  ( -1.000000000000000000, 0.000000000000000000, 0.000000000000000000 ) ) ;
#3176 = EDGE_CURVE ( 'NONE', #21488, #15324, #33189, .T. ) ;
#3177 = FACE_OUTER_BOUND ( 'NONE', #25310, .T. ) ;
#3178 = EDGE_CURVE ( 'NONE', #52634, #66712, #35446, .T. ) ;
#3179 = VECTOR ( 'NONE', #34237, 1000.000000000000000 ) ;
#3180 = AXIS2_PLACEMENT_3D ( 'NONE', #30604, #20685, #15398 ) ;
#3181 = ORIENTED_EDGE ( 'NONE', *, *, #35327, .T. ) ;
#3182 = VERTEX_POINT ( 'NONE', #26671 ) ;
#3183 = CARTESIAN_POINT ( 'NONE',  ( -16.94999999999999929, -0.2000000000000000111, -22.50000000000000000 ) ) ;
#3184 = CARTESIAN_POINT ( 'NONE',  ( 1.690483450353351458, -9.841277389592800517, 455.0000000000000568 ) ) ;
#3186 = ORIENTED_EDGE ( 'NONE', *, *, #28073, .T. ) ;
#3185 = EDGE_CURVE ( 'NONE', #51099, #18545, #16283, .T. ) ;
#3187 = CARTESIAN_POINT ( 'NONE',  ( 11.50000000000000000, -11.50000000000000000, 11.00000000000000000 ) ) ;
#3188 = FACE_OUTER_BOUND ( 'NONE', #37267, .T. ) ;
#3189 = CARTESIAN_POINT ( 'NONE',  ( -15.50000000000000000, -5.000000000000000000, 22.50000000000000000 ) ) ;
#3190 = AXIS2_PLACEMENT_3D ( 'NONE', #3692, #51429, #51784 ) ;
#3191 = CARTESIAN_POINT ( 'NONE',  ( 7.000000000000000000, -32.45000000000000995, 12.69999999999999929 ) ) ;
#3192 = ORIENTED_EDGE ( 'NONE', *, *, #52966, .T. ) ;
#3193 = CARTESIAN_POINT ( 'NONE',  ( 14.89999999999999680, -14.06939075806900163, -20.80000000000000426 ) ) ;
#3194 = VERTEX_POINT ( 'NONE', #38667 ) ;
#3195 = CARTESIAN_POINT ( 'NONE',  ( 49.00000000000000000, -14.06939075806900163, -20.80000000000000426 ) ) ;
#3196 = ORIENTED_EDGE ( 'NONE', *, *, #111, .F. ) ;
#3197 = LINE ( 'NONE', #39608, #25745 ) ;
#3198 = CARTESIAN_POINT ( 'NONE',  ( 8.689999999999999503, 9.750000000000000000, -5.000000000000000000 ) ) ;
#3199 = ORIENTED_EDGE ( 'NONE', *, *, #57483, .F. ) ;
#3200 = ORIENTED_EDGE ( 'NONE', *, *, #59766, .F. ) ;
#3201 = LINE ( 'NONE', #30417, #21667 ) ;
#3202 = ORIENTED_EDGE ( 'NONE', *, *, #38585, .T. ) ;
#3203 = ORIENTED_EDGE ( 'NONE', *, *, #12982, .F. ) ;
#3204 = EDGE_CURVE ( 'NONE', #7460, #20883, #34325, .T. ) ;
#3205 = DIRECTION ( 'NONE',  ( 0.000000000000000000, 0.000000000000000000, 1.000000000000000000 ) ) ;
#3206 = LINE ( 'NONE', #2492, #35776 ) ;
#3207 = CARTESIAN_POINT ( 'NONE',  ( 8.211283450353379365, -6.006483450353394815, 195.0000000000000284 ) ) ;
#3208 = DIRECTION ( 'NONE',  ( -9.912705577010344285E-15, -1.000000000000000000, 0.000000000000000000 ) ) ;
#3209 = VERTEX_POINT ( 'NONE', #15715 ) ;
#3210 = DIRECTION ( 'NONE',  ( 1.000000000000000000, 0.000000000000000000, 0.000000000000000000 ) ) ;
#3212 = LINE ( 'NONE', #19805, #32364 ) ;
#3211 = CARTESIAN_POINT ( 'NONE',  ( 11.78648345035337819, -7.606483450353493936, 455.0000000000000568 ) ) ;
#3213 = VERTEX_POINT ( 'NONE', #42924 ) ;
#3215 = EDGE_LOOP ( 'NONE', ( #12569, #14902, #54564, #45194 ) ) ;
#3214 = CARTESIAN_POINT ( 'NONE',  ( -7.342976262117273833, -4.961189459950004377, 54.00000000000000711 ) ) ;
#3216 = ORIENTED_EDGE ( 'NONE', *, *, #36059, .T. ) ;
#3217 = ORIENTED_EDGE ( 'NONE', *, *, #22049, .T. ) ;
#3218 = EDGE_CURVE ( 'NONE', #41932, #56820, #22413, .T. ) ;
#3219 = DIRECTION ( 'NONE',  ( 0.000000000000000000, 0.000000000000000000, 1.000000000000000000 ) ) ;
#3220 = VECTOR ( 'NONE', #47636, 1000.000000000000000 ) ;
#3221 = CYLINDRICAL_SURFACE ( 'NONE', #21422, 5.000000000000000000 ) ;
#3222 = EDGE_CURVE ( 'NONE', #7022, #61584, #27588, .T. ) ;
#3223 = ORIENTED_EDGE ( 'NONE', *, *, #41811, .T. ) ;
#3224 = ORIENTED_EDGE ( 'NONE', *, *, #29632, .T. ) ;
#3225 = VECTOR ( 'NONE', #41858, 1000.000000000000000 ) ;
#3226 = LINE ( 'NONE', #20528, #7050 ) ;
#3227 = DIRECTION ( 'NONE',  ( 0.000000000000000000, -1.000000000000000000, 3.989863994748342081E-13 ) ) ;
#3228 = ORIENTED_EDGE ( 'NONE', *, *, #20624, .T. ) ;
#3229 = ORIENTED_EDGE ( 'NONE', *, *, #51999, .T. ) ;
#3230 = DIRECTION ( 'NONE',  ( 0.000000000000000000, 0.000000000000000000, 1.000000000000000000 ) ) ;
#3231 = DIRECTION ( 'NONE',  ( -1.000000000000000000, 0.000000000000000000, 0.000000000000000000 ) ) ;
#3232 = EDGE_LOOP ( 'NONE', ( #29472, #40885, #34702, #23697 ) ) ;
#3233 = AXIS2_PLACEMENT_3D ( 'NONE', #4580, #53714, #26844 ) ;
#3234 = DIRECTION ( 'NONE',  ( 0.000000000000000000, 1.000000000000000000, 0.000000000000000000 ) ) ;
#3235 = CARTESIAN_POINT ( 'NONE',  ( 8.406483450353379183, -5.668387132716048882, 455.0000000000000568 ) ) ;
#3237 = ORIENTED_EDGE ( 'NONE', *, *, #59425, .T. ) ;
#3236 = DIRECTION ( 'NONE',  ( -0.000000000000000000, -0.000000000000000000, -1.000000000000000000 ) ) ;
#3238 = EDGE_LOOP ( 'NONE', ( #61198, #10889, #1184, #15590, #5381, #30874, #63407, #27845, #43213, #49891, #12745, #26400, #49474, #15884, #11198, #61357, #41052, #52342, #10629, #38416, #27315, #43348, #47848, #18286, #15373, #67091, #24435, #31034, #54275, #64877, #17293, #56855, #11270, #38580, #54597 ) ) ;
#3239 = FACE_OUTER_BOUND ( 'NONE', #59744, .T. ) ;
#3240 = CARTESIAN_POINT ( 'NONE',  ( 11.00000000000000000, -13.79999999999979998, 17.64999999999988844 ) ) ;
#3241 = FACE_OUTER_BOUND ( 'NONE', #11427, .T. ) ;
#3242 = DIRECTION ( 'NONE',  ( -0.000000000000000000, -0.000000000000000000, -1.000000000000000000 ) ) ;
#3243 = CYLINDRICAL_SURFACE ( 'NONE', #5265, 0.1749999999999989342 ) ;
#3244 = CARTESIAN_POINT ( 'NONE',  ( 8.250000000000005329, -7.249999999999998224, -26.00000000000001066 ) ) ;
#3245 = CARTESIAN_POINT ( 'NONE',  ( -30.00000000000000000, -10.85999999999999943, 9.350000000000269651 ) ) ;
#3246 = VERTEX_POINT ( 'NONE', #37285 ) ;
#3247 = DIRECTION ( 'NONE',  ( 0.000000000000000000, -0.1111111111108840643, -0.9938079899999319178 ) ) ;
#3249 = ORIENTED_EDGE ( 'NONE', *, *, #62051, .F. ) ;
#3248 = LINE ( 'NONE', #26219, #24336 ) ;
#3250 = CYLINDRICAL_SURFACE ( 'NONE', #59219, 0.4999999999991850963 ) ;
#3251 = LINE ( 'NONE', #20210, #35750 ) ;
#3252 = LINE ( 'NONE', #61230, #63039 ) ;
#3253 = EDGE_CURVE ( 'NONE', #49587, #26502, #48936, .T. ) ;
#3254 = CARTESIAN_POINT ( 'NONE',  ( 283.0000000000000568, -20.50000000000000000, -13.00000000000000178 ) ) ;
#3255 = FACE_OUTER_BOUND ( 'NONE', #16063, .T. ) ;
#3256 = ORIENTED_EDGE ( 'NONE', *, *, #22041, .F. ) ;
#3257 = CARTESIAN_POINT ( 'NONE',  ( 1.090483450353420425, 11.33351654964659971, 455.0000000000000568 ) ) ;
#3258 = CARTESIAN_POINT ( 'NONE',  ( 30.00000000000000000, -17.00000000000000000, 15.70499999999969809 ) ) ;
#3260 = EDGE_LOOP ( 'NONE', ( #42424, #45796, #10768, #67926 ) ) ;
#3259 = EDGE_CURVE ( 'NONE', #49352, #54496, #52434, .T. ) ;
#3261 = AXIS2_PLACEMENT_3D ( 'NONE', #52173, #62773, #31329 ) ;
#3262 = DIRECTION ( 'NONE',  ( 0.000000000000000000, 1.000000000000000000, 0.000000000000000000 ) ) ;
#3263 = DIRECTION ( 'NONE',  ( 0.000000000000000000, 0.000000000000000000, 1.000000000000000000 ) ) ;
#3264 = ORIENTED_EDGE ( 'NONE', *, *, #33454, .T. ) ;
#3265 = DIRECTION ( 'NONE',  ( 1.000000000000000000, 0.000000000000000000, 0.000000000000000000 ) ) ;
#3266 = ORIENTED_EDGE ( 'NONE', *, *, #38956, .F. ) ;
#3267 = VERTEX_POINT ( 'NONE', #58850 ) ;
#3268 = CIRCLE ( 'NONE', #40553, 0.1749999999999998224 ) ;
#3269 = CARTESIAN_POINT ( 'NONE',  ( -7.450000000000001954, 7.250000000000000000, -19.00000000000000000 ) ) ;
#3270 = FACE_OUTER_BOUND ( 'NONE', #56070, .T. ) ;
#3271 = CARTESIAN_POINT ( 'NONE',  ( -11.33351654964668676, -1.090483450353329165, 455.0000000000000568 ) ) ;
#3272 = VECTOR ( 'NONE', #62564, 1000.000000000000000 ) ;
#3273 = FACE_OUTER_BOUND ( 'NONE', #61987, .T. ) ;
#3274 = EDGE_CURVE ( 'NONE', #41781, #62241, #43962, .T. ) ;
#3275 = DIRECTION ( 'NONE',  ( -0.000000000000000000, -0.000000000000000000, -1.000000000000000000 ) ) ;
#3276 = ORIENTED_EDGE ( 'NONE', *, *, #32419, .F. ) ;
#3277 = ORIENTED_EDGE ( 'NONE', *, *, #49222, .T. ) ;
#3279 = ORIENTED_EDGE ( 'NONE', *, *, #69682, .T. ) ;
#3278 = LINE ( 'NONE', #24848, #10360 ) ;
#3280 = ORIENTED_EDGE ( 'NONE', *, *, #54319, .T. ) ;
#3282 = CIRCLE ( 'NONE', #36036, 4.500000000000191847 ) ;
#3281 = AXIS2_PLACEMENT_3D ( 'NONE', #43789, #49779, #33852 ) ;
#3283 = CARTESIAN_POINT ( 'NONE',  ( -9.722976262117226653, -2.544523737882726344, 54.00000000000000711 ) ) ;
#3284 = CYLINDRICAL_SURFACE ( 'NONE', #16265, 1.000000000000001776 ) ;
#3285 = LINE ( 'NONE', #62322, #4134 ) ;
#3286 = DIRECTION ( 'NONE',  ( 0.000000000000000000, 1.000000000000000000, -0.000000000000000000 ) ) ;
#3287 = LINE ( 'NONE', #40045, #20947 ) ;
#3288 = AXIS2_PLACEMENT_3D ( 'NONE', #16995, #60461, #32910 ) ;
#3289 = CARTESIAN_POINT ( 'NONE',  ( 283.0000000000000568, -31.30000000000000071, -8.400000000000000355 ) ) ;
#3290 = ORIENTED_EDGE ( 'NONE', *, *, #31771, .T. ) ;
#3291 = ORIENTED_EDGE ( 'NONE', *, *, #57211, .T. ) ;
#3292 = ORIENTED_EDGE ( 'NONE', *, *, #47515, .F. ) ;
#3293 = VERTEX_POINT ( 'NONE', #59881 ) ;
#3294 = CARTESIAN_POINT ( 'NONE',  ( -7.252248008019455128, 5.380658396643134722, 455.0000000000000568 ) ) ;
#3295 = DIRECTION ( 'NONE',  ( 0.000000000000000000, -1.000000000000000000, -6.036837696397607468E-13 ) ) ;
#3296 = EDGE_CURVE ( 'NONE', #35441, #11801, #21937, .T. ) ;
#3297 = CARTESIAN_POINT ( 'NONE',  ( -15.50000000000000000, -0.2038245569916614930, 23.94337567297399971 ) ) ;
#3298 = EDGE_CURVE ( 'NONE', #8082, #16593, #42224, .T. ) ;
#3299 = EDGE_LOOP ( 'NONE', ( #41233, #6220, #68864, #10764 ) ) ;
#3300 = ORIENTED_EDGE ( 'NONE', *, *, #39904, .T. ) ;
#3301 = EDGE_CURVE ( 'NONE', #4233, #28489, #11436, .T. ) ;
#3302 = ORIENTED_EDGE ( 'NONE', *, *, #31296, .F. ) ;
#3303 = CARTESIAN_POINT ( 'NONE',  ( -11.18999999999999950, 11.18999999999999950, -4.250000000000000000 ) ) ;
#3304 = VERTEX_POINT ( 'NONE', #69451 ) ;
#3305 = EDGE_CURVE ( 'NONE', #46781, #47718, #31982, .T. ) ;
#3306 = ORIENTED_EDGE ( 'NONE', *, *, #66074, .F. ) ;
#3307 = LINE ( 'NONE', #15322, #23200 ) ;
#3309 = ORIENTED_EDGE ( 'NONE', *, *, #2427, .T. ) ;
#3308 = EDGE_CURVE ( 'NONE', #4926, #35831, #60283, .T. ) ;
#3310 = VECTOR ( 'NONE', #44330, 1000.000000000000000 ) ;
#3311 = ORIENTED_EDGE ( 'NONE', *, *, #8644, .T. ) ;
#3313 = EDGE_CURVE ( 'NONE', #30867, #14406, #5465, .T. ) ;
#3312 = LINE ( 'NONE', #47159, #48567 ) ;
#3314 = EDGE_CURVE ( 'NONE', #28510, #61067, #38835, .T. ) ;
#3316 = VERTEX_POINT ( 'NONE', #21713 ) ;
#3315 = CARTESIAN_POINT ( 'NONE',  ( 151.5599459900709860, -10.00000000000000178, 282.8454385697650082 ) ) ;
#3317 = AXIS2_PLACEMENT_3D ( 'NONE', #23011, #24669, #56830 ) ;
#3319 = ORIENTED_EDGE ( 'NONE', *, *, #51400, .F. ) ;
#3318 = ADVANCED_FACE ( 'NONE', ( #16408 ), #37985, .F. ) ;
#3320 = VECTOR ( 'NONE', #17628, 1000.000000000000000 ) ;
#3321 = PLANE ( 'NONE',  #17664 ) ;
#3322 = DIRECTION ( 'NONE',  ( 0.000000000000000000, 0.000000000000000000, -1.000000000000000000 ) ) ;
#3323 = LINE ( 'NONE', #18174, #21152 ) ;
#3325 = EDGE_LOOP ( 'NONE', ( #7327, #55183, #54105, #41269 ) ) ;
#3324 = LINE ( 'NONE', #30545, #14302 ) ;
#3326 = ORIENTED_EDGE ( 'NONE', *, *, #63904, .T. ) ;
#3327 = AXIS2_PLACEMENT_3D ( 'NONE', #14478, #24021, #51607 ) ;
#3328 = CYLINDRICAL_SURFACE ( 'NONE', #13095, 0.4000000000000010214 ) ;
#3329 = DIRECTION ( 'NONE',  ( 1.000000000000000000, -5.981805089575194965E-17, 0.000000000000000000 ) ) ;
#3330 = CARTESIAN_POINT ( 'NONE',  ( 41.09999999999999432, -0.2000000000000000111, 0.000000000000000000 ) ) ;
#3331 = AXIS2_PLACEMENT_3D ( 'NONE', #24277, #2011, #13660 ) ;
#3332 = DIRECTION ( 'NONE',  ( 1.115702204244422993E-14, 1.000000000000000000, 1.836970198721015882E-16 ) ) ;
#3333 = ORIENTED_EDGE ( 'NONE', *, *, #44868, .T. ) ;
#3334 = DIRECTION ( 'NONE',  ( 0.000000000000000000, 0.000000000000000000, 1.000000000000000000 ) ) ;
#3335 = CIRCLE ( 'NONE', #36085, 2.458500000000000796 ) ;
#3336 = CARTESIAN_POINT ( 'NONE',  ( -7.250000000000000888, 7.450000000000003730, -8.000000000000000000 ) ) ;
#3337 = CARTESIAN_POINT ( 'NONE',  ( 8.612468434717241550, -1.480523737882815549, 26.00000000000000711 ) ) ;
#3338 = VERTEX_POINT ( 'NONE', #11098 ) ;
#3339 = FACE_OUTER_BOUND ( 'NONE', #41905, .T. ) ;
#3340 = LINE ( 'NONE', #15352, #11412 ) ;
#3341 = VECTOR ( 'NONE', #5233, 1000.000000000000000 ) ;
#3342 = CARTESIAN_POINT ( 'NONE',  ( 7.250000000000005329, 7.250000000000000888, -12.00000000000000000 ) ) ;
#3343 = ORIENTED_EDGE ( 'NONE', *, *, #39047, .F. ) ;
#3344 = SURFACE_STYLE_FILL_AREA ( #18546 ) ;
#3345 = CARTESIAN_POINT ( 'NONE',  ( 9.562023737882805463, 8.130476262117184660, 54.00000000000000711 ) ) ;
#3346 = DIRECTION ( 'NONE',  ( 0.000000000000000000, 0.7066873191084661610, -0.7075259945834421194 ) ) ;
#3347 = ORIENTED_EDGE ( 'NONE', *, *, #5702, .F. ) ;
#3348 = VECTOR ( 'NONE', #6942, 1000.000000000000000 ) ;
#3349 = DIRECTION ( 'NONE',  ( 1.000000000000000000, 0.000000000000000000, 0.000000000000000000 ) ) ;
#3350 = CARTESIAN_POINT ( 'NONE',  ( -11.07551654964683330, -11.48848345035333907, 455.0000000000000568 ) ) ;
#3351 = LINE ( 'NONE', #18556, #5960 ) ;
#3352 = DIRECTION ( 'NONE',  ( -1.000000000000000000, 0.000000000000000000, 0.000000000000000000 ) ) ;
#3353 = DIRECTION ( 'NONE',  ( 0.000000000000000000, -0.1111111111108840643, -0.9938079899999319178 ) ) ;
#3355 = ORIENTED_EDGE ( 'NONE', *, *, #7512, .T. ) ;
#3354 = EDGE_CURVE ( 'NONE', #11776, #53694, #5804, .T. ) ;
#3356 = DIRECTION ( 'NONE',  ( 1.836970198721029934E-16, 1.836970198721010706E-16, -1.000000000000000000 ) ) ;
#3357 = DIRECTION ( 'NONE',  ( 0.000000000000000000, 0.000000000000000000, -1.000000000000000000 ) ) ;
#3358 = DIRECTION ( 'NONE',  ( -1.000000000000000000, 0.000000000000000000, 0.000000000000000000 ) ) ;
#3359 = EDGE_CURVE ( 'NONE', #20472, #66751, #38884, .T. ) ;
#3360 =( REPRESENTATION_RELATIONSHIP ('NONE','NONE', #4299, #64796 ) REPRESENTATION_RELATIONSHIP_WITH_TRANSFORMATION ( #50434 )SHAPE_REPRESENTATION_RELATIONSHIP( ) );
#3361 = CARTESIAN_POINT ( 'NONE',  ( 10.31452373788281562, -6.849523737882823760, 54.00000000000000711 ) ) ;
#3362 = ORIENTED_EDGE ( 'NONE', *, *, #44019, .F. ) ;
#3363 = VECTOR ( 'NONE', #67292, 1000.000000000000000 ) ;
#3365 = EDGE_LOOP ( 'NONE', ( #430, #37714, #11740, #16677 ) ) ;
#3364 = DIRECTION ( 'NONE',  ( 0.000000000000000000, -0.000000000000000000, 1.000000000000000000 ) ) ;
#3366 = AXIS2_PLACEMENT_3D ( 'NONE', #66680, #45450, #40505 ) ;
#3367 = AXIS2_PLACEMENT_3D ( 'NONE', #28552, #666, #6648 ) ;
#3368 = DIRECTION ( 'NONE',  ( 0.000000000000000000, 0.000000000000000000, 1.000000000000000000 ) ) ;
#3369 = CARTESIAN_POINT ( 'NONE',  ( 106.4257688009193998, 10.00000000000000000, 285.9830310981789125 ) ) ;
#3370 = CARTESIAN_POINT ( 'NONE',  ( 7.450000000000006395, 7.250000000000000888, -12.50000000000000000 ) ) ;
#3372 = ORIENTED_EDGE ( 'NONE', *, *, #44899, .T. ) ;
#3371 = EDGE_CURVE ( 'NONE', #56924, #37001, #24051, .T. ) ;
#3373 = AXIS2_PLACEMENT_3D ( 'NONE', #57861, #35952, #9429 ) ;
#3374 = CARTESIAN_POINT ( 'NONE',  ( -7.261609891743268541, -8.000000000000000000, 0.000000000000000000 ) ) ;
#3375 = VERTEX_POINT ( 'NONE', #61520 ) ;
#3376 = EDGE_CURVE ( 'NONE', #587, #30271, #29014, .T. ) ;
#3377 = CIRCLE ( 'NONE', #41737, 0.9999999999999991118 ) ;
#3378 = VERTEX_POINT ( 'NONE', #24760 ) ;
#3379 = ORIENTED_EDGE ( 'NONE', *, *, #5782, .F. ) ;
#3380 = CARTESIAN_POINT ( 'NONE',  ( 0.000000000000000000, 0.000000000000000000, -13.50000000000000178 ) ) ;
#3381 = AXIS2_PLACEMENT_3D ( 'NONE', #44339, #55658, #65913 ) ;
#3382 = CARTESIAN_POINT ( 'NONE',  ( -7.450000000000001954, 0.000000000000000000, -8.500000000000000000 ) ) ;
#3383 = CIRCLE ( 'NONE', #57587, 2.000000000000001776 ) ;
#3384 = CYLINDRICAL_SURFACE ( 'NONE', #32649, 1.000000000000000000 ) ;
#3385 = CARTESIAN_POINT ( 'NONE',  ( 27.00000000000000000, 0.000000000000000000, 0.000000000000000000 ) ) ;
#3386 = EDGE_CURVE ( 'NONE', #42535, #43129, #14504, .T. ) ;
#3387 = ORIENTED_EDGE ( 'NONE', *, *, #56039, .T. ) ;
#3388 = ORIENTED_EDGE ( 'NONE', *, *, #14739, .T. ) ;
#3389 = FACE_OUTER_BOUND ( 'NONE', #19594, .T. ) ;
#3390 = DIRECTION ( 'NONE',  ( -1.000000000000000000, 0.000000000000000000, 0.000000000000000000 ) ) ;
#3391 = VERTEX_POINT ( 'NONE', #67552 ) ;
#3392 = VERTEX_POINT ( 'NONE', #3198 ) ;
#3393 = VERTEX_POINT ( 'NONE', #13088 ) ;
#3394 = ORIENTED_EDGE ( 'NONE', *, *, #64702, .T. ) ;
#3395 = DIRECTION ( 'NONE',  ( 0.000000000000000000, 0.000000000000000000, 1.000000000000000000 ) ) ;
#3396 = UNCERTAINTY_MEASURE_WITH_UNIT (LENGTH_MEASURE( 1.000000000000000082E-05 ), #31112, 'distance_accuracy_value', 'NONE');
#3397 = EDGE_CURVE ( 'NONE', #54169, #19545, #33242, .T. ) ;
#3399 = EDGE_LOOP ( 'NONE', ( #57939, #47283, #25392, #29218 ) ) ;
#3398 = PLANE ( 'NONE',  #17543 ) ;
#3400 = EDGE_CURVE ( 'NONE', #53683, #49178, #41009, .T. ) ;
#3401 = CARTESIAN_POINT ( 'NONE',  ( -7.517976262117252340, -3.848229544836285321, 54.00000000000000711 ) ) ;
#3402 = CARTESIAN_POINT ( 'NONE',  ( 283.0000000000000568, -39.80000000000000426, -8.400000000000000355 ) ) ;
#3403 = VECTOR ( 'NONE', #9401, 1000.000000000000000 ) ;
#3404 = ORIENTED_EDGE ( 'NONE', *, *, #505, .T. ) ;
#3405 = ORIENTED_EDGE ( 'NONE', *, *, #45452, .F. ) ;
#3406 = ADVANCED_FACE ( 'NONE', ( #50923 ), #41365, .F. ) ;
#3407 = DIRECTION ( 'NONE',  ( -0.000000000000000000, -0.000000000000000000, -1.000000000000000000 ) ) ;
#3408 = LINE ( 'NONE', #46530, #27763 ) ;
#3409 = LINE ( 'NONE', #24977, #36083 ) ;
#3410 = VECTOR ( 'NONE', #21932, 1000.000000000000000 ) ;
#3411 = VECTOR ( 'NONE', #55701, 1000.000000000000000 ) ;
#3412 = FACE_OUTER_BOUND ( 'NONE', #37528, .T. ) ;
#3413 = DIRECTION ( 'NONE',  ( 1.920885163218982051E-15, 1.000000000000000000, 1.836970198721033139E-16 ) ) ;
#3415 = EDGE_LOOP ( 'NONE', ( #53166, #25420, #5626, #20052 ) ) ;
#3414 = FACE_OUTER_BOUND ( 'NONE', #14135, .T. ) ;
#3416 = ORIENTED_EDGE ( 'NONE', *, *, #51689, .T. ) ;
#3417 = DIRECTION ( 'NONE',  ( -0.000000000000000000, -0.000000000000000000, -1.000000000000000000 ) ) ;
#3419 = CARTESIAN_POINT ( 'NONE',  ( 0.000000000000000000, 0.000000000000000000, -5.000000000000000000 ) ) ;
#3418 = VECTOR ( 'NONE', #30647, 1000.000000000000000 ) ;
#3420 = CARTESIAN_POINT ( 'NONE',  ( -8.750000000000003553, 7.750000000000001776, -5.000000000000000000 ) ) ;
#3421 = DIRECTION ( 'NONE',  ( 1.000000000000000000, -0.000000000000000000, -0.000000000000000000 ) ) ;
#3422 = AXIS2_PLACEMENT_3D ( 'NONE', #30318, #14410, #61419 ) ;
#3423 = EDGE_CURVE ( 'NONE', #23467, #13987, #41157, .T. ) ;
#3424 = DIRECTION ( 'NONE',  ( 1.000000000000000000, -1.088659024508174415E-14, 1.836970198721009966E-16 ) ) ;
#3425 = ORIENTED_EDGE ( 'NONE', *, *, #10973, .F. ) ;
#3426 = FACE_OUTER_BOUND ( 'NONE', #17614, .T. ) ;
#3428 = VECTOR ( 'NONE', #42885, 1000.000000000000000 ) ;
#3427 = CARTESIAN_POINT ( 'NONE',  ( 11.50000000000000000, -11.50000000000000000, 15.00000000000000000 ) ) ;
#3429 = LINE ( 'NONE', #41607, #53628 ) ;
#3430 = EDGE_CURVE ( 'NONE', #58177, #49212, #18750, .T. ) ;
#3431 = CARTESIAN_POINT ( 'NONE',  ( 39.00000000000000000, 14.08845687959340331, 21.00000000000000000 ) ) ;
#3432 = LINE ( 'NONE', #46902, #51843 ) ;
#3433 = FACE_OUTER_BOUND ( 'NONE', #8361, .T. ) ;
#3434 = EDGE_CURVE ( 'NONE', #69122, #11772, #8482, .T. ) ;
#3435 = AXIS2_PLACEMENT_3D ( 'NONE', #14473, #18714, #56545 ) ;
#3436 = TOROIDAL_SURFACE ( 'NONE', #2321, 3.299999999999474909, 0.2000000000005234813 ) ;
#3437 = CARTESIAN_POINT ( 'NONE',  ( 10.50702373788278265, 3.650476262117142934, 54.00000000000000711 ) ) ;
#3438 = ORIENTED_EDGE ( 'NONE', *, *, #49140, .T. ) ;
#3439 = DIRECTION ( 'NONE',  ( -1.000000000000000000, 0.000000000000000000, 0.000000000000000000 ) ) ;
#3440 = EDGE_CURVE ( 'NONE', #58150, #29117, #2141, .T. ) ;
#3441 = CARTESIAN_POINT ( 'NONE',  ( -25.50000000000000355, 0.000000000000000000, 24.12099999999999866 ) ) ;
#3442 = ORIENTED_EDGE ( 'NONE', *, *, #15762, .F. ) ;
#3443 = DIRECTION ( 'NONE',  ( -0.7671651518153087546, -0.6414496315691469164, 2.309356642089053889E-17 ) ) ;
#3444 = PLANE ( 'NONE',  #58361 ) ;
#3445 = LINE ( 'NONE', #46216, #62608 ) ;
#3446 = FILL_AREA_STYLE_COLOUR ( '', #8265 ) ;
#3447 = ADVANCED_FACE ( 'NONE', ( #40667 ), #14143, .F. ) ;
#3448 = LINE ( 'NONE', #13349, #32751 ) ;
#3449 = ORIENTED_EDGE ( 'NONE', *, *, #54668, .T. ) ;
#3450 = DIRECTION ( 'NONE',  ( -1.836970198721029934E-16, 1.836970198721036344E-16, -1.000000000000000000 ) ) ;
#3451 = EDGE_LOOP ( 'NONE', ( #69149, #41449, #59312, #58498 ) ) ;
#3452 = DIRECTION ( 'NONE',  ( 0.000000000000000000, -1.000000000000000000, 0.000000000000000000 ) ) ;
#3453 = CIRCLE ( 'NONE', #42975, 0.5000000000023371305 ) ;
#3454 = CARTESIAN_POINT ( 'NONE',  ( 10.50000000000000000, -9.690000000000001279, -4.250000000000000000 ) ) ;
#3456 = ORIENTED_EDGE ( 'NONE', *, *, #11388, .F. ) ;
#3455 = EDGE_CURVE ( 'NONE', #32370, #69553, #19790, .T. ) ;
#3457 = DIRECTION ( 'NONE',  ( 0.9375000000000006661, 0.000000000000000000, -0.3479852726768744020 ) ) ;
#3458 = ADVANCED_FACE ( 'NONE', ( #35707 ), #61889, .F. ) ;
#3459 = ORIENTED_EDGE ( 'NONE', *, *, #52326, .F. ) ;
#3460 = ADVANCED_FACE ( 'NONE', ( #35342 ), #56238, .F. ) ;
#3461 = ADVANCED_FACE ( 'NONE', ( #18387 ), #67896, .T. ) ;
#3462 = DIRECTION ( 'NONE',  ( -1.000000000000000000, 1.794541526872559352E-16, 0.000000000000000000 ) ) ;
#3463 = EDGE_LOOP ( 'NONE', ( #60874, #36949, #10789, #64791 ) ) ;
#3464 = ORIENTED_EDGE ( 'NONE', *, *, #62935, .T. ) ;
#3465 = CARTESIAN_POINT ( 'NONE',  ( 41.09999999999999432, -14.06939075806900163, 20.80000000000000426 ) ) ;
#3466 = AXIS2_PLACEMENT_3D ( 'NONE', #13833, #35746, #30452 ) ;
#3467 = ORIENTED_EDGE ( 'NONE', *, *, #28860, .T. ) ;
#3468 = ORIENTED_EDGE ( 'NONE', *, *, #50494, .T. ) ;
#3469 = EDGE_CURVE ( 'NONE', #53282, #48333, #29350, .T. ) ;
#3470 = LINE ( 'NONE', #41640, #39481 ) ;
#3471 = CARTESIAN_POINT ( 'NONE',  ( 9.417013320880768035, 1.853252480934615809, 455.0000000000000568 ) ) ;
#3473 = CARTESIAN_POINT ( 'NONE',  ( 6.500000000000000888, -6.500000000000002665, 0.000000000000000000 ) ) ;
#3472 = CIRCLE ( 'NONE', #55406, 1.224999999999998757 ) ;
#3474 = VERTEX_POINT ( 'NONE', #21220 ) ;
#3475 = AXIS2_PLACEMENT_3D ( 'NONE', #51966, #18732, #3529 ) ;
#3476 = DIRECTION ( 'NONE',  ( -1.000000000000000000, 0.000000000000000000, 0.000000000000000000 ) ) ;
#3478 = DIRECTION ( 'NONE',  ( 1.000000000000000000, 0.000000000000000000, 0.000000000000000000 ) ) ;
#3477 = FACE_BOUND ( 'NONE', #33256, .T. ) ;
#3479 = EDGE_LOOP ( 'NONE', ( #24456, #63406, #9131, #37658 ) ) ;
#3481 = ORIENTED_EDGE ( 'NONE', *, *, #4609, .T. ) ;
#3480 = FACE_OUTER_BOUND ( 'NONE', #44384, .T. ) ;
#3482 = ORIENTED_EDGE ( 'NONE', *, *, #23570, .T. ) ;
#3483 = AXIS2_PLACEMENT_3D ( 'NONE', #17526, #1606, #19274 ) ;
#3484 = AXIS2_PLACEMENT_3D ( 'NONE', #16611, #20858, #54435 ) ;
#3485 = CYLINDRICAL_SURFACE ( 'NONE', #29912, 2.458500000000000796 ) ;
#3486 = EDGE_CURVE ( 'NONE', #61959, #17055, #48428, .T. ) ;
#3488 = ORIENTED_EDGE ( 'NONE', *, *, #47137, .T. ) ;
#3487 = CARTESIAN_POINT ( 'NONE',  ( -1.077516549646670541, 11.33351654964656596, 195.0000000000000284 ) ) ;
#3489 = AXIS2_PLACEMENT_3D ( 'NONE', #35172, #13618, #24589 ) ;
#3490 = EDGE_CURVE ( 'NONE', #7275, #44289, #26170, .T. ) ;
#3491 = DIRECTION ( 'NONE',  ( -1.000000000000000000, 0.000000000000000000, 0.000000000000000000 ) ) ;
#3492 = CARTESIAN_POINT ( 'NONE',  ( 39.00000000000000000, -16.96999999999999886, -21.00000000000000000 ) ) ;
#3493 = ORIENTED_EDGE ( 'NONE', *, *, #45198, .F. ) ;
#3494 = ORIENTED_EDGE ( 'NONE', *, *, #61274, .T. ) ;
#3495 = AXIS2_PLACEMENT_3D ( 'NONE', #36380, #10213, #53700 ) ;
#3496 = LINE ( 'NONE', #68552, #42494 ) ;
#3497 = ORIENTED_EDGE ( 'NONE', *, *, #39576, .F. ) ;
#3498 = DIRECTION ( 'NONE',  ( -1.000000000000000000, 0.000000000000000000, 0.000000000000000000 ) ) ;
#3499 = DIRECTION ( 'NONE',  ( 0.000000000000000000, 0.000000000000000000, -1.000000000000000000 ) ) ;
#3500 = CARTESIAN_POINT ( 'NONE',  ( -15.50000000000000000, -5.000000000000000000, -22.50000000000000000 ) ) ;
#3501 = EDGE_LOOP ( 'NONE', ( #50528, #8821, #8600, #31541, #54176, #52794 ) ) ;
#3502 = PLANE ( 'NONE',  #8712 ) ;
#3503 = DIRECTION ( 'NONE',  ( -0.7071067811865446862, -0.7071067811865503483, -0.000000000000000000 ) ) ;
#3505 = EDGE_LOOP ( 'NONE', ( #52893, #35686, #40265, #27042, #44988, #7102, #57814, #55494, #69032, #68711, #23358, #61982, #3569, #22742, #29398, #40872, #51710 ) ) ;
#3504 = FACE_OUTER_BOUND ( 'NONE', #69071, .T. ) ;
#3507 = ORIENTED_EDGE ( 'NONE', *, *, #58339, .T. ) ;
#3506 = LINE ( 'NONE', #39913, #472 ) ;
#3508 = LINE ( 'NONE', #45573, #46427 ) ;
#3509 = EDGE_CURVE ( 'NONE', #4816, #36688, #544, .T. ) ;
#3510 = DIRECTION ( 'NONE',  ( -1.000000000000000000, 5.626525616968433120E-15, 0.000000000000000000 ) ) ;
#3511 = CARTESIAN_POINT ( 'NONE',  ( 9.929523737882748335, 0.9414762621171531842, 26.00000000000000711 ) ) ;
#3512 = CARTESIAN_POINT ( 'NONE',  ( 4.186483450353335023, -12.00648345035347830, 455.0000000000000568 ) ) ;
#3513 = CARTESIAN_POINT ( 'NONE',  ( 11.12648345035337982, 4.193516549646526315, 455.0000000000000568 ) ) ;
#3514 = VERTEX_POINT ( 'NONE', #40360 ) ;
#3515 = CARTESIAN_POINT ( 'NONE',  ( 4.396432944014530442, 8.593516549646635028, 195.0000000000000284 ) ) ;
#3516 = LINE ( 'NONE', #46639, #13510 ) ;
#3517 = VECTOR ( 'NONE', #19741, 1000.000000000000000 ) ;
#3518 = EDGE_CURVE ( 'NONE', #24611, #26279, #6193, .T. ) ;
#3520 = VERTEX_POINT ( 'NONE', #42769 ) ;
#3519 = LINE ( 'NONE', #67868, #25490 ) ;
#3521 = VECTOR ( 'NONE', #55241, 1000.000000000000000 ) ;
#3522 = LINE ( 'NONE', #9525, #57261 ) ;
#3523 = CARTESIAN_POINT ( 'NONE',  ( -9.547976262117254365, 8.130476262117182884, 26.00000000000000711 ) ) ;
#3525 = ADVANCED_FACE ( 'NONE', ( #5308 ), #28733, .F. ) ;
#3524 = CIRCLE ( 'NONE', #42988, 0.5250000000000003553 ) ;
#3526 = EDGE_LOOP ( 'NONE', ( #10495, #65986, #69084, #16453 ) ) ;
#3527 = DIRECTION ( 'NONE',  ( -3.491481338843133355E-15, -1.000000000000000000, -1.836970198721029934E-16 ) ) ;
#3528 = EDGE_CURVE ( 'NONE', #36748, #48159, #15236, .T. ) ;
#3529 = DIRECTION ( 'NONE',  ( -1.000000000000000000, 0.000000000000000000, 0.000000000000000000 ) ) ;
#3530 = ADVANCED_FACE ( 'NONE', ( #52336 ), #53048, .T. ) ;
#3531 = ORIENTED_EDGE ( 'NONE', *, *, #54033, .F. ) ;
#3532 = VECTOR ( 'NONE', #22074, 1000.000000000000000 ) ;
#3533 = CONICAL_SURFACE ( 'NONE', #5812, 1.621000000000000885, 0.7853981633974518317 ) ;
#3534 = DIRECTION ( 'NONE',  ( 0.000000000000000000, 3.673940397442059868E-16, -1.000000000000000000 ) ) ;
#3535 = DIRECTION ( 'NONE',  ( -0.000000000000000000, 0.000000000000000000, -1.000000000000000000 ) ) ;
#3536 = EDGE_CURVE ( 'NONE', #30152, #40696, #20853, .T. ) ;
#3537 = EDGE_CURVE ( 'NONE', #32501, #53195, #14049, .T. ) ;
#3538 = CARTESIAN_POINT ( 'NONE',  ( 7.250000000000005329, -7.249999999999998224, -16.50000000000000000 ) ) ;
#3539 = AXIS2_PLACEMENT_3D ( 'NONE', #3985, #58442, #30499 ) ;
#3540 = DIRECTION ( 'NONE',  ( 1.000000000000000000, -0.000000000000000000, -0.000000000000000000 ) ) ;
#3541 = CIRCLE ( 'NONE', #52093, 2.000000000000001776 ) ;
#3542 = ORIENTED_EDGE ( 'NONE', *, *, #24613, .F. ) ;
#3543 = CARTESIAN_POINT ( 'NONE',  ( 30.00000000000000000, -5.599999999999999645, 9.000000000000001776 ) ) ;
#3544 = ORIENTED_EDGE ( 'NONE', *, *, #2138, .T. ) ;
#3545 = VERTEX_POINT ( 'NONE', #36782 ) ;
#3546 = ORIENTED_EDGE ( 'NONE', *, *, #24130, .F. ) ;
#3547 = DIRECTION ( 'NONE',  ( 0.000000000000000000, 1.000000000000000000, 0.000000000000000000 ) ) ;
#3548 = CIRCLE ( 'NONE', #48718, 0.2000000000000005107 ) ;
#3549 = CARTESIAN_POINT ( 'NONE',  ( 39.90000000000000568, 16.96999999999999886, 21.00000000000000000 ) ) ;
#3550 = CARTESIAN_POINT ( 'NONE',  ( -1.077516549646670541, 11.33351654964656596, 455.0000000000000568 ) ) ;
#3551 = VERTEX_POINT ( 'NONE', #58354 ) ;
#3552 = EDGE_LOOP ( 'NONE', ( #16167, #31327, #33798, #441 ) ) ;
#3553 = DIRECTION ( 'NONE',  ( 1.000000000000000000, 0.000000000000000000, 0.000000000000000000 ) ) ;
#3554 = EDGE_LOOP ( 'NONE', ( #19642, #44567, #61700, #49917 ) ) ;
#3555 = EDGE_LOOP ( 'NONE', ( #29131, #48787, #32367, #5146 ) ) ;
#3556 = FACE_OUTER_BOUND ( 'NONE', #15906, .T. ) ;
#3557 = DIRECTION ( 'NONE',  ( -0.000000000000000000, 3.673940397442059868E-16, -1.000000000000000000 ) ) ;
#3558 = DIRECTION ( 'NONE',  ( 0.000000000000000000, -1.000000000000000000, 0.000000000000000000 ) ) ;
#3559 = AXIS2_PLACEMENT_3D ( 'NONE', #54291, #5849, #21760 ) ;
#3560 = DIRECTION ( 'NONE',  ( -1.836970198721029934E-16, -1.836970198721010706E-16, 1.000000000000000000 ) ) ;
#3561 = ORIENTED_EDGE ( 'NONE', *, *, #66313, .F. ) ;
#3562 = CARTESIAN_POINT ( 'NONE',  ( 7.606483450353420217, 11.31351654964657349, 455.0000000000000568 ) ) ;
#3564 = DIRECTION ( 'NONE',  ( 0.000000000000000000, 0.000000000000000000, 1.000000000000000000 ) ) ;
#3563 = DIRECTION ( 'NONE',  ( -1.794541526872559352E-16, -1.000000000000000000, 0.000000000000000000 ) ) ;
#3565 = ORIENTED_EDGE ( 'NONE', *, *, #35368, .T. ) ;
#3567 = ORIENTED_EDGE ( 'NONE', *, *, #20849, .T. ) ;
#3566 = FACE_OUTER_BOUND ( 'NONE', #31041, .T. ) ;
#3568 = EDGE_LOOP ( 'NONE', ( #64677, #30089, #9976, #16076 ) ) ;
#3569 = ORIENTED_EDGE ( 'NONE', *, *, #37008, .T. ) ;
#3570 = DIRECTION ( 'NONE',  ( -1.000000000000000000, 0.000000000000000000, 0.000000000000000000 ) ) ;
#3571 = VECTOR ( 'NONE', #17072, 1000.000000000000000 ) ;
#3572 = EDGE_CURVE ( 'NONE', #7104, #67892, #25823, .T. ) ;
#3573 = CARTESIAN_POINT ( 'NONE',  ( 10.92648345035336277, 2.893516549646527825, 455.0000000000000568 ) ) ;
#3574 = AXIS2_PLACEMENT_3D ( 'NONE', #56195, #7741, #2445 ) ;
#3575 = ORIENTED_EDGE ( 'NONE', *, *, #66520, .T. ) ;
#3576 = ORIENTED_EDGE ( 'NONE', *, *, #62843, .F. ) ;
#3577 = ADVANCED_FACE ( 'NONE', ( #9203, #25464 ), #42422, .T. ) ;
#3578 = DIRECTION ( 'NONE',  ( 1.000000000000000000, -1.047444401652940007E-14, 1.836970198721010706E-16 ) ) ;
#3579 = PLANE ( 'NONE',  #5205 ) ;
#3580 = ORIENTED_EDGE ( 'NONE', *, *, #28905, .T. ) ;
#3581 = AXIS2_PLACEMENT_3D ( 'NONE', #32433, #68861, #42328 ) ;
#3582 = CLOSED_SHELL ( 'NONE', ( #40542, #64342, #11733, #10084, #58799, #54196, #14833, #66593, #59238, #46770 ) ) ;
#3583 = ORIENTED_EDGE ( 'NONE', *, *, #49603, .T. ) ;
#3584 = LINE ( 'NONE', #13477, #42106 ) ;
#3585 = FACE_OUTER_BOUND ( 'NONE', #30082, .T. ) ;
#3586 = ORIENTED_EDGE ( 'NONE', *, *, #6130, .T. ) ;
#3587 = CIRCLE ( 'NONE', #12587, 1.000000000000000000 ) ;
#3588 = LINE ( 'NONE', #4983, #38010 ) ;
#3589 = CARTESIAN_POINT ( 'NONE',  ( 146.5599459900709860, 9.000000000000001776, 280.7801873289890295 ) ) ;
#3591 = VERTEX_POINT ( 'NONE', #48080 ) ;
#3590 = CARTESIAN_POINT ( 'NONE',  ( 0.000000000000000000, -7.449999999999998401, -15.50000000000000000 ) ) ;
#3592 = ORIENTED_EDGE ( 'NONE', *, *, #9385, .T. ) ;
#3594 = LINE ( 'NONE', #46364, #7930 ) ;
#3593 = VECTOR ( 'NONE', #52772, 1000.000000000000114 ) ;
#3595 = DIRECTION ( 'NONE',  ( 0.000000000000000000, -3.673940397442059868E-16, 1.000000000000000000 ) ) ;
#3596 = DIRECTION ( 'NONE',  ( -1.836970198721029934E-16, 1.836970198721036344E-16, -1.000000000000000000 ) ) ;
#3597 = CARTESIAN_POINT ( 'NONE',  ( -30.00000000000000000, -5.200000000000001066, -9.400000000000000355 ) ) ;
#3598 = CARTESIAN_POINT ( 'NONE',  ( 29.89999999999999858, -0.000000000000000000, -20.80000000000000071 ) ) ;
#3599 = CARTESIAN_POINT ( 'NONE',  ( -7.250000000000000888, 7.250000000000001776, -26.00000000000001066 ) ) ;
#3600 = ORIENTED_EDGE ( 'NONE', *, *, #3776, .F. ) ;
#3601 = CARTESIAN_POINT ( 'NONE',  ( 8.250000000000005329, -7.249999999999998224, -26.00000000000001066 ) ) ;
#3603 = ORIENTED_EDGE ( 'NONE', *, *, #66111, .T. ) ;
#3602 = DIRECTION ( 'NONE',  ( -1.000000000000000000, 0.000000000000000000, 0.000000000000000000 ) ) ;
#3604 = ADVANCED_FACE ( 'NONE', ( #69659 ), #20158, .F. ) ;
#3605 = DIRECTION ( 'NONE',  ( -0.8660254037844485886, 0.000000000000000000, -0.4999999999999827360 ) ) ;
#3606 = LINE ( 'NONE', #14555, #28987 ) ;
#3607 = AXIS2_PLACEMENT_3D ( 'NONE', #56709, #29833, #2970 ) ;
#3608 = DIRECTION ( 'NONE',  ( -1.000000000000000000, 0.000000000000000000, 0.000000000000000000 ) ) ;
#3609 = EDGE_CURVE ( 'NONE', #11215, #21581, #16340, .T. ) ;
#3610 = ORIENTED_EDGE ( 'NONE', *, *, #62298, .F. ) ;
#3611 = LINE ( 'NONE', #1259, #55065 ) ;
#3612 = EDGE_CURVE ( 'NONE', #18662, #27404, #52484, .T. ) ;
#3613 = DIRECTION ( 'NONE',  ( -1.000000000000000000, 0.000000000000000000, 0.000000000000000000 ) ) ;
#3614 = EDGE_CURVE ( 'NONE', #43972, #62304, #23133, .T. ) ;
#3615 = ORIENTED_EDGE ( 'NONE', *, *, #46826, .F. ) ;
#3616 = PLANE ( 'NONE',  #58297 ) ;
#3617 = DIRECTION ( 'NONE',  ( 0.000000000000000000, 0.000000000000000000, -1.000000000000000000 ) ) ;
#3618 = ADVANCED_FACE ( 'NONE', ( #4263 ), #63652, .T. ) ;
#3619 = EDGE_CURVE ( 'NONE', #36815, #35302, #5091, .T. ) ;
#3620 = VECTOR ( 'NONE', #24809, 1000.000000000000000 ) ;
#3621 = DIRECTION ( 'NONE',  ( -0.6414496315691420314, 0.7671651518153128624, 2.587583378555127804E-16 ) ) ;
#3622 = EDGE_CURVE ( 'NONE', #15670, #38025, #33193, .T. ) ;
#3623 = EDGE_LOOP ( 'NONE', ( #63033, #36895, #20347, #67571 ) ) ;
#3624 = DIRECTION ( 'NONE',  ( 1.000000000000000000, 0.000000000000000000, 0.000000000000000000 ) ) ;
#3625 = EDGE_LOOP ( 'NONE', ( #26612, #20607, #510, #68968 ) ) ;
#3626 = VERTEX_POINT ( 'NONE', #50144 ) ;
#3627 = LINE ( 'NONE', #40748, #20027 ) ;
#3628 = PLANE ( 'NONE',  #12760 ) ;
#3629 = CARTESIAN_POINT ( 'NONE',  ( -8.250000000000001776, 7.250000000000000888, -23.50000000000000000 ) ) ;
#3630 = VECTOR ( 'NONE', #21031, 1000.000000000000000 ) ;
#3631 = CARTESIAN_POINT ( 'NONE',  ( -3.650476262117223314, 10.30047626211716683, 26.00000000000000711 ) ) ;
#3632 = CARTESIAN_POINT ( 'NONE',  ( -7.603567055985586798, -8.406483450353363196, 195.0000000000000284 ) ) ;
#3633 = ORIENTED_EDGE ( 'NONE', *, *, #37832, .F. ) ;
#3634 = ORIENTED_EDGE ( 'NONE', *, *, #44778, .F. ) ;
#3636 = ORIENTED_EDGE ( 'NONE', *, *, #39034, .T. ) ;
#3635 = DIRECTION ( 'NONE',  ( 1.000000000000000000, 0.000000000000000000, 0.000000000000000000 ) ) ;
#3637 = AXIS2_PLACEMENT_3D ( 'NONE', #50835, #67105, #45529 ) ;
#3638 = ORIENTED_EDGE ( 'NONE', *, *, #55636, .T. ) ;
#3639 = CARTESIAN_POINT ( 'NONE',  ( 41.09999999999999432, 21.00000000000000000, 13.98999642601811999 ) ) ;
#3640 = DIRECTION ( 'NONE',  ( -1.000000000000000000, 0.000000000000000000, 0.000000000000000000 ) ) ;
#3641 = CARTESIAN_POINT ( 'NONE',  ( -5.993516549646776603, -6.006483450353426790, 455.0000000000000568 ) ) ;
#3642 = FACE_BOUND ( 'NONE', #3505, .T. ) ;
#3643 = AXIS2_PLACEMENT_3D ( 'NONE', #659, #33172, #27875 ) ;
#3644 = DIRECTION ( 'NONE',  ( 0.000000000000000000, 1.000000000000000000, 0.000000000000000000 ) ) ;
#3645 = CARTESIAN_POINT ( 'NONE',  ( -7.605476262117258024, 9.722976262117178692, 26.00000000000000711 ) ) ;
#3646 = ORIENTED_EDGE ( 'NONE', *, *, #28667, .F. ) ;
#3647 = VERTEX_POINT ( 'NONE', #44145 ) ;
#3648 = ORIENTED_EDGE ( 'NONE', *, *, #68475, .F. ) ;
#3649 = ORIENTED_EDGE ( 'NONE', *, *, #66500, .T. ) ;
#3650 = DIRECTION ( 'NONE',  ( 0.000000000000000000, 0.000000000000000000, 1.000000000000000000 ) ) ;
#3651 = DIRECTION ( 'NONE',  ( 1.000000000000000000, -0.000000000000000000, 0.000000000000000000 ) ) ;
#3652 =( NAMED_UNIT ( * ) PLANE_ANGLE_UNIT ( ) SI_UNIT ( $, .RADIAN. ) );
#3653 = DIRECTION ( 'NONE',  ( 0.000000000000000000, -1.000000000000000000, -0.000000000000000000 ) ) ;
#3654 = ORIENTED_EDGE ( 'NONE', *, *, #3793, .T. ) ;
#3655 = ORIENTED_EDGE ( 'NONE', *, *, #40229, .F. ) ;
#3656 = VERTEX_POINT ( 'NONE', #10943 ) ;
#3657 = ADVANCED_FACE ( 'NONE', ( #7001 ), #43813, .T. ) ;
#3658 = ADVANCED_FACE ( 'NONE', ( #60402 ), #28233, .F. ) ;
#3659 = EDGE_CURVE ( 'NONE', #32467, #18730, #38514, .T. ) ;
#3660 = DIRECTION ( 'NONE',  ( 1.011922027653139155E-14, 1.000000000000000000, 0.000000000000000000 ) ) ;
#3661 = EDGE_LOOP ( 'NONE', ( #22537, #17400, #69287, #31174 ) ) ;
#3662 = ORIENTED_EDGE ( 'NONE', *, *, #33384, .T. ) ;
#3663 = DIRECTION ( 'NONE',  ( 0.000000000000000000, 0.000000000000000000, 1.000000000000000000 ) ) ;
#3664 = EDGE_CURVE ( 'NONE', #41185, #51551, #8435, .T. ) ;
#3665 = ORIENTED_EDGE ( 'NONE', *, *, #21227, .T. ) ;
#3666 = ORIENTED_EDGE ( 'NONE', *, *, #36786, .F. ) ;
#3667 = CARTESIAN_POINT ( 'NONE',  ( 9.690000000000001279, 10.50000000000000000, -5.000000000000000000 ) ) ;
#3668 = CIRCLE ( 'NONE', #58986, 5.000000000000000000 ) ;
#3670 = ORIENTED_EDGE ( 'NONE', *, *, #42572, .T. ) ;
#3669 = DIRECTION ( 'NONE',  ( -1.836970198721029934E-16, 1.836970198721036344E-16, -1.000000000000000000 ) ) ;
#3671 = VERTEX_POINT ( 'NONE', #22589 ) ;
#3672 = CARTESIAN_POINT ( 'NONE',  ( -9.547976262117300550, -8.144523737882753522, 26.00000000000000000 ) ) ;
#3673 = CARTESIAN_POINT ( 'NONE',  ( 275.0000000000000000, -23.50007830495750127, 12.58007262201399890 ) ) ;
#3674 = DIRECTION ( 'NONE',  ( -1.000000000000000000, 0.000000000000000000, 0.000000000000000000 ) ) ;
#3676 = VERTEX_POINT ( 'NONE', #54432 ) ;
#3675 = CARTESIAN_POINT ( 'NONE',  ( -7.259684009079930611, 7.798499376343971612, 455.0000000000000568 ) ) ;
#3677 = ORIENTED_EDGE ( 'NONE', *, *, #60020, .F. ) ;
#3678 = CARTESIAN_POINT ( 'NONE',  ( 289.5000000000001705, -42.50000000000007105, -26.49999999999997158 ) ) ;
#3679 = DIRECTION ( 'NONE',  ( 0.000000000000000000, -1.000000000000000000, 0.000000000000000000 ) ) ;
#3680 = AXIS2_PLACEMENT_3D ( 'NONE', #27732, #890, #38685 ) ;
#3681 = DIRECTION ( 'NONE',  ( 1.836970198721029934E-16, -1.836970198721036344E-16, 1.000000000000000000 ) ) ;
#3682 = CARTESIAN_POINT ( 'NONE',  ( 11.90000000000000036, -0.2000000000089119934, 8.909539772616881237E-12 ) ) ;
#3683 = ORIENTED_EDGE ( 'NONE', *, *, #63341, .T. ) ;
#3684 = CARTESIAN_POINT ( 'NONE',  ( 35.89999999999999858, 3.010794155703768650E-16, -2.458500000000000796 ) ) ;
#3685 = DIRECTION ( 'NONE',  ( 0.000000000000000000, 1.000000000000000000, 0.000000000000000000 ) ) ;
#3686 = VECTOR ( 'NONE', #21728, 1000.000000000000114 ) ;
#3687 = ORIENTED_EDGE ( 'NONE', *, *, #48386, .F. ) ;
#3688 = FACE_OUTER_BOUND ( 'NONE', #61355, .T. ) ;
#3690 = CARTESIAN_POINT ( 'NONE',  ( 105.8309041053263257, 61.65740854044500452, 2.000000000000000000 ) ) ;
#3689 = CIRCLE ( 'NONE', #66911, 0.1999999999999996503 ) ;
#3691 = VECTOR ( 'NONE', #57312, 1000.000000000000000 ) ;
#3692 = CARTESIAN_POINT ( 'NONE',  ( 17.51999999999999957, -15.50000000000000000, -26.00000000000000355 ) ) ;
#3693 = ORIENTED_EDGE ( 'NONE', *, *, #48923, .F. ) ;
#3694 = DIRECTION ( 'NONE',  ( 1.000000000000000000, -0.000000000000000000, -0.000000000000000000 ) ) ;
#3695 = VECTOR ( 'NONE', #64312, 1000.000000000000000 ) ;
#3696 = DIRECTION ( 'NONE',  ( -1.000000000000000000, 0.000000000000000000, 0.000000000000000000 ) ) ;
#3697 = ADVANCED_FACE ( 'NONE', ( #688 ), #11955, .F. ) ;
#3698 = EDGE_CURVE ( 'NONE', #1302, #63520, #69438, .T. ) ;
#3699 = CARTESIAN_POINT ( 'NONE',  ( 283.0000000000000568, -31.30000000000000071, -12.69999999999999929 ) ) ;
#3700 = VERTEX_POINT ( 'NONE', #27900 ) ;
#3701 = CYLINDRICAL_SURFACE ( 'NONE', #24787, 0.4999999999945534124 ) ;
#3702 = DIRECTION ( 'NONE',  ( 0.000000000000000000, 1.000000000000000000, 0.000000000000000000 ) ) ;
#3703 = ADVANCED_FACE ( 'NONE', ( #22254 ), #335, .F. ) ;
#3704 = DIRECTION ( 'NONE',  ( 0.000000000000000000, 0.000000000000000000, 1.000000000000000000 ) ) ;
#3705 = FACE_OUTER_BOUND ( 'NONE', #11044, .T. ) ;
#3706 = CARTESIAN_POINT ( 'NONE',  ( 7.250000000000004441, 7.450000000000001954, -10.50000000000000000 ) ) ;
#3707 = ORIENTED_EDGE ( 'NONE', *, *, #10214, .F. ) ;
#3708 = DIRECTION ( 'NONE',  ( 0.000000000000000000, 1.000000000000000000, 0.000000000000000000 ) ) ;
#3709 = DIRECTION ( 'NONE',  ( -1.000000000000000000, 0.000000000000000000, 0.000000000000000000 ) ) ;
#3710 = EDGE_CURVE ( 'NONE', #8669, #66944, #38839, .T. ) ;
#3711 = VECTOR ( 'NONE', #4679, 1000.000000000000000 ) ;
#3712 = CARTESIAN_POINT ( 'NONE',  ( -7.250000000000000888, -8.249999999999998224, -12.50000000000000000 ) ) ;
#3713 = CARTESIAN_POINT ( 'NONE',  ( -9.093516549646711411, 10.08346604330776941, 455.0000000000000568 ) ) ;
#3714 = ADVANCED_FACE ( 'NONE', ( #28573 ), #27546, .F. ) ;
#3715 = LINE ( 'NONE', #53559, #19271 ) ;
#3716 = VECTOR ( 'NONE', #40186, 1000.000000000000000 ) ;
#3717 = ORIENTED_EDGE ( 'NONE', *, *, #64847, .T. ) ;
#3719 = EDGE_LOOP ( 'NONE', ( #20012, #42351, #27753, #59783, #45690, #7277, #18294, #48856 ) ) ;
#3718 = DIRECTION ( 'NONE',  ( 1.000000000000000000, 0.000000000000000000, 0.000000000000000000 ) ) ;
#3720 = EDGE_CURVE ( 'NONE', #29410, #14602, #11612, .T. ) ;
#3721 = DIRECTION ( 'NONE',  ( 0.000000000000000000, -1.000000000000000000, 3.989863994748342081E-13 ) ) ;
#3722 = FACE_OUTER_BOUND ( 'NONE', #15976, .T. ) ;
#3723 = DIRECTION ( 'NONE',  ( -0.000000000000000000, 1.000000000000000000, -0.000000000000000000 ) ) ;
#3724 = ORIENTED_EDGE ( 'NONE', *, *, #56640, .F. ) ;
#3725 = LINE ( 'NONE', #36594, #8094 ) ;
#3726 = ORIENTED_EDGE ( 'NONE', *, *, #37311, .F. ) ;
#3727 = ORIENTED_EDGE ( 'NONE', *, *, #15369, .T. ) ;
#3728 = VERTEX_POINT ( 'NONE', #32856 ) ;
#3729 = DIRECTION ( 'NONE',  ( -1.000000000000000000, 0.000000000000000000, 0.000000000000000000 ) ) ;
#3730 = CARTESIAN_POINT ( 'NONE',  ( 283.0000000000000568, -40.30000000000000426, -12.20000000000000107 ) ) ;
#3731 = FACE_OUTER_BOUND ( 'NONE', #5062, .T. ) ;
#3732 = VERTEX_POINT ( 'NONE', #54772 ) ;
#3733 = ORIENTED_EDGE ( 'NONE', *, *, #55453, .T. ) ;
#3734 = DIRECTION ( 'NONE',  ( 0.7671651518152963201, 0.6414496315691619044, 2.356647714346269747E-16 ) ) ;
#3735 = AXIS2_PLACEMENT_3D ( 'NONE', #17345, #28646, #34288 ) ;
#3736 = CARTESIAN_POINT ( 'NONE',  ( -11.50000000000000000, -11.70000000000000284, -11.00000000000000000 ) ) ;
#3737 = ORIENTED_EDGE ( 'NONE', *, *, #11898, .F. ) ;
#3738 = MECHANICAL_DESIGN_GEOMETRIC_PRESENTATION_REPRESENTATION (  '', ( #22908 ), #57942 ) ;
#3739 = ORIENTED_EDGE ( 'NONE', *, *, #24449, .T. ) ;
#3740 = ADVANCED_FACE ( 'NONE', ( #1368 ), #39193, .T. ) ;
#3741 = ORIENTED_EDGE ( 'NONE', *, *, #19407, .F. ) ;
#3742 = ORIENTED_EDGE ( 'NONE', *, *, #25915, .F. ) ;
#3743 = LINE ( 'NONE', #68456, #51962 ) ;
#3744 = CIRCLE ( 'NONE', #15058, 4.000000000000000888 ) ;
#3746 = ORIENTED_EDGE ( 'NONE', *, *, #37832, .T. ) ;
#3745 = CARTESIAN_POINT ( 'NONE',  ( 41.09999999999999432, 13.66939075806899950, 20.80000000000000426 ) ) ;
#3747 = DIRECTION ( 'NONE',  ( 0.000000000000000000, 0.000000000000000000, -1.000000000000000000 ) ) ;
#3748 = DIRECTION ( 'NONE',  ( 1.000000000000000000, -0.000000000000000000, 0.000000000000000000 ) ) ;
#3749 = ORIENTED_EDGE ( 'NONE', *, *, #32880, .F. ) ;
#3750 = ORIENTED_EDGE ( 'NONE', *, *, #9607, .F. ) ;
#3751 = EDGE_CURVE ( 'NONE', #28596, #9113, #60752, .T. ) ;
#3752 = AXIS2_PLACEMENT_3D ( 'NONE', #58775, #5024, #54516 ) ;
#3753 = DIRECTION ( 'NONE',  ( 0.4999999999999786282, -0.8660254037844510311, 0.000000000000000000 ) ) ;
#3754 = EDGE_CURVE ( 'NONE', #48682, #34666, #54876, .T. ) ;
#3755 = VECTOR ( 'NONE', #66982, 1000.000000000000000 ) ;
#3756 = FACE_OUTER_BOUND ( 'NONE', #23093, .T. ) ;
#3757 = VERTEX_POINT ( 'NONE', #35616 ) ;
#3758 = FACE_OUTER_BOUND ( 'NONE', #61316, .T. ) ;
#3759 = DIRECTION ( 'NONE',  ( 0.000000000000000000, 0.000000000000000000, -1.000000000000000000 ) ) ;
#3760 = DIRECTION ( 'NONE',  ( 0.000000000000000000, -0.1111111111108840643, -0.9938079899999319178 ) ) ;
#3761 = ORIENTED_EDGE ( 'NONE', *, *, #62597, .F. ) ;
#3762 = AXIS2_PLACEMENT_3D ( 'NONE', #49136, #10962, #60082 ) ;
#3763 = CARTESIAN_POINT ( 'NONE',  ( 7.000000000000000000, -38.64999999999999858, 15.00000000000000000 ) ) ;
#3764 = DIRECTION ( 'NONE',  ( -0.7671651518153028704, -0.6414496315691537998, -2.587583378555113506E-16 ) ) ;
#3765 = LINE ( 'NONE', #46191, #28524 ) ;
#3766 = CARTESIAN_POINT ( 'NONE',  ( 7.250000000000005329, -8.249999999999998224, -18.00000000000000000 ) ) ;
#3767 = EDGE_CURVE ( 'NONE', #33875, #43298, #46234, .T. ) ;
#3768 = DIRECTION ( 'NONE',  ( -1.000000000000000000, -1.671920889371702854E-15, -0.000000000000000000 ) ) ;
#3769 = EDGE_LOOP ( 'NONE', ( #26954, #2399, #45318, #68730 ) ) ;
#3770 = CYLINDRICAL_SURFACE ( 'NONE', #5363, 4.000000000000000000 ) ;
#3771 = DIRECTION ( 'NONE',  ( 1.000000000000000000, -0.000000000000000000, 0.000000000000000000 ) ) ;
#3772 = CARTESIAN_POINT ( 'NONE',  ( 20.90000000000000213, -21.00000000000000000, 13.86939075806900057 ) ) ;
#3773 = CARTESIAN_POINT ( 'NONE',  ( 9.562023737882805463, 8.130476262117184660, 54.00000000000000711 ) ) ;
#3774 = CIRCLE ( 'NONE', #59104, 24.99999999998784972 ) ;
#3775 = VECTOR ( 'NONE', #68253, 1000.000000000000000 ) ;
#3776 = EDGE_CURVE ( 'NONE', #28873, #9556, #39867, .T. ) ;
#3777 = DIRECTION ( 'NONE',  ( 0.000000000000000000, 0.000000000000000000, 1.000000000000000000 ) ) ;
#3778 = CARTESIAN_POINT ( 'NONE',  ( -11.00000000000000000, -5.599999999999999645, 27.00000000000000000 ) ) ;
#3779 = AXIS2_PLACEMENT_3D ( 'NONE', #28224, #29250, #2049 ) ;
#3780 = FACE_OUTER_BOUND ( 'NONE', #37420, .T. ) ;
#3781 = DIRECTION ( 'NONE',  ( -1.203165845134433242E-14, -1.000000000000000000, -1.836970198721014403E-16 ) ) ;
#3782 = ORIENTED_EDGE ( 'NONE', *, *, #46884, .F. ) ;
#3783 = CIRCLE ( 'NONE', #33155, 1.224999999999998757 ) ;
#3784 = PLANE ( 'NONE',  #8400 ) ;
#3785 = DIRECTION ( 'NONE',  ( 1.000000000000000000, 0.000000000000000000, 0.000000000000000000 ) ) ;
#3786 = VERTEX_POINT ( 'NONE', #57198 ) ;
#3787 = DIRECTION ( 'NONE',  ( 1.000000000000000000, -5.981805089575194965E-17, 0.000000000000000000 ) ) ;
#3788 = FACE_OUTER_BOUND ( 'NONE', #14959, .T. ) ;
#3789 = LINE ( 'NONE', #36313, #55849 ) ;
#3790 = VECTOR ( 'NONE', #48729, 1000.000000000000000 ) ;
#3792 = AXIS2_PLACEMENT_3D ( 'NONE', #23738, #28343, #39976 ) ;
#3791 = CARTESIAN_POINT ( 'NONE',  ( -3.593516549646701197, 7.415254214038210279, 195.0000000000000284 ) ) ;
#3793 = EDGE_CURVE ( 'NONE', #44814, #28277, #8761, .T. ) ;
#3794 = CYLINDRICAL_SURFACE ( 'NONE', #39545, 2.250000000000001776 ) ;
#3795 = ORIENTED_EDGE ( 'NONE', *, *, #51195, .F. ) ;
#3796 = ADVANCED_FACE ( 'NONE', ( #67470 ), #45884, .F. ) ;
#3797 = LINE ( 'NONE', #9374, #8204 ) ;
#3798 = VERTEX_POINT ( 'NONE', #34913 ) ;
#3799 = CARTESIAN_POINT ( 'NONE',  ( 9.900000000000000355, -21.00000000000000000, -18.00000000000000355 ) ) ;
#3800 = DIRECTION ( 'NONE',  ( 1.000000000000000000, 0.000000000000000000, 0.000000000000000000 ) ) ;
#3801 = ORIENTED_EDGE ( 'NONE', *, *, #39425, .F. ) ;
#3802 = FACE_OUTER_BOUND ( 'NONE', #3552, .T. ) ;
#3803 = CARTESIAN_POINT ( 'NONE',  ( 275.0000000000000000, -37.15000000000001279, -7.700000000000000178 ) ) ;
#3804 = EDGE_CURVE ( 'NONE', #1760, #37044, #30020, .T. ) ;
#3805 = ORIENTED_EDGE ( 'NONE', *, *, #30524, .F. ) ;
#3806 = LINE ( 'NONE', #21123, #37921 ) ;
#3807 = ORIENTED_EDGE ( 'NONE', *, *, #24948, .T. ) ;
#3808 = ORIENTED_EDGE ( 'NONE', *, *, #33309, .F. ) ;
#3809 = DIRECTION ( 'NONE',  ( 1.000000000000000000, 0.000000000000000000, 0.000000000000000000 ) ) ;
#3810 = ORIENTED_EDGE ( 'NONE', *, *, #60185, .T. ) ;
#3811 = VERTEX_POINT ( 'NONE', #17960 ) ;
#3812 = CARTESIAN_POINT ( 'NONE',  ( 11.50000000000000000, -11.50000000000100009, -15.00000000000084910 ) ) ;
#3813 = DIRECTION ( 'NONE',  ( 1.836970198721029934E-16, 1.836970198721010706E-16, -1.000000000000000000 ) ) ;
#3814 = CARTESIAN_POINT ( 'NONE',  ( 0.000000000000000000, 8.750000000000001776, -26.00000000000001066 ) ) ;
#3815 = ADVANCED_FACE ( 'NONE', ( #39525 ), #56493, .F. ) ;
#3816 = VERTEX_POINT ( 'NONE', #61807 ) ;
#3817 = CARTESIAN_POINT ( 'NONE',  ( 39.90000000000000568, 20.60000000000000142, 3.447897592003593022E-15 ) ) ;
#3819 = DIRECTION ( 'NONE',  ( -1.836970198721029934E-16, 1.836970198721036590E-16, -1.000000000000000000 ) ) ;
#3818 = PLANE ( 'NONE',  #29311 ) ;
#3820 = ORIENTED_EDGE ( 'NONE', *, *, #42974, .F. ) ;
#3822 = ORIENTED_EDGE ( 'NONE', *, *, #33697, .F. ) ;
#3821 = CARTESIAN_POINT ( 'NONE',  ( 0.000000000000000000, -8.249999999999998224, -11.50000000000000000 ) ) ;
#3823 = VERTEX_POINT ( 'NONE', #51901 ) ;
#3824 = EDGE_CURVE ( 'NONE', #47349, #28596, #26606, .T. ) ;
#3825 = PRODUCT_CONTEXT ( 'NONE', #11498, 'mechanical' ) ;
#3826 = LINE ( 'NONE', #14795, #33312 ) ;
#3828 = VERTEX_POINT ( 'NONE', #45172 ) ;
#3827 = DIRECTION ( 'NONE',  ( -6.308085367188448025E-15, -1.000000000000000000, 0.000000000000000000 ) ) ;
#3829 = ADVANCED_FACE ( 'NONE', ( #7349 ), #34209, .F. ) ;
#3830 = DIRECTION ( 'NONE',  ( -0.000000000000000000, -0.000000000000000000, -1.000000000000000000 ) ) ;
#3831 = CIRCLE ( 'NONE', #62561, 0.1749999999999998224 ) ;
#3832 = VECTOR ( 'NONE', #182, 1000.000000000000000 ) ;
#3833 = LINE ( 'NONE', #3492, #32777 ) ;
#3834 = ORIENTED_EDGE ( 'NONE', *, *, #43361, .T. ) ;
#3835 = ORIENTED_EDGE ( 'NONE', *, *, #8071, .T. ) ;
#3836 = ADVANCED_FACE ( 'NONE', ( #25030 ), #55801, .F. ) ;
#3837 = AXIS2_PLACEMENT_3D ( 'NONE', #11107, #65217, #33706 ) ;
#3838 = VECTOR ( 'NONE', #66631, 1000.000000000000000 ) ;
#3839 = EDGE_CURVE ( 'NONE', #16920, #43746, #23614, .T. ) ;
#3840 = CARTESIAN_POINT ( 'NONE',  ( -7.813516549646791098, -12.00648345035336284, 195.0000000000000284 ) ) ;
#3841 = EDGE_LOOP ( 'NONE', ( #46707, #12659, #16235, #39354 ) ) ;
#3842 = PLANE ( 'NONE',  #5415 ) ;
#3843 = CARTESIAN_POINT ( 'NONE',  ( 39.00000000000000000, 3.010794155703768650E-16, -2.458500000000000796 ) ) ;
#3844 = CIRCLE ( 'NONE', #15107, 3.499999999999855227 ) ;
#3845 = VECTOR ( 'NONE', #35074, 1000.000000000000000 ) ;
#3846 = EDGE_CURVE ( 'NONE', #50458, #44289, #8392, .T. ) ;
#3847 = LINE ( 'NONE', #68195, #3517 ) ;
#3848 = EDGE_LOOP ( 'NONE', ( #26711, #21221, #61645, #48073 ) ) ;
#3849 = DIRECTION ( 'NONE',  ( 0.000000000000000000, 0.000000000000000000, 1.000000000000000000 ) ) ;
#3850 = CARTESIAN_POINT ( 'NONE',  ( 24.00000000000000000, -15.50000000000000000, 19.33772233983200195 ) ) ;
#3851 = ADVANCED_FACE ( 'NONE', ( #61429 ), #51188, .T. ) ;
#3853 = EDGE_LOOP ( 'NONE', ( #26943, #60184, #16348, #45531 ) ) ;
#3852 = CARTESIAN_POINT ( 'NONE',  ( 1.090483450353370687, 10.73351654964664625, 195.0000000000000284 ) ) ;
#3855 = ORIENTED_EDGE ( 'NONE', *, *, #51825, .F. ) ;
#3854 = FACE_OUTER_BOUND ( 'NONE', #20620, .T. ) ;
#3857 = EDGE_CURVE ( 'NONE', #16139, #43734, #18658, .T. ) ;
#3856 = AXIS2_PLACEMENT_3D ( 'NONE', #8936, #4363, #25925 ) ;
#3858 = DIRECTION ( 'NONE',  ( 0.5000000000000019984, 0.8660254037844375974, 3.181725716174716554E-16 ) ) ;
#3859 = CARTESIAN_POINT ( 'NONE',  ( -8.250000000000001776, -7.249999999999998224, -17.50000000000000000 ) ) ;
#3860 = ADVANCED_FACE ( 'NONE', ( #67102 ), #40227, .F. ) ;
#3861 = DIRECTION ( 'NONE',  ( 1.000000000000000000, -0.000000000000000000, 0.000000000000000000 ) ) ;
#3862 = EDGE_CURVE ( 'NONE', #54387, #3671, #9464, .T. ) ;
#3863 = EDGE_CURVE ( 'NONE', #41566, #21801, #41276, .T. ) ;
#3864 = DIRECTION ( 'NONE',  ( -0.8660254037850523279, 0.000000000000000000, 0.4999999999989371835 ) ) ;
#3865 = CARTESIAN_POINT ( 'NONE',  ( -4.383466043307920224, -8.406483450353396947, 195.0000000000000284 ) ) ;
#3866 = ORIENTED_EDGE ( 'NONE', *, *, #120, .F. ) ;
#3867 = CARTESIAN_POINT ( 'NONE',  ( -8.198316549646712303, 5.993516549646603409, 195.0000000000000284 ) ) ;
#3868 = DIRECTION ( 'NONE',  ( 0.000000000000000000, 0.000000000000000000, 1.000000000000000000 ) ) ;
#3869 = EDGE_CURVE ( 'NONE', #59906, #3912, #25737, .T. ) ;
#3870 = DIRECTION ( 'NONE',  ( 1.836970198721029934E-16, 1.836970198721010706E-16, -1.000000000000000000 ) ) ;
#3872 = VERTEX_POINT ( 'NONE', #10504 ) ;
#3871 = LINE ( 'NONE', #9172, #18647 ) ;
#3873 = PLANE ( 'NONE',  #15546 ) ;
#3874 = EDGE_CURVE ( 'NONE', #64729, #37150, #26083, .T. ) ;
#3875 = VECTOR ( 'NONE', #27020, 1000.000000000000000 ) ;
#3876 = CARTESIAN_POINT ( 'NONE',  ( -9.293516549646710700, 10.91351654964659801, 195.0000000000000284 ) ) ;
#3877 = EDGE_CURVE ( 'NONE', #65338, #69217, #14423, .T. ) ;
#3878 = CARTESIAN_POINT ( 'NONE',  ( 25.50000000000000355, -15.12100000000000044, 22.50000000000000000 ) ) ;
#3879 = ORIENTED_EDGE ( 'NONE', *, *, #45949, .F. ) ;
#3880 = CARTESIAN_POINT ( 'NONE',  ( 30.00000000000000000, -11.70000000000000284, 12.50000000000000000 ) ) ;
#3881 = FACE_OUTER_BOUND ( 'NONE', #9573, .T. ) ;
#3882 = VECTOR ( 'NONE', #20490, 1000.000000000000000 ) ;
#3883 = EDGE_LOOP ( 'NONE', ( #51739, #53835, #65818, #22194 ) ) ;
#3884 = DIRECTION ( 'NONE',  ( 0.000000000000000000, -1.000000000000000000, 0.000000000000000000 ) ) ;
#3885 = CARTESIAN_POINT ( 'NONE',  ( 41.09999999999999432, -0.2000000000000000111, 0.000000000000000000 ) ) ;
#3886 = DIRECTION ( 'NONE',  ( -1.000000000000000000, 0.000000000000000000, 0.000000000000000000 ) ) ;
#3887 = EDGE_CURVE ( 'NONE', #4257, #52360, #69569, .T. ) ;
#3888 = CARTESIAN_POINT ( 'NONE',  ( 25.50000000000000355, -15.50000000000000000, 22.50000000000000000 ) ) ;
#3889 = EDGE_CURVE ( 'NONE', #10676, #61094, #57544, .T. ) ;
#3890 = CARTESIAN_POINT ( 'NONE',  ( -25.49999999999869971, -17.50000000000000000, 22.50000000000000000 ) ) ;
#3891 = VECTOR ( 'NONE', #57736, 1000.000000000000000 ) ;
#3892 = EDGE_LOOP ( 'NONE', ( #48021, #5906, #66933, #45636 ) ) ;
#3893 = CARTESIAN_POINT ( 'NONE',  ( -8.821682069070746479, -2.369523737882742953, 54.00000000000000711 ) ) ;
#3894 = ORIENTED_EDGE ( 'NONE', *, *, #14685, .T. ) ;
#3895 = DIRECTION ( 'NONE',  ( 0.000000000000000000, 0.000000000000000000, 1.000000000000000000 ) ) ;
#3896 = ORIENTED_EDGE ( 'NONE', *, *, #49673, .T. ) ;
#3897 = EDGE_LOOP ( 'NONE', ( #26435, #40381, #63681, #65893 ) ) ;
#3898 = CARTESIAN_POINT ( 'NONE',  ( 49.00000000000000000, -21.00000000000000000, 13.86939075806900057 ) ) ;
#3899 = VECTOR ( 'NONE', #31828, 1000.000000000000000 ) ;
#3900 = AXIS2_PLACEMENT_3D ( 'NONE', #62723, #13938, #41514 ) ;
#3901 = DIRECTION ( 'NONE',  ( 1.000000000000000000, -5.981805089575196197E-17, 0.000000000000000000 ) ) ;
#3902 = VECTOR ( 'NONE', #59045, 1000.000000000000114 ) ;
#3903 = DIRECTION ( 'NONE',  ( 1.000000000000000000, -0.000000000000000000, -0.000000000000000000 ) ) ;
#3904 = ORIENTED_EDGE ( 'NONE', *, *, #56288, .F. ) ;
#3905 = ORIENTED_EDGE ( 'NONE', *, *, #4942, .T. ) ;
#3906 = CARTESIAN_POINT ( 'NONE',  ( -8.250000000000001776, -7.249999999999998224, -14.50000000000000000 ) ) ;
#3907 = ORIENTED_EDGE ( 'NONE', *, *, #4372, .F. ) ;
#3908 = ORIENTED_EDGE ( 'NONE', *, *, #62298, .T. ) ;
#3909 = CYLINDRICAL_SURFACE ( 'NONE', #67668, 24.99999999998784972 ) ;
#3910 = DIRECTION ( 'NONE',  ( -0.000000000000000000, 3.673940397442059868E-16, -1.000000000000000000 ) ) ;
#3911 = DIRECTION ( 'NONE',  ( 1.000000000000000000, -0.000000000000000000, -0.000000000000000000 ) ) ;
#3912 = VERTEX_POINT ( 'NONE', #37386 ) ;
#3913 = CIRCLE ( 'NONE', #33283, 1.620999999999997332 ) ;
#3914 = DIRECTION ( 'NONE',  ( -1.000000000000000000, 0.000000000000000000, 0.000000000000000000 ) ) ;
#3916 = LINE ( 'NONE', #56252, #46988 ) ;
#3915 = DIRECTION ( 'NONE',  ( 1.000000000000000000, -0.000000000000000000, 0.000000000000000000 ) ) ;
#3917 = ORIENTED_EDGE ( 'NONE', *, *, #41787, .F. ) ;
#3919 = EDGE_LOOP ( 'NONE', ( #66401, #34503, #7870, #64097, #35086, #969, #106, #32997 ) ) ;
#3918 = DIRECTION ( 'NONE',  ( 0.000000000000000000, 0.000000000000000000, 1.000000000000000000 ) ) ;
#3920 = VERTEX_POINT ( 'NONE', #4519 ) ;
#3921 = CARTESIAN_POINT ( 'NONE',  ( 78.77321854994620765, 47.95351654967443977, 43.00000000000000000 ) ) ;
#3922 = EDGE_CURVE ( 'NONE', #26084, #36185, #15479, .T. ) ;
#3923 = LINE ( 'NONE', #15595, #37239 ) ;
#3924 = VERTEX_POINT ( 'NONE', #15814 ) ;
#3925 = ORIENTED_EDGE ( 'NONE', *, *, #14477, .T. ) ;
#3926 = AXIS2_PLACEMENT_3D ( 'NONE', #36416, #41717, #43111 ) ;
#3927 = EDGE_CURVE ( 'NONE', #4784, #69381, #15124, .T. ) ;
#3928 = CARTESIAN_POINT ( 'NONE',  ( 16.75000000000000000, -2.500000000000000000, 23.22168783648699986 ) ) ;
#3929 = EDGE_CURVE ( 'NONE', #65979, #60826, #35981, .T. ) ;
#3930 = DIRECTION ( 'NONE',  ( 1.000000000000000000, -0.000000000000000000, 0.000000000000000000 ) ) ;
#3931 = AXIS2_PLACEMENT_3D ( 'NONE', #61788, #18641, #17608 ) ;
#3932 = ORIENTED_EDGE ( 'NONE', *, *, #45631, .F. ) ;
#3933 = ORIENTED_EDGE ( 'NONE', *, *, #29321, .T. ) ;
#3934 = CARTESIAN_POINT ( 'NONE',  ( 8.580623737882818958, -8.930623737882855906, 54.00000000000000711 ) ) ;
#3935 = ADVANCED_FACE ( 'NONE', ( #52962 ), #4172, .F. ) ;
#3936 = FACE_OUTER_BOUND ( 'NONE', #28872, .T. ) ;
#3937 = VERTEX_POINT ( 'NONE', #58951 ) ;
#3938 = VECTOR ( 'NONE', #25880, 1000.000000000000000 ) ;
#3939 = CIRCLE ( 'NONE', #48000, 3.499999999999849454 ) ;
#3940 = DIRECTION ( 'NONE',  ( -1.836970198721029934E-16, 1.836970198721036344E-16, -1.000000000000000000 ) ) ;
#3941 = CYLINDRICAL_SURFACE ( 'NONE', #30567, 3.500000000000003109 ) ;
#3943 = EDGE_LOOP ( 'NONE', ( #64335, #2578, #18772, #55088, #63262, #8375 ) ) ;
#3942 = CARTESIAN_POINT ( 'NONE',  ( 3.677663764522608680, 6.350872789121272177, 54.00000000000000711 ) ) ;
#3944 = ORIENTED_EDGE ( 'NONE', *, *, #9244, .T. ) ;
#3945 = CARTESIAN_POINT ( 'NONE',  ( 0.000000000000000000, 0.000000000000000000, -9.500000000000001776 ) ) ;
#3946 = AXIS2_PLACEMENT_3D ( 'NONE', #67895, #14858, #47024 ) ;
#3947 = CARTESIAN_POINT ( 'NONE',  ( -9.942044687070620057, -9.247904806590648619, 195.0000000000000284 ) ) ;
#3948 = DIRECTION ( 'NONE',  ( 0.000000000000000000, 0.000000000000000000, 1.000000000000000000 ) ) ;
#3949 = CARTESIAN_POINT ( 'NONE',  ( 25.90000000000000213, 6.784888238205741802E-17, 0.5540281690140901327 ) ) ;
#3950 = EDGE_CURVE ( 'NONE', #20196, #54988, #40155, .T. ) ;
#3951 = CARTESIAN_POINT ( 'NONE',  ( -11.00000000000000000, -13.79999999999979998, 17.30000000000000071 ) ) ;
#3952 = VECTOR ( 'NONE', #65236, 1000.000000000000000 ) ;
#3953 = DIRECTION ( 'NONE',  ( 0.000000000000000000, 0.000000000000000000, -1.000000000000000000 ) ) ;
#3954 = ORIENTED_EDGE ( 'NONE', *, *, #38715, .T. ) ;
#3955 = DIRECTION ( 'NONE',  ( -0.000000000000000000, -0.000000000000000000, -1.000000000000000000 ) ) ;
#3957 = VERTEX_POINT ( 'NONE', #37048 ) ;
#3956 = CARTESIAN_POINT ( 'NONE',  ( -8.249999999999996447, 8.250000000000001776, 0.000000000000000000 ) ) ;
#3958 = FACE_OUTER_BOUND ( 'NONE', #16004, .T. ) ;
#3959 = CYLINDRICAL_SURFACE ( 'NONE', #40293, 0.3499999999998886224 ) ;
#3960 = AXIS2_PLACEMENT_3D ( 'NONE', #16038, #37608, #44969 ) ;
#3961 = AXIS2_PLACEMENT_3D ( 'NONE', #7837, #2540, #17770 ) ;
#3962 = DIRECTION ( 'NONE',  ( -0.000000000000000000, -0.000000000000000000, 1.000000000000000000 ) ) ;
#3963 = ORIENTED_EDGE ( 'NONE', *, *, #60940, .T. ) ;
#3964 = PLANE ( 'NONE',  #63662 ) ;
#3965 = CARTESIAN_POINT ( 'NONE',  ( 275.5000000000000000, 0.000000000000000000, -26.50000000000000000 ) ) ;
#3966 = ORIENTED_EDGE ( 'NONE', *, *, #57121, .T. ) ;
#3967 = DIRECTION ( 'NONE',  ( -1.000000000000000000, 2.602085213965213008E-15, 0.000000000000000000 ) ) ;
#3968 = DIRECTION ( 'NONE',  ( 1.000000000000000000, 0.000000000000000000, 0.000000000000000000 ) ) ;
#3969 = EDGE_CURVE ( 'NONE', #45427, #20102, #661, .T. ) ;
#3970 = EDGE_CURVE ( 'NONE', #803, #56608, #5161, .T. ) ;
#3971 = CARTESIAN_POINT ( 'NONE',  ( 3.677663764522614454, -6.364920264886869461, 26.00000000000000711 ) ) ;
#3972 = ORIENTED_EDGE ( 'NONE', *, *, #40481, .T. ) ;
#3973 = CARTESIAN_POINT ( 'NONE',  ( 2.765062094116041980, -9.955011587777324422, 455.0000000000000568 ) ) ;
#3974 = ORIENTED_EDGE ( 'NONE', *, *, #24102, .F. ) ;
#3975 = ADVANCED_FACE ( 'NONE', ( #5219 ), #62855, .F. ) ;
#3976 = ORIENTED_EDGE ( 'NONE', *, *, #61797, .F. ) ;
#3977 = CARTESIAN_POINT ( 'NONE',  ( -11.00000000000000000, -11.50000000000000000, 15.00000000000000000 ) ) ;
#3978 = CARTESIAN_POINT ( 'NONE',  ( 7.250000000000005329, -8.249999999999998224, -13.00000000000000178 ) ) ;
#3979 = DIRECTION ( 'NONE',  ( 0.000000000000000000, -2.854859206170826497E-12, 1.000000000000000000 ) ) ;
#3980 = AXIS2_PLACEMENT_3D ( 'NONE', #11441, #500, #22068 ) ;
#3981 = CARTESIAN_POINT ( 'NONE',  ( 10.50702373788281996, -3.664523737882826815, 54.00000000000000711 ) ) ;
#3982 = FACE_OUTER_BOUND ( 'NONE', #46968, .T. ) ;
#3983 = EDGE_LOOP ( 'NONE', ( #39861, #53404, #36851, #35733 ) ) ;
#3984 = ORIENTED_EDGE ( 'NONE', *, *, #52579, .T. ) ;
#3986 = ORIENTED_EDGE ( 'NONE', *, *, #18257, .T. ) ;
#3985 = CARTESIAN_POINT ( 'NONE',  ( 27.00000000000000000, 0.000000000000000000, 0.000000000000000000 ) ) ;
#3987 = VERTEX_POINT ( 'NONE', #4861 ) ;
#3988 = AXIS2_PLACEMENT_3D ( 'NONE', #46868, #15060, #9403 ) ;
#3989 = CIRCLE ( 'NONE', #50302, 0.5999999999999989786 ) ;
#3990 = CIRCLE ( 'NONE', #28791, 0.1999999999999996503 ) ;
#3991 = CARTESIAN_POINT ( 'NONE',  ( -9.750000000000001776, -9.690000000000001279, -5.000000000000000000 ) ) ;
#3992 = DIRECTION ( 'NONE',  ( 0.000000000000000000, -1.000000000000000000, 0.000000000000000000 ) ) ;
#3993 = CARTESIAN_POINT ( 'NONE',  ( 37.90000000000000568, 3.010794155703768650E-16, -2.458500000000000796 ) ) ;
#3994 = CARTESIAN_POINT ( 'NONE',  ( 35.89999999999999858, -14.06939075806900874, 20.80000000000001137 ) ) ;
#3995 = CARTESIAN_POINT ( 'NONE',  ( -8.393516549646779623, -6.344579767990844665, 455.0000000000000568 ) ) ;
#3996 = AXIS2_PLACEMENT_3D ( 'NONE', #34584, #29629, #35993 ) ;
#3998 = CARTESIAN_POINT ( 'NONE',  ( -29.50000000000000355, -11.50000000000000000, -19.00000000000000000 ) ) ;
#3997 = LINE ( 'NONE', #26262, #51289 ) ;
#3999 = ORIENTED_EDGE ( 'NONE', *, *, #113, .F. ) ;
#4000 = EDGE_LOOP ( 'NONE', ( #10172, #49038, #56270, #10583 ) ) ;
#4001 = ORIENTED_EDGE ( 'NONE', *, *, #15083, .F. ) ;
#4003 = ORIENTED_EDGE ( 'NONE', *, *, #3253, .T. ) ;
#4002 = TOROIDAL_SURFACE ( 'NONE', #50268, 5.000000000000003553, 1.000000000000000000 ) ;
#4004 = DIRECTION ( 'NONE',  ( 0.000000000000000000, -1.000000000000000000, 0.000000000000000000 ) ) ;
#4005 = LINE ( 'NONE', #36519, #59211 ) ;
#4006 =( LENGTH_UNIT ( ) NAMED_UNIT ( * ) SI_UNIT ( .MILLI., .METRE. ) );
#4007 = EDGE_CURVE ( 'NONE', #22338, #26887, #57896, .T. ) ;
#4008 = AXIS2_PLACEMENT_3D ( 'NONE', #60290, #11847, #13600 ) ;
#4009 = DIRECTION ( 'NONE',  ( 0.000000000000000000, 1.000000000000000000, -0.000000000000000000 ) ) ;
#4010 = EDGE_LOOP ( 'NONE', ( #52793, #35835, #26362, #19222 ) ) ;
#4011 = EDGE_LOOP ( 'NONE', ( #67663, #22369 ) ) ;
#4012 = ORIENTED_EDGE ( 'NONE', *, *, #40364, .F. ) ;
#4013 = AXIS2_PLACEMENT_3D ( 'NONE', #34975, #18720, #12703 ) ;
#4014 = EDGE_CURVE ( 'NONE', #21676, #20566, #3806, .T. ) ;
#4015 = DIRECTION ( 'NONE',  ( 0.000000000000000000, 0.000000000000000000, -1.000000000000000000 ) ) ;
#4016 = ORIENTED_EDGE ( 'NONE', *, *, #59672, .F. ) ;
#4017 = ORIENTED_EDGE ( 'NONE', *, *, #46102, .T. ) ;
#4018 = ADVANCED_FACE ( 'NONE', ( #42682 ), #68515, .F. ) ;
#4019 = CARTESIAN_POINT ( 'NONE',  ( 10.00000000000000000, 18.00000000000000355, 21.00000000000000000 ) ) ;
#4020 = ADVANCED_FACE ( 'NONE', ( #27122 ), #48687, .F. ) ;
#4021 = VERTEX_POINT ( 'NONE', #55049 ) ;
#4022 = ORIENTED_EDGE ( 'NONE', *, *, #36112, .F. ) ;
#4023 = LINE ( 'NONE', #68015, #62107 ) ;
#4024 = EDGE_CURVE ( 'NONE', #26009, #29819, #53717, .T. ) ;
#4025 = EDGE_CURVE ( 'NONE', #27370, #12812, #62728, .T. ) ;
#4027 = ORIENTED_EDGE ( 'NONE', *, *, #21227, .F. ) ;
#4026 = CARTESIAN_POINT ( 'NONE',  ( 8.250000000000005329, -7.249999999999998224, -26.00000000000001066 ) ) ;
#4028 = ORIENTED_EDGE ( 'NONE', *, *, #12725, .F. ) ;
#4029 = LINE ( 'NONE', #68732, #45374 ) ;
#4030 = ADVANCED_FACE ( 'NONE', ( #16858 ), #28154, .T. ) ;
#4031 = DIRECTION ( 'NONE',  ( 0.000000000000000000, 1.000000000000000000, 0.000000000000000000 ) ) ;
#4032 = AXIS2_PLACEMENT_3D ( 'NONE', #35572, #34866, #7999 ) ;
#4034 = ORIENTED_EDGE ( 'NONE', *, *, #22127, .T. ) ;
#4033 = FACE_OUTER_BOUND ( 'NONE', #19286, .T. ) ;
#4035 = VERTEX_POINT ( 'NONE', #43024 ) ;
#4036 = CARTESIAN_POINT ( 'NONE',  ( 14.25000000000000000, -0.2038245569916330158, 21.77831216351300014 ) ) ;
#4037 = AXIS2_PLACEMENT_3D ( 'NONE', #24317, #46225, #67461 ) ;
#4038 = PLANE ( 'NONE',  #1291 ) ;
#4039 = CYLINDRICAL_SURFACE ( 'NONE', #54931, 5.000000000000000000 ) ;
#4040 = FACE_OUTER_BOUND ( 'NONE', #28519, .T. ) ;
#4041 = ORIENTED_EDGE ( 'NONE', *, *, #64230, .T. ) ;
#4042 = CARTESIAN_POINT ( 'NONE',  ( 283.0000000000000568, -25.60000000000000142, -17.60000000000000142 ) ) ;
#4043 = AXIS2_PLACEMENT_3D ( 'NONE', #24540, #9322, #41499 ) ;
#4044 = AXIS2_PLACEMENT_3D ( 'NONE', #14396, #8734, #23940 ) ;
#4046 = PLANE ( 'NONE',  #68239 ) ;
#4045 = AXIS2_PLACEMENT_3D ( 'NONE', #813, #64809, #456 ) ;
#4047 = DIRECTION ( 'NONE',  ( 0.000000000000000000, 0.000000000000000000, 1.000000000000000000 ) ) ;
#4048 = ORIENTED_EDGE ( 'NONE', *, *, #69876, .F. ) ;
#4049 = DIRECTION ( 'NONE',  ( -0.000000000000000000, -0.000000000000000000, -1.000000000000000000 ) ) ;
#4050 = DIRECTION ( 'NONE',  ( 0.000000000000000000, 0.000000000000000000, 1.000000000000000000 ) ) ;
#4051 = CIRCLE ( 'NONE', #39059, 3.500000000000003109 ) ;
#4052 = VECTOR ( 'NONE', #40336, 1000.000000000000000 ) ;
#4053 = DIRECTION ( 'NONE',  ( 1.349135440953254805E-14, 1.000000000000000000, 1.836970198721035604E-16 ) ) ;
#4054 = ORIENTED_EDGE ( 'NONE', *, *, #59982, .F. ) ;
#4055 = VECTOR ( 'NONE', #37453, 1000.000000000000000 ) ;
#4056 = DIRECTION ( 'NONE',  ( -0.000000000000000000, 3.673940397442059868E-16, -1.000000000000000000 ) ) ;
#4057 = CARTESIAN_POINT ( 'NONE',  ( 276.8775010008008053, -25.00000000000000000, 17.50000000000000000 ) ) ;
#4058 = EDGE_CURVE ( 'NONE', #40904, #26371, #38431, .T. ) ;
#4059 = CIRCLE ( 'NONE', #45830, 0.6000000000000006439 ) ;
#4060 = DIRECTION ( 'NONE',  ( -1.000000000000000000, 0.000000000000000000, 0.000000000000000000 ) ) ;
#4061 = ORIENTED_EDGE ( 'NONE', *, *, #8787, .T. ) ;
#4062 = CARTESIAN_POINT ( 'NONE',  ( -30.00000000000000000, -16.28999999999999915, 14.50000000000000000 ) ) ;
#4063 = CARTESIAN_POINT ( 'NONE',  ( -4.706725378239217328, 4.141586236041038482, 54.00000000000000711 ) ) ;
#4064 = FACE_OUTER_BOUND ( 'NONE', #10426, .T. ) ;
#4065 = EDGE_CURVE ( 'NONE', #24148, #53899, #65019, .T. ) ;
#4066 = VECTOR ( 'NONE', #40194, 1000.000000000000000 ) ;
#4067 = EDGE_CURVE ( 'NONE', #34255, #28070, #959, .T. ) ;
#4068 = FACE_OUTER_BOUND ( 'NONE', #34195, .T. ) ;
#4069 = CARTESIAN_POINT ( 'NONE',  ( 7.261609891743268541, -8.000000000000000000, 5.000000000000000000 ) ) ;
#4070 = VERTEX_POINT ( 'NONE', #64952 ) ;
#4071 = DIRECTION ( 'NONE',  ( -8.540177112501197482E-15, -1.000000000000000000, -3.673940397442060361E-16 ) ) ;
#4072 = CARTESIAN_POINT ( 'NONE',  ( 6.657023737882818537, -10.31452373788281207, 26.00000000000000000 ) ) ;
#4073 = DIRECTION ( 'NONE',  ( 1.000000000000000000, -0.000000000000000000, 1.224646799147353207E-16 ) ) ;
#4074 = EDGE_CURVE ( 'NONE', #34907, #34803, #31159, .T. ) ;
#4075 = CARTESIAN_POINT ( 'NONE',  ( -9.689726262117330791, -10.05377373788272699, 54.00000000000000711 ) ) ;
#4076 = LINE ( 'NONE', #15728, #48655 ) ;
#4077 = ORIENTED_EDGE ( 'NONE', *, *, #16945, .T. ) ;
#4079 = VERTEX_POINT ( 'NONE', #17192 ) ;
#4078 = LINE ( 'NONE', #14333, #2358 ) ;
#4080 = DIRECTION ( 'NONE',  ( 0.000000000000000000, -1.000000000000000000, 0.000000000000000000 ) ) ;
#4081 = DIRECTION ( 'NONE',  ( -1.000000000000000000, 2.135044278125299371E-15, 0.000000000000000000 ) ) ;
#4082 = CARTESIAN_POINT ( 'NONE',  ( 1.866219381641484931, 9.404046420174006826, 455.0000000000000568 ) ) ;
#4083 = ORIENTED_EDGE ( 'NONE', *, *, #31977, .F. ) ;
#4084 = AXIS2_PLACEMENT_3D ( 'NONE', #63865, #32040, #64221 ) ;
#4085 = DIRECTION ( 'NONE',  ( -1.000000000000000000, 0.000000000000000000, 0.000000000000000000 ) ) ;
#4086 = LINE ( 'NONE', #69475, #8152 ) ;
#4087 = CIRCLE ( 'NONE', #27794, 2.000000000000001776 ) ;
#4088 = ORIENTED_EDGE ( 'NONE', *, *, #48607, .F. ) ;
#4089 = VERTEX_POINT ( 'NONE', #33797 ) ;
#4090 = AXIS2_PLACEMENT_3D ( 'NONE', #10754, #58153, #48246 ) ;
#4091 = ORIENTED_EDGE ( 'NONE', *, *, #8062, .F. ) ;
#4092 = CARTESIAN_POINT ( 'NONE',  ( 9.841277389592722358, -1.690483450353490680, 455.0000000000000568 ) ) ;
#4093 = LINE ( 'NONE', #63834, #21903 ) ;
#4094 = DIRECTION ( 'NONE',  ( 0.000000000000000000, 0.000000000000000000, 1.000000000000000000 ) ) ;
#4095 = FACE_OUTER_BOUND ( 'NONE', #26759, .T. ) ;
#4096 = AXIS2_PLACEMENT_3D ( 'NONE', #42900, #37955, #37261 ) ;
#4097 = VECTOR ( 'NONE', #53812, 1000.000000000000000 ) ;
#4098 = VECTOR ( 'NONE', #8426, 1000.000000000000000 ) ;
#4099 = ORIENTED_EDGE ( 'NONE', *, *, #15452, .F. ) ;
#4100 = ORIENTED_EDGE ( 'NONE', *, *, #35693, .F. ) ;
#4101 = PLANE ( 'NONE',  #60614 ) ;
#4102 = LINE ( 'NONE', #52903, #59873 ) ;
#4103 = VECTOR ( 'NONE', #43325, 1000.000000000000000 ) ;
#4104 = VECTOR ( 'NONE', #39112, 1000.000000000000000 ) ;
#4105 = AXIS2_PLACEMENT_3D ( 'NONE', #28246, #66067, #16254 ) ;
#4106 = VERTEX_POINT ( 'NONE', #60319 ) ;
#4107 = VERTEX_POINT ( 'NONE', #251 ) ;
#4108 = ORIENTED_EDGE ( 'NONE', *, *, #19014, .T. ) ;
#4109 = ORIENTED_EDGE ( 'NONE', *, *, #40177, .F. ) ;
#4110 = CIRCLE ( 'NONE', #30025, 0.9999999999999991118 ) ;
#4111 = CARTESIAN_POINT ( 'NONE',  ( -5.380658396643274166, -7.265214908726128407, 195.0000000000000284 ) ) ;
#4112 = UNCERTAINTY_MEASURE_WITH_UNIT (LENGTH_MEASURE( 1.000000000000000082E-05 ), #36386, 'distance_accuracy_value', 'NONE');
#4113 = EDGE_CURVE ( 'NONE', #35743, #69116, #6306, .T. ) ;
#4115 = EDGE_LOOP ( 'NONE', ( #47796, #49763, #45969, #63380 ) ) ;
#4114 = CARTESIAN_POINT ( 'NONE',  ( 7.408280051175172076, -3.724485858128701032, 54.00000000000000711 ) ) ;
#4116 = CARTESIAN_POINT ( 'NONE',  ( 39.00000000000000000, -16.96999999999999886, 21.00000000000000000 ) ) ;
#4117 = AXIS2_PLACEMENT_3D ( 'NONE', #13343, #12975, #2386 ) ;
#4118 = DIRECTION ( 'NONE',  ( 0.7071067811865474617, -0.7071067811865474617, 0.000000000000000000 ) ) ;
#4119 = ADVANCED_FACE ( 'NONE', ( #21465 ), #1286, .F. ) ;
#4120 = CARTESIAN_POINT ( 'NONE',  ( 49.00000000000000000, -0.1999999999911795112, 8.826273045769999343E-12 ) ) ;
#4121 = ORIENTED_EDGE ( 'NONE', *, *, #67855, .T. ) ;
#4122 = ORIENTED_EDGE ( 'NONE', *, *, #9999, .F. ) ;
#4123 = DIRECTION ( 'NONE',  ( 0.000000000000000000, 1.000000000000000000, 0.000000000000000000 ) ) ;
#4124 = CARTESIAN_POINT ( 'NONE',  ( 9.899999999999998579, 20.60000000000000142, -13.86939075806900057 ) ) ;
#4125 = ORIENTED_EDGE ( 'NONE', *, *, #64390, .T. ) ;
#4126 = SURFACE_SIDE_STYLE ('',( #68468 ) ) ;
#4127 = LINE ( 'NONE', #63523, #65216 ) ;
#4128 = VECTOR ( 'NONE', #32655, 1000.000000000000000 ) ;
#4129 = CARTESIAN_POINT ( 'NONE',  ( 30.00000000000000000, -12.00000000000000000, 12.20000000000000107 ) ) ;
#4130 = ORIENTED_EDGE ( 'NONE', *, *, #39443, .F. ) ;
#4131 = DIRECTION ( 'NONE',  ( 1.000000000000000000, -0.000000000000000000, -0.000000000000000000 ) ) ;
#4132 = CARTESIAN_POINT ( 'NONE',  ( -4.727349090213552429, -4.201500623656063915, 455.0000000000000568 ) ) ;
#4133 = DIRECTION ( 'NONE',  ( 0.000000000000000000, 1.000000000000000000, 0.000000000000000000 ) ) ;
#4134 = VECTOR ( 'NONE', #19539, 1000.000000000000000 ) ;
#4135 = CARTESIAN_POINT ( 'NONE',  ( -4.393516549646667713, 11.77351654964658856, 455.0000000000000568 ) ) ;
#4136 = VECTOR ( 'NONE', #59430, 1000.000000000000000 ) ;
#4137 = CIRCLE ( 'NONE', #13144, 24.99999999998789946 ) ;
#4138 = CARTESIAN_POINT ( 'NONE',  ( 7.450000000000004619, -1.336933437520057563E-15, -21.00000000000000000 ) ) ;
#4139 = VERTEX_POINT ( 'NONE', #59647 ) ;
#4140 = FACE_OUTER_BOUND ( 'NONE', #49209, .T. ) ;
#4141 = DIRECTION ( 'NONE',  ( -0.000000000000000000, 1.000000000000000000, -0.000000000000000000 ) ) ;
#4142 = DIRECTION ( 'NONE',  ( -1.000000000000000000, 0.000000000000000000, 0.000000000000000000 ) ) ;
#4143 = DIRECTION ( 'NONE',  ( 0.000000000000000000, 0.000000000000000000, 1.000000000000000000 ) ) ;
#4144 = VECTOR ( 'NONE', #39933, 1000.000000000000000 ) ;
#4145 = CIRCLE ( 'NONE', #43661, 4.500000000000191847 ) ;
#4146 = CARTESIAN_POINT ( 'NONE',  ( 6.364920264886889001, 6.822336235477383326, 54.00000000000000711 ) ) ;
#4147 = CARTESIAN_POINT ( 'NONE',  ( 8.093267424590459669, 8.697938382363064491, 54.00000000000000711 ) ) ;
#4148 = VECTOR ( 'NONE', #36924, 1000.000000000000000 ) ;
#4149 = DIRECTION ( 'NONE',  ( 0.7071067811865475727, 0.000000000000000000, -0.7071067811865475727 ) ) ;
#4150 = CARTESIAN_POINT ( 'NONE',  ( -7.250000000000000888, 8.250000000000001776, -11.00000000000000000 ) ) ;
#4151 = EDGE_LOOP ( 'NONE', ( #36352, #18853, #17435, #38167 ) ) ;
#4152 = CARTESIAN_POINT ( 'NONE',  ( 7.250000000000005329, 7.250000000000000888, -11.50000000000000000 ) ) ;
#4153 = LINE ( 'NONE', #58591, #47431 ) ;
#4154 = LINE ( 'NONE', #25360, #24438 ) ;
#4155 = CARTESIAN_POINT ( 'NONE',  ( 49.00000000000000000, -0.2000000000089119934, 8.909539772616881237E-12 ) ) ;
#4156 = EDGE_CURVE ( 'NONE', #64280, #17297, #43732, .T. ) ;
#4157 = CIRCLE ( 'NONE', #16569, 0.1999999999999987899 ) ;
#4158 = CARTESIAN_POINT ( 'NONE',  ( 0.000000000000000000, -7.449999999999998401, -24.50000000000000000 ) ) ;
#4159 = LINE ( 'NONE', #64940, #45505 ) ;
#4160 = CARTESIAN_POINT ( 'NONE',  ( -4.727349090213463612, 4.188533722949258298, 195.0000000000000284 ) ) ;
#4161 = ORIENTED_EDGE ( 'NONE', *, *, #6444, .F. ) ;
#4162 = VECTOR ( 'NONE', #3242, 1000.000000000000000 ) ;
#4163 = ORIENTED_EDGE ( 'NONE', *, *, #33390, .T. ) ;
#4164 = FACE_BOUND ( 'NONE', #5904, .T. ) ;
#4165 = LINE ( 'NONE', #42322, #709 ) ;
#4166 = EDGE_LOOP ( 'NONE', ( #8247, #45435, #33540, #69517, #60919, #30958, #48425, #39786 ) ) ;
#4167 = DIRECTION ( 'NONE',  ( -0.000000000000000000, -0.000000000000000000, -1.000000000000000000 ) ) ;
#4168 = ADVANCED_FACE ( 'NONE', ( #54345, #65308 ), #33464, .T. ) ;
#4169 = CARTESIAN_POINT ( 'NONE',  ( -7.450000000000001954, 0.000000000000000000, -15.50000000000000000 ) ) ;
#4170 = ORIENTED_EDGE ( 'NONE', *, *, #52157, .T. ) ;
#4171 = EDGE_CURVE ( 'NONE', #30626, #5395, #64601, .T. ) ;
#4172 = PLANE ( 'NONE',  #19825 ) ;
#4173 = ORIENTED_EDGE ( 'NONE', *, *, #12908, .F. ) ;
#4174 = ORIENTED_EDGE ( 'NONE', *, *, #14016, .F. ) ;
#4175 = CARTESIAN_POINT ( 'NONE',  ( 8.930623737882818602, -10.05377373788281581, 26.00000000000000000 ) ) ;
#4176 = VERTEX_POINT ( 'NONE', #60677 ) ;
#4177 = ORIENTED_EDGE ( 'NONE', *, *, #22780, .T. ) ;
#4178 = LINE ( 'NONE', #68161, #40656 ) ;
#4179 = CARTESIAN_POINT ( 'NONE',  ( 6.836383711243002814, 6.350872789121261519, 54.00000000000000711 ) ) ;
#4180 = DIRECTION ( 'NONE',  ( 1.836970198721029934E-16, -1.836970198721036344E-16, 1.000000000000000000 ) ) ;
#4181 = AXIS2_PLACEMENT_3D ( 'NONE', #37881, #15965, #10648 ) ;
#4182 = ORIENTED_EDGE ( 'NONE', *, *, #33978, .F. ) ;
#4183 = DIRECTION ( 'NONE',  ( 1.000000000000000000, -1.115702204244422993E-14, -1.836970198721050395E-16 ) ) ;
#4185 = CARTESIAN_POINT ( 'NONE',  ( -5.380658396643321240, -7.265214908726175480, 455.0000000000000568 ) ) ;
#4184 = FACE_BOUND ( 'NONE', #45616, .T. ) ;
#4186 = VERTEX_POINT ( 'NONE', #32436 ) ;
#4187 = ORIENTED_EDGE ( 'NONE', *, *, #26534, .T. ) ;
#4188 = AXIS2_PLACEMENT_3D ( 'NONE', #53003, #19492, #9867 ) ;
#4189 = VERTEX_POINT ( 'NONE', #12224 ) ;
#4190 = ORIENTED_EDGE ( 'NONE', *, *, #70, .T. ) ;
#4191 = VECTOR ( 'NONE', #29938, 1000.000000000000000 ) ;
#4192 = AXIS2_PLACEMENT_3D ( 'NONE', #10203, #26469, #15522 ) ;
#4193 = DIRECTION ( 'NONE',  ( -1.000000000000000000, 0.000000000000000000, 0.000000000000000000 ) ) ;
#4195 = ORIENTED_EDGE ( 'NONE', *, *, #53465, .F. ) ;
#4194 = CARTESIAN_POINT ( 'NONE',  ( 16.74999999999999289, -0.3152037684892571301, -22.74589050208021845 ) ) ;
#4196 = EDGE_CURVE ( 'NONE', #35525, #57629, #55383, .T. ) ;
#4197 = VECTOR ( 'NONE', #21443, 1000.000000000000000 ) ;
#4198 = AXIS2_PLACEMENT_3D ( 'NONE', #48291, #2779, #42275 ) ;
#4199 = DIRECTION ( 'NONE',  ( 1.000000000000000000, 0.000000000000000000, 0.000000000000000000 ) ) ;
#4200 = DIRECTION ( 'NONE',  ( -1.000000000000000000, 0.000000000000000000, 0.000000000000000000 ) ) ;
#4201 = AXIS2_PLACEMENT_3D ( 'NONE', #58090, #5049, #36520 ) ;
#4202 = EDGE_CURVE ( 'NONE', #3514, #39584, #34836, .T. ) ;
#4203 = VERTEX_POINT ( 'NONE', #13279 ) ;
#4204 = EDGE_CURVE ( 'NONE', #14841, #66296, #29537, .T. ) ;
#4205 = ORIENTED_EDGE ( 'NONE', *, *, #46348, .T. ) ;
#4206 = CIRCLE ( 'NONE', #39156, 0.1749999999999998224 ) ;
#4207 = VECTOR ( 'NONE', #48089, 1000.000000000000114 ) ;
#4208 = PLANE ( 'NONE',  #67377 ) ;
#4209 = EDGE_CURVE ( 'NONE', #1245, #64281, #39787, .T. ) ;
#4210 = VERTEX_POINT ( 'NONE', #6921 ) ;
#4211 = DIRECTION ( 'NONE',  ( 0.000000000000000000, 0.000000000000000000, 1.000000000000000000 ) ) ;
#4213 = CIRCLE ( 'NONE', #49383, 0.8128000000000145109 ) ;
#4212 = CARTESIAN_POINT ( 'NONE',  ( 11.19368345035336532, -11.19368345035347723, 455.0000000000000568 ) ) ;
#4214 = EDGE_CURVE ( 'NONE', #30799, #2028, #7266, .T. ) ;
#4215 = FACE_OUTER_BOUND ( 'NONE', #41784, .T. ) ;
#4216 = ORIENTED_EDGE ( 'NONE', *, *, #62803, .T. ) ;
#4217 = EDGE_CURVE ( 'NONE', #25895, #55193, #17886, .T. ) ;
#4218 = CIRCLE ( 'NONE', #32426, 1.000000000000000000 ) ;
#4219 = CARTESIAN_POINT ( 'NONE',  ( 4.406483450353373854, 11.77351654964663119, 195.0000000000000284 ) ) ;
#4220 = VERTEX_POINT ( 'NONE', #56072 ) ;
#4222 = ORIENTED_EDGE ( 'NONE', *, *, #59508, .F. ) ;
#4221 = DIRECTION ( 'NONE',  ( 1.000000000000000000, 0.000000000000000000, 0.000000000000000000 ) ) ;
#4223 = CYLINDRICAL_SURFACE ( 'NONE', #42205, 0.3999999999999993006 ) ;
#4224 = CARTESIAN_POINT ( 'NONE',  ( 46.39999999999999858, 21.00000000000000000, 1.250000000000000000 ) ) ;
#4225 = CARTESIAN_POINT ( 'NONE',  ( 30.00000000000000000, -17.14999999999999858, -27.00000000000000000 ) ) ;
#4226 = CARTESIAN_POINT ( 'NONE',  ( 7.250000000000005329, -8.249999999999998224, -26.00000000000001066 ) ) ;
#4227 = PLANE ( 'NONE',  #24017 ) ;
#4228 = ORIENTED_EDGE ( 'NONE', *, *, #3174, .F. ) ;
#4229 = DIRECTION ( 'NONE',  ( 1.836970198721029934E-16, 1.836970198721010706E-16, -1.000000000000000000 ) ) ;
#4230 = CYLINDRICAL_SURFACE ( 'NONE', #12377, 0.3500000000002719824 ) ;
#4231 = DIRECTION ( 'NONE',  ( 0.000000000000000000, 1.000000000000000000, 0.000000000000000000 ) ) ;
#4233 = VERTEX_POINT ( 'NONE', #50421 ) ;
#4232 = FACE_OUTER_BOUND ( 'NONE', #2187, .T. ) ;
#4234 = CARTESIAN_POINT ( 'NONE',  ( 11.00000000000000000, -5.599999999999999645, 9.400000000000000355 ) ) ;
#4235 = ADVANCED_FACE ( 'NONE', ( #18227 ), #23890, .F. ) ;
#4236 = MECHANICAL_DESIGN_GEOMETRIC_PRESENTATION_REPRESENTATION (  '', ( #64106 ), #6496 ) ;
#4237 = FACE_OUTER_BOUND ( 'NONE', #37732, .T. ) ;
#4238 = CARTESIAN_POINT ( 'NONE',  ( 10.92648345035337343, -2.706483450353490916, 455.0000000000000568 ) ) ;
#4239 = ORIENTED_EDGE ( 'NONE', *, *, #55745, .F. ) ;
#4240 = DIRECTION ( 'NONE',  ( 1.836970198721029934E-16, 1.836970198721010706E-16, -1.000000000000000000 ) ) ;
#4241 = FACE_OUTER_BOUND ( 'NONE', #1790, .T. ) ;
#4242 = ORIENTED_EDGE ( 'NONE', *, *, #13850, .F. ) ;
#4243 =( NAMED_UNIT ( * ) PLANE_ANGLE_UNIT ( ) SI_UNIT ( $, .RADIAN. ) );
#4244 = EDGE_CURVE ( 'NONE', #6097, #48107, #2667, .T. ) ;
#4245 = DIRECTION ( 'NONE',  ( -1.000000000000000000, 0.000000000000000000, 0.000000000000000000 ) ) ;
#4246 = AXIS2_PLACEMENT_3D ( 'NONE', #27082, #10132, #16127 ) ;
#4247 = AXIS2_PLACEMENT_3D ( 'NONE', #9068, #14725, #36288 ) ;
#4248 = CARTESIAN_POINT ( 'NONE',  ( 25.57999999999999829, 0.000000000000000000, 2.458500000000000796 ) ) ;
#4249 = CARTESIAN_POINT ( 'NONE',  ( 16.89999999999999858, 13.66939075806899240, -20.79999999999999361 ) ) ;
#4251 = CARTESIAN_POINT ( 'NONE',  ( 11.12648345035337982, -4.206483450353492692, 455.0000000000000568 ) ) ;
#4250 = VECTOR ( 'NONE', #58114, 1000.000000000000000 ) ;
#4252 = ORIENTED_EDGE ( 'NONE', *, *, #52302, .F. ) ;
#4253 = PRODUCT_DEFINITION_FORMATION_WITH_SPECIFIED_SOURCE ( 'ANY', '', #8578, .NOT_KNOWN. ) ;
#4254 = ORIENTED_EDGE ( 'NONE', *, *, #3619, .F. ) ;
#4255 = CARTESIAN_POINT ( 'NONE',  ( 13.00000000000000178, -15.50000000000000000, 14.50000000000000000 ) ) ;
#4256 = ORIENTED_EDGE ( 'NONE', *, *, #18153, .F. ) ;
#4257 = VERTEX_POINT ( 'NONE', #24242 ) ;
#4258 = CARTESIAN_POINT ( 'NONE',  ( 15.50000000000000000, -5.000000000000000000, 22.50000000000000000 ) ) ;
#4259 = CIRCLE ( 'NONE', #887, 0.1999999999999987899 ) ;
#4260 = CIRCLE ( 'NONE', #26870, 1.224999999999999423 ) ;
#4261 = LINE ( 'NONE', #3549, #34342 ) ;
#4262 = ADVANCED_FACE ( 'NONE', ( #50063 ), #34482, .F. ) ;
#4263 = FACE_OUTER_BOUND ( 'NONE', #51756, .T. ) ;
#4264 = ORIENTED_EDGE ( 'NONE', *, *, #54338, .F. ) ;
#4265 = ORIENTED_EDGE ( 'NONE', *, *, #2032, .T. ) ;
#4266 = CARTESIAN_POINT ( 'NONE',  ( -30.00000000000000000, -13.79999999999979998, 17.64999999999988844 ) ) ;
#4267 = ORIENTED_EDGE ( 'NONE', *, *, #22951, .F. ) ;
#4268 = ORIENTED_EDGE ( 'NONE', *, *, #10077, .T. ) ;
#4269 = CIRCLE ( 'NONE', #30247, 25.39999999999999858 ) ;
#4270 = PLANE ( 'NONE',  #19155 ) ;
#4271 = CARTESIAN_POINT ( 'NONE',  ( 176.0064834503533575, -29.01119750012555443, 0.000000000000000000 ) ) ;
#4272 = DIRECTION ( 'NONE',  ( 1.000000000000000000, 0.000000000000000000, 0.000000000000000000 ) ) ;
#4273 = EDGE_CURVE ( 'NONE', #54217, #9481, #36511, .T. ) ;
#4274 = EDGE_LOOP ( 'NONE', ( #42183, #28152, #10158, #38515 ) ) ;
#4275 = EDGE_CURVE ( 'NONE', #59373, #24243, #49106, .T. ) ;
#4276 = CARTESIAN_POINT ( 'NONE',  ( -9.942044687070568543, 9.234937905883914055, 195.0000000000000284 ) ) ;
#4278 = CARTESIAN_POINT ( 'NONE',  ( 7.357023737882806280, 6.651770455163672935, 54.00000000000000711 ) ) ;
#4277 = LINE ( 'NONE', #47390, #19676 ) ;
#4279 = VERTEX_POINT ( 'NONE', #12567 ) ;
#4282 = ADVANCED_FACE ( 'NONE', ( #28831 ), #18942, .F. ) ;
#4281 = VERTEX_POINT ( 'NONE', #1977 ) ;
#4280 = CARTESIAN_POINT ( 'NONE',  ( 9.955011587777271131, 9.234937905883876752, 455.0000000000000568 ) ) ;
#4283 = ORIENTED_EDGE ( 'NONE', *, *, #54113, .T. ) ;
#4284 = ADVANCED_FACE ( 'NONE', ( #40497 ), #45098, .F. ) ;
#4285 = EDGE_CURVE ( 'NONE', #49731, #46063, #30863, .T. ) ;
#4286 = FACE_OUTER_BOUND ( 'NONE', #66115, .T. ) ;
#4287 = EDGE_CURVE ( 'NONE', #55626, #54387, #20251, .T. ) ;
#4288 = DIRECTION ( 'NONE',  ( 0.000000000000000000, 0.000000000000000000, 1.000000000000000000 ) ) ;
#4289 = EDGE_CURVE ( 'NONE', #40726, #9110, #66161, .T. ) ;
#4290 = ORIENTED_EDGE ( 'NONE', *, *, #19172, .T. ) ;
#4291 = VECTOR ( 'NONE', #22053, 1000.000000000000000 ) ;
#4292 = VERTEX_POINT ( 'NONE', #37228 ) ;
#4293 = EDGE_CURVE ( 'NONE', #8038, #11924, #16003, .T. ) ;
#4294 = DIRECTION ( 'NONE',  ( 0.000000000000000000, 0.000000000000000000, 1.000000000000000000 ) ) ;
#4295 = CARTESIAN_POINT ( 'NONE',  ( 7.250000000000005329, -7.249999999999998224, -25.50000000000000355 ) ) ;
#4296 = VERTEX_POINT ( 'NONE', #52805 ) ;
#4297 = ORIENTED_EDGE ( 'NONE', *, *, #55372, .T. ) ;
#4298 = CARTESIAN_POINT ( 'NONE',  ( -7.250000000000000000, -7.449999999999998401, -12.00000000000000000 ) ) ;
#4299 = SHAPE_REPRESENTATION ( 'Actuator  Carriage Assembly', ( #49371, #15508, #29004, #4201, #18863, #58416, #40310, #24525 ), #60654 ) ;
#4300 = ADVANCED_FACE ( 'NONE', ( #5040 ), #26263, .F. ) ;
#4301 = DIRECTION ( 'NONE',  ( -1.000000000000000000, 0.000000000000000000, 0.000000000000000000 ) ) ;
#4302 = ORIENTED_EDGE ( 'NONE', *, *, #33168, .F. ) ;
#4303 = EDGE_CURVE ( 'NONE', #63139, #35171, #11039, .T. ) ;
#4304 = CIRCLE ( 'NONE', #60701, 0.5000000000001392220 ) ;
#4305 = CARTESIAN_POINT ( 'NONE',  ( 275.5000000000000000, -42.50000000000000000, 15.10000000000000142 ) ) ;
#4306 = FACE_OUTER_BOUND ( 'NONE', #37137, .T. ) ;
#4307 = CIRCLE ( 'NONE', #13304, 1.620999999999997332 ) ;
#4309 = ORIENTED_EDGE ( 'NONE', *, *, #42655, .F. ) ;
#4308 = CARTESIAN_POINT ( 'NONE',  ( -7.250000000000000888, 8.250000000000001776, -26.00000000000001066 ) ) ;
#4311 = EDGE_LOOP ( 'NONE', ( #42824, #25465, #46743, #26360 ) ) ;
#4310 = LINE ( 'NONE', #26555, #1788 ) ;
#4312 = CARTESIAN_POINT ( 'NONE',  ( 39.90000000000000568, 21.00000000000000000, -16.96999999999999886 ) ) ;
#4313 = VECTOR ( 'NONE', #16390, 1000.000000000000000 ) ;
#4314 = LINE ( 'NONE', #40716, #30668 ) ;
#4315 = EDGE_CURVE ( 'NONE', #49314, #52260, #43612, .T. ) ;
#4316 = LINE ( 'NONE', #25870, #54996 ) ;
#4317 = CARTESIAN_POINT ( 'NONE',  ( 7.616533956692244089, 8.393516549646575342, 455.0000000000000568 ) ) ;
#4318 = CARTESIAN_POINT ( 'NONE',  ( 7.250000000000005329, -7.449999999999998401, -12.50000000000000000 ) ) ;
#4319 = DIRECTION ( 'NONE',  ( -0.000000000000000000, -0.000000000000000000, -1.000000000000000000 ) ) ;
#4320 = ORIENTED_EDGE ( 'NONE', *, *, #14739, .F. ) ;
#4321 = CARTESIAN_POINT ( 'NONE',  ( -11.75000000000000000, -5.200000000000001066, 26.25000000000000000 ) ) ;
#4323 = VERTEX_POINT ( 'NONE', #47817 ) ;
#4322 = DIRECTION ( 'NONE',  ( 0.000000000000000000, 1.000000000000000000, 0.000000000000000000 ) ) ;
#4324 = VECTOR ( 'NONE', #64231, 1000.000000000000000 ) ;
#4325 = DIRECTION ( 'NONE',  ( 1.000000000000000000, 0.000000000000000000, 0.000000000000000000 ) ) ;
#4326 = DIRECTION ( 'NONE',  ( 0.000000000000000000, -3.673940397442059868E-16, 1.000000000000000000 ) ) ;
#4327 = PLANE ( 'NONE',  #22883 ) ;
#4328 = CARTESIAN_POINT ( 'NONE',  ( 69.47321854994619628, 47.95351654967443977, 40.00000000000000000 ) ) ;
#4329 = ORIENTED_EDGE ( 'NONE', *, *, #49172, .T. ) ;
#4330 = CARTESIAN_POINT ( 'NONE',  ( -5.993516549646711766, 5.993516549646603409, 455.0000000000000568 ) ) ;
#4331 = CARTESIAN_POINT ( 'NONE',  ( 7.186223737882818874, -5.257023737882825287, 54.00000000000000711 ) ) ;
#4332 = VERTEX_POINT ( 'NONE', #10007 ) ;
#4333 = EDGE_CURVE ( 'NONE', #10103, #68276, #26662, .T. ) ;
#4334 = LINE ( 'NONE', #25890, #54925 ) ;
#4335 = CARTESIAN_POINT ( 'NONE',  ( 275.0000000000000000, -31.30000000000095284, 12.19999999999906315 ) ) ;
#4336 = ADVANCED_FACE ( 'NONE', ( #92 ), #48182, .T. ) ;
#4337 = LINE ( 'NONE', #63015, #43358 ) ;
#4338 = ORIENTED_EDGE ( 'NONE', *, *, #51451, .T. ) ;
#4339 = DIRECTION ( 'NONE',  ( 0.000000000000000000, 0.000000000000000000, -1.000000000000000000 ) ) ;
#4340 = ORIENTED_EDGE ( 'NONE', *, *, #41331, .T. ) ;
#4341 =( GEOMETRIC_REPRESENTATION_CONTEXT ( 3 ) GLOBAL_UNCERTAINTY_ASSIGNED_CONTEXT ( ( #9763 ) ) GLOBAL_UNIT_ASSIGNED_CONTEXT ( ( #4671, #19867, #35783 ) ) REPRESENTATION_CONTEXT ( 'NONE', 'WORKASPACE' ) );
#4342 = EDGE_CURVE ( 'NONE', #2487, #56322, #32261, .T. ) ;
#4343 = ORIENTED_EDGE ( 'NONE', *, *, #24183, .F. ) ;
#4344 = DIRECTION ( 'NONE',  ( -0.000000000000000000, 3.673940397442059868E-16, -1.000000000000000000 ) ) ;
#4345 = DIRECTION ( 'NONE',  ( 0.000000000000000000, 0.6801302850037830305, 0.7330912599538155217 ) ) ;
#4346 = LINE ( 'NONE', #14235, #19810 ) ;
#4347 = EDGE_CURVE ( 'NONE', #60085, #27370, #9655, .T. ) ;
#4348 = CARTESIAN_POINT ( 'NONE',  ( 283.0000000000000568, -25.93000000000544958, -9.412893218815410634 ) ) ;
#4349 = ADVANCED_FACE ( 'NONE', ( #69388 ), #31233, .T. ) ;
#4350 = CARTESIAN_POINT ( 'NONE',  ( 2.544523737882809833, 8.821682069070735821, 26.00000000000000711 ) ) ;
#4351 = ORIENTED_EDGE ( 'NONE', *, *, #68525, .F. ) ;
#4352 = ORIENTED_EDGE ( 'NONE', *, *, #30352, .F. ) ;
#4354 = ORIENTED_EDGE ( 'NONE', *, *, #19983, .F. ) ;
#4353 = CARTESIAN_POINT ( 'NONE',  ( 25.50000000000000355, -15.50000000000000000, -22.50000000000000000 ) ) ;
#4355 = ORIENTED_EDGE ( 'NONE', *, *, #6868, .T. ) ;
#4356 = LINE ( 'NONE', #10343, #58599 ) ;
#4357 = CYLINDRICAL_SURFACE ( 'NONE', #30951, 4.500000000000188294 ) ;
#4358 = DIRECTION ( 'NONE',  ( -1.000000000000000000, 1.079558018506126625E-14, 1.836970198721049656E-16 ) ) ;
#4359 = EDGE_CURVE ( 'NONE', #29457, #43425, #42520, .T. ) ;
#4360 = EDGE_CURVE ( 'NONE', #43019, #9455, #64110, .T. ) ;
#4361 = VECTOR ( 'NONE', #19726, 1000.000000000000000 ) ;
#4362 = CARTESIAN_POINT ( 'NONE',  ( 11.00000000000000000, -10.85999999999999943, -9.000000000000001776 ) ) ;
#4364 = DIRECTION ( 'NONE',  ( -0.000000000000000000, -0.000000000000000000, -1.000000000000000000 ) ) ;
#4363 = DIRECTION ( 'NONE',  ( -0.6414496315691446959, 0.7671651518153106419, 2.818519042764040589E-16 ) ) ;
#4365 = EDGE_LOOP ( 'NONE', ( #25783, #56255 ) ) ;
#4366 = EDGE_LOOP ( 'NONE', ( #188, #52403, #25502, #1882 ) ) ;
#4367 = VERTEX_POINT ( 'NONE', #26609 ) ;
#4368 = EDGE_CURVE ( 'NONE', #45380, #47595, #64444, .T. ) ;
#4369 = ADVANCED_FACE ( 'NONE', ( #5409 ), #48525, .T. ) ;
#4370 = LINE ( 'NONE', #30514, #54770 ) ;
#4371 = LINE ( 'NONE', #36891, #53611 ) ;
#4372 = EDGE_CURVE ( 'NONE', #14815, #30184, #43211, .T. ) ;
#4373 = CARTESIAN_POINT ( 'NONE',  ( 0.000000000000000000, 0.000000000000000000, 0.000000000000000000 ) ) ;
#4374 = CIRCLE ( 'NONE', #37121, 24.99999999998794920 ) ;
#4375 = CARTESIAN_POINT ( 'NONE',  ( -11.77351654964679106, -7.606483450353366038, 455.0000000000000568 ) ) ;
#4376 = VERTEX_POINT ( 'NONE', #53155 ) ;
#4377 = ORIENTED_EDGE ( 'NONE', *, *, #32603, .F. ) ;
#4378 = ORIENTED_EDGE ( 'NONE', *, *, #22449, .T. ) ;
#4379 = DIRECTION ( 'NONE',  ( 8.359604446858500663E-15, 1.000000000000000000, 0.000000000000000000 ) ) ;
#4380 = ORIENTED_EDGE ( 'NONE', *, *, #15369, .F. ) ;
#4381 = EDGE_LOOP ( 'NONE', ( #56656, #9144, #23807, #28461 ) ) ;
#4382 = CARTESIAN_POINT ( 'NONE',  ( -11.50000000000000000, -12.00000000000000000, -10.69999999999999929 ) ) ;
#4383 = ORIENTED_EDGE ( 'NONE', *, *, #69682, .F. ) ;
#4384 = VERTEX_POINT ( 'NONE', #59483 ) ;
#4385 = CARTESIAN_POINT ( 'NONE',  ( -7.250000000000000000, -7.449999999999998401, -15.50000000000000000 ) ) ;
#4386 = EDGE_CURVE ( 'NONE', #30841, #9491, #52662, .T. ) ;
#4388 = ORIENTED_EDGE ( 'NONE', *, *, #15461, .F. ) ;
#4387 = DIRECTION ( 'NONE',  ( 0.000000000000000000, 0.000000000000000000, 1.000000000000000000 ) ) ;
#4389 = ORIENTED_EDGE ( 'NONE', *, *, #57376, .F. ) ;
#4390 = ADVANCED_FACE ( 'NONE', ( #4696 ), #438, .F. ) ;
#4391 = DIRECTION ( 'NONE',  ( 3.540251991789405856E-15, 1.000000000000000000, 0.000000000000000000 ) ) ;
#4392 = DIRECTION ( 'NONE',  ( 0.000000000000000000, 0.000000000000000000, -1.000000000000000000 ) ) ;
#4394 = EDGE_LOOP ( 'NONE', ( #30886, #32218, #19485, #18906 ) ) ;
#4393 = DIRECTION ( 'NONE',  ( 1.000000000000000000, -3.491481338843132961E-15, 0.000000000000000000 ) ) ;
#4395 = ORIENTED_EDGE ( 'NONE', *, *, #37098, .T. ) ;
#4396 = CARTESIAN_POINT ( 'NONE',  ( 15.50000000000000000, -0.2038245569916610489, 21.05662432702600029 ) ) ;
#4397 = LINE ( 'NONE', #25959, #48691 ) ;
#4398 = LINE ( 'NONE', #25611, #27812 ) ;
#4399 = CIRCLE ( 'NONE', #48448, 0.2000000000000005107 ) ;
#4400 = CARTESIAN_POINT ( 'NONE',  ( -5.993516549646728642, -6.006483450353378828, 195.0000000000000284 ) ) ;
#4401 = ORIENTED_EDGE ( 'NONE', *, *, #47876, .F. ) ;
#4402 = DIRECTION ( 'NONE',  ( 0.000000000000000000, 0.000000000000000000, -1.000000000000000000 ) ) ;
#4403 = VECTOR ( 'NONE', #56674, 1000.000000000000000 ) ;
#4404 = CARTESIAN_POINT ( 'NONE',  ( 15.00000000000000000, -21.00000000000000000, 8.000000000000000000 ) ) ;
#4405 = DIRECTION ( 'NONE',  ( -1.000000000000000000, 0.000000000000000000, 0.000000000000000000 ) ) ;
#4406 = CARTESIAN_POINT ( 'NONE',  ( 2.765062094116059743, 9.942044687070495712, 195.0000000000000284 ) ) ;
#4407 = FACE_OUTER_BOUND ( 'NONE', #30855, .T. ) ;
#4408 = CIRCLE ( 'NONE', #43899, 0.5249999999999994671 ) ;
#4409 = CARTESIAN_POINT ( 'NONE',  ( 9.690000000000001279, 10.50000000000000000, -4.250000000000000000 ) ) ;
#4410 = VERTEX_POINT ( 'NONE', #55215 ) ;
#4411 = VECTOR ( 'NONE', #28649, 1000.000000000000000 ) ;
#4412 = FILL_AREA_STYLE ('',( #20306 ) ) ;
#4413 = CYLINDRICAL_SURFACE ( 'NONE', #35571, 0.1749999999999998224 ) ;
#4414 = TOROIDAL_SURFACE ( 'NONE', #49569, 0.06000000000000080963, 0.7500000000000000000 ) ;
#4415 = EDGE_CURVE ( 'NONE', #27000, #50982, #18062, .T. ) ;
#4416 = CARTESIAN_POINT ( 'NONE',  ( -7.342976262117277386, -5.552858015815541393, 26.00000000000000711 ) ) ;
#4417 = ORIENTED_EDGE ( 'NONE', *, *, #41119, .T. ) ;
#4418 = DIRECTION ( 'NONE',  ( 1.000000000000000000, -1.047444401652940007E-14, 1.836970198721010706E-16 ) ) ;
#4419 = FACE_OUTER_BOUND ( 'NONE', #51295, .T. ) ;
#4420 = DIRECTION ( 'NONE',  ( 0.000000000000000000, 0.000000000000000000, 1.000000000000000000 ) ) ;
#4421 = ADVANCED_FACE ( 'NONE', ( #59827 ), #66164, .F. ) ;
#4422 = DIRECTION ( 'NONE',  ( -0.000000000000000000, -0.000000000000000000, -1.000000000000000000 ) ) ;
#4423 = AXIS2_PLACEMENT_3D ( 'NONE', #18803, #61934, #24468 ) ;
#4424 = DIRECTION ( 'NONE',  ( -0.000000000000000000, -0.000000000000000000, -1.000000000000000000 ) ) ;
#4425 = ORIENTED_EDGE ( 'NONE', *, *, #29502, .F. ) ;
#4426 = LINE ( 'NONE', #9361, #47989 ) ;
#4427 = FACE_OUTER_BOUND ( 'NONE', #39518, .T. ) ;
#4428 = EDGE_CURVE ( 'NONE', #48708, #33185, #43902, .T. ) ;
#4429 = EDGE_CURVE ( 'NONE', #10667, #39124, #38270, .T. ) ;
#4430 = CARTESIAN_POINT ( 'NONE',  ( -7.447976262117260049, 9.880476262117177555, 25.99999580000000421 ) ) ;
#4431 =( NAMED_UNIT ( * ) SI_UNIT ( $, .STERADIAN. ) SOLID_ANGLE_UNIT ( ) );
#4432 = EDGE_CURVE ( 'NONE', #11140, #3786, #12065, .T. ) ;
#4433 = CARTESIAN_POINT ( 'NONE',  ( -11.11351654964668612, 8.693516549646636449, 455.0000000000000568 ) ) ;
#4434 = ADVANCED_FACE ( 'NONE', ( #65481 ), #6760, .F. ) ;
#4435 = VERTEX_POINT ( 'NONE', #798 ) ;
#4437 = ORIENTED_EDGE ( 'NONE', *, *, #14219, .F. ) ;
#4436 = DIRECTION ( 'NONE',  ( 0.000000000000000000, 0.000000000000000000, -1.000000000000000000 ) ) ;
#4438 = LINE ( 'NONE', #64184, #62088 ) ;
#4439 = LINE ( 'NONE', #63822, #53806 ) ;
#4440 = CARTESIAN_POINT ( 'NONE',  ( -7.250000000000001776, -7.249999999999998224, -26.00000000000001066 ) ) ;
#4441 = VERTEX_POINT ( 'NONE', #33972 ) ;
#4442 = LINE ( 'NONE', #32346, #51427 ) ;
#4443 = CARTESIAN_POINT ( 'NONE',  ( 40.90000000000000568, 14.08845687959340331, -21.00000000000000000 ) ) ;
#4444 = VERTEX_POINT ( 'NONE', #60161 ) ;
#4445 = ORIENTED_EDGE ( 'NONE', *, *, #57166, .F. ) ;
#4446 = VERTEX_POINT ( 'NONE', #39290 ) ;
#4447 = FACE_OUTER_BOUND ( 'NONE', #40394, .T. ) ;
#4448 = VECTOR ( 'NONE', #14149, 1000.000000000000000 ) ;
#4449 = CARTESIAN_POINT ( 'NONE',  ( 41.09999999999999432, -21.00000000000000000, 13.86939075806900057 ) ) ;
#4450 = DIRECTION ( 'NONE',  ( -0.5773502691896246208, 0.5773502691896263972, -0.5773502691896263972 ) ) ;
#4451 = VERTEX_POINT ( 'NONE', #60847 ) ;
#4452 = VERTEX_POINT ( 'NONE', #28327 ) ;
#4453 = DIRECTION ( 'NONE',  ( 1.952517519553884087E-14, 1.000000000000000000, 1.836970198721046697E-16 ) ) ;
#4454 = CIRCLE ( 'NONE', #43950, 0.1749999999999993783 ) ;
#4455 = DIRECTION ( 'NONE',  ( 0.000000000000000000, -1.000000000000000000, 0.000000000000000000 ) ) ;
#4456 = ORIENTED_EDGE ( 'NONE', *, *, #69411, .F. ) ;
#4457 = VERTEX_POINT ( 'NONE', #11379 ) ;
#4458 = ORIENTED_EDGE ( 'NONE', *, *, #6978, .T. ) ;
#4459 = ORIENTED_EDGE ( 'NONE', *, *, #60331, .T. ) ;
#4460 = DIRECTION ( 'NONE',  ( -1.053224967557347660E-14, -1.000000000000000000, 0.000000000000000000 ) ) ;
#4462 = ORIENTED_EDGE ( 'NONE', *, *, #3874, .T. ) ;
#4461 = FACE_OUTER_BOUND ( 'NONE', #3142, .T. ) ;
#4463 = AXIS2_PLACEMENT_3D ( 'NONE', #32410, #18206, #67356 ) ;
#4464 = CARTESIAN_POINT ( 'NONE',  ( 7.250000000000005329, -8.249999999999998224, -11.00000000000000000 ) ) ;
#4465 = EDGE_CURVE ( 'NONE', #36902, #64226, #8566, .T. ) ;
#4466 = CARTESIAN_POINT ( 'NONE',  ( 15.50000000000000000, 0.000000000000000000, -22.50000000000000000 ) ) ;
#4467 = CARTESIAN_POINT ( 'NONE',  ( -17.51999999999999957, -15.50000000000000000, -26.00000000000000355 ) ) ;
#4468 = ORIENTED_EDGE ( 'NONE', *, *, #43195, .F. ) ;
#4469 = EDGE_CURVE ( 'NONE', #40228, #12566, #49898, .T. ) ;
#4470 = VERTEX_POINT ( 'NONE', #6086 ) ;
#4471 = AXIS2_PLACEMENT_3D ( 'NONE', #16296, #38229, #37527 ) ;
#4472 = DIRECTION ( 'NONE',  ( -1.000000000000000000, 0.000000000000000000, 0.000000000000000000 ) ) ;
#4473 = DIRECTION ( 'NONE',  ( 0.000000000000000000, 0.000000000000000000, 1.000000000000000000 ) ) ;
#4474 = ORIENTED_EDGE ( 'NONE', *, *, #26056, .F. ) ;
#4475 = LINE ( 'NONE', #31698, #58284 ) ;
#4476 = FACE_OUTER_BOUND ( 'NONE', #11717, .T. ) ;
#4477 = CARTESIAN_POINT ( 'NONE',  ( 3.606483450353397568, 4.609516549646590633, 455.0000000000000568 ) ) ;
#4478 = ORIENTED_EDGE ( 'NONE', *, *, #24906, .T. ) ;
#4479 = CARTESIAN_POINT ( 'NONE',  ( 9.703773737882785966, -8.580623737882845603, 26.00000000000000000 ) ) ;
#4480 = DIRECTION ( 'NONE',  ( 1.214636490590110272E-14, 1.000000000000000000, 1.836970198721032892E-16 ) ) ;
#4481 = FACE_OUTER_BOUND ( 'NONE', #44101, .T. ) ;
#4482 = CARTESIAN_POINT ( 'NONE',  ( 283.0000000000000568, -27.13000000000000611, -13.50000000000000000 ) ) ;
#4483 = DIRECTION ( 'NONE',  ( 0.000000000000000000, 0.000000000000000000, 1.000000000000000000 ) ) ;
#4484 = VERTEX_POINT ( 'NONE', #2155 ) ;
#4485 = DIRECTION ( 'NONE',  ( 1.000000000000000000, 0.000000000000000000, 0.000000000000000000 ) ) ;
#4486 = CARTESIAN_POINT ( 'NONE',  ( 176.4833316329832940, -10.00000000000000178, 326.8892501111512843 ) ) ;
#4487 = AXIS2_PLACEMENT_3D ( 'NONE', #23184, #27114, #1278 ) ;
#4488 = DIRECTION ( 'NONE',  ( -7.751221965937476285E-17, 1.000000000000000000, 0.000000000000000000 ) ) ;
#4489 = CIRCLE ( 'NONE', #36068, 24.99999999998784972 ) ;
#4490 = DIRECTION ( 'NONE',  ( 1.000000000000000000, 0.000000000000000000, 0.000000000000000000 ) ) ;
#4491 = EDGE_CURVE ( 'NONE', #43562, #42042, #29029, .T. ) ;
#4492 = ORIENTED_EDGE ( 'NONE', *, *, #1672, .T. ) ;
#4493 = DIRECTION ( 'NONE',  ( 0.000000000000000000, 0.000000000000000000, 1.000000000000000000 ) ) ;
#4494 = CARTESIAN_POINT ( 'NONE',  ( -11.00000000000000000, -11.70000000000000284, -12.50000000000000000 ) ) ;
#4495 = VECTOR ( 'NONE', #47777, 1000.000000000000000 ) ;
#4496 = CARTESIAN_POINT ( 'NONE',  ( -8.250000000000001776, 0.000000000000000000, -10.00000000000000000 ) ) ;
#4497 = CARTESIAN_POINT ( 'NONE',  ( -13.00000000000000178, -17.35230188589299516, -15.35019951917100478 ) ) ;
#4498 = EDGE_LOOP ( 'NONE', ( #61576, #27278, #69900, #68635 ) ) ;
#4499 = DIRECTION ( 'NONE',  ( 8.903847840905249551E-15, 1.000000000000000000, 0.000000000000000000 ) ) ;
#4500 = LINE ( 'NONE', #64247, #9176 ) ;
#4501 = CARTESIAN_POINT ( 'NONE',  ( 6.832023737882812142, 9.722976262117196455, 26.00000000000000711 ) ) ;
#4502 = VECTOR ( 'NONE', #41875, 1000.000000000000000 ) ;
#4503 = DIRECTION ( 'NONE',  ( -0.7071067811865474617, 0.7071067811865474617, 0.000000000000000000 ) ) ;
#4504 =( LENGTH_UNIT ( ) NAMED_UNIT ( * ) SI_UNIT ( .MILLI., .METRE. ) );
#4505 = EDGE_CURVE ( 'NONE', #42529, #26273, #49278, .T. ) ;
#4506 = DIRECTION ( 'NONE',  ( -0.000000000000000000, -0.000000000000000000, -1.000000000000000000 ) ) ;
#4507 = EDGE_CURVE ( 'NONE', #66814, #39291, #11714, .T. ) ;
#4508 = VERTEX_POINT ( 'NONE', #22357 ) ;
#4509 = VECTOR ( 'NONE', #25546, 1000.000000000000000 ) ;
#4510 = EDGE_LOOP ( 'NONE', ( #10401, #32620, #25605, #28328 ) ) ;
#4511 = EDGE_CURVE ( 'NONE', #34571, #43764, #41326, .T. ) ;
#4512 = DIRECTION ( 'NONE',  ( 1.000000000000000000, 0.000000000000000000, 0.000000000000000000 ) ) ;
#4513 = CARTESIAN_POINT ( 'NONE',  ( -14.25000000000000000, -0.2038245569916330158, 23.22168783648699986 ) ) ;
#4514 = VERTEX_POINT ( 'NONE', #1808 ) ;
#4515 = CARTESIAN_POINT ( 'NONE',  ( -15.50000000000000000, -1.037157890325000054, -22.50000000000000000 ) ) ;
#4516 = VECTOR ( 'NONE', #8405, 1000.000000000000000 ) ;
#4517 = CARTESIAN_POINT ( 'NONE',  ( -7.250000000000000000, -7.449999999999998401, -22.50000000000000000 ) ) ;
#4518 = ORIENTED_EDGE ( 'NONE', *, *, #13575, .F. ) ;
#4519 = CARTESIAN_POINT ( 'NONE',  ( 1.480523737882813773, 8.598420958951637161, 54.00000000000000711 ) ) ;
#4520 = VERTEX_POINT ( 'NONE', #34312 ) ;
#4521 = ORIENTED_EDGE ( 'NONE', *, *, #37165, .F. ) ;
#4522 = DIRECTION ( 'NONE',  ( 0.000000000000000000, 0.000000000000000000, -1.000000000000000000 ) ) ;
#4523 = ORIENTED_EDGE ( 'NONE', *, *, #7471, .T. ) ;
#4524 = CARTESIAN_POINT ( 'NONE',  ( 283.0000000000000568, -25.14575131106458272, -17.35424868893542083 ) ) ;
#4525 = DIRECTION ( 'NONE',  ( -0.000000000000000000, 3.673940397442059868E-16, -1.000000000000000000 ) ) ;
#4526 = CARTESIAN_POINT ( 'NONE',  ( 7.250000000000005329, -7.249999999999998224, -17.50000000000000000 ) ) ;
#4527 = EDGE_LOOP ( 'NONE', ( #11360, #45754, #13267, #67656 ) ) ;
#4528 = LINE ( 'NONE', #20776, #35726 ) ;
#4530 = DIRECTION ( 'NONE',  ( 0.000000000000000000, -1.000000000000000000, 0.000000000000000000 ) ) ;
#4529 = DIRECTION ( 'NONE',  ( -1.000000000000000000, 0.000000000000000000, -0.000000000000000000 ) ) ;
#4531 = VERTEX_POINT ( 'NONE', #55899 ) ;
#4532 = ORIENTED_EDGE ( 'NONE', *, *, #15523, .F. ) ;
#4533 = EDGE_LOOP ( 'NONE', ( #14549, #19404, #15661, #65984, #47333, #34143, #61422, #28531 ) ) ;
#4535 = EDGE_LOOP ( 'NONE', ( #30832, #55391, #69238, #23107 ) ) ;
#4534 = CONTEXT_DEPENDENT_SHAPE_REPRESENTATION ( #690, #12056 ) ;
#4536 = DIRECTION ( 'NONE',  ( -0.000000000000000000, 0.000000000000000000, 1.000000000000000000 ) ) ;
#4537 = VECTOR ( 'NONE', #13186, 1000.000000000000114 ) ;
#4538 = AXIS2_PLACEMENT_3D ( 'NONE', #47300, #30337, #58615 ) ;
#4540 = ORIENTED_EDGE ( 'NONE', *, *, #43052, .F. ) ;
#4539 = LINE ( 'NONE', #20441, #55689 ) ;
#4541 = CARTESIAN_POINT ( 'NONE',  ( 39.90000000000000568, -0.1999999999911430404, -8.864436962241481021E-12 ) ) ;
#4542 = AXIS2_PLACEMENT_3D ( 'NONE', #57181, #7679, #35593 ) ;
#4543 = CARTESIAN_POINT ( 'NONE',  ( -4.609516549646752281, -3.606483450353441533, 455.0000000000000568 ) ) ;
#4544 = VERTEX_POINT ( 'NONE', #7455 ) ;
#4545 = ORIENTED_EDGE ( 'NONE', *, *, #18365, .T. ) ;
#4546 = EDGE_CURVE ( 'NONE', #20667, #40341, #33300, .T. ) ;
#4547 = VECTOR ( 'NONE', #50115, 1000.000000000000000 ) ;
#4548 = EDGE_CURVE ( 'NONE', #47484, #62940, #54879, .T. ) ;
#4549 = EDGE_CURVE ( 'NONE', #32931, #16848, #6435, .T. ) ;
#4550 = DIRECTION ( 'NONE',  ( 0.000000000000000000, 0.000000000000000000, -1.000000000000000000 ) ) ;
#4551 = ORIENTED_EDGE ( 'NONE', *, *, #8116, .F. ) ;
#4552 = EDGE_CURVE ( 'NONE', #10667, #67031, #35359, .T. ) ;
#4553 = VECTOR ( 'NONE', #6655, 1000.000000000000000 ) ;
#4554 = CARTESIAN_POINT ( 'NONE',  ( -15.50000000000000000, -0.2038245569916614930, -23.94337567297399971 ) ) ;
#4555 = DIRECTION ( 'NONE',  ( 0.000000000000000000, -1.000000000000000000, 0.000000000000000000 ) ) ;
#4556 = LINE ( 'NONE', #47328, #6878 ) ;
#4557 = AXIS2_PLACEMENT_3D ( 'NONE', #49999, #39046, #65582 ) ;
#4558 = ORIENTED_EDGE ( 'NONE', *, *, #59813, .T. ) ;
#4559 = CIRCLE ( 'NONE', #19068, 4.000000000000000888 ) ;
#4560 = PLANE ( 'NONE',  #67257 ) ;
#4561 = PLANE ( 'NONE',  #41420 ) ;
#4563 = ORIENTED_EDGE ( 'NONE', *, *, #35453, .T. ) ;
#4562 = LINE ( 'NONE', #26128, #63618 ) ;
#4565 = ORIENTED_EDGE ( 'NONE', *, *, #34150, .T. ) ;
#4564 = DIRECTION ( 'NONE',  ( -1.000000000000000000, 0.000000000000000000, 0.000000000000000000 ) ) ;
#4566 = DIRECTION ( 'NONE',  ( -1.000000000000000000, 0.000000000000000000, 0.000000000000000000 ) ) ;
#4567 = AXIS2_PLACEMENT_3D ( 'NONE', #61571, #54570, #6120 ) ;
#4568 = CARTESIAN_POINT ( 'NONE',  ( 15.00000000000000000, -42.00000000000000000, -26.50000000000000000 ) ) ;
#4569 = CARTESIAN_POINT ( 'NONE',  ( 46.39999999999999858, 21.00000000000000000, -1.250000000000000000 ) ) ;
#4570 = DIRECTION ( 'NONE',  ( 0.000000000000000000, 0.000000000000000000, 1.000000000000000000 ) ) ;
#4571 = LINE ( 'NONE', #20815, #49963 ) ;
#4572 = ORIENTED_EDGE ( 'NONE', *, *, #38966, .F. ) ;
#4573 = LINE ( 'NONE', #25793, #56101 ) ;
#4574 = FACE_OUTER_BOUND ( 'NONE', #14499, .T. ) ;
#4575 = CARTESIAN_POINT ( 'NONE',  ( 9.306483450353418618, 10.91351654964656426, 455.0000000000000568 ) ) ;
#4577 = ORIENTED_EDGE ( 'NONE', *, *, #57799, .T. ) ;
#4576 = DIRECTION ( 'NONE',  ( -1.000000000000000000, 0.000000000000000000, 0.000000000000000000 ) ) ;
#4578 = FACE_OUTER_BOUND ( 'NONE', #56776, .T. ) ;
#4579 = CIRCLE ( 'NONE', #33914, 0.5000000000079367624 ) ;
#4580 = CARTESIAN_POINT ( 'NONE',  ( 78.77321854994620765, 47.95351654967443977, 20.00000000000000000 ) ) ;
#4581 = LINE ( 'NONE', #26488, #23964 ) ;
#4582 = DIRECTION ( 'NONE',  ( 1.671920889371702854E-15, 1.000000000000000000, -0.000000000000000000 ) ) ;
#4583 = ORIENTED_EDGE ( 'NONE', *, *, #60205, .T. ) ;
#4584 = DIRECTION ( 'NONE',  ( -0.7071067811865401342, 0.7071067811865550112, 0.000000000000000000 ) ) ;
#4585 = DIRECTION ( 'NONE',  ( 0.000000000000000000, -1.000000000000000000, 0.000000000000000000 ) ) ;
#4586 = ORIENTED_EDGE ( 'NONE', *, *, #9742, .F. ) ;
#4587 = CARTESIAN_POINT ( 'NONE',  ( -8.250000000000001776, -7.249999999999998224, -24.00000000000000000 ) ) ;
#4588 = DIRECTION ( 'NONE',  ( 0.000000000000000000, 1.000000000000000000, 0.000000000000000000 ) ) ;
#4589 = FACE_OUTER_BOUND ( 'NONE', #29434, .T. ) ;
#4590 = FACE_BOUND ( 'NONE', #12126, .T. ) ;
#4591 = VECTOR ( 'NONE', #64046, 1000.000000000000000 ) ;
#4592 = EDGE_CURVE ( 'NONE', #6741, #68576, #3916, .T. ) ;
#4593 = CYLINDRICAL_SURFACE ( 'NONE', #51068, 5.000000000000000000 ) ;
#4594 = AXIS2_PLACEMENT_3D ( 'NONE', #32061, #41967, #32417 ) ;
#4595 = VERTEX_POINT ( 'NONE', #56938 ) ;
#4596 = EDGE_CURVE ( 'NONE', #20240, #701, #25552, .T. ) ;
#4597 = ORIENTED_EDGE ( 'NONE', *, *, #48549, .T. ) ;
#4598 = DIRECTION ( 'NONE',  ( -0.000000000000000000, -0.000000000000000000, -1.000000000000000000 ) ) ;
#4599 = VERTEX_POINT ( 'NONE', #57299 ) ;
#4600 = EDGE_CURVE ( 'NONE', #2646, #13864, #49158, .T. ) ;
#4601 = ORIENTED_EDGE ( 'NONE', *, *, #69559, .T. ) ;
#4602 = VECTOR ( 'NONE', #1948, 1000.000000000000000 ) ;
#4603 = CARTESIAN_POINT ( 'NONE',  ( 4.456444791733522252E-16, 7.450000000000002842, -17.00000000000000000 ) ) ;
#4604 = EDGE_CURVE ( 'NONE', #13479, #14411, #39965, .T. ) ;
#4605 = VECTOR ( 'NONE', #12900, 1000.000000000000000 ) ;
#4606 = DIRECTION ( 'NONE',  ( 7.808916176531286882E-15, 1.000000000000000000, -0.000000000000000000 ) ) ;
#4607 = CARTESIAN_POINT ( 'NONE',  ( 0.000000000000000000, 0.000000000000000000, -23.00000000000000000 ) ) ;
#4608 = ORIENTED_EDGE ( 'NONE', *, *, #52674, .F. ) ;
#4609 = EDGE_CURVE ( 'NONE', #22670, #4860, #7796, .T. ) ;
#4610 = ORIENTED_EDGE ( 'NONE', *, *, #61252, .F. ) ;
#4611 = DIRECTION ( 'NONE',  ( -0.000000000000000000, 0.000000000000000000, 1.000000000000000000 ) ) ;
#4613 = VERTEX_POINT ( 'NONE', #61531 ) ;
#4612 = EDGE_CURVE ( 'NONE', #24514, #64746, #44589, .T. ) ;
#4614 = ORIENTED_EDGE ( 'NONE', *, *, #42496, .F. ) ;
#4615 = DIRECTION ( 'NONE',  ( -0.000000000000000000, -0.000000000000000000, -1.000000000000000000 ) ) ;
#4616 = CARTESIAN_POINT ( 'NONE',  ( 14.50000000000000178, -42.50000000000000000, 26.50000000000000000 ) ) ;
#4617 = DIRECTION ( 'NONE',  ( 0.000000000000000000, 0.000000000000000000, -1.000000000000000000 ) ) ;
#4618 = EDGE_LOOP ( 'NONE', ( #31498, #14160, #45071, #3467 ) ) ;
#4619 = CARTESIAN_POINT ( 'NONE',  ( 7.250000000000005329, 8.250000000000001776, -14.00000000000000000 ) ) ;
#4620 = AXIS2_PLACEMENT_3D ( 'NONE', #20904, #15260, #31532 ) ;
#4622 = DIRECTION ( 'NONE',  ( 0.000000000000000000, 0.000000000000000000, -1.000000000000000000 ) ) ;
#4621 = CARTESIAN_POINT ( 'NONE',  ( -1.466476262117315743, -8.612468434717266419, 54.00000000000000711 ) ) ;
#4623 = EDGE_LOOP ( 'NONE', ( #42884, #29273, #44952, #1420 ) ) ;
#4625 = ORIENTED_EDGE ( 'NONE', *, *, #66897, .F. ) ;
#4624 = DIRECTION ( 'NONE',  ( 1.047444401652940007E-14, 1.000000000000000000, 1.836970198721029934E-16 ) ) ;
#4626 = VERTEX_POINT ( 'NONE', #67568 ) ;
#4627 = CARTESIAN_POINT ( 'NONE',  ( 6.006483450353379716, -6.006483450353394815, 195.0000000000000284 ) ) ;
#4628 = CARTESIAN_POINT ( 'NONE',  ( -7.250000000000000888, 7.450000000000003730, -14.50000000000000000 ) ) ;
#4629 = CIRCLE ( 'NONE', #29428, 0.1999999999999996503 ) ;
#4630 = EDGE_LOOP ( 'NONE', ( #37370, #41116, #18560, #21222 ) ) ;
#4631 = CARTESIAN_POINT ( 'NONE',  ( -10.30047626211724854, -3.664523737882715348, 54.00000000000000711 ) ) ;
#4632 = DIRECTION ( 'NONE',  ( -0.000000000000000000, 1.000000000000000000, 3.673940397442059868E-16 ) ) ;
#4633 = ORIENTED_EDGE ( 'NONE', *, *, #33935, .F. ) ;
#4634 = ORIENTED_EDGE ( 'NONE', *, *, #67184, .F. ) ;
#4635 = DIRECTION ( 'NONE',  ( 0.000000000000000000, 0.000000000000000000, -1.000000000000000000 ) ) ;
#4636 = DIRECTION ( 'NONE',  ( -3.596772705736696467E-15, -1.000000000000000000, 0.000000000000000000 ) ) ;
#4637 = CIRCLE ( 'NONE', #44131, 1.000000000000000000 ) ;
#4638 = ORIENTED_EDGE ( 'NONE', *, *, #9454, .F. ) ;
#4639 = VECTOR ( 'NONE', #35749, 1000.000000000000000 ) ;
#4640 = DIRECTION ( 'NONE',  ( 0.000000000000000000, 0.000000000000000000, 1.000000000000000000 ) ) ;
#4641 = CARTESIAN_POINT ( 'NONE',  ( 106.4257688009193998, 0.000000000000000000, 285.9830310981789125 ) ) ;
#4642 = EDGE_LOOP ( 'NONE', ( #34547, #10846, #39368, #15040 ) ) ;
#4644 = ORIENTED_EDGE ( 'NONE', *, *, #59158, .T. ) ;
#4643 = CARTESIAN_POINT ( 'NONE',  ( 0.7669999999999959073, 0.000000000000000000, 0.000000000000000000 ) ) ;
#4645 = AXIS2_PLACEMENT_3D ( 'NONE', #40648, #2467, #41346 ) ;
#4646 = CARTESIAN_POINT ( 'NONE',  ( 3.430747519065335815, 7.839518282750141509, 455.0000000000000568 ) ) ;
#4647 = EDGE_CURVE ( 'NONE', #55229, #2503, #3212, .T. ) ;
#4648 = DIRECTION ( 'NONE',  ( 0.000000000000000000, 1.000000000000000000, 0.000000000000000000 ) ) ;
#4649 = FACE_BOUND ( 'NONE', #66272, .T. ) ;
#4650 = LINE ( 'NONE', #9603, #60613 ) ;
#4651 = AXIS2_PLACEMENT_3D ( 'NONE', #38676, #27379, #506 ) ;
#4652 = CIRCLE ( 'NONE', #24973, 0.5999999999999998668 ) ;
#4653 = FACE_OUTER_BOUND ( 'NONE', #56511, .T. ) ;
#4654 = EDGE_CURVE ( 'NONE', #53071, #58452, #58195, .T. ) ;
#4655 = DIRECTION ( 'NONE',  ( 1.000000000000000000, -0.000000000000000000, 0.000000000000000000 ) ) ;
#4656 = EDGE_LOOP ( 'NONE', ( #51797, #21497, #10771, #16036, #186 ) ) ;
#4657 = DIRECTION ( 'NONE',  ( 1.000000000000000000, 0.000000000000000000, 0.000000000000000000 ) ) ;
#4659 = ORIENTED_EDGE ( 'NONE', *, *, #40983, .F. ) ;
#4658 = SURFACE_STYLE_USAGE ( .BOTH. , #53108 ) ;
#4660 = CARTESIAN_POINT ( 'NONE',  ( -5.993516549646776603, -6.006483450353426790, 455.0000000000000568 ) ) ;
#4661 = LINE ( 'NONE', #47432, #27893 ) ;
#4662 = EDGE_CURVE ( 'NONE', #26479, #17661, #18399, .T. ) ;
#4663 = DIRECTION ( 'NONE',  ( 0.000000000000000000, 0.000000000000000000, -1.000000000000000000 ) ) ;
#4664 = AXIS2_PLACEMENT_3D ( 'NONE', #46465, #14648, #68042 ) ;
#4665 = ORIENTED_EDGE ( 'NONE', *, *, #30439, .F. ) ;
#4666 = DIRECTION ( 'NONE',  ( -1.000000000000000000, 0.000000000000000000, 0.000000000000000000 ) ) ;
#4667 = FACE_OUTER_BOUND ( 'NONE', #68562, .T. ) ;
#4668 = ADVANCED_FACE ( 'NONE', ( #41385 ), #8497, .F. ) ;
#4669 = EDGE_LOOP ( 'NONE', ( #22113, #32249, #4389, #36307 ) ) ;
#4670 = DIRECTION ( 'NONE',  ( 0.000000000000000000, 0.000000000000000000, 1.000000000000000000 ) ) ;
#4671 =( LENGTH_UNIT ( ) NAMED_UNIT ( * ) SI_UNIT ( .MILLI., .METRE. ) );
#4672 = FACE_OUTER_BOUND ( 'NONE', #26852, .T. ) ;
#4673 = ORIENTED_EDGE ( 'NONE', *, *, #15062, .T. ) ;
#4674 = EDGE_CURVE ( 'NONE', #4323, #44422, #46876, .T. ) ;
#4675 = FACE_OUTER_BOUND ( 'NONE', #2618, .T. ) ;
#4676 = ORIENTED_EDGE ( 'NONE', *, *, #56521, .F. ) ;
#4677 = ORIENTED_EDGE ( 'NONE', *, *, #2803, .F. ) ;
#4678 = CARTESIAN_POINT ( 'NONE',  ( 5.257023737882801306, 5.242976262117200470, 54.00000000000000711 ) ) ;
#4679 = DIRECTION ( 'NONE',  ( 0.000000000000000000, 1.000000000000000000, 0.000000000000000000 ) ) ;
#4680 = CARTESIAN_POINT ( 'NONE',  ( -11.00000000000000000, -17.14999999999900027, -26.64999999999900027 ) ) ;
#4681 = CARTESIAN_POINT ( 'NONE',  ( 15.50000000000000000, -17.50000000000000000, 22.50000000000000000 ) ) ;
#4682 = VERTEX_POINT ( 'NONE', #29367 ) ;
#4683 = EDGE_CURVE ( 'NONE', #33316, #35467, #50938, .T. ) ;
#4684 = ORIENTED_EDGE ( 'NONE', *, *, #39373, .T. ) ;
#4685 = AXIS2_PLACEMENT_3D ( 'NONE', #22389, #43935, #26996 ) ;
#4687 = ORIENTED_EDGE ( 'NONE', *, *, #34281, .T. ) ;
#4686 = PLANE ( 'NONE',  #30633 ) ;
#4689 = VERTEX_POINT ( 'NONE', #45625 ) ;
#4688 = ADVANCED_FACE ( 'NONE', ( #46336 ), #24779, .T. ) ;
#4690 = CIRCLE ( 'NONE', #46410, 1.000000000000000888 ) ;
#4691 = LINE ( 'NONE', #64783, #21349 ) ;
#4692 = CARTESIAN_POINT ( 'NONE',  ( 8.249999999999996447, -7.848062532927998269, 5.000000000000000000 ) ) ;
#4693 = CARTESIAN_POINT ( 'NONE',  ( -11.00000000000000000, -15.46862696659690073, 14.50000000000000000 ) ) ;
#4694 = LINE ( 'NONE', #10348, #27765 ) ;
#4696 = FACE_OUTER_BOUND ( 'NONE', #4721, .T. ) ;
#4695 = DIRECTION ( 'NONE',  ( 0.000000000000000000, 0.000000000000000000, -1.000000000000000000 ) ) ;
#4697 = ORIENTED_EDGE ( 'NONE', *, *, #41343, .T. ) ;
#4698 = VERTEX_POINT ( 'NONE', #40338 ) ;
#4699 = ADVANCED_FACE ( 'NONE', ( #24430 ), #19462, .T. ) ;
#4700 = EDGE_LOOP ( 'NONE', ( #17136, #9793 ) ) ;
#4701 = EDGE_LOOP ( 'NONE', ( #11092, #8591, #13126, #47125 ) ) ;
#4702 = AXIS2_PLACEMENT_3D ( 'NONE', #4859, #15811, #10157 ) ;
#4703 = CLOSED_SHELL ( 'NONE', ( #20308, #65639, #64798, #26382, #9854, #18775, #21464, #38650, #4716, #57354, #54283, #67592, #35845, #61503, #54406, #44138, #27674, #13355, #14310, #34419, #13084, #15592, #46934, #3714, #39287, #11540, #38173, #12032, #41110, #21331, #54486, #19255, #25332, #52895, #30048, #34138, #2962, #60131, #28061, #30259, #53163, #52738, #2720, #30835, #6018, #25811, #53129, #53605, #34182, #35937, #34718, #52715, #58899, #29466, #13092, #16229, #20845, #44403, #41047, #18547, #7696, #38697, #59078, #42656, #17326, #4668, #7008, #38456, #9606, #42053, #61641, #34318, #37496, #4885, #2147, #49045, #22612, #33529, #25573, #18239, #32648, #11650, #57656, #5990, #57754, #22181, #18528, #34974, #27088, #40558, #6020, #58643, #33616, #56199, #20299, #48962, #61149, #14398, #17255, #18056, #45916, #42003, #15549, #10302, #63149, #44759, #16878, #18378, #43352, #21694, #8541, #20803, #24053, #5824, #9061, #21598, #35516, #6532, #43809, #60116, #10289, #40766, #18997, #24847, #57740, #38749, #16246, #57953, #52234, #65532, #54487, #66366, #46087, #4893, #58789, #38045, #48376, #28018, #11634, #66283, #39949, #4262, #1172, #37696, #19824, #13134, #27443, #46343, #58381, #56610, #2975, #20018, #15681, #51896, #58704, #9561, #17767, #56690, #31585, #29212, #14165, #64611, #65052, #32106, #43563, #9934, #36157, #25821, #37627, #51488, #40469, #66826, #67308, #67343, #781, #11818, #14286, #1610, #15682, #37697, #12251, #67143, #25009, #50472, #53107, #43187, #61462, #38732, #3975, #23647, #25237, #11603, #7418, #57512, #66134, #13854, #57813, #38489, #8528, #36599, #46493, #53745, #64787, #11015, #2163, #21199, #25469, #29789, #19410, #14131, #13902, #15032, #13283, #65833, #63423, #30521, #24311, #48612, #68333, #24232, #24553, #19651, #13345, #48030, #44865, #65573, #33474, #48810, #54860, #38747, #21190, #60681, #24188, #15937, #33678, #35125, #23353, #42594, #52321, #10770, #25289, #25703, #15797, #22131, #68354, #14266, #56063, #45413, #16745, #36410, #61603, #15477, #59260, #10341, #44804, #579, #46091, #15187, #69014, #12062, #29018, #54202, #6634, #42339, #24757, #61206, #42094, #41568, #59166, #54365, #69966, #55412, #63452, #68829, #62584, #58377, #65496, #52630, #23520, #63665, #27033, #44617, #18563, #37896, #16795, #43108, #50168, #13740, #19522, #36734, #62030, #39816, #1885, #46789, #46958, #59632, #12521, #9735, #23160, #48327, #22984, #63474, #1109, #53624, #43459, #21657, #21338, #64692, #68870, #26681, #40159, #3697, #59585, #67817, #629, #19003, #48432, #48190, #17460, #67423, #66077, #64302, #43219, #21270, #33232, #39056, #43771, #19221, #69317, #47988, #68793, #62559, #3836, #20198, #35398, #63639, #59649, #63919, #36195, #64771, #11572, #14922, #29286, #39300, #22928, #35011, #44912, #28047, #55261, #20836, #63060, #64772, #28762, #11655, #23836, #54150, #29293, #59739, #39559, #34529, #21224, #39189, #2242, #1154, #20543, #56673, #40318, #13496, #12513, #39781, #54422, #27965 ) ) ;
#4704 = CYLINDRICAL_SURFACE ( 'NONE', #20905, 0.5250000000000004663 ) ;
#4705 = FACE_OUTER_BOUND ( 'NONE', #53811, .T. ) ;
#4706 = VECTOR ( 'NONE', #55627, 1000.000000000000000 ) ;
#4707 = LINE ( 'NONE', #15668, #19584 ) ;
#4708 = ORIENTED_EDGE ( 'NONE', *, *, #62170, .F. ) ;
#4709 = ORIENTED_EDGE ( 'NONE', *, *, #43609, .T. ) ;
#4710 = ORIENTED_EDGE ( 'NONE', *, *, #42, .T. ) ;
#4712 = DIRECTION ( 'NONE',  ( -1.000000000000000000, 0.000000000000000000, 0.000000000000000000 ) ) ;
#4711 = AXIS2_PLACEMENT_3D ( 'NONE', #37971, #54234, #32313 ) ;
#4713 = ORIENTED_EDGE ( 'NONE', *, *, #14794, .T. ) ;
#4714 = DIRECTION ( 'NONE',  ( 0.000000000000000000, 0.000000000000000000, -1.000000000000000000 ) ) ;
#4715 = ORIENTED_EDGE ( 'NONE', *, *, #41936, .T. ) ;
#4716 = ADVANCED_FACE ( 'NONE', ( #61902 ), #46684, .F. ) ;
#4717 = ORIENTED_EDGE ( 'NONE', *, *, #5310, .F. ) ;
#4718 = PLANE ( 'NONE',  #11355 ) ;
#4720 = ORIENTED_EDGE ( 'NONE', *, *, #44326, .F. ) ;
#4719 = DIRECTION ( 'NONE',  ( 0.000000000000000000, 1.000000000000000000, 0.000000000000000000 ) ) ;
#4721 = EDGE_LOOP ( 'NONE', ( #19732, #61744, #10164, #19730, #66416, #53845, #61548, #62593, #51560, #18821, #37537, #1042 ) ) ;
#4722 = ADVANCED_FACE ( 'NONE', ( #42084 ), #31844, .T. ) ;
#4723 = DIRECTION ( 'NONE',  ( 1.000000000000000000, -0.000000000000000000, 0.000000000000000000 ) ) ;
#4724 = VECTOR ( 'NONE', #24186, 1000.000000000000000 ) ;
#4725 = DIRECTION ( 'NONE',  ( -1.000000000000000000, 0.000000000000000000, 0.000000000000000000 ) ) ;
#4726 = EDGE_CURVE ( 'NONE', #53942, #4894, #68339, .T. ) ;
#4728 = ORIENTED_EDGE ( 'NONE', *, *, #8290, .F. ) ;
#4727 = CARTESIAN_POINT ( 'NONE',  ( 274.9999999999998863, -42.00000000000005684, 26.50000000000005329 ) ) ;
#4729 = VERTEX_POINT ( 'NONE', #48096 ) ;
#4730 = CARTESIAN_POINT ( 'NONE',  ( 7.757955312929523117, -8.465062094116182934, 455.0000000000000568 ) ) ;
#4731 = FACE_OUTER_BOUND ( 'NONE', #65903, .T. ) ;
#4732 = EDGE_CURVE ( 'NONE', #36943, #29826, #5328, .T. ) ;
#4733 = CARTESIAN_POINT ( 'NONE',  ( 41.09999999999999432, -21.00000000000000000, -13.86939075806900057 ) ) ;
#4734 = CARTESIAN_POINT ( 'NONE',  ( -4.727349090213463612, 4.188533722949258298, 455.0000000000000568 ) ) ;
#4735 = CARTESIAN_POINT ( 'NONE',  ( -1.853252480934758584, 9.404046420173985510, 455.0000000000000568 ) ) ;
#4736 = EDGE_CURVE ( 'NONE', #37577, #67274, #35559, .T. ) ;
#4737 = EDGE_LOOP ( 'NONE', ( #2267, #64202, #58598, #45820 ) ) ;
#4738 = DIRECTION ( 'NONE',  ( -0.000000000000000000, 0.000000000000000000, -1.000000000000000000 ) ) ;
#4739 = ORIENTED_EDGE ( 'NONE', *, *, #44869, .T. ) ;
#4740 = CARTESIAN_POINT ( 'NONE',  ( 7.757955312929523117, -8.465062094116087010, 195.0000000000000284 ) ) ;
#4741 = AXIS2_PLACEMENT_3D ( 'NONE', #4986, #26553, #15945 ) ;
#4742 = CARTESIAN_POINT ( 'NONE',  ( 16.74999999999999289, -0.3152037684892571301, 22.25410949791978155 ) ) ;
#4743 = EDGE_CURVE ( 'NONE', #7648, #10709, #63311, .T. ) ;
#4744 = DIRECTION ( 'NONE',  ( -0.7071067811865451302, 0.7071067811865500152, 2.597868168706484541E-16 ) ) ;
#4745 = ADVANCED_FACE ( 'NONE', ( #14873 ), #32179, .F. ) ;
#4746 = FACE_OUTER_BOUND ( 'NONE', #9273, .T. ) ;
#4747 = LINE ( 'NONE', #31626, #937 ) ;
#4748 = EDGE_CURVE ( 'NONE', #3096, #42177, #31495, .T. ) ;
#4750 = EDGE_CURVE ( 'NONE', #3676, #21914, #21568, .T. ) ;
#4749 = CIRCLE ( 'NONE', #33006, 24.99999999998789946 ) ;
#4751 = ADVANCED_FACE ( 'NONE', ( #59396 ), #10267, .F. ) ;
#4752 = AXIS2_PLACEMENT_3D ( 'NONE', #8304, #33186, #18568 ) ;
#4753 = ORIENTED_EDGE ( 'NONE', *, *, #33031, .T. ) ;
#4754 = CARTESIAN_POINT ( 'NONE',  ( 11.00000000000000000, -15.97213595500069871, -14.50000000000000000 ) ) ;
#4755 =( NAMED_UNIT ( * ) SI_UNIT ( $, .STERADIAN. ) SOLID_ANGLE_UNIT ( ) );
#4756 = EDGE_CURVE ( 'NONE', #21542, #41212, #66217, .T. ) ;
#4757 = FACE_OUTER_BOUND ( 'NONE', #3325, .T. ) ;
#4758 = ORIENTED_EDGE ( 'NONE', *, *, #22470, .T. ) ;
#4759 = DIRECTION ( 'NONE',  ( 1.000000000000000000, -5.981805089575196197E-17, 0.000000000000000000 ) ) ;
#4760 = CARTESIAN_POINT ( 'NONE',  ( 7.000000000000000000, -25.50000000000000355, -14.74860679774999994 ) ) ;
#4761 = CARTESIAN_POINT ( 'NONE',  ( 7.811466277050736373, -4.740315990920255018, 455.0000000000000568 ) ) ;
#4762 = AXIS2_PLACEMENT_3D ( 'NONE', #61497, #44544, #60812 ) ;
#4763 = CARTESIAN_POINT ( 'NONE',  ( 9.912023737882815766, -3.857023737882825820, 54.00000000000000711 ) ) ;
#4764 = CARTESIAN_POINT ( 'NONE',  ( -11.07551654964667520, 9.791916549646639822, 455.0000000000000568 ) ) ;
#4765 = EDGE_LOOP ( 'NONE', ( #60610, #67998, #59549, #68943 ) ) ;
#4766 = DIRECTION ( 'NONE',  ( 1.000000000000000000, -0.000000000000000000, -0.000000000000000000 ) ) ;
#4767 = CARTESIAN_POINT ( 'NONE',  ( 158.8349105750994568, -35.83962462487175316, 0.000000000000000000 ) ) ;
#4768 = CARTESIAN_POINT ( 'NONE',  ( 10.92648345035331303, 2.693516549646575609, 195.0000000000000284 ) ) ;
#4769 = DIRECTION ( 'NONE',  ( -1.000000000000000000, 0.000000000000000000, 0.000000000000000000 ) ) ;
#4770 = CARTESIAN_POINT ( 'NONE',  ( 10.09643294401448443, 2.693516549646584934, 195.0000000000000284 ) ) ;
#4771 = EDGE_CURVE ( 'NONE', #52692, #63059, #53408, .T. ) ;
#4772 = VERTEX_POINT ( 'NONE', #10959 ) ;
#4774 = ORIENTED_EDGE ( 'NONE', *, *, #40768, .T. ) ;
#4773 = LINE ( 'NONE', #51804, #10255 ) ;
#4775 = EDGE_CURVE ( 'NONE', #1435, #52904, #52720, .T. ) ;
#4776 = CARTESIAN_POINT ( 'NONE',  ( 11.78648345035337819, -7.826483450353491023, 455.0000000000000568 ) ) ;
#4777 = DIRECTION ( 'NONE',  ( 1.000000000000000000, 0.000000000000000000, 0.000000000000000000 ) ) ;
#4778 = DIRECTION ( 'NONE',  ( -0.000000000000000000, 3.673940397442059868E-16, -1.000000000000000000 ) ) ;
#4779 = ORIENTED_EDGE ( 'NONE', *, *, #2638, .F. ) ;
#4780 = CARTESIAN_POINT ( 'NONE',  ( -9.547976262117254365, 2.355476262117183417, 54.00000000000000711 ) ) ;
#4781 = CARTESIAN_POINT ( 'NONE',  ( 14.50000000000000000, -0.5000000000000000000, 27.00000000000000000 ) ) ;
#4782 = CIRCLE ( 'NONE', #2481, 0.1999999999999987899 ) ;
#4783 = ORIENTED_EDGE ( 'NONE', *, *, #13263, .T. ) ;
#4784 = VERTEX_POINT ( 'NONE', #68620 ) ;
#4785 = ORIENTED_EDGE ( 'NONE', *, *, #63798, .F. ) ;
#4786 = VECTOR ( 'NONE', #58656, 1000.000000000000000 ) ;
#4787 = DIRECTION ( 'NONE',  ( 0.000000000000000000, 1.000000000000000000, 0.000000000000000000 ) ) ;
#4788 = DIRECTION ( 'NONE',  ( -1.000000000000000000, 0.000000000000000000, 0.000000000000000000 ) ) ;
#4789 = CYLINDRICAL_SURFACE ( 'NONE', #57379, 0.2000000000000005107 ) ;
#4790 = ORIENTED_EDGE ( 'NONE', *, *, #31297, .F. ) ;
#4791 = ORIENTED_EDGE ( 'NONE', *, *, #9033, .F. ) ;
#4792 = CIRCLE ( 'NONE', #42031, 0.3499999999998879008 ) ;
#4793 = LINE ( 'NONE', #62781, #68911 ) ;
#4794 = ORIENTED_EDGE ( 'NONE', *, *, #23519, .T. ) ;
#4795 = VERTEX_POINT ( 'NONE', #37490 ) ;
#4796 = VECTOR ( 'NONE', #11796, 1000.000000000000000 ) ;
#4797 = ORIENTED_EDGE ( 'NONE', *, *, #29392, .F. ) ;
#4798 = EDGE_LOOP ( 'NONE', ( #14111, #15823, #10542, #22744 ) ) ;
#4799 = DIRECTION ( 'NONE',  ( -1.836970198721029934E-16, -1.836970198721010706E-16, 1.000000000000000000 ) ) ;
#4800 = UNCERTAINTY_MEASURE_WITH_UNIT (LENGTH_MEASURE( 1.000000000000000082E-05 ), #66052, 'distance_accuracy_value', 'NONE');
#4802 = ORIENTED_EDGE ( 'NONE', *, *, #41907, .T. ) ;
#4801 = LINE ( 'NONE', #30276, #7386 ) ;
#4803 = ADVANCED_FACE ( 'NONE', ( #10603 ), #58709, .T. ) ;
#4804 = FACE_OUTER_BOUND ( 'NONE', #58913, .T. ) ;
#4806 = CARTESIAN_POINT ( 'NONE',  ( 0.000000000000000000, 8.250000000000001776, -19.50000000000000000 ) ) ;
#4805 = AXIS2_PLACEMENT_3D ( 'NONE', #5821, #42943, #47897 ) ;
#4807 = DIRECTION ( 'NONE',  ( 0.000000000000000000, 0.7096009616570518874, 0.7046037717862339012 ) ) ;
#4808 = ORIENTED_EDGE ( 'NONE', *, *, #66111, .F. ) ;
#4809 = EDGE_CURVE ( 'NONE', #14583, #45832, #8, .T. ) ;
#4810 = ORIENTED_EDGE ( 'NONE', *, *, #67802, .T. ) ;
#4811 = VECTOR ( 'NONE', #41250, 1000.000000000000114 ) ;
#4812 = EDGE_CURVE ( 'NONE', #44524, #27495, #16307, .T. ) ;
#4813 = DIRECTION ( 'NONE',  ( 0.000000000000000000, 1.000000000000000000, 0.000000000000000000 ) ) ;
#4814 = EDGE_CURVE ( 'NONE', #20264, #56954, #57998, .T. ) ;
#4815 = DIRECTION ( 'NONE',  ( 0.000000000000000000, 1.000000000000000000, 0.000000000000000000 ) ) ;
#4816 = VERTEX_POINT ( 'NONE', #64698 ) ;
#4817 = VECTOR ( 'NONE', #3230, 1000.000000000000000 ) ;
#4818 = CARTESIAN_POINT ( 'NONE',  ( 72.77321854994619343, 47.95351654967443977, 26.00000000000000355 ) ) ;
#4819 = DIRECTION ( 'NONE',  ( 0.000000000000000000, 0.000000000000000000, -1.000000000000000000 ) ) ;
#4820 = LINE ( 'NONE', #54922, #51388 ) ;
#4821 = ORIENTED_EDGE ( 'NONE', *, *, #55596, .T. ) ;
#4822 = CARTESIAN_POINT ( 'NONE',  ( -7.450000000000001954, -7.249999999999998224, -25.50000000000000355 ) ) ;
#4823 = DIRECTION ( 'NONE',  ( -1.000000000000000000, 7.304098846218132892E-15, -0.000000000000000000 ) ) ;
#4824 = CARTESIAN_POINT ( 'NONE',  ( 14.50000000000000000, 0.000000000000000000, -26.50000000000000000 ) ) ;
#4825 = CARTESIAN_POINT ( 'NONE',  ( 2.906483450353417375, 10.08346604330775875, 455.0000000000000568 ) ) ;
#4826 = VECTOR ( 'NONE', #4840, 1000.000000000000000 ) ;
#4827 = EDGE_CURVE ( 'NONE', #30457, #25912, #36797, .T. ) ;
#4828 = DIRECTION ( 'NONE',  ( 0.000000000000000000, 0.000000000000000000, 1.000000000000000000 ) ) ;
#4829 = ORIENTED_EDGE ( 'NONE', *, *, #62195, .T. ) ;
#4830 = LINE ( 'NONE', #58920, #59553 ) ;
#4831 = DIRECTION ( 'NONE',  ( -0.000000000000000000, 1.000000000000000000, -0.000000000000000000 ) ) ;
#4832 = VECTOR ( 'NONE', #64916, 999.9999999999998863 ) ;
#4833 = CARTESIAN_POINT ( 'NONE',  ( 7.450000000000006395, 7.250000000000000888, -17.00000000000000000 ) ) ;
#4834 = FACE_OUTER_BOUND ( 'NONE', #14785, .T. ) ;
#4835 = VERTEX_POINT ( 'NONE', #6679 ) ;
#4836 = CARTESIAN_POINT ( 'NONE',  ( 283.0000000000000568, -20.40000000000000213, -17.60000000000000142 ) ) ;
#4837 = DIRECTION ( 'NONE',  ( -0.000000000000000000, -1.000000000000000000, 0.000000000000000000 ) ) ;
#4838 = VECTOR ( 'NONE', #14518, 1000.000000000000000 ) ;
#4839 = CARTESIAN_POINT ( 'NONE',  ( 6.836383711243005479, -6.364920264886905876, 54.00000000000000711 ) ) ;
#4840 = DIRECTION ( 'NONE',  ( -0.000000000000000000, -0.000000000000000000, -1.000000000000000000 ) ) ;
#4841 = ORIENTED_EDGE ( 'NONE', *, *, #4935, .T. ) ;
#4842 = LINE ( 'NONE', #36308, #45647 ) ;
#4843 = DIRECTION ( 'NONE',  ( -1.000000000000000000, 0.000000000000000000, 0.000000000000000000 ) ) ;
#4844 = CARTESIAN_POINT ( 'NONE',  ( -4.135079735113167843, 6.822336235477362010, 54.00000000000000711 ) ) ;
#4845 = FACE_BOUND ( 'NONE', #37652, .T. ) ;
#4846 = CARTESIAN_POINT ( 'NONE',  ( -4.383466043307858939, 8.593516549646588842, 195.0000000000000284 ) ) ;
#4847 = EDGE_CURVE ( 'NONE', #52241, #42601, #43472, .T. ) ;
#4848 = ORIENTED_EDGE ( 'NONE', *, *, #60594, .F. ) ;
#4849 = EDGE_CURVE ( 'NONE', #47832, #66711, #24222, .T. ) ;
#4850 = AXIS2_PLACEMENT_3D ( 'NONE', #46496, #68070, #57107 ) ;
#4851 = ORIENTED_EDGE ( 'NONE', *, *, #23641, .T. ) ;
#4852 = CARTESIAN_POINT ( 'NONE',  ( 8.093267424590459669, 8.697938382363064491, 54.00000000000000711 ) ) ;
#4853 = FACE_BOUND ( 'NONE', #62401, .T. ) ;
#4854 = ORIENTED_EDGE ( 'NONE', *, *, #60336, .F. ) ;
#4855 = EDGE_CURVE ( 'NONE', #14910, #35722, #6345, .T. ) ;
#4856 = DIRECTION ( 'NONE',  ( 0.000000000000000000, -5.800915303574361727E-12, -1.000000000000000000 ) ) ;
#4857 = VECTOR ( 'NONE', #40201, 1000.000000000000114 ) ;
#4858 = AXIS2_PLACEMENT_3D ( 'NONE', #36671, #21111, #20403 ) ;
#4859 = CARTESIAN_POINT ( 'NONE',  ( -15.50000000000000000, -0.2000000000000000111, -22.50000000000000000 ) ) ;
#4860 = VERTEX_POINT ( 'NONE', #48791 ) ;
#4861 = CARTESIAN_POINT ( 'NONE',  ( -7.450000000000001954, 7.250000000000000000, -14.50000000000000000 ) ) ;
#4862 = ORIENTED_EDGE ( 'NONE', *, *, #50829, .F. ) ;
#4863 = AXIS2_PLACEMENT_3D ( 'NONE', #10909, #32487, #38142 ) ;
#4864 = ORIENTED_EDGE ( 'NONE', *, *, #24056, .T. ) ;
#4865 = LINE ( 'NONE', #69572, #17057 ) ;
#4866 = EDGE_LOOP ( 'NONE', ( #2767, #54818, #65620, #28844 ) ) ;
#4867 = CARTESIAN_POINT ( 'NONE',  ( 4.201500623656053257, 4.727349090213338378, 455.0000000000000568 ) ) ;
#4868 = DIRECTION ( 'NONE',  ( -1.000000000000000000, 0.000000000000000000, 0.000000000000000000 ) ) ;
#4869 = CARTESIAN_POINT ( 'NONE',  ( -1.466476262117324181, -9.404523737882843903, 54.00000000000000711 ) ) ;
#4870 = CARTESIAN_POINT ( 'NONE',  ( 11.32648345035340398, 7.593516549646563085, 455.0000000000000568 ) ) ;
#4871 = ORIENTED_EDGE ( 'NONE', *, *, #29362, .F. ) ;
#4872 = VERTEX_POINT ( 'NONE', #27561 ) ;
#4873 = LINE ( 'NONE', #30696, #65130 ) ;
#4875 = DIRECTION ( 'NONE',  ( 1.836970198721029934E-16, 1.836970198721010706E-16, -1.000000000000000000 ) ) ;
#4874 = CARTESIAN_POINT ( 'NONE',  ( -7.250000000000000888, 7.250000000000001776, -21.50000000000000000 ) ) ;
#4876 = ORIENTED_EDGE ( 'NONE', *, *, #44012, .F. ) ;
#4877 = CIRCLE ( 'NONE', #64679, 1.000000000000002665 ) ;
#4878 = ORIENTED_EDGE ( 'NONE', *, *, #66902, .F. ) ;
#4880 = VERTEX_POINT ( 'NONE', #33892 ) ;
#4879 = ITEM_DEFINED_TRANSFORMATION ( 'NONE', 'NONE', #21155,  #45918 ) ;
#4881 = FACE_OUTER_BOUND ( 'NONE', #68791, .T. ) ;
#4882 = AXIS2_PLACEMENT_3D ( 'NONE', #40466, #62024, #2998 ) ;
#4884 = EDGE_LOOP ( 'NONE', ( #48792, #45078, #51432, #22386 ) ) ;
#4883 = PLANE ( 'NONE',  #51141 ) ;
#4885 = ADVANCED_FACE ( 'NONE', ( #17975 ), #11626, .F. ) ;
#4886 = CARTESIAN_POINT ( 'NONE',  ( 30.00000000000000000, -9.487228132326899654, 12.50000000000000000 ) ) ;
#4887 = LINE ( 'NONE', #58632, #36254 ) ;
#4888 = ORIENTED_EDGE ( 'NONE', *, *, #59801, .T. ) ;
#4889 = ORIENTED_EDGE ( 'NONE', *, *, #27630, .T. ) ;
#4890 = AXIS2_PLACEMENT_3D ( 'NONE', #44852, #18676, #28250 ) ;
#4891 = PLANE ( 'NONE',  #31265 ) ;
#4892 = EDGE_CURVE ( 'NONE', #8722, #62416, #54787, .T. ) ;
#4893 = ADVANCED_FACE ( 'NONE', ( #49819 ), #55817, .F. ) ;
#4894 = VERTEX_POINT ( 'NONE', #60079 ) ;
#4895 = PLANE ( 'NONE',  #47185 ) ;
#4896 = LINE ( 'NONE', #27156, #46927 ) ;
#4897 = EDGE_CURVE ( 'NONE', #60569, #67306, #1050, .T. ) ;
#4898 = CARTESIAN_POINT ( 'NONE',  ( -10.03972626211731445, -8.930623737882747548, 26.00000000000000000 ) ) ;
#4899 = EDGE_CURVE ( 'NONE', #46497, #39124, #22015, .T. ) ;
#4900 = EDGE_LOOP ( 'NONE', ( #7180, #16964, #36523, #34985 ) ) ;
#4901 = AXIS2_PLACEMENT_3D ( 'NONE', #51732, #3286, #14594 ) ;
#4902 = EDGE_CURVE ( 'NONE', #2503, #29317, #50208, .T. ) ;
#4903 = CARTESIAN_POINT ( 'NONE',  ( 3.157023737882809655, -6.501044194225470640, 26.00000000000000711 ) ) ;
#4905 = VERTEX_POINT ( 'NONE', #44161 ) ;
#4904 = DIRECTION ( 'NONE',  ( 0.000000000000000000, 0.000000000000000000, -1.000000000000000000 ) ) ;
#4906 = EDGE_LOOP ( 'NONE', ( #12626, #1695, #33315, #22611 ) ) ;
#4907 = LINE ( 'NONE', #59340, #52408 ) ;
#4908 = AXIS2_PLACEMENT_3D ( 'NONE', #3713, #12899, #30583 ) ;
#4910 = AXIS2_PLACEMENT_3D ( 'NONE', #1138, #65827, #17381 ) ;
#4909 = CARTESIAN_POINT ( 'NONE',  ( 30.00000000000000000, -10.85999999999999943, 9.000000000000001776 ) ) ;
#4911 = CARTESIAN_POINT ( 'NONE',  ( 8.711985858128693749, -2.420780051175180692, 54.00000000000000711 ) ) ;
#4912 = CARTESIAN_POINT ( 'NONE',  ( -25.50000000000000355, -5.578999999999999737, -22.50000000000000000 ) ) ;
#4913 = MECHANICAL_DESIGN_GEOMETRIC_PRESENTATION_REPRESENTATION (  '', ( #11648 ), #35370 ) ;
#4914 = AXIS2_PLACEMENT_3D ( 'NONE', #16826, #38392, #59950 ) ;
#4915 = CARTESIAN_POINT ( 'NONE',  ( 2.706483450353343478, -10.92648345035336632, 195.0000000000000284 ) ) ;
#4916 = VERTEX_POINT ( 'NONE', #43826 ) ;
#4917 = CARTESIAN_POINT ( 'NONE',  ( 106.4257688009193430, 0.000000000000000000, 330.9830310981789694 ) ) ;
#4918 = CARTESIAN_POINT ( 'NONE',  ( -7.798499376344109280, -4.740315990920159095, 455.0000000000000568 ) ) ;
#4919 = CARTESIAN_POINT ( 'NONE',  ( 275.0000000000000000, -25.50000000000000355, 17.00000000000000000 ) ) ;
#4921 = ORIENTED_EDGE ( 'NONE', *, *, #21919, .T. ) ;
#4920 = CARTESIAN_POINT ( 'NONE',  ( -7.250000000000000888, -8.249999999999998224, -17.00000000000000000 ) ) ;
#4922 = DIRECTION ( 'NONE',  ( -1.000000000000000000, 0.000000000000000000, 0.000000000000000000 ) ) ;
#4923 = DIRECTION ( 'NONE',  ( 0.000000000000000000, 0.000000000000000000, -1.000000000000000000 ) ) ;
#4924 = CARTESIAN_POINT ( 'NONE',  ( -3.663616288757091333, -4.149127210878728711, 54.00000000000000711 ) ) ;
#4925 = CARTESIAN_POINT ( 'NONE',  ( -7.342976262117259623, 5.538810540049946773, 54.00000000000000711 ) ) ;
#4926 = VERTEX_POINT ( 'NONE', #59743 ) ;
#4927 = CARTESIAN_POINT ( 'NONE',  ( -30.00000000000000000, -14.04000000000000092, -17.04524521594300523 ) ) ;
#4928 = CARTESIAN_POINT ( 'NONE',  ( -0.9414762621172296786, 9.390476262117148920, 54.00000000000000711 ) ) ;
#4929 = AXIS2_PLACEMENT_3D ( 'NONE', #44564, #12044, #35973 ) ;
#4930 = ORIENTED_EDGE ( 'NONE', *, *, #64219, .F. ) ;
#4931 = LINE ( 'NONE', #26853, #19837 ) ;
#4932 = PLANE ( 'NONE',  #18642 ) ;
#4933 = CARTESIAN_POINT ( 'NONE',  ( 10.20488345035345290, 9.791916549646566992, 455.0000000000000568 ) ) ;
#4934 = PLANE ( 'NONE',  #51985 ) ;
#4935 = EDGE_CURVE ( 'NONE', #66583, #42686, #65057, .T. ) ;
#4936 = LINE ( 'NONE', #5634, #18296 ) ;
#4937 = ORIENTED_EDGE ( 'NONE', *, *, #54203, .F. ) ;
#4938 = ORIENTED_EDGE ( 'NONE', *, *, #16792, .T. ) ;
#4939 = DIRECTION ( 'NONE',  ( -1.000000000000000000, 0.000000000000000000, 0.000000000000000000 ) ) ;
#4940 = VERTEX_POINT ( 'NONE', #27917 ) ;
#4941 = ORIENTED_EDGE ( 'NONE', *, *, #15528, .F. ) ;
#4942 = EDGE_CURVE ( 'NONE', #16354, #53017, #49167, .T. ) ;
#4943 = CARTESIAN_POINT ( 'NONE',  ( 15.50000000000000000, -0.2000000000000000111, -22.50000000000000000 ) ) ;
#4944 = EDGE_CURVE ( 'NONE', #36995, #4210, #2862, .T. ) ;
#4945 = ADVANCED_FACE ( 'NONE', ( #1382, #22943 ), #16625, .T. ) ;
#4946 = CARTESIAN_POINT ( 'NONE',  ( -7.450000000000001954, 7.250000000000000000, -11.50000000000000000 ) ) ;
#4947 = CARTESIAN_POINT ( 'NONE',  ( 7.826483450353374671, 11.99351654964662295, 195.0000000000000284 ) ) ;
#4948 = EDGE_LOOP ( 'NONE', ( #20658, #4302, #61906, #5545 ) ) ;
#4949 = ORIENTED_EDGE ( 'NONE', *, *, #35078, .F. ) ;
#4950 = LINE ( 'NONE', #26515, #12493 ) ;
#4951 = ORIENTED_EDGE ( 'NONE', *, *, #29385, .T. ) ;
#4952 = VERTEX_POINT ( 'NONE', #38528 ) ;
#4953 = CARTESIAN_POINT ( 'NONE',  ( 15.50000000000000000, -0.2038245569916610489, -23.94337567297399971 ) ) ;
#4954 = CARTESIAN_POINT ( 'NONE',  ( 88.07321854994620480, 47.95351654967443977, 40.00000000000000000 ) ) ;
#4955 = AXIS2_PLACEMENT_3D ( 'NONE', #30477, #56301, #52052 ) ;
#4956 = AXIS2_PLACEMENT_3D ( 'NONE', #23195, #23543, #12571 ) ;
#4957 = DIRECTION ( 'NONE',  ( -2.135044278125301343E-15, 1.000000000000000000, 0.000000000000000000 ) ) ;
#4958 = VERTEX_POINT ( 'NONE', #16960 ) ;
#4959 = PLANE ( 'NONE',  #22165 ) ;
#4961 = DIRECTION ( 'NONE',  ( 0.000000000000000000, 0.000000000000000000, 1.000000000000000000 ) ) ;
#4960 = LINE ( 'NONE', #59742, #68256 ) ;
#4962 = AXIS2_PLACEMENT_3D ( 'NONE', #39357, #27378, #12472 ) ;
#4964 = ORIENTED_EDGE ( 'NONE', *, *, #28113, .T. ) ;
#4963 = AXIS2_PLACEMENT_3D ( 'NONE', #57244, #51233, #29307 ) ;
#4966 = EDGE_LOOP ( 'NONE', ( #35996, #16475, #56923, #27003 ) ) ;
#4965 = CARTESIAN_POINT ( 'NONE',  ( 6.006483450353379716, -6.006483450353490738, 455.0000000000000568 ) ) ;
#4967 = ORIENTED_EDGE ( 'NONE', *, *, #64706, .F. ) ;
#4968 = CIRCLE ( 'NONE', #50110, 1.000000000000000000 ) ;
#4969 = AXIS2_PLACEMENT_3D ( 'NONE', #51304, #34326, #61201 ) ;
#4970 = CARTESIAN_POINT ( 'NONE',  ( -25.49999999999869971, -15.50000000000000000, -22.50000000000000000 ) ) ;
#4971 = LINE ( 'NONE', #26536, #2183 ) ;
#4972 = ORIENTED_EDGE ( 'NONE', *, *, #1163, .T. ) ;
#4973 = CARTESIAN_POINT ( 'NONE',  ( 8.711985858128693749, -8.093267424590470327, 54.00000000000000711 ) ) ;
#4974 = LINE ( 'NONE', #16974, #2969 ) ;
#4975 = ORIENTED_EDGE ( 'NONE', *, *, #12525, .T. ) ;
#4976 = ORIENTED_EDGE ( 'NONE', *, *, #50896, .F. ) ;
#4977 = DIRECTION ( 'NONE',  ( 0.000000000000000000, -0.7071067811865496822, 0.7071067811865454633 ) ) ;
#4978 = CARTESIAN_POINT ( 'NONE',  ( 15.50000000000000000, -17.50000000000000000, -25.99999999999985079 ) ) ;
#4979 = DIRECTION ( 'NONE',  ( -1.000000000000000000, 0.000000000000000000, 0.000000000000000000 ) ) ;
#4980 = EDGE_CURVE ( 'NONE', #5469, #51099, #11291, .T. ) ;
#4981 = ORIENTED_EDGE ( 'NONE', *, *, #49669, .T. ) ;
#4982 = EDGE_CURVE ( 'NONE', #17940, #67565, #23287, .T. ) ;
#4983 = CARTESIAN_POINT ( 'NONE',  ( -1.853252480934758584, 9.404046420173985510, 455.0000000000000568 ) ) ;
#4984 = DIRECTION ( 'NONE',  ( -1.000000000000000000, 0.000000000000000000, 0.000000000000000000 ) ) ;
#4985 = EDGE_CURVE ( 'NONE', #68576, #22889, #32872, .T. ) ;
#4987 = ORIENTED_EDGE ( 'NONE', *, *, #60049, .T. ) ;
#4986 = CARTESIAN_POINT ( 'NONE',  ( -8.593516549646711411, 4.383466043307770121, 455.0000000000000568 ) ) ;
#4989 = ORIENTED_EDGE ( 'NONE', *, *, #21980, .T. ) ;
#4988 = DIRECTION ( 'NONE',  ( 0.000000000000000000, 0.000000000000000000, -1.000000000000000000 ) ) ;
#4990 = DIRECTION ( 'NONE',  ( 0.000000000000000000, 0.000000000000000000, -1.000000000000000000 ) ) ;
#4991 = CARTESIAN_POINT ( 'NONE',  ( 6.849523737882814878, 10.49297626211720136, 26.00000000000000711 ) ) ;
#4992 = STYLED_ITEM ( 'NONE', ( #39934 ), #21524 ) ;
#4993 = CARTESIAN_POINT ( 'NONE',  ( 7.000000000000000000, -31.30000000000045191, -8.900000000000430234 ) ) ;
#4994 = CARTESIAN_POINT ( 'NONE',  ( -2.530476262117318242, -8.835729544836354421, 54.00000000000000711 ) ) ;
#4995 = DIRECTION ( 'NONE',  ( 0.000000000000000000, 0.000000000000000000, -1.000000000000000000 ) ) ;
#4996 = LINE ( 'NONE', #36839, #63151 ) ;
#4997 = VERTEX_POINT ( 'NONE', #29988 ) ;
#4998 = CYLINDRICAL_SURFACE ( 'NONE', #56408, 0.5000000000009441337 ) ;
#4999 = ADVANCED_FACE ( 'NONE', ( #56508 ), #7712, .T. ) ;
#5001 = ORIENTED_EDGE ( 'NONE', *, *, #32110, .F. ) ;
#5000 = DIRECTION ( 'NONE',  ( 0.000000000000000000, 0.000000000000000000, 1.000000000000000000 ) ) ;
#5002 = CARTESIAN_POINT ( 'NONE',  ( 15.50000000000000000, -1.037157890325000054, 22.50000000000000000 ) ) ;
#5003 = CIRCLE ( 'NONE', #46726, 3.500000000000000000 ) ;
#5004 = VECTOR ( 'NONE', #13984, 1000.000000000000000 ) ;
#5005 = CARTESIAN_POINT ( 'NONE',  ( -9.404046420174124066, 1.853252480934674651, 455.0000000000000568 ) ) ;
#5006 = CARTESIAN_POINT ( 'NONE',  ( 35.89999999999999858, 20.60000000000000142, 13.86939075806899702 ) ) ;
#5007 = VECTOR ( 'NONE', #66146, 1000.000000000000000 ) ;
#5008 = VECTOR ( 'NONE', #42909, 1000.000000000000000 ) ;
#5009 = ORIENTED_EDGE ( 'NONE', *, *, #1795, .T. ) ;
#5010 = CARTESIAN_POINT ( 'NONE',  ( 3.677663764522616230, 4.135079735113117216, 26.00000000000000711 ) ) ;
#5011 = DIRECTION ( 'NONE',  ( 0.7071067811865480168, 0.7071067811865470176, 0.000000000000000000 ) ) ;
#5012 = ORIENTED_EDGE ( 'NONE', *, *, #53945, .F. ) ;
#5013 = CARTESIAN_POINT ( 'NONE',  ( 105.8309041053263257, 3.657408540445008960, 2.000000000000000000 ) ) ;
#5014 = AXIS2_PLACEMENT_3D ( 'NONE', #5320, #69669, #11621 ) ;
#5015 = CARTESIAN_POINT ( 'NONE',  ( 6.836383711243005479, -4.149127210878743810, 54.00000000000000711 ) ) ;
#5016 = AXIS2_PLACEMENT_3D ( 'NONE', #34872, #66713, #18264 ) ;
#5017 = AXIS2_PLACEMENT_3D ( 'NONE', #68114, #30295, #45485 ) ;
#5018 = ORIENTED_EDGE ( 'NONE', *, *, #31637, .T. ) ;
#5019 = CARTESIAN_POINT ( 'NONE',  ( -1.620245201994373829, -8.241237374594328813, 54.00000000000000711 ) ) ;
#5020 = EDGE_LOOP ( 'NONE', ( #27987, #6673, #7293, #59754 ) ) ;
#5021 = ORIENTED_EDGE ( 'NONE', *, *, #14964, .F. ) ;
#5022 = VECTOR ( 'NONE', #5408, 1000.000000000000000 ) ;
#5023 = FACE_OUTER_BOUND ( 'NONE', #56683, .T. ) ;
#5024 = DIRECTION ( 'NONE',  ( 0.000000000000000000, 0.000000000000000000, 1.000000000000000000 ) ) ;
#5025 = ADVANCED_FACE ( 'NONE', ( #57213 ), #30344, .T. ) ;
#5026 = FACE_BOUND ( 'NONE', #9818, .T. ) ;
#5027 = CARTESIAN_POINT ( 'NONE',  ( 9.404523737882819034, -0.9555237378828257411, 54.00000000000000711 ) ) ;
#5028 = ORIENTED_EDGE ( 'NONE', *, *, #18459, .T. ) ;
#5029 = ORIENTED_EDGE ( 'NONE', *, *, #51056, .F. ) ;
#5031 = ORIENTED_EDGE ( 'NONE', *, *, #18494, .F. ) ;
#5030 = DIRECTION ( 'NONE',  ( 1.000000000000000000, -5.120954910632640039E-15, 0.000000000000000000 ) ) ;
#5032 = ORIENTED_EDGE ( 'NONE', *, *, #13681, .T. ) ;
#5033 = CARTESIAN_POINT ( 'NONE',  ( -8.250000000000001776, -7.249999999999998224, -20.00000000000000000 ) ) ;
#5034 = LINE ( 'NONE', #48871, #28661 ) ;
#5035 = CARTESIAN_POINT ( 'NONE',  ( 33.89999999999999858, 20.60000000000000142, -13.86939075806900057 ) ) ;
#5036 = AXIS2_PLACEMENT_3D ( 'NONE', #7439, #45264, #30060 ) ;
#5037 = DIRECTION ( 'NONE',  ( 0.6414496315691617934, 0.7671651518152962090, -0.000000000000000000 ) ) ;
#5038 = ADVANCED_FACE ( 'NONE', ( #51915 ), #40939, .F. ) ;
#5040 = FACE_OUTER_BOUND ( 'NONE', #27941, .T. ) ;
#5039 = CARTESIAN_POINT ( 'NONE',  ( 69.92576880110368620, 10.00000000000000000, 281.4830310981151911 ) ) ;
#5041 = ORIENTED_EDGE ( 'NONE', *, *, #57692, .T. ) ;
#5042 = ORIENTED_EDGE ( 'NONE', *, *, #23162, .F. ) ;
#5043 = VECTOR ( 'NONE', #39850, 1000.000000000000000 ) ;
#5044 = VERTEX_POINT ( 'NONE', #40242 ) ;
#5045 = VERTEX_POINT ( 'NONE', #57559 ) ;
#5046 = ADVANCED_FACE ( 'NONE', ( #40596 ), #14443, .F. ) ;
#5047 = CARTESIAN_POINT ( 'NONE',  ( 29.50000000000000355, -11.50000000000000000, -15.00000000000000000 ) ) ;
#5048 = DIRECTION ( 'NONE',  ( -1.000000000000000000, 0.000000000000000000, 0.000000000000000000 ) ) ;
#5049 = DIRECTION ( 'NONE',  ( 0.000000000000000000, 0.000000000000000000, 1.000000000000000000 ) ) ;
#5050 = AXIS2_PLACEMENT_3D ( 'NONE', #56742, #57096, #62747 ) ;
#5051 = LINE ( 'NONE', #10699, #38761 ) ;
#5052 = ORIENTED_EDGE ( 'NONE', *, *, #25202, .F. ) ;
#5053 = EDGE_LOOP ( 'NONE', ( #13814, #45545, #67410, #2512, #68724, #53831, #49420, #7440, #20352, #17005, #38027, #49410, #52425, #36063, #25547, #25850, #67607 ) ) ;
#5054 = ORIENTED_EDGE ( 'NONE', *, *, #54110, .T. ) ;
#5055 = DIRECTION ( 'NONE',  ( -0.4999999999999695244, 0.8660254037844563602, 0.000000000000000000 ) ) ;
#5056 = ORIENTED_EDGE ( 'NONE', *, *, #68198, .F. ) ;
#5057 = STYLED_ITEM ( 'NONE', ( #55543 ), #66857 ) ;
#5058 = AXIS2_PLACEMENT_3D ( 'NONE', #62334, #46083, #51384 ) ;
#5059 = FACE_OUTER_BOUND ( 'NONE', #19519, .T. ) ;
#5060 = PLANE ( 'NONE',  #34492 ) ;
#5061 = ORIENTED_EDGE ( 'NONE', *, *, #39679, .F. ) ;
#5062 = EDGE_LOOP ( 'NONE', ( #44246, #6596, #41817, #15793 ) ) ;
#5063 = DIRECTION ( 'NONE',  ( 0.000000000000000000, 0.000000000000000000, 1.000000000000000000 ) ) ;
#5064 = AXIS2_PLACEMENT_3D ( 'NONE', #41643, #31407, #20081 ) ;
#5066 = ORIENTED_EDGE ( 'NONE', *, *, #3857, .T. ) ;
#5065 = CARTESIAN_POINT ( 'NONE',  ( -15.91242688423474050, -0.3152598339554945062, -23.70526090034005051 ) ) ;
#5067 = EDGE_LOOP ( 'NONE', ( #27138, #45544, #17339, #51747, #16203 ) ) ;
#5068 = EDGE_CURVE ( 'NONE', #47329, #12465, #66765, .T. ) ;
#5069 =( GEOMETRIC_REPRESENTATION_CONTEXT ( 3 ) GLOBAL_UNCERTAINTY_ASSIGNED_CONTEXT ( ( #30274 ) ) GLOBAL_UNIT_ASSIGNED_CONTEXT ( ( #5183, #54315, #21786 ) ) REPRESENTATION_CONTEXT ( 'NONE', 'WORKASPACE' ) );
#5070 = EDGE_CURVE ( 'NONE', #325, #8276, #19375, .T. ) ;
#5071 = LINE ( 'NONE', #41503, #56213 ) ;
#5072 = EDGE_CURVE ( 'NONE', #11985, #50419, #13012, .T. ) ;
#5074 = EDGE_LOOP ( 'NONE', ( #22341, #17229, #48029, #30149 ) ) ;
#5073 = CARTESIAN_POINT ( 'NONE',  ( 169.1780563256071446, -35.83962462487175316, 5.000000000000000000 ) ) ;
#5075 = VECTOR ( 'NONE', #48095, 1000.000000000000000 ) ;
#5076 = ORIENTED_EDGE ( 'NONE', *, *, #31945, .T. ) ;
#5077 = CARTESIAN_POINT ( 'NONE',  ( -4.383466043307859827, 8.393516549646589553, 195.0000000000000284 ) ) ;
#5078 = DIRECTION ( 'NONE',  ( 1.836970198721029934E-16, -1.836970198721036344E-16, 1.000000000000000000 ) ) ;
#5079 = EDGE_CURVE ( 'NONE', #4997, #14602, #29272, .T. ) ;
#5080 = DIRECTION ( 'NONE',  ( -0.7071067811865421326, 0.7071067811865530128, 0.000000000000000000 ) ) ;
#5081 = CARTESIAN_POINT ( 'NONE',  ( 15.89999999999999680, -21.00000000000001421, -13.86939075806900945 ) ) ;
#5082 = ADVANCED_FACE ( 'NONE', ( #8057 ), #62868, .T. ) ;
#5083 = DIRECTION ( 'NONE',  ( -8.951101527228104953E-17, -1.000000000000000000, 0.000000000000000000 ) ) ;
#5084 = ADVANCED_FACE ( 'NONE', ( #35631, #51202 ), #50515, .F. ) ;
#5085 = ORIENTED_EDGE ( 'NONE', *, *, #14015, .T. ) ;
#5086 = CARTESIAN_POINT ( 'NONE',  ( -5.242976262117259978, 7.172176262117182510, 54.00000000000000711 ) ) ;
#5087 = EDGE_CURVE ( 'NONE', #59852, #40687, #46248, .T. ) ;
#5088 = ORIENTED_EDGE ( 'NONE', *, *, #58233, .T. ) ;
#5089 = CARTESIAN_POINT ( 'NONE',  ( 30.00000000000000000, -13.54524521594299991, -17.53999999999999915 ) ) ;
#5090 = DIRECTION ( 'NONE',  ( 0.000000000000000000, 0.000000000000000000, -1.000000000000000000 ) ) ;
#5091 = CIRCLE ( 'NONE', #1673, 3.499999999999849454 ) ;
#5092 = CARTESIAN_POINT ( 'NONE',  ( 11.50000000000000000, -11.50000000000000000, -15.00000000000000000 ) ) ;
#5093 = CARTESIAN_POINT ( 'NONE',  ( 7.250000000000005329, -7.249999999999998224, -17.50000000000000000 ) ) ;
#5094 = CARTESIAN_POINT ( 'NONE',  ( -9.234937905884127218, -9.955011587777249815, 455.0000000000000568 ) ) ;
#5095 = ORIENTED_EDGE ( 'NONE', *, *, #35435, .T. ) ;
#5096 = LINE ( 'NONE', #26667, #26843 ) ;
#5097 = DIRECTION ( 'NONE',  ( 0.000000000000000000, 0.000000000000000000, 1.000000000000000000 ) ) ;
#5098 = VECTOR ( 'NONE', #39583, 1000.000000000000000 ) ;
#5099 = AXIS2_PLACEMENT_3D ( 'NONE', #8155, #45998, #62968 ) ;
#5100 = EDGE_LOOP ( 'NONE', ( #21115, #17151, #35362, #1655 ) ) ;
#5101 = DIRECTION ( 'NONE',  ( -1.836970198721029934E-16, -1.836970198721010706E-16, 1.000000000000000000 ) ) ;
#5102 = ADVANCED_FACE ( 'NONE', ( #23980 ), #62496, .T. ) ;
#5103 = CARTESIAN_POINT ( 'NONE',  ( -7.250000000000001776, -7.249999999999998224, -15.50000000000000000 ) ) ;
#5104 = CYLINDRICAL_SURFACE ( 'NONE', #62456, 1.399999999999998579 ) ;
#5105 = ORIENTED_EDGE ( 'NONE', *, *, #9602, .T. ) ;
#5106 = LINE ( 'NONE', #47198, #43752 ) ;
#5107 = LINE ( 'NONE', #27024, #57914 ) ;
#5108 = VECTOR ( 'NONE', #26798, 1000.000000000000000 ) ;
#5109 = AXIS2_PLACEMENT_3D ( 'NONE', #31128, #19447, #62945 ) ;
#5110 = ORIENTED_EDGE ( 'NONE', *, *, #12381, .T. ) ;
#5111 = FACE_OUTER_BOUND ( 'NONE', #37457, .T. ) ;
#5112 = DIRECTION ( 'NONE',  ( -0.000000000000000000, -0.000000000000000000, 1.000000000000000000 ) ) ;
#5113 = EDGE_CURVE ( 'NONE', #9139, #45628, #11890, .T. ) ;
#5114 = AXIS2_PLACEMENT_3D ( 'NONE', #42049, #31805, #26149 ) ;
#5115 = DIRECTION ( 'NONE',  ( 1.000000000000000000, 0.000000000000000000, 0.000000000000000000 ) ) ;
#5116 = CARTESIAN_POINT ( 'NONE',  ( -15.50000000000000000, -0.2000000000000000111, -25.79999999999947136 ) ) ;
#5117 = ORIENTED_EDGE ( 'NONE', *, *, #15164, .T. ) ;
#5119 = VERTEX_POINT ( 'NONE', #18674 ) ;
#5118 = CARTESIAN_POINT ( 'NONE',  ( -23.48000000000000043, -15.50000000000000000, 26.00000000000000355 ) ) ;
#5120 = EDGE_CURVE ( 'NONE', #50235, #32493, #66050, .T. ) ;
#5121 = VECTOR ( 'NONE', #6813, 1000.000000000000114 ) ;
#5122 = DIRECTION ( 'NONE',  ( 1.000000000000000000, 0.000000000000000000, 0.000000000000000000 ) ) ;
#5123 = LINE ( 'NONE', #38343, #40246 ) ;
#5124 = CARTESIAN_POINT ( 'NONE',  ( 0.5000000000000000000, -0.5000000000000000000, -27.00000000000000000 ) ) ;
#5125 = ORIENTED_EDGE ( 'NONE', *, *, #545, .F. ) ;
#5126 = STYLED_ITEM ( 'NONE', ( #67428 ), #43268 ) ;
#5127 = DIRECTION ( 'NONE',  ( 1.000000000000000000, -0.000000000000000000, 0.000000000000000000 ) ) ;
#5128 = ORIENTED_EDGE ( 'NONE', *, *, #20766, .T. ) ;
#5129 = ORIENTED_EDGE ( 'NONE', *, *, #30495, .F. ) ;
#5130 = EDGE_LOOP ( 'NONE', ( #17385, #55770, #31793, #50830 ) ) ;
#5131 = EDGE_CURVE ( 'NONE', #11718, #36648, #8406, .T. ) ;
#5132 = CYLINDRICAL_SURFACE ( 'NONE', #50097, 0.5000000000009372503 ) ;
#5133 = DIRECTION ( 'NONE',  ( 1.000000000000000000, 0.000000000000000000, 0.000000000000000000 ) ) ;
#5134 = ORIENTED_EDGE ( 'NONE', *, *, #53278, .T. ) ;
#5135 = EDGE_CURVE ( 'NONE', #44422, #26906, #25389, .T. ) ;
#5136 = EDGE_LOOP ( 'NONE', ( #29991, #48536, #26102, #42583 ) ) ;
#5137 = EDGE_CURVE ( 'NONE', #37491, #51717, #58965, .T. ) ;
#5138 = CARTESIAN_POINT ( 'NONE',  ( 30.00000000000000000, -17.00000000000000000, -15.70499999999969809 ) ) ;
#5139 = VERTEX_POINT ( 'NONE', #52980 ) ;
#5140 = EDGE_CURVE ( 'NONE', #11259, #37252, #57911, .T. ) ;
#5141 = VECTOR ( 'NONE', #7340, 1000.000000000000000 ) ;
#5142 = ORIENTED_EDGE ( 'NONE', *, *, #65693, .T. ) ;
#5143 = EDGE_CURVE ( 'NONE', #17827, #40029, #26440, .T. ) ;
#5144 = EDGE_CURVE ( 'NONE', #57095, #54700, #10521, .T. ) ;
#5145 = VERTEX_POINT ( 'NONE', #58622 ) ;
#5146 = ORIENTED_EDGE ( 'NONE', *, *, #1222, .T. ) ;
#5147 = AXIS2_PLACEMENT_3D ( 'NONE', #25098, #9185, #30754 ) ;
#5148 = DIRECTION ( 'NONE',  ( 0.000000000000000000, 0.000000000000000000, 1.000000000000000000 ) ) ;
#5150 = EDGE_LOOP ( 'NONE', ( #34977, #10089, #66327, #54719 ) ) ;
#5149 = DIRECTION ( 'NONE',  ( 0.000000000000000000, 0.000000000000000000, -1.000000000000000000 ) ) ;
#5151 = EDGE_CURVE ( 'NONE', #21321, #17475, #31756, .T. ) ;
#5152 = CARTESIAN_POINT ( 'NONE',  ( 38.90000000000000568, 0.000000000000000000, 3.232403992503367940E-15 ) ) ;
#5153 = AXIS2_PLACEMENT_3D ( 'NONE', #16452, #38034, #54288 ) ;
#5154 = VECTOR ( 'NONE', #11247, 1000.000000000000000 ) ;
#5155 = VECTOR ( 'NONE', #3663, 1000.000000000000000 ) ;
#5156 = DIRECTION ( 'NONE',  ( -1.000000000000000000, 0.000000000000000000, 0.000000000000000000 ) ) ;
#5157 = EDGE_CURVE ( 'NONE', #38076, #1682, #37749, .T. ) ;
#5158 = LINE ( 'NONE', #912, #44840 ) ;
#5159 = VERTEX_POINT ( 'NONE', #53328 ) ;
#5160 = EDGE_CURVE ( 'NONE', #12117, #31270, #10175, .T. ) ;
#5161 = CIRCLE ( 'NONE', #44644, 1.399999999999999245 ) ;
#5162 = AXIS2_PLACEMENT_3D ( 'NONE', #20945, #58080, #53488 ) ;
#5163 = DIRECTION ( 'NONE',  ( -0.7071067811865401342, 0.7071067811865550112, 1.355854680848613865E-30 ) ) ;
#5164 = VECTOR ( 'NONE', #42360, 1000.000000000000000 ) ;
#5165 = EDGE_CURVE ( 'NONE', #16165, #26713, #20778, .T. ) ;
#5166 = FACE_OUTER_BOUND ( 'NONE', #12152, .T. ) ;
#5167 = VERTEX_POINT ( 'NONE', #63929 ) ;
#5168 = DIRECTION ( 'NONE',  ( -1.836970198721029934E-16, 1.836970198721036590E-16, -1.000000000000000000 ) ) ;
#5169 = EDGE_CURVE ( 'NONE', #6350, #7925, #64278, .T. ) ;
#5170 = VECTOR ( 'NONE', #59016, 1000.000000000000000 ) ;
#5171 = CARTESIAN_POINT ( 'NONE',  ( -7.450000000000001954, 0.000000000000000000, -10.50000000000000000 ) ) ;
#5172 = DIRECTION ( 'NONE',  ( 1.000000000000000000, -0.000000000000000000, 0.000000000000000000 ) ) ;
#5173 = VECTOR ( 'NONE', #34005, 1000.000000000000000 ) ;
#5174 = VERTEX_POINT ( 'NONE', #42000 ) ;
#5175 = VECTOR ( 'NONE', #10642, 1000.000000000000114 ) ;
#5176 = DIRECTION ( 'NONE',  ( 0.000000000000000000, -3.673940397442059868E-16, 1.000000000000000000 ) ) ;
#5177 = DIRECTION ( 'NONE',  ( 0.000000000000000000, 0.000000000000000000, 1.000000000000000000 ) ) ;
#5178 = CARTESIAN_POINT ( 'NONE',  ( -6.486996718459899114, -2.632023737882779102, 26.00000000000000711 ) ) ;
#5179 = EDGE_CURVE ( 'NONE', #31769, #62248, #69584, .T. ) ;
#5180 = DIRECTION ( 'NONE',  ( 0.000000000000000000, -0.7096009616570518874, 0.7046037717862339012 ) ) ;
#5181 = CARTESIAN_POINT ( 'NONE',  ( 14.90000000000000036, 0.000000000000000000, 6.464807985006735683E-16 ) ) ;
#5182 = CARTESIAN_POINT ( 'NONE',  ( 75.42576880091937142, 0.000000000000000000, 285.9830310981789125 ) ) ;
#5183 =( LENGTH_UNIT ( ) NAMED_UNIT ( * ) SI_UNIT ( .MILLI., .METRE. ) );
#5184 = DIRECTION ( 'NONE',  ( 0.000000000000000000, 0.000000000000000000, 1.000000000000000000 ) ) ;
#5185 = ORIENTED_EDGE ( 'NONE', *, *, #5830, .F. ) ;
#5186 = DIRECTION ( 'NONE',  ( -1.000000000000000000, 0.000000000000000000, 0.000000000000000000 ) ) ;
#5187 = VECTOR ( 'NONE', #56032, 1000.000000000000000 ) ;
#5188 = DIRECTION ( 'NONE',  ( 0.6414496315691617934, -0.7671651518152962090, 0.000000000000000000 ) ) ;
#5189 = LINE ( 'NONE', #47617, #4197 ) ;
#5190 = CARTESIAN_POINT ( 'NONE',  ( -29.25000000000000000, -5.200000000000001066, 26.25000000000000000 ) ) ;
#5191 = ORIENTED_EDGE ( 'NONE', *, *, #42420, .F. ) ;
#5192 = FACE_OUTER_BOUND ( 'NONE', #46422, .T. ) ;
#5193 = DIRECTION ( 'NONE',  ( 1.000000000000000000, -0.000000000000000000, -0.000000000000000000 ) ) ;
#5194 = VECTOR ( 'NONE', #58164, 1000.000000000000000 ) ;
#5195 = CARTESIAN_POINT ( 'NONE',  ( 6.006483450353409914, 8.198316549646580853, 455.0000000000000568 ) ) ;
#5196 = ADVANCED_FACE ( 'NONE', ( #21139 ), #14784, .F. ) ;
#5197 = LINE ( 'NONE', #69887, #14051 ) ;
#5198 = AXIS2_PLACEMENT_3D ( 'NONE', #33783, #27797, #16839 ) ;
#5199 = DIRECTION ( 'NONE',  ( -0.000000000000000000, -0.000000000000000000, -1.000000000000000000 ) ) ;
#5200 = LINE ( 'NONE', #14757, #60996 ) ;
#5201 = ORIENTED_EDGE ( 'NONE', *, *, #68435, .T. ) ;
#5202 = EDGE_CURVE ( 'NONE', #50939, #37548, #15826, .T. ) ;
#5203 = AXIS2_PLACEMENT_3D ( 'NONE', #59152, #37251, #31942 ) ;
#5204 = VECTOR ( 'NONE', #40108, 1000.000000000000000 ) ;
#5205 = AXIS2_PLACEMENT_3D ( 'NONE', #13827, #35380, #67925 ) ;
#5206 = ORIENTED_EDGE ( 'NONE', *, *, #64188, .T. ) ;
#5207 = DIRECTION ( 'NONE',  ( -1.000000000000000000, 0.000000000000000000, 0.000000000000000000 ) ) ;
#5208 = LINE ( 'NONE', #32073, #40187 ) ;
#5209 = ORIENTED_EDGE ( 'NONE', *, *, #39436, .T. ) ;
#5210 = EDGE_CURVE ( 'NONE', #28379, #36190, #44593, .T. ) ;
#5211 = PLANE ( 'NONE',  #11142 ) ;
#5212 = CIRCLE ( 'NONE', #15353, 0.1749999999999993783 ) ;
#5213 = AXIS2_PLACEMENT_3D ( 'NONE', #20598, #5746, #21997 ) ;
#5214 = AXIS2_PLACEMENT_3D ( 'NONE', #42433, #52002, #31842 ) ;
#5215 = DIRECTION ( 'NONE',  ( 0.000000000000000000, -1.000000000000000000, 0.000000000000000000 ) ) ;
#5216 = EDGE_CURVE ( 'NONE', #44788, #27591, #43041, .T. ) ;
#5217 = ORIENTED_EDGE ( 'NONE', *, *, #28109, .T. ) ;
#5218 = AXIS2_PLACEMENT_3D ( 'NONE', #41926, #20361, #63508 ) ;
#5219 = FACE_OUTER_BOUND ( 'NONE', #19050, .T. ) ;
#5220 = ORIENTED_EDGE ( 'NONE', *, *, #55453, .F. ) ;
#5221 = EDGE_CURVE ( 'NONE', #65046, #19943, #37404, .T. ) ;
#5222 = ORIENTED_EDGE ( 'NONE', *, *, #36754, .F. ) ;
#5223 = LINE ( 'NONE', #601, #26106 ) ;
#5224 = EDGE_LOOP ( 'NONE', ( #53534, #51564, #4320, #6005 ) ) ;
#5225 = FACE_OUTER_BOUND ( 'NONE', #66472, .T. ) ;
#5226 = CARTESIAN_POINT ( 'NONE',  ( 0.000000000000000000, -17.79289321881345032, -20.50000000000000000 ) ) ;
#5227 = CARTESIAN_POINT ( 'NONE',  ( 83.77321854994620765, 47.95351654967443977, 15.00000000000000000 ) ) ;
#5228 = VECTOR ( 'NONE', #34028, 1000.000000000000000 ) ;
#5229 = ORIENTED_EDGE ( 'NONE', *, *, #69960, .T. ) ;
#5230 = ORIENTED_EDGE ( 'NONE', *, *, #69230, .T. ) ;
#5231 = VECTOR ( 'NONE', #54743, 1000.000000000000000 ) ;
#5232 = DIRECTION ( 'NONE',  ( 0.8660254037844363761, -0.5000000000000038858, -1.836970198721044232E-16 ) ) ;
#5234 = CARTESIAN_POINT ( 'NONE',  ( 41.09999999999999432, -14.06939075806900163, 20.80000000000000426 ) ) ;
#5233 = DIRECTION ( 'NONE',  ( -1.000000000000000000, 3.016910393003147986E-15, 1.108394896831706469E-30 ) ) ;
#5235 = ORIENTED_EDGE ( 'NONE', *, *, #8801, .F. ) ;
#5236 = ORIENTED_EDGE ( 'NONE', *, *, #52654, .F. ) ;
#5237 = EDGE_CURVE ( 'NONE', #67361, #52010, #64617, .T. ) ;
#5238 = ORIENTED_EDGE ( 'NONE', *, *, #1057, .T. ) ;
#5239 = DIRECTION ( 'NONE',  ( 0.6414496315691617934, 0.7671651518152962090, -0.000000000000000000 ) ) ;
#5241 = VERTEX_POINT ( 'NONE', #16176 ) ;
#5240 = CYLINDRICAL_SURFACE ( 'NONE', #20569, 0.5999999999999989786 ) ;
#5242 = LINE ( 'NONE', #26812, #16468 ) ;
#5243 = CARTESIAN_POINT ( 'NONE',  ( 9.703773737882785966, -8.580623737882845603, 26.00000000000000000 ) ) ;
#5244 = VERTEX_POINT ( 'NONE', #26100 ) ;
#5245 = AXIS2_PLACEMENT_3D ( 'NONE', #59534, #846, #69797 ) ;
#5246 = ORIENTED_EDGE ( 'NONE', *, *, #744, .F. ) ;
#5247 = CARTESIAN_POINT ( 'NONE',  ( 283.0000000000000568, -25.60000000000000142, -15.10000000000000142 ) ) ;
#5248 = AXIS2_PLACEMENT_3D ( 'NONE', #61976, #60586, #28401 ) ;
#5249 = VERTEX_POINT ( 'NONE', #47653 ) ;
#5250 = CARTESIAN_POINT ( 'NONE',  ( 11.50000000000000000, -11.50000000000000000, 15.00000000000000000 ) ) ;
#5251 = DIRECTION ( 'NONE',  ( -1.000000000000000000, 0.000000000000000000, 0.000000000000000000 ) ) ;
#5252 = AXIS2_PLACEMENT_3D ( 'NONE', #53220, #26328, #47886 ) ;
#5253 = CYLINDRICAL_SURFACE ( 'NONE', #30565, 0.3999999999999993006 ) ;
#5254 = EDGE_CURVE ( 'NONE', #56335, #48411, #42349, .T. ) ;
#5255 = VERTEX_POINT ( 'NONE', #59663 ) ;
#5256 = EDGE_CURVE ( 'NONE', #1599, #61271, #28167, .T. ) ;
#5257 = VECTOR ( 'NONE', #18796, 1000.000000000000000 ) ;
#5258 = AXIS2_PLACEMENT_3D ( 'NONE', #17341, #38915, #60478 ) ;
#5259 = CARTESIAN_POINT ( 'NONE',  ( -3.667976262117227382, 9.897976262117168744, 26.00000000000000711 ) ) ;
#5260 = LINE ( 'NONE', #5936, #45963 ) ;
#5262 = ORIENTED_EDGE ( 'NONE', *, *, #29993, .F. ) ;
#5261 = CARTESIAN_POINT ( 'NONE',  ( -4.609516549646713202, 3.593516549646603941, 455.0000000000000568 ) ) ;
#5263 = ORIENTED_EDGE ( 'NONE', *, *, #55206, .F. ) ;
#5264 = LINE ( 'NONE', #36735, #2666 ) ;
#5265 = AXIS2_PLACEMENT_3D ( 'NONE', #7134, #56633, #34010 ) ;
#5266 = AXIS2_PLACEMENT_3D ( 'NONE', #31409, #52977, #47304 ) ;
#5267 = FACE_OUTER_BOUND ( 'NONE', #44755, .T. ) ;
#5268 = CARTESIAN_POINT ( 'NONE',  ( 30.00000000000000000, -14.33999999999999986, -14.50000000000000000 ) ) ;
#5269 = DIRECTION ( 'NONE',  ( 0.000000000000000000, 0.000000000000000000, -1.000000000000000000 ) ) ;
#5270 = AXIS2_PLACEMENT_3D ( 'NONE', #65420, #12679, #28610 ) ;
#5271 = CARTESIAN_POINT ( 'NONE',  ( 26.90000000000000213, 13.66939075806899240, -20.79999999999999361 ) ) ;
#5272 = ORIENTED_EDGE ( 'NONE', *, *, #23632, .F. ) ;
#5273 = LINE ( 'NONE', #16910, #58405 ) ;
#5274 = CARTESIAN_POINT ( 'NONE',  ( 40.90000000000000568, 16.96999999999999886, 21.00000000000000000 ) ) ;
#5275 = LINE ( 'NONE', #26839, #36826 ) ;
#5277 = ORIENTED_EDGE ( 'NONE', *, *, #35378, .T. ) ;
#5276 = DIRECTION ( 'NONE',  ( 0.000000000000000000, -1.000000000000000000, 0.000000000000000000 ) ) ;
#5278 = PRODUCT_DEFINITION_SHAPE ( 'NONE', 'NONE',  #69998 ) ;
#5279 = VECTOR ( 'NONE', #68847, 1000.000000000000000 ) ;
#5280 = LINE ( 'NONE', #6302, #1940 ) ;
#5281 = CYLINDRICAL_SURFACE ( 'NONE', #45007, 0.3499999999999614531 ) ;
#5282 = DIRECTION ( 'NONE',  ( 0.000000000000000000, 0.000000000000000000, -1.000000000000000000 ) ) ;
#5283 = CARTESIAN_POINT ( 'NONE',  ( -7.450000000000001954, 7.250000000000000000, -23.00000000000000000 ) ) ;
#5284 = ORIENTED_EDGE ( 'NONE', *, *, #22187, .F. ) ;
#5285 = LINE ( 'NONE', #28216, #21902 ) ;
#5286 = DIRECTION ( 'NONE',  ( 0.000000000000000000, 0.000000000000000000, 1.000000000000000000 ) ) ;
#5287 = VERTEX_POINT ( 'NONE', #66345 ) ;
#5288 = CARTESIAN_POINT ( 'NONE',  ( 4.206483450353373676, 11.11351654964663282, 195.0000000000000284 ) ) ;
#5289 = LINE ( 'NONE', #48760, #36741 ) ;
#5290 = DIRECTION ( 'NONE',  ( 0.7071067811865361374, -0.7071067811865588970, 0.000000000000000000 ) ) ;
#5291 = DIRECTION ( 'NONE',  ( -1.000000000000000000, 0.000000000000000000, 0.000000000000000000 ) ) ;
#5292 = EDGE_CURVE ( 'NONE', #25620, #1191, #17549, .T. ) ;
#5293 = DIRECTION ( 'NONE',  ( 0.5773502691896257311, -0.5773502691896257311, -0.5773502691896257311 ) ) ;
#5294 = ORIENTED_EDGE ( 'NONE', *, *, #29619, .F. ) ;
#5295 = ORIENTED_EDGE ( 'NONE', *, *, #62799, .T. ) ;
#5296 = DIRECTION ( 'NONE',  ( 4.336808689942006692E-15, 1.000000000000000000, 0.000000000000000000 ) ) ;
#5297 = VERTEX_POINT ( 'NONE', #11889 ) ;
#5298 = VECTOR ( 'NONE', #44203, 1000.000000000000000 ) ;
#5299 = EDGE_LOOP ( 'NONE', ( #22492, #54011, #281, #11533 ) ) ;
#5300 = EDGE_CURVE ( 'NONE', #56820, #23370, #45766, .T. ) ;
#5301 = DIRECTION ( 'NONE',  ( 0.000000000000000000, -3.673940397442059868E-16, 1.000000000000000000 ) ) ;
#5302 = COLOUR_RGB ( '', 0.09019608, 0.27058824, 0.51372549) ;
#5303 = EDGE_CURVE ( 'NONE', #15679, #13897, #33478, .T. ) ;
#5304 = EDGE_CURVE ( 'NONE', #34775, #33396, #28796, .T. ) ;
#5305 = CARTESIAN_POINT ( 'NONE',  ( 3.848229544836323512, -7.357023737882802727, 26.00000000000000000 ) ) ;
#5306 = VECTOR ( 'NONE', #7057, 1000.000000000000000 ) ;
#5307 = AXIS2_PLACEMENT_3D ( 'NONE', #19057, #45932, #7042 ) ;
#5308 = FACE_OUTER_BOUND ( 'NONE', #8413, .T. ) ;
#5309 = ORIENTED_EDGE ( 'NONE', *, *, #26315, .T. ) ;
#5310 = EDGE_CURVE ( 'NONE', #24647, #14509, #49734, .T. ) ;
#5311 = VERTEX_POINT ( 'NONE', #65983 ) ;
#5312 = EDGE_CURVE ( 'NONE', #15307, #64032, #6608, .T. ) ;
#5313 = LINE ( 'NONE', #65389, #55566 ) ;
#5314 = VERTEX_POINT ( 'NONE', #54024 ) ;
#5315 = ORIENTED_EDGE ( 'NONE', *, *, #43942, .T. ) ;
#5316 = AXIS2_PLACEMENT_3D ( 'NONE', #19677, #52584, #62830 ) ;
#5317 = AXIS2_PLACEMENT_3D ( 'NONE', #49148, #59414, #69688 ) ;
#5318 = CARTESIAN_POINT ( 'NONE',  ( -2.693516549646682190, 10.08346604330774454, 455.0000000000000568 ) ) ;
#5319 = LINE ( 'NONE', #26881, #26818 ) ;
#5320 = CARTESIAN_POINT ( 'NONE',  ( 15.50000000000000000, -0.2000000000000000111, -22.50000000000000000 ) ) ;
#5321 = EDGE_CURVE ( 'NONE', #59441, #56315, #613, .T. ) ;
#5322 = AXIS2_PLACEMENT_3D ( 'NONE', #39546, #55823, #60775 ) ;
#5323 = ORIENTED_EDGE ( 'NONE', *, *, #54468, .F. ) ;
#5324 = CARTESIAN_POINT ( 'NONE',  ( 29.50000000000000355, -11.70000000000000284, -11.00000000000000000 ) ) ;
#5325 = VECTOR ( 'NONE', #35946, 1000.000000000000000 ) ;
#5326 = VECTOR ( 'NONE', #2337, 999.9999999999998863 ) ;
#5328 = LINE ( 'NONE', #41731, #25439 ) ;
#5327 = CARTESIAN_POINT ( 'NONE',  ( 10.47821035407136137, -25.18021646000299540, 17.31978353999700460 ) ) ;
#5329 = ORIENTED_EDGE ( 'NONE', *, *, #32771, .T. ) ;
#5330 = ORIENTED_EDGE ( 'NONE', *, *, #32681, .F. ) ;
#5332 = VERTEX_POINT ( 'NONE', #5916 ) ;
#5331 = LINE ( 'NONE', #11294, #28586 ) ;
#5333 = ORIENTED_EDGE ( 'NONE', *, *, #49358, .F. ) ;
#5334 = CIRCLE ( 'NONE', #16463, 24.99999999998784972 ) ;
#5335 = CYLINDRICAL_SURFACE ( 'NONE', #54761, 0.5249999999999999112 ) ;
#5336 = CIRCLE ( 'NONE', #67395, 0.9999999999999991118 ) ;
#5337 = LINE ( 'NONE', #68267, #22540 ) ;
#5338 = ORIENTED_EDGE ( 'NONE', *, *, #24519, .F. ) ;
#5339 = PLANE ( 'NONE',  #3026 ) ;
#5340 = DIRECTION ( 'NONE',  ( 0.000000000000000000, 1.000000000000000000, 0.000000000000000000 ) ) ;
#5341 = ORIENTED_EDGE ( 'NONE', *, *, #64622, .F. ) ;
#5342 = ORIENTED_EDGE ( 'NONE', *, *, #48606, .F. ) ;
#5343 = CARTESIAN_POINT ( 'NONE',  ( 5.257023737882795977, 5.242976262117205799, 26.00000000000000711 ) ) ;
#5344 = CARTESIAN_POINT ( 'NONE',  ( -4.734785091273987057, -6.619341603356850179, 195.0000000000000284 ) ) ;
#5345 = CARTESIAN_POINT ( 'NONE',  ( 14.89999999999999680, -21.00000000000000000, 13.86939075806900057 ) ) ;
#5346 = EDGE_LOOP ( 'NONE', ( #20860, #29043, #29, #6725 ) ) ;
#5347 = EDGE_CURVE ( 'NONE', #17361, #65338, #25441, .T. ) ;
#5348 = DIRECTION ( 'NONE',  ( -1.000000000000000000, 0.000000000000000000, 0.000000000000000000 ) ) ;
#5349 = FACE_OUTER_BOUND ( 'NONE', #11418, .T. ) ;
#5350 = PRESENTATION_LAYER_ASSIGNMENT (  '', '', ( #64106 ) ) ;
#5353 = ORIENTED_EDGE ( 'NONE', *, *, #40160, .T. ) ;
#5352 = EDGE_CURVE ( 'NONE', #19307, #26597, #32781, .T. ) ;
#5351 = CYLINDRICAL_SURFACE ( 'NONE', #5848, 2.500000000000000000 ) ;
#5355 = ORIENTED_EDGE ( 'NONE', *, *, #58982, .T. ) ;
#5354 = CARTESIAN_POINT ( 'NONE',  ( 7.750000000000001776, 7.750000000000000000, 5.000000000000000000 ) ) ;
#5356 = EDGE_CURVE ( 'NONE', #191, #1311, #64970, .T. ) ;
#5357 = DIRECTION ( 'NONE',  ( 1.000000000000000000, -0.000000000000000000, -0.000000000000000000 ) ) ;
#5358 = CARTESIAN_POINT ( 'NONE',  ( 10.20488345035338007, -11.48848345035349361, 455.0000000000000568 ) ) ;
#5359 = DIRECTION ( 'NONE',  ( 0.000000000000000000, -0.000000000000000000, 1.000000000000000000 ) ) ;
#5360 = DIRECTION ( 'NONE',  ( 0.000000000000000000, 0.000000000000000000, 1.000000000000000000 ) ) ;
#5361 = EDGE_CURVE ( 'NONE', #65486, #10069, #62115, .T. ) ;
#5362 = CARTESIAN_POINT ( 'NONE',  ( -11.47551654964677326, -10.20488345035332145, 195.0000000000000284 ) ) ;
#5363 = AXIS2_PLACEMENT_3D ( 'NONE', #52937, #4485, #9079 ) ;
#5364 = CARTESIAN_POINT ( 'NONE',  ( -7.415254214038356828, -3.606483450353401121, 455.0000000000000568 ) ) ;
#5365 = ORIENTED_EDGE ( 'NONE', *, *, #13341, .T. ) ;
#5366 = DIRECTION ( 'NONE',  ( 0.000000000000000000, 0.000000000000000000, -1.000000000000000000 ) ) ;
#5368 = ORIENTED_EDGE ( 'NONE', *, *, #44076, .F. ) ;
#5367 = PLANE ( 'NONE',  #36779 ) ;
#5369 = AXIS2_PLACEMENT_3D ( 'NONE', #64508, #20656, #47541 ) ;
#5372 = ORIENTED_EDGE ( 'NONE', *, *, #4217, .F. ) ;
#5371 = DIRECTION ( 'NONE',  ( 0.000000000000000000, 1.000000000000000000, 0.000000000000000000 ) ) ;
#5370 = VECTOR ( 'NONE', #21761, 1000.000000000000114 ) ;
#5373 = DIRECTION ( 'NONE',  ( -1.000000000000000000, 0.000000000000000000, 0.000000000000000000 ) ) ;
#5374 = EDGE_LOOP ( 'NONE', ( #22596, #46775, #38858, #21998 ) ) ;
#5375 = CARTESIAN_POINT ( 'NONE',  ( 47.00000000000000000, 0.7500000000000000000, 4.943429983321300014 ) ) ;
#5376 = VECTOR ( 'NONE', #27776, 1000.000000000000227 ) ;
#5377 = VECTOR ( 'NONE', #45181, 1000.000000000000000 ) ;
#5378 = ORIENTED_EDGE ( 'NONE', *, *, #55995, .T. ) ;
#5379 = DIRECTION ( 'NONE',  ( 0.7071067811865401342, -0.7071067811865550112, -1.355854680848614216E-30 ) ) ;
#5380 = CARTESIAN_POINT ( 'NONE',  ( 13.00000000000000178, -17.35230188589299871, 15.35019951917099945 ) ) ;
#5381 = ORIENTED_EDGE ( 'NONE', *, *, #24597, .F. ) ;
#5382 = LINE ( 'NONE', #26233, #63954 ) ;
#5383 = DIRECTION ( 'NONE',  ( 0.000000000000000000, -0.7075494706728322480, 0.7066638143775262337 ) ) ;
#5384 = VECTOR ( 'NONE', #30023, 1000.000000000000000 ) ;
#5385 = EDGE_CURVE ( 'NONE', #47516, #1435, #54360, .T. ) ;
#5386 = ORIENTED_EDGE ( 'NONE', *, *, #29409, .T. ) ;
#5387 = DIRECTION ( 'NONE',  ( -0.000000000000000000, 3.673940397442059868E-16, -1.000000000000000000 ) ) ;
#5388 = B_SPLINE_CURVE_WITH_KNOTS ( 'NONE', 3,
 ( #30707, #15145, #52271, #4194, #68177, #25768 ),
 .UNSPECIFIED., .F., .F.,
 ( 4, 2, 4 ),
 ( 1.820537833122030991, 2.555393473688635453, 3.290249114255240137 ),
 .UNSPECIFIED. ) ;
#5389 = VERTEX_POINT ( 'NONE', #65323 ) ;
#5390 = ORIENTED_EDGE ( 'NONE', *, *, #66520, .F. ) ;
#5391 = CARTESIAN_POINT ( 'NONE',  ( 26.90000000000000213, 0.000000000000000000, 1.939442395502021001E-15 ) ) ;
#5392 = CARTESIAN_POINT ( 'NONE',  ( -28.00000000000000000, -17.50000000000000000, -20.05051025721700242 ) ) ;
#5393 = CARTESIAN_POINT ( 'NONE',  ( -7.250000000000000888, -8.249999999999998224, -15.50000000000000000 ) ) ;
#5394 = FACE_OUTER_BOUND ( 'NONE', #17067, .T. ) ;
#5395 = VERTEX_POINT ( 'NONE', #16874 ) ;
#5396 = EDGE_CURVE ( 'NONE', #46624, #63930, #28504, .T. ) ;
#5397 = EDGE_LOOP ( 'NONE', ( #15840, #40139, #67385, #117, #801, #5510, #69473, #21839, #53673, #6333, #51791, #11188, #1559, #37850, #39398, #7037 ) ) ;
#5398 = EDGE_CURVE ( 'NONE', #28218, #51205, #50078, .T. ) ;
#5400 = VERTEX_POINT ( 'NONE', #38106 ) ;
#5399 = LINE ( 'NONE', #31911, #63404 ) ;
#5401 = ORIENTED_EDGE ( 'NONE', *, *, #47197, .F. ) ;
#5402 = DIRECTION ( 'NONE',  ( -0.000000000000000000, 0.000000000000000000, -1.000000000000000000 ) ) ;
#5403 = CARTESIAN_POINT ( 'NONE',  ( 275.0000000000000000, -41.99999999999906208, -14.49999999999903899 ) ) ;
#5404 = EDGE_CURVE ( 'NONE', #41930, #27322, #1628, .T. ) ;
#5405 = LINE ( 'NONE', #42160, #65858 ) ;
#5406 = VECTOR ( 'NONE', #4056, 1000.000000000000000 ) ;
#5407 = PLANE ( 'NONE',  #52606 ) ;
#5409 = FACE_OUTER_BOUND ( 'NONE', #49902, .T. ) ;
#5408 = DIRECTION ( 'NONE',  ( 1.000000000000000000, -0.000000000000000000, 0.000000000000000000 ) ) ;
#5410 = ORIENTED_EDGE ( 'NONE', *, *, #47764, .F. ) ;
#5412 = ORIENTED_EDGE ( 'NONE', *, *, #35527, .F. ) ;
#5411 = DIRECTION ( 'NONE',  ( -1.000000000000000000, 0.000000000000000000, 0.000000000000000000 ) ) ;
#5413 = ORIENTED_EDGE ( 'NONE', *, *, #53447, .T. ) ;
#5414 = ORIENTED_EDGE ( 'NONE', *, *, #31507, .F. ) ;
#5415 = AXIS2_PLACEMENT_3D ( 'NONE', #63947, #58290, #41666 ) ;
#5416 = VECTOR ( 'NONE', #62439, 1000.000000000000000 ) ;
#5417 = DIRECTION ( 'NONE',  ( -8.728482790395504563E-15, -1.000000000000000000, 0.000000000000000000 ) ) ;
#5418 = PLANE ( 'NONE',  #60342 ) ;
#5419 = CARTESIAN_POINT ( 'NONE',  ( -69.91216426482253610, 59.49351654964636538, 318.8237994620729410 ) ) ;
#5420 = AXIS2_PLACEMENT_3D ( 'NONE', #13441, #67185, #61170 ) ;
#5421 = CIRCLE ( 'NONE', #9902, 0.5250000000000003553 ) ;
#5422 = CARTESIAN_POINT ( 'NONE',  ( 18.89999999999999858, -14.06939075806900163, -20.80000000000000426 ) ) ;
#5423 = VERTEX_POINT ( 'NONE', #32451 ) ;
#5424 = ORIENTED_EDGE ( 'NONE', *, *, #68240, .T. ) ;
#5425 = EDGE_LOOP ( 'NONE', ( #36136, #69585, #69436, #55041 ) ) ;
#5426 = DIRECTION ( 'NONE',  ( -1.000000000000000000, 0.000000000000000000, 0.000000000000000000 ) ) ;
#5427 = CIRCLE ( 'NONE', #14440, 4.500000000000191847 ) ;
#5428 = AXIS2_PLACEMENT_3D ( 'NONE', #6602, #48695, #22523 ) ;
#5429 = DIRECTION ( 'NONE',  ( 0.000000000000000000, 0.000000000000000000, -1.000000000000000000 ) ) ;
#5430 = CARTESIAN_POINT ( 'NONE',  ( -11.75000000000000000, -5.000000000000000000, -11.75000000000000000 ) ) ;
#5431 = VERTEX_POINT ( 'NONE', #22529 ) ;
#5432 = EDGE_LOOP ( 'NONE', ( #41029, #66035, #12162, #13730, #68902, #33731, #1269, #59984, #38672 ) ) ;
#5433 = CARTESIAN_POINT ( 'NONE',  ( 6.006483450353401921, 5.993516549646582092, 455.0000000000000568 ) ) ;
#5434 = CARTESIAN_POINT ( 'NONE',  ( 6.006483450353353959, 5.993516549646629166, 195.0000000000000284 ) ) ;
#5435 = VERTEX_POINT ( 'NONE', #21826 ) ;
#5436 = AXIS2_PLACEMENT_3D ( 'NONE', #42293, #31706, #53277 ) ;
#5437 = LINE ( 'NONE', #48551, #16713 ) ;
#5440 = ORIENTED_EDGE ( 'NONE', *, *, #12061, .F. ) ;
#5439 = EDGE_CURVE ( 'NONE', #19639, #21838, #43385, .T. ) ;
#5438 = DIRECTION ( 'NONE',  ( -1.000000000000000000, 0.000000000000000000, 0.000000000000000000 ) ) ;
#5441 = ORIENTED_EDGE ( 'NONE', *, *, #7941, .F. ) ;
#5442 = EDGE_CURVE ( 'NONE', #69858, #63180, #67401, .T. ) ;
#5443 = ADVANCED_FACE ( 'NONE', ( #51121 ), #19295, .T. ) ;
#5444 = CARTESIAN_POINT ( 'NONE',  ( -4.193516549646673752, 11.31351654964658771, 455.0000000000000568 ) ) ;
#5445 = CYLINDRICAL_SURFACE ( 'NONE', #11979, 0.2000000000000005107 ) ;
#5446 = DIRECTION ( 'NONE',  ( -8.612436249475772606E-15, -1.000000000000000000, -1.836970198721020566E-16 ) ) ;
#5447 = DIRECTION ( 'NONE',  ( -1.000000000000000000, 0.000000000000000000, 0.000000000000000000 ) ) ;
#5448 = ADVANCED_FACE ( 'NONE', ( #66686 ), #35191, .F. ) ;
#5449 = LINE ( 'NONE', #69079, #46281 ) ;
#5450 = VERTEX_POINT ( 'NONE', #8328 ) ;
#5451 = LINE ( 'NONE', #16744, #54115 ) ;
#5452 = EDGE_LOOP ( 'NONE', ( #30410, #1916, #40791, #41088, #41742, #37734 ) ) ;
#5453 = DIRECTION ( 'NONE',  ( 1.836970198721029934E-16, -1.836970198721036344E-16, 1.000000000000000000 ) ) ;
#5454 = CARTESIAN_POINT ( 'NONE',  ( -30.00000000000000000, -12.00000000000000000, 10.52786404500095863 ) ) ;
#5455 = DIRECTION ( 'NONE',  ( 0.7071067811865475727, -0.7071067811865475727, 0.000000000000000000 ) ) ;
#5456 = DIRECTION ( 'NONE',  ( 1.000000000000000000, 0.000000000000000000, 0.000000000000000000 ) ) ;
#5457 = DIRECTION ( 'NONE',  ( 0.7071067811865514585, 0.7071067811865435759, -0.000000000000000000 ) ) ;
#5458 = VERTEX_POINT ( 'NONE', #39462 ) ;
#5459 = ADVANCED_FACE ( 'NONE', ( #67737 ), #39799, .T. ) ;
#5460 = CARTESIAN_POINT ( 'NONE',  ( 6.789561617636934443, 7.394232575409549035, 54.00000000000000711 ) ) ;
#5461 = CARTESIAN_POINT ( 'NONE',  ( 10.00000000000000000, 21.00000000000000000, -18.00000000000000355 ) ) ;
#5462 = VECTOR ( 'NONE', #61426, 1000.000000000000000 ) ;
#5463 = ORIENTED_EDGE ( 'NONE', *, *, #10741, .F. ) ;
#5464 = DIRECTION ( 'NONE',  ( 0.000000000000000000, 0.000000000000000000, -1.000000000000000000 ) ) ;
#5465 = LINE ( 'NONE', #53548, #69332 ) ;
#5466 = VERTEX_POINT ( 'NONE', #56773 ) ;
#5467 = DIRECTION ( 'NONE',  ( -1.000000000000000000, 0.000000000000000000, -0.000000000000000000 ) ) ;
#5468 = CARTESIAN_POINT ( 'NONE',  ( 4.406483450353335662, -11.78648345035337996, 195.0000000000000284 ) ) ;
#5469 = VERTEX_POINT ( 'NONE', #45112 ) ;
#5470 = DIRECTION ( 'NONE',  ( 0.000000000000000000, -1.000000000000000000, 0.000000000000000000 ) ) ;
#5471 = DIRECTION ( 'NONE',  ( 0.000000000000000000, 1.000000000000000000, -0.000000000000000000 ) ) ;
#5472 = CARTESIAN_POINT ( 'NONE',  ( -15.50000000000000000, -0.4000000000005236034, -19.20000000000052509 ) ) ;
#5473 = DIRECTION ( 'NONE',  ( 0.8660254037844482555, 0.000000000000000000, -0.4999999999999831801 ) ) ;
#5474 = VERTEX_POINT ( 'NONE', #40511 ) ;
#5476 = VERTEX_POINT ( 'NONE', #68087 ) ;
#5475 = FACE_OUTER_BOUND ( 'NONE', #34502, .T. ) ;
#5477 = ADVANCED_FACE ( 'NONE', ( #18241 ), #61022, .F. ) ;
#5478 = AXIS2_PLACEMENT_3D ( 'NONE', #51074, #61678, #66299 ) ;
#5479 = LINE ( 'NONE', #49306, #49691 ) ;
#5480 = EDGE_CURVE ( 'NONE', #35475, #34278, #50766, .T. ) ;
#5481 = FACE_OUTER_BOUND ( 'NONE', #52020, .T. ) ;
#5482 = LINE ( 'NONE', #64870, #10450 ) ;
#5483 = ORIENTED_EDGE ( 'NONE', *, *, #6732, .F. ) ;
#5484 = EDGE_CURVE ( 'NONE', #16384, #1200, #34848, .T. ) ;
#5485 = DIRECTION ( 'NONE',  ( -1.836970198721029934E-16, 1.836970198721036344E-16, -1.000000000000000000 ) ) ;
#5486 = EDGE_CURVE ( 'NONE', #12677, #13563, #13292, .T. ) ;
#5487 = ORIENTED_EDGE ( 'NONE', *, *, #18733, .T. ) ;
#5488 = VERTEX_POINT ( 'NONE', #1988 ) ;
#5489 = EDGE_CURVE ( 'NONE', #10374, #33734, #44060, .T. ) ;
#5490 = EDGE_CURVE ( 'NONE', #67015, #21542, #62071, .T. ) ;
#5491 = ORIENTED_EDGE ( 'NONE', *, *, #55035, .T. ) ;
#5492 = EDGE_CURVE ( 'NONE', #33426, #9547, #12398, .T. ) ;
#5493 = LINE ( 'NONE', #27045, #32102 ) ;
#5494 = EDGE_CURVE ( 'NONE', #26597, #41272, #23552, .T. ) ;
#5495 = CARTESIAN_POINT ( 'NONE',  ( 9.404523737882753309, 0.9414762621171547385, 54.00000000000000711 ) ) ;
#5496 = ORIENTED_EDGE ( 'NONE', *, *, #60049, .F. ) ;
#5497 = ORIENTED_EDGE ( 'NONE', *, *, #21383, .F. ) ;
#5498 = CARTESIAN_POINT ( 'NONE',  ( 4.456444791733522252E-16, 7.450000000000002842, -24.50000000000000000 ) ) ;
#5499 = ORIENTED_EDGE ( 'NONE', *, *, #10003, .T. ) ;
#5500 = ORIENTED_EDGE ( 'NONE', *, *, #38404, .F. ) ;
#5501 = VERTEX_POINT ( 'NONE', #23902 ) ;
#5502 = VERTEX_POINT ( 'NONE', #34498 ) ;
#5503 = DIRECTION ( 'NONE',  ( 0.000000000000000000, 0.000000000000000000, -1.000000000000000000 ) ) ;
#5504 = UNCERTAINTY_MEASURE_WITH_UNIT (LENGTH_MEASURE( 1.000000000000000082E-05 ), #41262, 'distance_accuracy_value', 'NONE');
#5506 = ORIENTED_EDGE ( 'NONE', *, *, #3430, .T. ) ;
#5505 = CARTESIAN_POINT ( 'NONE',  ( 9.841277389592722358, -2.290483450353395067, 195.0000000000000284 ) ) ;
#5507 = PLANE ( 'NONE',  #44699 ) ;
#5508 = CARTESIAN_POINT ( 'NONE',  ( -7.813516549646711162, 11.77351654964660277, 455.0000000000000568 ) ) ;
#5509 = CARTESIAN_POINT ( 'NONE',  ( 14.50000000000000000, -42.50000000000000000, 15.10000000000000142 ) ) ;
#5510 = ORIENTED_EDGE ( 'NONE', *, *, #41287, .F. ) ;
#5511 = AXIS2_PLACEMENT_3D ( 'NONE', #11833, #12185, #39747 ) ;
#5512 = CARTESIAN_POINT ( 'NONE',  ( -14.25000000000000000, -0.2038245569916330158, 23.22168783648699986 ) ) ;
#5513 = DIRECTION ( 'NONE',  ( 0.000000000000000000, 1.000000000000000000, 0.000000000000000000 ) ) ;
#5514 = ORIENTED_EDGE ( 'NONE', *, *, #19273, .F. ) ;
#5515 = CARTESIAN_POINT ( 'NONE',  ( 9.900000000000000355, -18.00000000000000355, 21.00000000000000000 ) ) ;
#5516 = VECTOR ( 'NONE', #32137, 1000.000000000000000 ) ;
#5517 = CYLINDRICAL_SURFACE ( 'NONE', #48092, 0.1749999999999980738 ) ;
#5518 = DIRECTION ( 'NONE',  ( -0.000000000000000000, -0.000000000000000000, 1.000000000000000000 ) ) ;
#5519 = ORIENTED_EDGE ( 'NONE', *, *, #6978, .F. ) ;
#5520 = LINE ( 'NONE', #20381, #27914 ) ;
#5521 = ADVANCED_FACE ( 'NONE', ( #18589 ), #40153, .F. ) ;
#5522 = CARTESIAN_POINT ( 'NONE',  ( 9.690000000000001279, 9.750000000000001776, -5.000000000000000000 ) ) ;
#5523 = PLANE ( 'NONE',  #14452 ) ;
#5524 = EDGE_CURVE ( 'NONE', #23882, #51221, #24253, .T. ) ;
#5525 = CARTESIAN_POINT ( 'NONE',  ( 4.149127210878726935, -6.836383711243002814, 54.00000000000000711 ) ) ;
#5526 = LINE ( 'NONE', #54658, #871 ) ;
#5527 = LINE ( 'NONE', #54659, #12428 ) ;
#5528 = DIRECTION ( 'NONE',  ( -0.7071067811865527908, -0.7071067811865422437, 0.000000000000000000 ) ) ;
#5529 = LINE ( 'NONE', #25714, #23245 ) ;
#5530 = ORIENTED_EDGE ( 'NONE', *, *, #22139, .F. ) ;
#5531 = LINE ( 'NONE', #5879, #47299 ) ;
#5532 = ADVANCED_FACE ( 'NONE', ( #35545 ), #57128, .T. ) ;
#5533 = CARTESIAN_POINT ( 'NONE',  ( 0.2500000000000124345, -0.2499999999999875933, -26.74999999999999289 ) ) ;
#5534 = CARTESIAN_POINT ( 'NONE',  ( 8.250000000000005329, -8.249999999999998224, -26.00000000000001066 ) ) ;
#5535 = CARTESIAN_POINT ( 'NONE',  ( 11.00000000000000000, -14.33999999999999986, 14.50000000000000000 ) ) ;
#5536 = ORIENTED_EDGE ( 'NONE', *, *, #53905, .F. ) ;
#5537 = CYLINDRICAL_SURFACE ( 'NONE', #7290, 1.224999999999999423 ) ;
#5538 = CARTESIAN_POINT ( 'NONE',  ( 7.250000000000005329, -7.449999999999998401, -7.500000000000000000 ) ) ;
#5539 = EDGE_CURVE ( 'NONE', #38308, #43722, #4102, .T. ) ;
#5540 = DIRECTION ( 'NONE',  ( 0.000000000000000000, 0.000000000000000000, -1.000000000000000000 ) ) ;
#5541 = VECTOR ( 'NONE', #66340, 1000.000000000000000 ) ;
#5542 = DIRECTION ( 'NONE',  ( 1.000000000000000000, 0.000000000000000000, 0.000000000000000000 ) ) ;
#5543 = DIRECTION ( 'NONE',  ( -1.794541526872559352E-16, -1.000000000000000000, 0.000000000000000000 ) ) ;
#5544 = LINE ( 'NONE', #10838, #61036 ) ;
#5545 = ORIENTED_EDGE ( 'NONE', *, *, #63518, .T. ) ;
#5546 = VECTOR ( 'NONE', #38937, 1000.000000000000000 ) ;
#5547 = ORIENTED_EDGE ( 'NONE', *, *, #25288, .F. ) ;
#5548 = DIRECTION ( 'NONE',  ( 0.000000000000000000, -0.9938079899998859545, 0.1111111111112941946 ) ) ;
#5549 = EDGE_CURVE ( 'NONE', #21753, #59333, #30610, .T. ) ;
#5550 = CARTESIAN_POINT ( 'NONE',  ( -7.250000000000000888, 7.250000000000001776, -14.50000000000000000 ) ) ;
#5551 = VERTEX_POINT ( 'NONE', #52178 ) ;
#5552 = FACE_OUTER_BOUND ( 'NONE', #16121, .T. ) ;
#5553 = CIRCLE ( 'NONE', #37209, 1.000000000000000000 ) ;
#5554 = CARTESIAN_POINT ( 'NONE',  ( 24.90000000000000213, 13.66939075806899240, -20.79999999999999361 ) ) ;
#5555 = VERTEX_POINT ( 'NONE', #36983 ) ;
#5556 = VECTOR ( 'NONE', #68758, 1000.000000000000000 ) ;
#5557 = CARTESIAN_POINT ( 'NONE',  ( -29.25000000000000000, -5.200000000000001066, -11.75000000000000000 ) ) ;
#5558 = EDGE_LOOP ( 'NONE', ( #13980, #4677, #40424, #49067 ) ) ;
#5559 = VERTEX_POINT ( 'NONE', #68447 ) ;
#5561 = EDGE_CURVE ( 'NONE', #5255, #45628, #15403, .T. ) ;
#5560 = DIRECTION ( 'NONE',  ( 1.000000000000000000, -0.000000000000000000, -0.000000000000000000 ) ) ;
#5562 = ORIENTED_EDGE ( 'NONE', *, *, #53602, .T. ) ;
#5563 = CARTESIAN_POINT ( 'NONE',  ( -6.822336235477489019, -6.364920264886855250, 54.00000000000000711 ) ) ;
#5564 = EDGE_CURVE ( 'NONE', #18299, #36802, #4793, .T. ) ;
#5565 = CIRCLE ( 'NONE', #45054, 0.1749999999999998224 ) ;
#5566 = DIRECTION ( 'NONE',  ( 0.000000000000000000, 0.000000000000000000, -1.000000000000000000 ) ) ;
#5567 = CARTESIAN_POINT ( 'NONE',  ( 15.00000000000000000, 0.000000000000000000, 0.000000000000000000 ) ) ;
#5568 = ORIENTED_EDGE ( 'NONE', *, *, #49526, .F. ) ;
#5569 = ORIENTED_EDGE ( 'NONE', *, *, #45750, .F. ) ;
#5570 = CARTESIAN_POINT ( 'NONE',  ( 8.406483450353404052, 6.331612867284015955, 455.0000000000000568 ) ) ;
#5573 = CARTESIAN_POINT ( 'NONE',  ( 25.50000000000000355, -5.578999999999999737, 20.87899999999999778 ) ) ;
#5572 = DIRECTION ( 'NONE',  ( 1.836970198721029934E-16, 1.836970198721010706E-16, -1.000000000000000000 ) ) ;
#5571 = VECTOR ( 'NONE', #30815, 1000.000000000000114 ) ;
#5574 = ORIENTED_EDGE ( 'NONE', *, *, #28356, .F. ) ;
#5575 = EDGE_CURVE ( 'NONE', #35722, #52775, #46861, .T. ) ;
#5576 = ORIENTED_EDGE ( 'NONE', *, *, #16015, .T. ) ;
#5578 = VERTEX_POINT ( 'NONE', #21050 ) ;
#5577 = ITEM_DEFINED_TRANSFORMATION ( 'NONE', 'NONE', #48258,  #45918 ) ;
#5579 = LINE ( 'NONE', #32096, #19763 ) ;
#5581 = ORIENTED_EDGE ( 'NONE', *, *, #32046, .T. ) ;
#5580 = DIRECTION ( 'NONE',  ( 1.000000000000000000, -0.000000000000000000, 0.000000000000000000 ) ) ;
#5582 = LINE ( 'NONE', #21836, #50316 ) ;
#5583 = DIRECTION ( 'NONE',  ( 0.000000000000000000, 0.000000000000000000, 1.000000000000000000 ) ) ;
#5584 = EDGE_LOOP ( 'NONE', ( #58968, #62665, #21953, #68941 ) ) ;
#5585 = ORIENTED_EDGE ( 'NONE', *, *, #8302, .T. ) ;
#5586 = DIRECTION ( 'NONE',  ( -2.135044278125299371E-15, -1.000000000000000000, -3.673940397442060361E-16 ) ) ;
#5587 = ORIENTED_EDGE ( 'NONE', *, *, #61652, .F. ) ;
#5588 = EDGE_CURVE ( 'NONE', #1729, #64431, #9753, .T. ) ;
#5589 = LINE ( 'NONE', #48722, #30388 ) ;
#5590 = DIRECTION ( 'NONE',  ( -1.000000000000000000, 0.000000000000000000, 0.000000000000000000 ) ) ;
#5591 = ORIENTED_EDGE ( 'NONE', *, *, #63078, .T. ) ;
#5592 = AXIS2_PLACEMENT_3D ( 'NONE', #9456, #20409, #4512 ) ;
#5593 = CIRCLE ( 'NONE', #45089, 5.250000000000000000 ) ;
#5594 = EDGE_CURVE ( 'NONE', #4689, #10719, #6807, .T. ) ;
#5595 = CARTESIAN_POINT ( 'NONE',  ( 9.737023737882816832, -6.832023737882813919, 26.00000000000000000 ) ) ;
#5596 = LINE ( 'NONE', #20805, #9845 ) ;
#5598 = ORIENTED_EDGE ( 'NONE', *, *, #44976, .F. ) ;
#5597 = PLANE ( 'NONE',  #8270 ) ;
#5599 = VERTEX_POINT ( 'NONE', #19638 ) ;
#5600 = EDGE_CURVE ( 'NONE', #24192, #11455, #20351, .T. ) ;
#5601 = LINE ( 'NONE', #6964, #13650 ) ;
#5602 = CONICAL_SURFACE ( 'NONE', #3327, 4.000000000000000000, 0.7853981633974730370 ) ;
#5603 = FACE_OUTER_BOUND ( 'NONE', #45191, .T. ) ;
#5604 = EDGE_CURVE ( 'NONE', #44650, #10374, #52534, .T. ) ;
#5605 = CARTESIAN_POINT ( 'NONE',  ( 46.39999999999999858, 33.00000000000000000, 2.250000000000000444 ) ) ;
#5606 = CARTESIAN_POINT ( 'NONE',  ( 7.428221114745003462, -3.006483450353490294, 455.0000000000000568 ) ) ;
#5607 = CIRCLE ( 'NONE', #23649, 0.3499999999999996447 ) ;
#5608 = EDGE_CURVE ( 'NONE', #8160, #26381, #57596, .T. ) ;
#5609 = CARTESIAN_POINT ( 'NONE',  ( 9.562023737882801910, 8.130476262117189989, 26.00000000000000711 ) ) ;
#5610 = VERTEX_POINT ( 'NONE', #10440 ) ;
#5611 = PLANE ( 'NONE',  #33538 ) ;
#5612 = CARTESIAN_POINT ( 'NONE',  ( -7.593516549646711411, 11.31351654964660014, 195.0000000000000284 ) ) ;
#5613 = LINE ( 'NONE', #27182, #20863 ) ;
#5614 = AXIS2_PLACEMENT_3D ( 'NONE', #13253, #51439, #18916 ) ;
#5616 = ORIENTED_EDGE ( 'NONE', *, *, #2822, .T. ) ;
#5615 = DIRECTION ( 'NONE',  ( 1.000000000000000000, 0.000000000000000000, 0.000000000000000000 ) ) ;
#5617 = DIRECTION ( 'NONE',  ( 0.000000000000000000, 0.000000000000000000, 1.000000000000000000 ) ) ;
#5618 = EDGE_CURVE ( 'NONE', #61956, #8473, #63840, .T. ) ;
#5619 = CARTESIAN_POINT ( 'NONE',  ( 7.186223737882794893, 5.242976262117198694, 26.00000000000000711 ) ) ;
#5620 = EDGE_CURVE ( 'NONE', #5167, #31147, #47919, .T. ) ;
#5621 = AXIS2_PLACEMENT_3D ( 'NONE', #64277, #42348, #63928 ) ;
#5622 = DIRECTION ( 'NONE',  ( 0.000000000000000000, -3.673940397442059868E-16, 1.000000000000000000 ) ) ;
#5623 = ORIENTED_EDGE ( 'NONE', *, *, #8037, .T. ) ;
#5624 = CARTESIAN_POINT ( 'NONE',  ( 11.75000000000000000, -5.000000000000000000, 11.75000000000000000 ) ) ;
#5625 = DIRECTION ( 'NONE',  ( -0.000000000000000000, -0.000000000000000000, -1.000000000000000000 ) ) ;
#5626 = ORIENTED_EDGE ( 'NONE', *, *, #47324, .T. ) ;
#5627 = CARTESIAN_POINT ( 'NONE',  ( -30.00000000000000000, -13.79999999999979998, 17.30000000000000071 ) ) ;
#5628 = ADVANCED_FACE ( 'NONE', ( #25677 ), #32017, .F. ) ;
#5629 = ADVANCED_FACE ( 'NONE', ( #35917 ), #57825, .T. ) ;
#5630 = CARTESIAN_POINT ( 'NONE',  ( -10.91351654964670814, 9.093516549646603053, 455.0000000000000568 ) ) ;
#5631 = PLANE ( 'NONE',  #42231 ) ;
#5632 = CARTESIAN_POINT ( 'NONE',  ( 7.000000000000000000, -26.42999999999999972, -9.412893218813501051 ) ) ;
#5633 = EDGE_CURVE ( 'NONE', #68720, #41169, #41799, .T. ) ;
#5634 = CARTESIAN_POINT ( 'NONE',  ( 0.000000000000000000, -7.449999999999998401, -14.00000000000000000 ) ) ;
#5635 = ORIENTED_EDGE ( 'NONE', *, *, #37687, .T. ) ;
#5636 = VERTEX_POINT ( 'NONE', #41915 ) ;
#5637 = FACE_OUTER_BOUND ( 'NONE', #61995, .T. ) ;
#5638 = VECTOR ( 'NONE', #32023, 1000.000000000000000 ) ;
#5639 = ORIENTED_EDGE ( 'NONE', *, *, #63017, .F. ) ;
#5640 = CARTESIAN_POINT ( 'NONE',  ( -2.355476262117229158, 9.547976262117156665, 54.00000000000000711 ) ) ;
#5641 = VERTEX_POINT ( 'NONE', #63493 ) ;
#5642 = CARTESIAN_POINT ( 'NONE',  ( -25.50000000000000355, 0.000000000000000000, 20.24999999999999645 ) ) ;
#5643 = LINE ( 'NONE', #32855, #60398 ) ;
#5644 = DIRECTION ( 'NONE',  ( 1.836970198721029934E-16, 1.836970198721010706E-16, -1.000000000000000000 ) ) ;
#5645 = ORIENTED_EDGE ( 'NONE', *, *, #22848, .T. ) ;
#5646 =( REPRESENTATION_RELATIONSHIP ('NONE','NONE', #33057, #4299 ) REPRESENTATION_RELATIONSHIP_WITH_TRANSFORMATION ( #36707 )SHAPE_REPRESENTATION_RELATIONSHIP( ) );
#5647 = ORIENTED_EDGE ( 'NONE', *, *, #48646, .F. ) ;
#5649 = EDGE_CURVE ( 'NONE', #46357, #50590, #15050, .T. ) ;
#5648 = LINE ( 'NONE', #37822, #23955 ) ;
#5650 = AXIS2_PLACEMENT_3D ( 'NONE', #48951, #48600, #172 ) ;
#5651 = EDGE_LOOP ( 'NONE', ( #59588, #14682, #30911, #68451 ) ) ;
#5652 = AXIS2_PLACEMENT_3D ( 'NONE', #57551, #15130, #52616 ) ;
#5653 = ORIENTED_EDGE ( 'NONE', *, *, #14984, .F. ) ;
#5654 = EDGE_CURVE ( 'NONE', #67578, #10486, #31336, .T. ) ;
#5655 = CARTESIAN_POINT ( 'NONE',  ( 14.50000000000000000, -42.50000000000000000, -26.50000000000000000 ) ) ;
#5656 = LINE ( 'NONE', #47733, #4207 ) ;
#5658 = CARTESIAN_POINT ( 'NONE',  ( 0.000000000000000000, -42.00000000000000000, -26.50000000000000000 ) ) ;
#5657 = VECTOR ( 'NONE', #23256, 1000.000000000000000 ) ;
#5659 = ORIENTED_EDGE ( 'NONE', *, *, #37991, .T. ) ;
#5660 = CIRCLE ( 'NONE', #50796, 4.000000000000000888 ) ;
#5661 = CARTESIAN_POINT ( 'NONE',  ( -11.47551654964667733, 10.19191654964664018, 455.0000000000000568 ) ) ;
#5663 = DIRECTION ( 'NONE',  ( 0.000000000000000000, -1.000000000000000000, 0.000000000000000000 ) ) ;
#5662 = DIRECTION ( 'NONE',  ( 0.000000000000000000, -0.1111111111108840643, -0.9938079899999319178 ) ) ;
#5664 = VERTEX_POINT ( 'NONE', #42960 ) ;
#5665 = VERTEX_POINT ( 'NONE', #54982 ) ;
#5667 = VERTEX_POINT ( 'NONE', #22097 ) ;
#5666 = CARTESIAN_POINT ( 'NONE',  ( -6.486996718459913325, -3.157023737882783454, 54.00000000000000711 ) ) ;
#5668 = ORIENTED_EDGE ( 'NONE', *, *, #36325, .F. ) ;
#5669 = CIRCLE ( 'NONE', #59809, 0.5249999999999990230 ) ;
#5670 = DIRECTION ( 'NONE',  ( 0.000000000000000000, -1.000000000000000000, 0.000000000000000000 ) ) ;
#5671 = CIRCLE ( 'NONE', #45149, 0.2000000000000005107 ) ;
#5672 = CARTESIAN_POINT ( 'NONE',  ( 4.740315990920131561, -7.811466277050742590, 195.0000000000000284 ) ) ;
#5673 = ORIENTED_EDGE ( 'NONE', *, *, #43160, .T. ) ;
#5674 = ORIENTED_EDGE ( 'NONE', *, *, #15461, .T. ) ;
#5675 = VECTOR ( 'NONE', #17075, 1000.000000000000000 ) ;
#5676 = AXIS2_PLACEMENT_3D ( 'NONE', #5138, #25309, #69486 ) ;
#5677 = DIRECTION ( 'NONE',  ( -1.000000000000000000, 0.000000000000000000, 0.000000000000000000 ) ) ;
#5678 = DIRECTION ( 'NONE',  ( -1.000000000000000000, 0.000000000000000000, 0.000000000000000000 ) ) ;
#5679 = EDGE_LOOP ( 'NONE', ( #56881, #54792, #37840, #26266 ) ) ;
#5680 = ORIENTED_EDGE ( 'NONE', *, *, #38569, .F. ) ;
#5681 = DIRECTION ( 'NONE',  ( -1.794541526872559352E-16, -1.000000000000000000, 0.000000000000000000 ) ) ;
#5682 = CARTESIAN_POINT ( 'NONE',  ( 30.00000000000000000, -9.200000000000120082, 17.64999999999993108 ) ) ;
#5683 = CARTESIAN_POINT ( 'NONE',  ( 34.89999999999999858, -14.06939075806900874, 20.80000000000001137 ) ) ;
#5684 = ORIENTED_EDGE ( 'NONE', *, *, #51339, .F. ) ;
#5685 = EDGE_CURVE ( 'NONE', #36105, #19358, #59920, .T. ) ;
#5686 = CARTESIAN_POINT ( 'NONE',  ( -7.250000000000001776, -7.249999999999998224, -16.50000000000000000 ) ) ;
#5687 = AXIS2_PLACEMENT_3D ( 'NONE', #13387, #7723, #46261 ) ;
#5688 = DIRECTION ( 'NONE',  ( -1.000000000000000000, 0.000000000000000000, 0.000000000000000000 ) ) ;
#5690 = ORIENTED_EDGE ( 'NONE', *, *, #2890, .F. ) ;
#5689 = CARTESIAN_POINT ( 'NONE',  ( -7.290476262117262962, 9.722976262117180468, 26.00000000000000711 ) ) ;
#5692 = ORIENTED_EDGE ( 'NONE', *, *, #41564, .T. ) ;
#5691 = CARTESIAN_POINT ( 'NONE',  ( 49.00000000000000000, 13.66939075806899950, 20.80000000000000426 ) ) ;
#5693 = EDGE_CURVE ( 'NONE', #21000, #28585, #47455, .T. ) ;
#5694 = PLANE ( 'NONE',  #31693 ) ;
#5695 = DIRECTION ( 'NONE',  ( 0.000000000000000000, 0.000000000000000000, -1.000000000000000000 ) ) ;
#5696 = ADVANCED_FACE ( 'NONE', ( #6537 ), #65246, .T. ) ;
#5697 = CARTESIAN_POINT ( 'NONE',  ( -8.689999999999999503, -8.750000000000000000, -7.000000000000000000 ) ) ;
#5698 = EDGE_CURVE ( 'NONE', #33150, #36374, #10210, .T. ) ;
#5699 = DIRECTION ( 'NONE',  ( -1.000000000000000000, 0.000000000000000000, 0.000000000000000000 ) ) ;
#5700 = CARTESIAN_POINT ( 'NONE',  ( 83.97321854994621049, 47.95351654967443977, 20.00000000000000000 ) ) ;
#5701 = ADVANCED_FACE ( 'NONE', ( #11469 ), #33733, .F. ) ;
#5702 = EDGE_CURVE ( 'NONE', #40029, #44854, #55316, .T. ) ;
#5703 = PLANE ( 'NONE',  #45063 ) ;
#5704 = ORIENTED_EDGE ( 'NONE', *, *, #69230, .F. ) ;
#5705 = DIRECTION ( 'NONE',  ( 0.000000000000000000, 0.000000000000000000, 1.000000000000000000 ) ) ;
#5706 = AXIS2_PLACEMENT_3D ( 'NONE', #8519, #20535, #47408 ) ;
#5708 = VERTEX_POINT ( 'NONE', #65576 ) ;
#5707 = FACE_OUTER_BOUND ( 'NONE', #33094, .T. ) ;
#5710 = ORIENTED_EDGE ( 'NONE', *, *, #50109, .T. ) ;
#5709 = CYLINDRICAL_SURFACE ( 'NONE', #36695, 0.3499999999999302558 ) ;
#5711 = CARTESIAN_POINT ( 'NONE',  ( 38.90000000000000568, 0.000000000000000000, 2.458500000000000796 ) ) ;
#5712 = CARTESIAN_POINT ( 'NONE',  ( 14.24999999999999822, -0.3152037684892591285, -22.25410949791979220 ) ) ;
#5713 = AXIS2_PLACEMENT_3D ( 'NONE', #37702, #28128, #565 ) ;
#5714 = VERTEX_POINT ( 'NONE', #33047 ) ;
#5715 = DIRECTION ( 'NONE',  ( 1.000000000000000000, 0.000000000000000000, 0.000000000000000000 ) ) ;
#5716 = DIRECTION ( 'NONE',  ( 0.000000000000000000, -1.000000000000000000, 0.000000000000000000 ) ) ;
#5717 = ORIENTED_EDGE ( 'NONE', *, *, #18235, .T. ) ;
#5718 = VECTOR ( 'NONE', #54758, 1000.000000000000000 ) ;
#5719 = LINE ( 'NONE', #42490, #23300 ) ;
#5720 = DIRECTION ( 'NONE',  ( -4.956352788505168198E-15, -1.000000000000000000, 0.000000000000000000 ) ) ;
#5721 = DIRECTION ( 'NONE',  ( 0.000000000000000000, -0.000000000000000000, 1.000000000000000000 ) ) ;
#5722 = VECTOR ( 'NONE', #54210, 1000.000000000000000 ) ;
#5723 = ORIENTED_EDGE ( 'NONE', *, *, #40940, .T. ) ;
#5724 = CARTESIAN_POINT ( 'NONE',  ( 7.250000000000005329, -7.249999999999998224, -19.50000000000000000 ) ) ;
#5725 = ORIENTED_EDGE ( 'NONE', *, *, #9775, .F. ) ;
#5726 = ORIENTED_EDGE ( 'NONE', *, *, #26304, .T. ) ;
#5727 = DIRECTION ( 'NONE',  ( 0.000000000000000000, 1.000000000000000000, 0.000000000000000000 ) ) ;
#5728 = VECTOR ( 'NONE', #2886, 1000.000000000000000 ) ;
#5729 = DIRECTION ( 'NONE',  ( 0.000000000000000000, 0.000000000000000000, -1.000000000000000000 ) ) ;
#5730 = CIRCLE ( 'NONE', #27170, 0.9999999999999991118 ) ;
#5731 = CARTESIAN_POINT ( 'NONE',  ( 11.25000000000000178, -11.18999999999999950, -5.000000000000000000 ) ) ;
#5732 = DIRECTION ( 'NONE',  ( 1.130039751537441866E-14, 1.000000000000000000, 1.836970198721015636E-16 ) ) ;
#5733 = ORIENTED_EDGE ( 'NONE', *, *, #65871, .F. ) ;
#5734 = ORIENTED_EDGE ( 'NONE', *, *, #61380, .F. ) ;
#5736 = EDGE_LOOP ( 'NONE', ( #18532, #64339, #15202, #56601 ) ) ;
#5735 = LINE ( 'NONE', #27302, #2407 ) ;
#5737 = VERTEX_POINT ( 'NONE', #60612 ) ;
#5738 = ADVANCED_FACE ( 'NONE', ( #48621 ), #49652, .F. ) ;
#5739 = LINE ( 'NONE', #27305, #33742 ) ;
#5740 = FACE_OUTER_BOUND ( 'NONE', #35982, .T. ) ;
#5741 = AXIS2_PLACEMENT_3D ( 'NONE', #3303, #36527, #69406 ) ;
#5742 = DIRECTION ( 'NONE',  ( 0.000000000000000000, 0.000000000000000000, 1.000000000000000000 ) ) ;
#5743 = EDGE_CURVE ( 'NONE', #12124, #56899, #37669, .T. ) ;
#5744 = LINE ( 'NONE', #12063, #13049 ) ;
#5746 = DIRECTION ( 'NONE',  ( -0.000000000000000000, 0.000000000000000000, 1.000000000000000000 ) ) ;
#5745 = CARTESIAN_POINT ( 'NONE',  ( -10.91351654964670637, 9.293516549646604119, 455.0000000000000568 ) ) ;
#5747 = VERTEX_POINT ( 'NONE', #60255 ) ;
#5749 = ORIENTED_EDGE ( 'NONE', *, *, #33259, .T. ) ;
#5748 = CARTESIAN_POINT ( 'NONE',  ( -3.142976262117261221, 4.031976262117183296, 54.00000000000000711 ) ) ;
#5750 = VERTEX_POINT ( 'NONE', #6181 ) ;
#5751 = ORIENTED_EDGE ( 'NONE', *, *, #23728, .T. ) ;
#5752 = LINE ( 'NONE', #17045, #9661 ) ;
#5753 = CARTESIAN_POINT ( 'NONE',  ( 0.000000000000000000, 0.000000000000000000, -1.000000000000000000 ) ) ;
#5754 = AXIS2_PLACEMENT_3D ( 'NONE', #17146, #10198, #58294 ) ;
#5755 = CARTESIAN_POINT ( 'NONE',  ( -4.188533722949335569, 7.259684009079808931, 455.0000000000000568 ) ) ;
#5756 = VECTOR ( 'NONE', #43495, 1000.000000000000000 ) ;
#5757 = EDGE_LOOP ( 'NONE', ( #9318, #8855, #67262, #44592 ) ) ;
#5758 = ORIENTED_EDGE ( 'NONE', *, *, #11901, .F. ) ;
#5759 = ORIENTED_EDGE ( 'NONE', *, *, #12475, .F. ) ;
#5760 = CIRCLE ( 'NONE', #15949, 1.000000000000000000 ) ;
#5761 = DIRECTION ( 'NONE',  ( -2.135044278125299371E-15, -1.000000000000000000, 0.000000000000000000 ) ) ;
#5762 = CARTESIAN_POINT ( 'NONE',  ( 7.969523737882813208, 8.821682069070710952, 54.00000000000000711 ) ) ;
#5763 = CARTESIAN_POINT ( 'NONE',  ( -3.663616288757094885, -6.364920264886888113, 54.00000000000000711 ) ) ;
#5764 = ORIENTED_EDGE ( 'NONE', *, *, #47528, .T. ) ;
#5765 = VECTOR ( 'NONE', #13266, 1000.000000000000000 ) ;
#5766 = VECTOR ( 'NONE', #20420, 1000.000000000000000 ) ;
#5767 = ORIENTED_EDGE ( 'NONE', *, *, #22268, .F. ) ;
#5768 = CARTESIAN_POINT ( 'NONE',  ( -9.722976262117256852, 7.955476262117183062, 54.00000000000000711 ) ) ;
#5769 = PLANE ( 'NONE',  #60499 ) ;
#5770 = ORIENTED_EDGE ( 'NONE', *, *, #41642, .T. ) ;
#5771 = AXIS2_PLACEMENT_3D ( 'NONE', #16771, #54257, #32677 ) ;
#5772 = ADVANCED_FACE ( 'NONE', ( #43996 ), #6854, .F. ) ;
#5773 = CARTESIAN_POINT ( 'NONE',  ( -10.49297626211725998, 9.781776262117173104, 26.00000000000000711 ) ) ;
#5775 = ORIENTED_EDGE ( 'NONE', *, *, #62161, .T. ) ;
#5774 = CARTESIAN_POINT ( 'NONE',  ( 283.0000000000000568, -25.56180396883900130, 14.25872597390799967 ) ) ;
#5776 = EDGE_LOOP ( 'NONE', ( #9566, #50589, #67407, #7637, #8249, #31339, #56998, #65191, #2260, #3034, #22347, #689, #49334, #63412, #65098, #28427, #19783, #45336, #58783, #44411, #12300, #22757, #68331, #40785, #25259, #43881, #17651, #50763, #41714, #57478, #63768, #21621, #31028, #5767, #63161, #958, #10464, #31887, #60563, #52535, #26625, #20816, #35464, #17183, #57949, #42703, #31556, #11568, #27091, #1187, #44095, #33885, #16811, #39956, #59652, #49638 ) ) ;
#5778 = LINE ( 'NONE', #58491, #59765 ) ;
#5777 = CIRCLE ( 'NONE', #14804, 0.2000000000000005107 ) ;
#5779 = DIRECTION ( 'NONE',  ( 3.717264591378874374E-15, 1.000000000000000000, 0.000000000000000000 ) ) ;
#5780 = DIRECTION ( 'NONE',  ( -1.000000000000000000, 0.000000000000000000, 0.000000000000000000 ) ) ;
#5781 = EDGE_CURVE ( 'NONE', #53834, #16791, #1225, .T. ) ;
#5782 = EDGE_CURVE ( 'NONE', #31198, #39723, #28422, .T. ) ;
#5783 = CARTESIAN_POINT ( 'NONE',  ( 9.912023737882776686, 3.667976262117155883, 26.00000000000000711 ) ) ;
#5784 = DIRECTION ( 'NONE',  ( -0.7071067811865435759, 0.7071067811865515695, 0.000000000000000000 ) ) ;
#5785 = EDGE_CURVE ( 'NONE', #61969, #21985, #17473, .T. ) ;
#5786 = ADVANCED_FACE ( 'NONE', ( #10778 ), #32362, .F. ) ;
#5787 = VERTEX_POINT ( 'NONE', #43308 ) ;
#5788 = LINE ( 'NONE', #53533, #69898 ) ;
#5789 = ORIENTED_EDGE ( 'NONE', *, *, #42442, .T. ) ;
#5790 = LINE ( 'NONE', #27355, #27611 ) ;
#5791 = CARTESIAN_POINT ( 'NONE',  ( -9.093516549646780689, -10.92648345035334145, 195.0000000000000284 ) ) ;
#5792 = EDGE_CURVE ( 'NONE', #54079, #5667, #7961, .T. ) ;
#5793 = CIRCLE ( 'NONE', #49778, 3.499999999999855227 ) ;
#5794 = DIRECTION ( 'NONE',  ( 1.836970198721029934E-16, 1.836970198721010706E-16, -1.000000000000000000 ) ) ;
#5795 = LINE ( 'NONE', #22402, #64527 ) ;
#5796 = LINE ( 'NONE', #54582, #65286 ) ;
#5797 = VERTEX_POINT ( 'NONE', #27401 ) ;
#5798 = DIRECTION ( 'NONE',  ( 0.000000000000000000, 0.000000000000000000, -1.000000000000000000 ) ) ;
#5799 = AXIS2_PLACEMENT_3D ( 'NONE', #24098, #66876, #18432 ) ;
#5800 = CARTESIAN_POINT ( 'NONE',  ( -9.689726262117325462, -10.05377373788272166, 26.00000000000000000 ) ) ;
#5801 = VECTOR ( 'NONE', #8883, 1000.000000000000000 ) ;
#5802 = ORIENTED_EDGE ( 'NONE', *, *, #60971, .F. ) ;
#5803 = LINE ( 'NONE', #59880, #47347 ) ;
#5804 = LINE ( 'NONE', #43628, #23084 ) ;
#5805 = ORIENTED_EDGE ( 'NONE', *, *, #60886, .T. ) ;
#5806 = CARTESIAN_POINT ( 'NONE',  ( 39.00000000000000000, 16.96999999999999886, 21.00000000000000000 ) ) ;
#5807 = CARTESIAN_POINT ( 'NONE',  ( 78.77321854994620765, 47.95351654967443977, 40.00000000000000000 ) ) ;
#5808 = EDGE_LOOP ( 'NONE', ( #30080, #576, #66937, #23035 ) ) ;
#5809 = DIRECTION ( 'NONE',  ( -0.000000000000000000, -0.000000000000000000, -1.000000000000000000 ) ) ;
#5810 = CARTESIAN_POINT ( 'NONE',  ( 30.00000000000000000, -9.454754784057099570, 17.53999999999999915 ) ) ;
#5811 = AXIS2_PLACEMENT_3D ( 'NONE', #59204, #37994, #11109 ) ;
#5812 = AXIS2_PLACEMENT_3D ( 'NONE', #29186, #39453, #17889 ) ;
#5813 = CYLINDRICAL_SURFACE ( 'NONE', #4962, 1.000000000000002665 ) ;
#5814 = LINE ( 'NONE', #12137, #1256 ) ;
#5815 = ORIENTED_EDGE ( 'NONE', *, *, #8037, .F. ) ;
#5817 = VERTEX_POINT ( 'NONE', #34408 ) ;
#5816 = FACE_OUTER_BOUND ( 'NONE', #69491, .T. ) ;
#5818 = VECTOR ( 'NONE', #30151, 1000.000000000000000 ) ;
#5819 = CARTESIAN_POINT ( 'NONE',  ( -7.415254214038309755, -3.606483450353353160, 195.0000000000000284 ) ) ;
#5820 = DIRECTION ( 'NONE',  ( -1.000000000000000000, 0.000000000000000000, 0.000000000000000000 ) ) ;
#5821 = CARTESIAN_POINT ( 'NONE',  ( 8.250000000000005329, 8.250000000000001776, -26.00000000000001066 ) ) ;
#5822 = ORIENTED_EDGE ( 'NONE', *, *, #68272, .F. ) ;
#5823 = EDGE_CURVE ( 'NONE', #6488, #6937, #29820, .T. ) ;
#5824 = ADVANCED_FACE ( 'NONE', ( #67311 ), #66265, .F. ) ;
#5825 = VECTOR ( 'NONE', #13859, 1000.000000000000000 ) ;
#5826 = CARTESIAN_POINT ( 'NONE',  ( 9.804883450353456098, 11.07551654964653132, 455.0000000000000568 ) ) ;
#5827 = LINE ( 'NONE', #49637, #16098 ) ;
#5828 = ORIENTED_EDGE ( 'NONE', *, *, #17065, .T. ) ;
#5829 = ORIENTED_EDGE ( 'NONE', *, *, #39275, .F. ) ;
#5830 = EDGE_CURVE ( 'NONE', #46964, #43093, #5730, .T. ) ;
#5831 = ORIENTED_EDGE ( 'NONE', *, *, #60462, .F. ) ;
#5832 = DIRECTION ( 'NONE',  ( 0.000000000000000000, -0.000000000000000000, 1.000000000000000000 ) ) ;
#5833 = DIRECTION ( 'NONE',  ( 0.000000000000000000, 0.000000000000000000, 1.000000000000000000 ) ) ;
#5834 = AXIS2_PLACEMENT_3D ( 'NONE', #50776, #23914, #45470 ) ;
#5835 = EDGE_LOOP ( 'NONE', ( #39234, #16059, #15395, #63726 ) ) ;
#5836 = ORIENTED_EDGE ( 'NONE', *, *, #40723, .F. ) ;
#5837 = ORIENTED_EDGE ( 'NONE', *, *, #46930, .T. ) ;
#5838 = DIRECTION ( 'NONE',  ( 0.000000000000000000, -0.1111111111108836896, -0.9938079899999319178 ) ) ;
#5839 = ORIENTED_EDGE ( 'NONE', *, *, #34039, .T. ) ;
#5840 = ORIENTED_EDGE ( 'NONE', *, *, #35281, .F. ) ;
#5841 = ORIENTED_EDGE ( 'NONE', *, *, #35520, .T. ) ;
#5842 = ORIENTED_EDGE ( 'NONE', *, *, #42893, .F. ) ;
#5843 = DIRECTION ( 'NONE',  ( 0.000000000000000000, 1.000000000000000000, 0.000000000000000000 ) ) ;
#5844 = CIRCLE ( 'NONE', #53300, 1.000000000000000000 ) ;
#5846 = ORIENTED_EDGE ( 'NONE', *, *, #47282, .F. ) ;
#5845 = DIRECTION ( 'NONE',  ( -1.000000000000000000, 0.000000000000000000, 0.000000000000000000 ) ) ;
#5847 = CARTESIAN_POINT ( 'NONE',  ( 40.90000000000000568, 16.96999999999999886, -21.00000000000000000 ) ) ;
#5848 = AXIS2_PLACEMENT_3D ( 'NONE', #48468, #43850, #64728 ) ;
#5849 = DIRECTION ( 'NONE',  ( 1.000000000000000000, -0.000000000000000000, -0.000000000000000000 ) ) ;
#5850 = DIRECTION ( 'NONE',  ( -1.000000000000000000, 0.000000000000000000, 0.000000000000000000 ) ) ;
#5851 = ORIENTED_EDGE ( 'NONE', *, *, #32727, .T. ) ;
#5852 = VECTOR ( 'NONE', #61519, 1000.000000000000000 ) ;
#5853 = CLOSED_SHELL ( 'NONE', ( #50046, #21725, #54852, #14534, #66643, #13406, #47801, #14301, #32297, #63488 ) ) ;
#5854 = CARTESIAN_POINT ( 'NONE',  ( 6.006483450353379716, -3.606483450353490827, 455.0000000000000568 ) ) ;
#5855 = VERTEX_POINT ( 'NONE', #18869 ) ;
#5856 = AXIS2_PLACEMENT_3D ( 'NONE', #18753, #24055, #38934 ) ;
#5857 = DIRECTION ( 'NONE',  ( -1.836970198721029934E-16, -1.836970198721010706E-16, 1.000000000000000000 ) ) ;
#5858 = EDGE_CURVE ( 'NONE', #23370, #57901, #2601, .T. ) ;
#5859 = PLANE ( 'NONE',  #50106 ) ;
#5860 = CARTESIAN_POINT ( 'NONE',  ( 8.580623737882849156, 9.689726262117156708, 54.00000000000000711 ) ) ;
#5861 = DIRECTION ( 'NONE',  ( 1.000000000000000000, 0.000000000000000000, 0.000000000000000000 ) ) ;
#5862 = EDGE_CURVE ( 'NONE', #12110, #46962, #51389, .T. ) ;
#5863 = EDGE_CURVE ( 'NONE', #3213, #55218, #9087, .T. ) ;
#5864 = ORIENTED_EDGE ( 'NONE', *, *, #13830, .T. ) ;
#5865 = CARTESIAN_POINT ( 'NONE',  ( 9.900000000000000355, 21.00000000000000000, -18.00000000000000355 ) ) ;
#5866 = VECTOR ( 'NONE', #15628, 1000.000000000000000 ) ;
#5867 = CYLINDRICAL_SURFACE ( 'NONE', #53397, 0.5249999999999990230 ) ;
#5868 = EDGE_CURVE ( 'NONE', #2526, #27219, #56696, .T. ) ;
#5869 = DIRECTION ( 'NONE',  ( 1.836970198721029934E-16, 1.836970198721010706E-16, -1.000000000000000000 ) ) ;
#5870 = PRODUCT_RELATED_PRODUCT_CATEGORY ( 'part', '', ( #37447 ) ) ;
#5871 = DIRECTION ( 'NONE',  ( 0.000000000000000000, 1.000000000000000000, 0.000000000000000000 ) ) ;
#5872 = EDGE_CURVE ( 'NONE', #30626, #58695, #41850, .T. ) ;
#5873 = PLANE ( 'NONE',  #29045 ) ;
#5874 = PLANE ( 'NONE',  #51980 ) ;
#5875 = EDGE_CURVE ( 'NONE', #25678, #25149, #29475, .T. ) ;
#5876 = CARTESIAN_POINT ( 'NONE',  ( 7.357023737882817827, -6.665817930929303969, 54.00000000000000711 ) ) ;
#5877 = VECTOR ( 'NONE', #1236, 1000.000000000000000 ) ;
#5878 = ORIENTED_EDGE ( 'NONE', *, *, #65910, .F. ) ;
#5879 = CARTESIAN_POINT ( 'NONE',  ( 105.8309041053263257, 63.65740854044500452, 10.00000000000000000 ) ) ;
#5880 = DIRECTION ( 'NONE',  ( 0.000000000000000000, -0.9921567416492215186, 0.1249999999999996531 ) ) ;
#5881 = CARTESIAN_POINT ( 'NONE',  ( -2.993516549646742853, -7.428221114745035436, 195.0000000000000284 ) ) ;
#5882 = DIRECTION ( 'NONE',  ( 1.836970198721029934E-16, -1.836970198721036344E-16, 1.000000000000000000 ) ) ;
#5883 = ORIENTED_EDGE ( 'NONE', *, *, #26537, .T. ) ;
#5884 = DIRECTION ( 'NONE',  ( 1.836970198721029934E-16, -1.836970198721036344E-16, 1.000000000000000000 ) ) ;
#5885 = CARTESIAN_POINT ( 'NONE',  ( 275.5000000000000000, -42.50000000000000000, 30.09999999999999787 ) ) ;
#5886 = AXIS2_PLACEMENT_3D ( 'NONE', #10922, #39842, #17939 ) ;
#5887 = LINE ( 'NONE', #44381, #66147 ) ;
#5888 = DIRECTION ( 'NONE',  ( 1.000000000000000000, -0.000000000000000000, 0.000000000000000000 ) ) ;
#5889 = CARTESIAN_POINT ( 'NONE',  ( 0.000000000000000000, 8.250000000000001776, -10.00000000000000000 ) ) ;
#5890 = CARTESIAN_POINT ( 'NONE',  ( 0.000000000000000000, -7.449999999999998401, -9.500000000000001776 ) ) ;
#5891 = AXIS2_PLACEMENT_3D ( 'NONE', #49436, #44110, #60361 ) ;
#5892 = ORIENTED_EDGE ( 'NONE', *, *, #4809, .F. ) ;
#5893 = ORIENTED_EDGE ( 'NONE', *, *, #27950, .T. ) ;
#5894 = CARTESIAN_POINT ( 'NONE',  ( -10.30047626211725742, 3.650476262117184234, 54.00000000000000711 ) ) ;
#5895 = LINE ( 'NONE', #27810, #57111 ) ;
#5896 = EDGE_LOOP ( 'NONE', ( #63825, #8103, #12593, #21492 ) ) ;
#5897 = VECTOR ( 'NONE', #25666, 1000.000000000000000 ) ;
#5898 = LINE ( 'NONE', #12222, #49904 ) ;
#5899 = ORIENTED_EDGE ( 'NONE', *, *, #27887, .T. ) ;
#5900 = VECTOR ( 'NONE', #6238, 1000.000000000000114 ) ;
#5901 = EDGE_CURVE ( 'NONE', #38222, #11065, #49992, .T. ) ;
#5902 = DIRECTION ( 'NONE',  ( 0.000000000000000000, -1.000000000000000000, 0.000000000000000000 ) ) ;
#5903 = ORIENTED_EDGE ( 'NONE', *, *, #36705, .F. ) ;
#5904 = EDGE_LOOP ( 'NONE', ( #32785, #59046 ) ) ;
#5905 = DIRECTION ( 'NONE',  ( -1.836970198721029934E-16, 1.836970198721036344E-16, -1.000000000000000000 ) ) ;
#5906 = ORIENTED_EDGE ( 'NONE', *, *, #10480, .T. ) ;
#5907 = VECTOR ( 'NONE', #48431, 1000.000000000000000 ) ;
#5908 = DIRECTION ( 'NONE',  ( -0.6414496315691645689, -0.7671651518152939886, -2.587583378555115478E-16 ) ) ;
#5909 = CYLINDRICAL_SURFACE ( 'NONE', #25997, 0.1749999999999993783 ) ;
#5910 = CARTESIAN_POINT ( 'NONE',  ( -7.450000000000001954, 7.250000000000000000, -16.00000000000000000 ) ) ;
#5911 = VECTOR ( 'NONE', #41265, 1000.000000000000000 ) ;
#5912 = EDGE_LOOP ( 'NONE', ( #35029, #8622, #42111, #22088 ) ) ;
#5913 = ORIENTED_EDGE ( 'NONE', *, *, #24591, .F. ) ;
#5914 = CARTESIAN_POINT ( 'NONE',  ( 26.90000000000000213, -0.2000000000089119934, -8.913009219568841313E-12 ) ) ;
#5915 = VECTOR ( 'NONE', #6304, 1000.000000000000000 ) ;
#5916 = CARTESIAN_POINT ( 'NONE',  ( -15.50000000000000000, -0.1999999999999999556, -23.94999999999999929 ) ) ;
#5917 = EDGE_CURVE ( 'NONE', #66963, #41832, #66947, .T. ) ;
#5918 = ORIENTED_EDGE ( 'NONE', *, *, #68534, .T. ) ;
#5919 = ORIENTED_EDGE ( 'NONE', *, *, #60476, .F. ) ;
#5920 = ORIENTED_EDGE ( 'NONE', *, *, #36838, .T. ) ;
#5921 = EDGE_CURVE ( 'NONE', #69139, #7820, #1553, .T. ) ;
#5922 = DIRECTION ( 'NONE',  ( -0.7671651518152895477, 0.6414496315691698980, -2.309356642088442522E-17 ) ) ;
#5924 = ORIENTED_EDGE ( 'NONE', *, *, #28054, .T. ) ;
#5923 = PLANE ( 'NONE',  #48946 ) ;
#5925 = DIRECTION ( 'NONE',  ( 0.000000000000000000, 0.000000000000000000, 1.000000000000000000 ) ) ;
#5926 = CARTESIAN_POINT ( 'NONE',  ( 40.90000000000000568, -21.00000000000000355, 14.57806571531352269 ) ) ;
#5927 = ORIENTED_EDGE ( 'NONE', *, *, #694, .F. ) ;
#5928 = ORIENTED_EDGE ( 'NONE', *, *, #48994, .F. ) ;
#5929 = AXIS2_PLACEMENT_3D ( 'NONE', #942, #59627, #32745 ) ;
#5930 = EDGE_CURVE ( 'NONE', #60486, #67015, #45378, .T. ) ;
#5931 = VERTEX_POINT ( 'NONE', #1912 ) ;
#5932 = DIRECTION ( 'NONE',  ( 1.000000000000000000, 0.000000000000000000, 0.000000000000000000 ) ) ;
#5933 = DIRECTION ( 'NONE',  ( -1.000000000000000000, 0.000000000000000000, 0.000000000000000000 ) ) ;
#5934 = VECTOR ( 'NONE', #52569, 1000.000000000000000 ) ;
#5935 = ORIENTED_EDGE ( 'NONE', *, *, #64147, .T. ) ;
#5936 = CARTESIAN_POINT ( 'NONE',  ( 9.737023737882806174, 7.955476262117184838, 54.00000000000000711 ) ) ;
#5937 = EDGE_CURVE ( 'NONE', #60780, #36470, #7557, .T. ) ;
#5939 = ORIENTED_EDGE ( 'NONE', *, *, #29986, .F. ) ;
#5938 = PLANE ( 'NONE',  #15057 ) ;
#5940 = EDGE_LOOP ( 'NONE', ( #37900, #27612, #12846, #8353 ) ) ;
#5941 = AXIS2_PLACEMENT_3D ( 'NONE', #41387, #31144, #62965 ) ;
#5942 = CARTESIAN_POINT ( 'NONE',  ( 7.357023737882800951, 6.651770455163678264, 26.00000000000000711 ) ) ;
#5943 = CYLINDRICAL_SURFACE ( 'NONE', #35227, 0.1999999999999987899 ) ;
#5944 = EDGE_CURVE ( 'NONE', #56315, #51110, #26066, .T. ) ;
#5945 = DIRECTION ( 'NONE',  ( 0.000000000000000000, -1.000000000000000000, 0.000000000000000000 ) ) ;
#5946 = DIRECTION ( 'NONE',  ( 0.000000000000000000, 0.000000000000000000, 1.000000000000000000 ) ) ;
#5947 = LINE ( 'NONE', #647, #29667 ) ;
#5948 = ADVANCED_FACE ( 'NONE', ( #8599 ), #23477, .T. ) ;
#5949 = VERTEX_POINT ( 'NONE', #29127 ) ;
#5950 = CARTESIAN_POINT ( 'NONE',  ( -0.9414762621173295987, -9.929523737882849588, 54.00000000000000711 ) ) ;
#5951 = CARTESIAN_POINT ( 'NONE',  ( 69.47321854994619628, 47.95351654967443977, 43.00000000000000000 ) ) ;
#5953 = ADVANCED_FACE ( 'NONE', ( #45031 ), #3436, .T. ) ;
#5952 = FACE_OUTER_BOUND ( 'NONE', #41701, .T. ) ;
#5955 = ORIENTED_EDGE ( 'NONE', *, *, #49483, .T. ) ;
#5954 = CARTESIAN_POINT ( 'NONE',  ( 275.0000000000000000, -20.50000000000000000, 17.00000000000000000 ) ) ;
#5956 = CARTESIAN_POINT ( 'NONE',  ( -3.593516549646790903, -7.428221114745077180, 455.0000000000000568 ) ) ;
#5957 = AXIS2_PLACEMENT_3D ( 'NONE', #39023, #55633, #2584 ) ;
#5958 = CARTESIAN_POINT ( 'NONE',  ( 7.250000000000005329, 7.250000000000000888, -26.00000000000001066 ) ) ;
#5959 = DIRECTION ( 'NONE',  ( 0.000000000000000000, 1.000000000000000000, 0.000000000000000000 ) ) ;
#5960 = VECTOR ( 'NONE', #18918, 1000.000000000000000 ) ;
#5961 = DIRECTION ( 'NONE',  ( 1.000000000000000000, -0.000000000000000000, -0.000000000000000000 ) ) ;
#5962 = AXIS2_PLACEMENT_3D ( 'NONE', #40742, #68678, #24834 ) ;
#5963 = VERTEX_POINT ( 'NONE', #23823 ) ;
#5964 = DIRECTION ( 'NONE',  ( -1.000000000000000000, 0.000000000000000000, 0.000000000000000000 ) ) ;
#5965 = FACE_OUTER_BOUND ( 'NONE', #47364, .T. ) ;
#5966 = ORIENTED_EDGE ( 'NONE', *, *, #41780, .T. ) ;
#5967 = CARTESIAN_POINT ( 'NONE',  ( 8.606483450353382025, 4.383466043307719495, 455.0000000000000568 ) ) ;
#5968 = DIRECTION ( 'NONE',  ( 0.000000000000000000, 0.000000000000000000, -1.000000000000000000 ) ) ;
#5969 = CARTESIAN_POINT ( 'NONE',  ( 12.90000000000000213, -14.06939075806900874, 20.80000000000001137 ) ) ;
#5971 = AXIS2_PLACEMENT_3D ( 'NONE', #67155, #61138, #13054 ) ;
#5970 = CYLINDRICAL_SURFACE ( 'NONE', #33063, 1.224999999999998757 ) ;
#5972 = CARTESIAN_POINT ( 'NONE',  ( 1.634292677759874302, 8.227189898828697778, 54.00000000000000711 ) ) ;
#5973 = CARTESIAN_POINT ( 'NONE',  ( 4.961189459950040792, 7.342976262117206332, 26.00000000000000711 ) ) ;
#5974 = AXIS2_PLACEMENT_3D ( 'NONE', #52371, #10621, #37852 ) ;
#5975 = ORIENTED_EDGE ( 'NONE', *, *, #24545, .T. ) ;
#5976 = DIRECTION ( 'NONE',  ( -0.6414496315691565753, 0.7671651518153006499, 0.000000000000000000 ) ) ;
#5977 = DIRECTION ( 'NONE',  ( -1.836970198721029934E-16, 1.836970198721036344E-16, -1.000000000000000000 ) ) ;
#5978 = EDGE_CURVE ( 'NONE', #69370, #62681, #34774, .T. ) ;
#5979 = ORIENTED_EDGE ( 'NONE', *, *, #36646, .T. ) ;
#5980 = DIRECTION ( 'NONE',  ( 0.000000000000000000, -1.000000000000000000, 0.000000000000000000 ) ) ;
#5981 = VECTOR ( 'NONE', #28064, 1000.000000000000000 ) ;
#5982 = EDGE_CURVE ( 'NONE', #60836, #38359, #30527, .T. ) ;
#5983 = DIRECTION ( 'NONE',  ( -0.3479852726768748461, 0.000000000000000000, 0.9375000000000006661 ) ) ;
#5984 = DIRECTION ( 'NONE',  ( 0.000000000000000000, 1.000000000000000000, 0.000000000000000000 ) ) ;
#5985 = ORIENTED_EDGE ( 'NONE', *, *, #10398, .F. ) ;
#5986 = ORIENTED_EDGE ( 'NONE', *, *, #7426, .T. ) ;
#5987 = CIRCLE ( 'NONE', #66939, 1.000000000000000000 ) ;
#5988 = DIRECTION ( 'NONE',  ( 0.000000000000000000, -0.000000000000000000, 1.000000000000000000 ) ) ;
#5989 = ORIENTED_EDGE ( 'NONE', *, *, #33220, .T. ) ;
#5990 = ADVANCED_FACE ( 'NONE', ( #58099 ), #36898, .T. ) ;
#5991 = ORIENTED_EDGE ( 'NONE', *, *, #14167, .F. ) ;
#5992 = FACE_OUTER_BOUND ( 'NONE', #43451, .T. ) ;
#5993 = CARTESIAN_POINT ( 'NONE',  ( -7.250000000000000000, -7.449999999999998401, -22.00000000000000000 ) ) ;
#5994 = CARTESIAN_POINT ( 'NONE',  ( 7.000000000000000000, -25.60000000000000142, -17.60000000000000142 ) ) ;
#5995 = ORIENTED_EDGE ( 'NONE', *, *, #30212, .T. ) ;
#5996 = EDGE_CURVE ( 'NONE', #35542, #68516, #28274, .T. ) ;
#5997 = CYLINDRICAL_SURFACE ( 'NONE', #67335, 3.999999999999993339 ) ;
#5999 = DIRECTION ( 'NONE',  ( -0.000000000000000000, -0.000000000000000000, 1.000000000000000000 ) ) ;
#5998 = LINE ( 'NONE', #54786, #37778 ) ;
#6000 = ORIENTED_EDGE ( 'NONE', *, *, #3296, .T. ) ;
#6001 = ORIENTED_EDGE ( 'NONE', *, *, #58403, .T. ) ;
#6002 = ADVANCED_FACE ( 'NONE', ( #30880 ), #46345, .T. ) ;
#6004 = VERTEX_POINT ( 'NONE', #47831 ) ;
#6003 = DIRECTION ( 'NONE',  ( -1.000000000000000000, -0.000000000000000000, -0.000000000000000000 ) ) ;
#6005 = ORIENTED_EDGE ( 'NONE', *, *, #24357, .T. ) ;
#6006 = EDGE_CURVE ( 'NONE', #14714, #69741, #20609, .T. ) ;
#6007 = CYLINDRICAL_SURFACE ( 'NONE', #27659, 3.499999999999055866 ) ;
#6008 = CARTESIAN_POINT ( 'NONE',  ( 12.00648345035333620, 4.173516549646563156, 195.0000000000000284 ) ) ;
#6009 = VECTOR ( 'NONE', #55896, 1000.000000000000000 ) ;
#6010 = ORIENTED_EDGE ( 'NONE', *, *, #36765, .T. ) ;
#6011 = EDGE_CURVE ( 'NONE', #67875, #37049, #57746, .T. ) ;
#6012 = ORIENTED_EDGE ( 'NONE', *, *, #31714, .T. ) ;
#6013 = EDGE_CURVE ( 'NONE', #32779, #47223, #52822, .T. ) ;
#6014 = AXIS2_PLACEMENT_3D ( 'NONE', #31636, #25270, #31295 ) ;
#6016 = DIRECTION ( 'NONE',  ( 0.000000000000000000, -1.000000000000000000, 0.000000000000000000 ) ) ;
#6015 = AXIS2_PLACEMENT_3D ( 'NONE', #32065, #10837, #20750 ) ;
#6017 = CARTESIAN_POINT ( 'NONE',  ( -9.689726262117227762, 10.03972626211718300, 54.00000000000000711 ) ) ;
#6018 = ADVANCED_FACE ( 'NONE', ( #20263 ), #9313, .F. ) ;
#6019 = EDGE_CURVE ( 'NONE', #6255, #63002, #2285, .T. ) ;
#6020 = ADVANCED_FACE ( 'NONE', ( #52098 ), #37243, .F. ) ;
#6021 = ORIENTED_EDGE ( 'NONE', *, *, #26181, .F. ) ;
#6022 = CARTESIAN_POINT ( 'NONE',  ( 283.0000000000000568, -26.50000000000000000, 9.080000000000000071 ) ) ;
#6023 = DIRECTION ( 'NONE',  ( 0.000000000000000000, 1.000000000000000000, -0.000000000000000000 ) ) ;
#6024 =( GEOMETRIC_REPRESENTATION_CONTEXT ( 3 ) GLOBAL_UNCERTAINTY_ASSIGNED_CONTEXT ( ( #42967 ) ) GLOBAL_UNIT_ASSIGNED_CONTEXT ( ( #31784, #53352, #64303 ) ) REPRESENTATION_CONTEXT ( 'NONE', 'WORKASPACE' ) );
#6025 = DIRECTION ( 'NONE',  ( 0.000000000000000000, 1.000000000000000000, 0.000000000000000000 ) ) ;
#6026 = ORIENTED_EDGE ( 'NONE', *, *, #2560, .T. ) ;
#6027 = ADVANCED_FACE ( 'NONE', ( #47488 ), #46435, .T. ) ;
#6028 = CARTESIAN_POINT ( 'NONE',  ( 28.90000000000000213, -0.2000000000089119934, 8.909539772616881237E-12 ) ) ;
#6029 = EDGE_CURVE ( 'NONE', #7366, #25592, #48633, .T. ) ;
#6030 = CARTESIAN_POINT ( 'NONE',  ( -11.00000000000000000, -5.599999999999999645, 27.00000000000000000 ) ) ;
#6032 = ORIENTED_EDGE ( 'NONE', *, *, #31995, .T. ) ;
#6031 = DIRECTION ( 'NONE',  ( 0.000000000000000000, 0.000000000000000000, -1.000000000000000000 ) ) ;
#6034 = ORIENTED_EDGE ( 'NONE', *, *, #9950, .F. ) ;
#6033 = DIRECTION ( 'NONE',  ( 0.000000000000000000, -0.1500000000000000777, 0.9886859966642594921 ) ) ;
#6035 = DIRECTION ( 'NONE',  ( -1.000000000000000000, 0.000000000000000000, 0.000000000000000000 ) ) ;
#6036 = CARTESIAN_POINT ( 'NONE',  ( -10.73351654964671198, 1.077516549646603483, 455.0000000000000568 ) ) ;
#6037 = AXIS2_PLACEMENT_3D ( 'NONE', #8916, #25551, #36139 ) ;
#6038 = FACE_OUTER_BOUND ( 'NONE', #50518, .T. ) ;
#6039 = DIRECTION ( 'NONE',  ( 0.000000000000000000, 0.000000000000000000, 1.000000000000000000 ) ) ;
#6040 = DIRECTION ( 'NONE',  ( -0.000000000000000000, -0.000000000000000000, -1.000000000000000000 ) ) ;
#6041 = LINE ( 'NONE', #65094, #27023 ) ;
#6042 = VECTOR ( 'NONE', #312, 1000.000000000000000 ) ;
#6043 = EDGE_CURVE ( 'NONE', #15881, #52921, #63763, .T. ) ;
#6044 = VERTEX_POINT ( 'NONE', #31592 ) ;
#6045 = DIRECTION ( 'NONE',  ( 1.000000000000000000, 0.000000000000000000, 0.000000000000000000 ) ) ;
#6048 = ORIENTED_EDGE ( 'NONE', *, *, #46875, .F. ) ;
#6047 = EDGE_CURVE ( 'NONE', #4682, #7560, #51750, .T. ) ;
#6046 = CARTESIAN_POINT ( 'NONE',  ( 41.09999999999999432, 13.66939075806899950, -20.80000000000000426 ) ) ;
#6050 = VERTEX_POINT ( 'NONE', #63055 ) ;
#6049 = CARTESIAN_POINT ( 'NONE',  ( 41.09999999999999432, -14.06939075806900163, 20.80000000000000426 ) ) ;
#6051 = LINE ( 'NONE', #48143, #22247 ) ;
#6052 = CIRCLE ( 'NONE', #38738, 2.500000000000000000 ) ;
#6053 = CARTESIAN_POINT ( 'NONE',  ( 14.24999999999999822, -0.2715193793361447838, -22.98718409945083252 ) ) ;
#6054 = VERTEX_POINT ( 'NONE', #26274 ) ;
#6055 = DIRECTION ( 'NONE',  ( -0.000000000000000000, 0.000000000000000000, 1.000000000000000000 ) ) ;
#6056 = DIRECTION ( 'NONE',  ( 1.000000000000000000, -0.000000000000000000, 0.000000000000000000 ) ) ;
#6057 = ADVANCED_FACE ( 'NONE', ( #35827 ), #57395, .F. ) ;
#6058 = ORIENTED_EDGE ( 'NONE', *, *, #6722, .T. ) ;
#6059 = CARTESIAN_POINT ( 'NONE',  ( 8.250000000000005329, 8.250000000000001776, -26.00000000000001066 ) ) ;
#6060 = DIRECTION ( 'NONE',  ( 0.000000000000000000, 0.000000000000000000, 1.000000000000000000 ) ) ;
#6061 = PRESENTATION_STYLE_ASSIGNMENT (( #59455 ) ) ;
#6062 = CARTESIAN_POINT ( 'NONE',  ( -4.193516549646782998, -11.12648345035339581, 195.0000000000000284 ) ) ;
#6063 = VECTOR ( 'NONE', #43521, 1000.000000000000000 ) ;
#6064 = ORIENTED_EDGE ( 'NONE', *, *, #47521, .F. ) ;
#6065 = DIRECTION ( 'NONE',  ( -1.000000000000000000, 0.000000000000000000, 0.000000000000000000 ) ) ;
#6066 = ORIENTED_EDGE ( 'NONE', *, *, #61649, .F. ) ;
#6067 = ORIENTED_EDGE ( 'NONE', *, *, #5872, .F. ) ;
#6068 = AXIS2_PLACEMENT_3D ( 'NONE', #44473, #6994, #676 ) ;
#6069 = LINE ( 'NONE', #11025, #24571 ) ;
#6070 = CARTESIAN_POINT ( 'NONE',  ( 6.665817930929283541, 7.342976262117200115, 26.00000000000000711 ) ) ;
#6071 = AXIS2_PLACEMENT_3D ( 'NONE', #29659, #30374, #13752 ) ;
#6072 = DIRECTION ( 'NONE',  ( -1.000000000000000000, 0.000000000000000000, 0.000000000000000000 ) ) ;
#6073 = AXIS2_PLACEMENT_3D ( 'NONE', #33295, #54871, #27993 ) ;
#6074 = CARTESIAN_POINT ( 'NONE',  ( 3.857023737882779635, -10.31452373788281029, 54.00000000000000711 ) ) ;
#6075 = ORIENTED_EDGE ( 'NONE', *, *, #51501, .F. ) ;
#6076 = ORIENTED_EDGE ( 'NONE', *, *, #29983, .T. ) ;
#6078 = VERTEX_POINT ( 'NONE', #14610 ) ;
#6077 = CARTESIAN_POINT ( 'NONE',  ( -8.593516549646711411, 7.603567055985436696, 455.0000000000000568 ) ) ;
#6079 = ORIENTED_EDGE ( 'NONE', *, *, #21253, .F. ) ;
#6080 = ADVANCED_FACE ( 'NONE', ( #36173 ), #45205, .F. ) ;
#6081 = DIRECTION ( 'NONE',  ( -0.000000000000000000, 1.000000000000000000, -0.000000000000000000 ) ) ;
#6082 = CARTESIAN_POINT ( 'NONE',  ( -31.00000000000000000, -2.500000000000000000, 45.00000000000000000 ) ) ;
#6083 = LINE ( 'NONE', #15998, #8258 ) ;
#6084 = ADVANCED_FACE ( 'NONE', ( #22014 ), #21322, .F. ) ;
#6086 = CARTESIAN_POINT ( 'NONE',  ( 10.20488345035345645, 11.47551654964653167, 455.0000000000000568 ) ) ;
#6085 = CARTESIAN_POINT ( 'NONE',  ( -3.667976262117227382, 9.897976262117168744, 54.00000000000000711 ) ) ;
#6087 = EDGE_LOOP ( 'NONE', ( #23796, #25144, #41401, #47122 ) ) ;
#6088 = ADVANCED_FACE ( 'NONE', ( #34241 ), #52014, .F. ) ;
#6090 = VERTEX_POINT ( 'NONE', #69770 ) ;
#6089 = LINE ( 'NONE', #49230, #66845 ) ;
#6091 = VERTEX_POINT ( 'NONE', #54547 ) ;
#6092 = ORIENTED_EDGE ( 'NONE', *, *, #58593, .T. ) ;
#6093 = DIRECTION ( 'NONE',  ( 0.000000000000000000, 0.000000000000000000, 1.000000000000000000 ) ) ;
#6094 = EDGE_CURVE ( 'NONE', #42963, #12117, #43230, .T. ) ;
#6095 = FACE_OUTER_BOUND ( 'NONE', #46324, .T. ) ;
#6096 = CARTESIAN_POINT ( 'NONE',  ( 7.250000000000005329, -7.449999999999998401, -25.50000000000000355 ) ) ;
#6097 = VERTEX_POINT ( 'NONE', #7031 ) ;
#6098 = ORIENTED_EDGE ( 'NONE', *, *, #16137, .T. ) ;
#6099 = VECTOR ( 'NONE', #14318, 1000.000000000000000 ) ;
#6100 = DIRECTION ( 'NONE',  ( 0.000000000000000000, 0.000000000000000000, 1.000000000000000000 ) ) ;
#6101 = DIRECTION ( 'NONE',  ( 9.912705577010336396E-15, 1.000000000000000000, 0.000000000000000000 ) ) ;
#6102 = ORIENTED_EDGE ( 'NONE', *, *, #49679, .F. ) ;
#6103 = EDGE_CURVE ( 'NONE', #12421, #68065, #56484, .T. ) ;
#6104 = VERTEX_POINT ( 'NONE', #26627 ) ;
#6105 = CARTESIAN_POINT ( 'NONE',  ( -6.350872789121327244, 6.822336235477381550, 54.00000000000000711 ) ) ;
#6106 = CARTESIAN_POINT ( 'NONE',  ( -16.54633693294649888, -0.2717122460102565085, -23.33927276307431598 ) ) ;
#6107 = VERTEX_POINT ( 'NONE', #27327 ) ;
#6108 = AXIS2_PLACEMENT_3D ( 'NONE', #21530, #38821, #22574 ) ;
#6109 = AXIS2_PLACEMENT_3D ( 'NONE', #68437, #5832, #54974 ) ;
#6110 = LINE ( 'NONE', #49584, #23456 ) ;
#6112 = ORIENTED_EDGE ( 'NONE', *, *, #8257, .T. ) ;
#6111 = CARTESIAN_POINT ( 'NONE',  ( 19.90000000000000213, 13.66939075806899240, 20.79999999999999361 ) ) ;
#6113 = ORIENTED_EDGE ( 'NONE', *, *, #12728, .F. ) ;
#6114 = LINE ( 'NONE', #55244, #52514 ) ;
#6115 = CARTESIAN_POINT ( 'NONE',  ( 55.00000000000000000, -16.96999999999999886, -21.00000000000000000 ) ) ;
#6116 = VECTOR ( 'NONE', #28740, 1000.000000000000000 ) ;
#6117 = CIRCLE ( 'NONE', #4963, 0.5249999999999994671 ) ;
#6118 = CARTESIAN_POINT ( 'NONE',  ( -11.00000000000000000, -17.50000000000000000, 15.70500000000000007 ) ) ;
#6119 = DIRECTION ( 'NONE',  ( 0.000000000000000000, 1.000000000000000000, 0.000000000000000000 ) ) ;
#6120 = DIRECTION ( 'NONE',  ( 1.000000000000000000, 0.000000000000000000, 0.000000000000000000 ) ) ;
#6121 = AXIS2_PLACEMENT_3D ( 'NONE', #53748, #4957, #49478 ) ;
#6122 = EDGE_CURVE ( 'NONE', #61720, #66978, #38440, .T. ) ;
#6123 = ORIENTED_EDGE ( 'NONE', *, *, #37747, .F. ) ;
#6124 = CARTESIAN_POINT ( 'NONE',  ( 2.544523737882818271, 9.722976262117205337, 54.00000000000000711 ) ) ;
#6127 = ORIENTED_EDGE ( 'NONE', *, *, #26781, .T. ) ;
#6126 = EDGE_CURVE ( 'NONE', #9548, #21103, #41810, .T. ) ;
#6125 = DIRECTION ( 'NONE',  ( -1.000000000000000000, 1.356437060717834182E-15, 0.000000000000000000 ) ) ;
#6128 = CARTESIAN_POINT ( 'NONE',  ( 11.00000000000000000, -11.85423089348099879, 9.852125413066602277 ) ) ;
#6129 = FACE_OUTER_BOUND ( 'NONE', #5940, .T. ) ;
#6130 = EDGE_CURVE ( 'NONE', #37690, #4176, #31932, .T. ) ;
#6131 = DIRECTION ( 'NONE',  ( -0.000000000000000000, -0.000000000000000000, -1.000000000000000000 ) ) ;
#6132 = CIRCLE ( 'NONE', #18523, 0.5000000000009372503 ) ;
#6133 = DIRECTION ( 'NONE',  ( -1.000000000000000000, 1.356437060717834182E-15, 0.000000000000000000 ) ) ;
#6134 = CARTESIAN_POINT ( 'NONE',  ( 7.357023737882817827, -6.665817930929303969, 54.00000000000000711 ) ) ;
#6135 = EDGE_LOOP ( 'NONE', ( #23678, #32633, #45265, #20030 ) ) ;
#6136 = ORIENTED_EDGE ( 'NONE', *, *, #11666, .T. ) ;
#6137 = DIRECTION ( 'NONE',  ( 1.836970198721029934E-16, 1.836970198721010706E-16, -1.000000000000000000 ) ) ;
#6138 = ORIENTED_EDGE ( 'NONE', *, *, #54075, .T. ) ;
#6139 = CARTESIAN_POINT ( 'NONE',  ( -7.250000000000000888, -8.249999999999998224, -26.00000000000001066 ) ) ;
#6140 = DIRECTION ( 'NONE',  ( 1.000000000000000000, -0.000000000000000000, -0.000000000000000000 ) ) ;
#6141 = VECTOR ( 'NONE', #10407, 1000.000000000000000 ) ;
#6142 = ORIENTED_EDGE ( 'NONE', *, *, #50305, .T. ) ;
#6143 = CARTESIAN_POINT ( 'NONE',  ( 11.50000000000000000, -11.50000000000000000, 15.00000000000000000 ) ) ;
#6144 = CARTESIAN_POINT ( 'NONE',  ( 9.750000000000000000, -9.690000000000001279, -5.000000000000000000 ) ) ;
#6145 = ORIENTED_EDGE ( 'NONE', *, *, #31772, .F. ) ;
#6146 = CARTESIAN_POINT ( 'NONE',  ( -7.250000000000000888, 7.250000000000001776, -26.00000000000001066 ) ) ;
#6147 = AXIS2_PLACEMENT_3D ( 'NONE', #17947, #40565, #22916 ) ;
#6148 = CARTESIAN_POINT ( 'NONE',  ( 7.900000000000000355, 21.00000000000000000, 18.00000000000000355 ) ) ;
#6149 = CYLINDRICAL_SURFACE ( 'NONE', #58046, 0.1999999999999987899 ) ;
#6150 = CARTESIAN_POINT ( 'NONE',  ( 7.250000000000005329, -7.249999999999998224, -21.00000000000000000 ) ) ;
#6151 = ORIENTED_EDGE ( 'NONE', *, *, #22855, .F. ) ;
#6153 = ORIENTED_EDGE ( 'NONE', *, *, #24112, .F. ) ;
#6152 = CARTESIAN_POINT ( 'NONE',  ( -7.250000000000000000, -8.749999999999998224, -30.00000000000001066 ) ) ;
#6154 = EDGE_CURVE ( 'NONE', #8669, #44324, #35028, .T. ) ;
#6155 = CIRCLE ( 'NONE', #47945, 0.1749999999999998224 ) ;
#6156 = DIRECTION ( 'NONE',  ( 0.8660254037844363761, -0.5000000000000038858, -1.836970198721044232E-16 ) ) ;
#6157 = FACE_OUTER_BOUND ( 'NONE', #19128, .T. ) ;
#6158 = DIRECTION ( 'NONE',  ( -1.000000000000000000, 0.000000000000000000, 0.000000000000000000 ) ) ;
#6159 = ORIENTED_EDGE ( 'NONE', *, *, #9694, .T. ) ;
#6160 = EDGE_CURVE ( 'NONE', #13636, #39877, #53505, .T. ) ;
#6161 = PLANE ( 'NONE',  #63860 ) ;
#6162 = AXIS2_PLACEMENT_3D ( 'NONE', #63025, #9991, #14581 ) ;
#6163 = CYLINDRICAL_SURFACE ( 'NONE', #3680, 0.1749999999999998224 ) ;
#6164 = VECTOR ( 'NONE', #53196, 1000.000000000000000 ) ;
#6165 = EDGE_CURVE ( 'NONE', #52181, #59688, #38287, .T. ) ;
#6166 = ORIENTED_EDGE ( 'NONE', *, *, #34471, .T. ) ;
#6167 = ORIENTED_EDGE ( 'NONE', *, *, #56541, .F. ) ;
#6168 = ADVANCED_FACE ( 'NONE', ( #66437 ), #16719, .F. ) ;
#6169 = ORIENTED_EDGE ( 'NONE', *, *, #66081, .T. ) ;
#6170 = CARTESIAN_POINT ( 'NONE',  ( 10.09643294401454661, -2.706483450353491804, 455.0000000000000568 ) ) ;
#6171 = EDGE_CURVE ( 'NONE', #59441, #2526, #4579, .T. ) ;
#6172 = EDGE_CURVE ( 'NONE', #18944, #57384, #3453, .T. ) ;
#6173 = CARTESIAN_POINT ( 'NONE',  ( 8.250000000000005329, 8.250000000000001776, -26.00000000000001066 ) ) ;
#6174 = DIRECTION ( 'NONE',  ( -3.304235192336773145E-15, -1.000000000000000000, 0.000000000000000000 ) ) ;
#6175 =( LENGTH_UNIT ( ) NAMED_UNIT ( * ) SI_UNIT ( .MILLI., .METRE. ) );
#6176 = ADVANCED_FACE ( 'NONE', ( #48894 ), #32278, .F. ) ;
#6177 = ORIENTED_EDGE ( 'NONE', *, *, #22848, .F. ) ;
#6178 = EDGE_LOOP ( 'NONE', ( #25089, #9906, #42540, #36778 ) ) ;
#6179 = EDGE_LOOP ( 'NONE', ( #57601, #45223, #58071, #58186 ) ) ;
#6180 = AXIS2_PLACEMENT_3D ( 'NONE', #69306, #52005, #63310 ) ;
#6181 = CARTESIAN_POINT ( 'NONE',  ( 8.930623737882848800, 10.03972626211715635, 54.00000000000000711 ) ) ;
#6182 = VERTEX_POINT ( 'NONE', #39551 ) ;
#6183 = ORIENTED_EDGE ( 'NONE', *, *, #24675, .T. ) ;
#6184 = ORIENTED_EDGE ( 'NONE', *, *, #45345, .T. ) ;
#6185 = ORIENTED_EDGE ( 'NONE', *, *, #61813, .F. ) ;
#6186 = CARTESIAN_POINT ( 'NONE',  ( 13.00000000000000178, -16.64230188589299786, -14.64519951917100116 ) ) ;
#6187 = UNCERTAINTY_MEASURE_WITH_UNIT (LENGTH_MEASURE( 1.000000000000000082E-05 ), #12318, 'distance_accuracy_value', 'NONE');
#6189 = VERTEX_POINT ( 'NONE', #48539 ) ;
#6188 = DIRECTION ( 'NONE',  ( 0.000000000000000000, 0.000000000000000000, -1.000000000000000000 ) ) ;
#6190 = CARTESIAN_POINT ( 'NONE',  ( -8.566576262117260754, 8.916576262117214213, 26.00000000000000711 ) ) ;
#6191 = CARTESIAN_POINT ( 'NONE',  ( 61.08342941274106153, 61.08342941274084126, 5.000000000000000000 ) ) ;
#6192 = DIRECTION ( 'NONE',  ( -1.000000000000000000, 0.000000000000000000, -0.000000000000000000 ) ) ;
#6193 = CIRCLE ( 'NONE', #19695, 2.458500000000000796 ) ;
#6194 = ORIENTED_EDGE ( 'NONE', *, *, #38350, .F. ) ;
#6195 = AXIS2_PLACEMENT_3D ( 'NONE', #32752, #5888, #27452 ) ;
#6196 = DIRECTION ( 'NONE',  ( 1.000000000000000000, 0.000000000000000000, 0.000000000000000000 ) ) ;
#6197 = ORIENTED_EDGE ( 'NONE', *, *, #69298, .F. ) ;
#6198 = DIRECTION ( 'NONE',  ( -0.000000000000000000, 3.673940397442059868E-16, -1.000000000000000000 ) ) ;
#6199 = EDGE_CURVE ( 'NONE', #24879, #43126, #57660, .T. ) ;
#6200 = VECTOR ( 'NONE', #61145, 1000.000000000000000 ) ;
#6202 = DIRECTION ( 'NONE',  ( 0.000000000000000000, 0.000000000000000000, -1.000000000000000000 ) ) ;
#6201 = VECTOR ( 'NONE', #38203, 1000.000000000000000 ) ;
#6203 = DIRECTION ( 'NONE',  ( -3.491481338843133355E-15, -1.000000000000000000, -1.836970198721029934E-16 ) ) ;
#6204 = DIRECTION ( 'NONE',  ( -0.7671651518153006499, 0.6414496315691565753, 0.000000000000000000 ) ) ;
#6205 = ORIENTED_EDGE ( 'NONE', *, *, #25417, .T. ) ;
#6206 = EDGE_CURVE ( 'NONE', #55340, #31859, #16358, .T. ) ;
#6207 = CARTESIAN_POINT ( 'NONE',  ( -7.839518282750280065, -3.430747519065322049, 455.0000000000000568 ) ) ;
#6208 = EDGE_CURVE ( 'NONE', #4107, #37811, #44074, .T. ) ;
#6209 = AXIS2_PLACEMENT_3D ( 'NONE', #16940, #1037, #6663 ) ;
#6210 = PLANE ( 'NONE',  #20617 ) ;
#6211 = FACE_OUTER_BOUND ( 'NONE', #59346, .T. ) ;
#6212 = ADVANCED_FACE ( 'NONE', ( #61837 ), #36004, .F. ) ;
#6213 = VECTOR ( 'NONE', #69635, 1000.000000000000000 ) ;
#6214 = CARTESIAN_POINT ( 'NONE',  ( 12.00000000000000000, -5.000000000000000000, 22.50000000000000000 ) ) ;
#6215 = CARTESIAN_POINT ( 'NONE',  ( 22.14589803375000088, -15.50000000000000000, -21.50000000000000000 ) ) ;
#6216 = FACE_OUTER_BOUND ( 'NONE', #52637, .T. ) ;
#6217 = PLANE ( 'NONE',  #6219 ) ;
#6218 = CARTESIAN_POINT ( 'NONE',  ( 21.90000000000000213, -14.06939075806900874, 20.80000000000001137 ) ) ;
#6219 = AXIS2_PLACEMENT_3D ( 'NONE', #50031, #66641, #60982 ) ;
#6220 = ORIENTED_EDGE ( 'NONE', *, *, #8069, .F. ) ;
#6221 = DIRECTION ( 'NONE',  ( -0.000000000000000000, 3.673940397442059868E-16, -1.000000000000000000 ) ) ;
#6222 = CARTESIAN_POINT ( 'NONE',  ( -5.380658396643233310, 7.252248008019342329, 455.0000000000000568 ) ) ;
#6223 = PRESENTATION_LAYER_ASSIGNMENT (  '', '', ( #59271 ) ) ;
#6224 = LINE ( 'NONE', #1596, #67375 ) ;
#6225 = DIRECTION ( 'NONE',  ( -1.000000000000000000, 0.000000000000000000, 0.000000000000000000 ) ) ;
#6226 = ORIENTED_EDGE ( 'NONE', *, *, #68431, .T. ) ;
#6227 = DIRECTION ( 'NONE',  ( -1.000000000000000000, 0.000000000000000000, 0.000000000000000000 ) ) ;
#6228 = DIRECTION ( 'NONE',  ( -1.000000000000000000, 0.000000000000000000, 0.000000000000000000 ) ) ;
#6229 = DIRECTION ( 'NONE',  ( 0.000000000000000000, 1.000000000000000000, 0.000000000000000000 ) ) ;
#6230 = CARTESIAN_POINT ( 'NONE',  ( 7.250000000000005329, 7.250000000000000888, -15.50000000000000000 ) ) ;
#6231 = CARTESIAN_POINT ( 'NONE',  ( 10.20488345035345468, 10.19191654964656735, 455.0000000000000568 ) ) ;
#6232 = ORIENTED_EDGE ( 'NONE', *, *, #42919, .T. ) ;
#6233 = EDGE_CURVE ( 'NONE', #29795, #49979, #56865, .T. ) ;
#6234 = EDGE_LOOP ( 'NONE', ( #33654, #29606 ) ) ;
#6235 = CARTESIAN_POINT ( 'NONE',  ( 3.857023737882813386, 9.897976262117209600, 26.00000000000000711 ) ) ;
#6236 = CARTESIAN_POINT ( 'NONE',  ( 30.00000000000000000, -15.97213595500069871, -14.50000000000000000 ) ) ;
#6237 = ORIENTED_EDGE ( 'NONE', *, *, #44925, .F. ) ;
#6238 = DIRECTION ( 'NONE',  ( 0.000000000000000000, -0.7071067811865474617, -0.7071067811865474617 ) ) ;
#6239 = AXIS2_PLACEMENT_3D ( 'NONE', #19966, #47544, #69110 ) ;
#6240 = ORIENTED_EDGE ( 'NONE', *, *, #40635, .F. ) ;
#6241 = AXIS2_PLACEMENT_3D ( 'NONE', #48415, #69977, #28906 ) ;
#6242 = DIRECTION ( 'NONE',  ( 0.000000000000000000, 1.000000000000000000, 0.000000000000000000 ) ) ;
#6243 = ORIENTED_EDGE ( 'NONE', *, *, #196, .T. ) ;
#6244 = EDGE_LOOP ( 'NONE', ( #28760, #276, #24416, #9245 ) ) ;
#6245 = DIRECTION ( 'NONE',  ( 1.000000000000000000, -5.981805089575194965E-17, 0.000000000000000000 ) ) ;
#6246 = EDGE_CURVE ( 'NONE', #51293, #48513, #13592, .T. ) ;
#6247 = ORIENTED_EDGE ( 'NONE', *, *, #29845, .F. ) ;
#6248 = CARTESIAN_POINT ( 'NONE',  ( 30.00000000000000000, -9.200000000000120082, 17.30000000000000071 ) ) ;
#6249 = CARTESIAN_POINT ( 'NONE',  ( -7.259684009079930611, 7.798499376343971612, 455.0000000000000568 ) ) ;
#6250 = CARTESIAN_POINT ( 'NONE',  ( -11.50000000000000000, -12.00000000000000000, 10.52786404500095863 ) ) ;
#6251 = AXIS2_PLACEMENT_3D ( 'NONE', #41577, #14364, #68458 ) ;
#6252 = AXIS2_PLACEMENT_3D ( 'NONE', #16914, #652, #7317 ) ;
#6253 = VECTOR ( 'NONE', #52632, 1000.000000000000000 ) ;
#6254 = EDGE_CURVE ( 'NONE', #44953, #26897, #67130, .T. ) ;
#6255 = VERTEX_POINT ( 'NONE', #67499 ) ;
#6256 = VERTEX_POINT ( 'NONE', #35280 ) ;
#6257 = DIRECTION ( 'NONE',  ( 0.000000000000000000, 0.000000000000000000, -1.000000000000000000 ) ) ;
#6258 = DIRECTION ( 'NONE',  ( 0.000000000000000000, 0.000000000000000000, -1.000000000000000000 ) ) ;
#6259 = VECTOR ( 'NONE', #6934, 1000.000000000000000 ) ;
#6260 = AXIS2_PLACEMENT_3D ( 'NONE', #58535, #10082, #26340 ) ;
#6261 = ORIENTED_EDGE ( 'NONE', *, *, #15712, .F. ) ;
#6262 = VERTEX_POINT ( 'NONE', #34599 ) ;
#6263 = ORIENTED_EDGE ( 'NONE', *, *, #28672, .F. ) ;
#6264 = VECTOR ( 'NONE', #58673, 1000.000000000000000 ) ;
#6265 = DIRECTION ( 'NONE',  ( 1.000000000000000000, 2.135044278125301343E-15, -0.000000000000000000 ) ) ;
#6267 = ORIENTED_EDGE ( 'NONE', *, *, #45456, .F. ) ;
#6266 = LINE ( 'NONE', #10530, #30870 ) ;
#6268 = ADVANCED_FACE ( 'NONE', ( #51212 ), #14454, .F. ) ;
#6269 = DIRECTION ( 'NONE',  ( 0.000000000000000000, 0.000000000000000000, -1.000000000000000000 ) ) ;
#6270 = AXIS2_PLACEMENT_3D ( 'NONE', #67354, #8990, #9352 ) ;
#6271 = DIRECTION ( 'NONE',  ( -1.000000000000000000, 0.000000000000000000, 0.000000000000000000 ) ) ;
#6272 = EDGE_LOOP ( 'NONE', ( #23945, #27490, #55634, #20712 ) ) ;
#6273 = ORIENTED_EDGE ( 'NONE', *, *, #58140, .T. ) ;
#6274 = VECTOR ( 'NONE', #65439, 1000.000000000000000 ) ;
#6275 = ORIENTED_EDGE ( 'NONE', *, *, #4196, .F. ) ;
#6276 = CARTESIAN_POINT ( 'NONE',  ( 7.000000000000000000, -25.93000000000544958, -9.412893218815410634 ) ) ;
#6277 = CARTESIAN_POINT ( 'NONE',  ( 11.18999999999999950, 11.18999999999999950, -4.250000000000000000 ) ) ;
#6278 = ORIENTED_EDGE ( 'NONE', *, *, #23486, .T. ) ;
#6279 = PRESENTATION_STYLE_ASSIGNMENT (( #66007 ) ) ;
#6280 = DIRECTION ( 'NONE',  ( 0.000000000000000000, 0.000000000000000000, -1.000000000000000000 ) ) ;
#6281 = AXIS2_PLACEMENT_3D ( 'NONE', #37688, #16119, #52197 ) ;
#6283 = EDGE_LOOP ( 'NONE', ( #59057, #46236, #30325, #67691 ) ) ;
#6282 = FILL_AREA_STYLE ('',( #39485 ) ) ;
#6284 = VERTEX_POINT ( 'NONE', #50859 ) ;
#6285 = EDGE_CURVE ( 'NONE', #34294, #35057, #23990, .T. ) ;
#6286 = CYLINDRICAL_SURFACE ( 'NONE', #40760, 1.000000000000000000 ) ;
#6287 = DIRECTION ( 'NONE',  ( -1.000000000000000000, 0.000000000000000000, 0.000000000000000000 ) ) ;
#6288 = AXIS2_PLACEMENT_3D ( 'NONE', #23607, #67092, #50490 ) ;
#6289 = FACE_OUTER_BOUND ( 'NONE', #3897, .T. ) ;
#6290 = CARTESIAN_POINT ( 'NONE',  ( -16.54633693294650953, -0.2717122460102549542, 21.66072723692568402 ) ) ;
#6291 = EDGE_CURVE ( 'NONE', #56517, #39731, #2432, .T. ) ;
#6292 = CIRCLE ( 'NONE', #27749, 1.000000000000000000 ) ;
#6293 = FACE_BOUND ( 'NONE', #17429, .T. ) ;
#6294 = ORIENTED_EDGE ( 'NONE', *, *, #40134, .F. ) ;
#6295 = DIRECTION ( 'NONE',  ( 0.000000000000000000, -0.7071067811865455743, 0.7071067811865495711 ) ) ;
#6296 = DIRECTION ( 'NONE',  ( -0.000000000000000000, -0.000000000000000000, 1.000000000000000000 ) ) ;
#6297 = DIRECTION ( 'NONE',  ( 1.000000000000000000, -0.000000000000000000, 0.000000000000000000 ) ) ;
#6298 = DIRECTION ( 'NONE',  ( 1.000000000000000000, 0.000000000000000000, 0.000000000000000000 ) ) ;
#6299 = AXIS2_PLACEMENT_3D ( 'NONE', #11069, #32635, #16726 ) ;
#6300 = AXIS2_PLACEMENT_3D ( 'NONE', #37704, #15090, #5184 ) ;
#6301 = CIRCLE ( 'NONE', #65013, 1.000000000000000000 ) ;
#6302 = CARTESIAN_POINT ( 'NONE',  ( 0.5000000000000000000, 18.00000000000000355, -21.00000000000000000 ) ) ;
#6303 = CARTESIAN_POINT ( 'NONE',  ( -7.415254214038345282, -3.006483450353401032, 455.0000000000000568 ) ) ;
#6304 = DIRECTION ( 'NONE',  ( -0.6414496315691420314, 0.7671651518153128624, 2.587583378555127804E-16 ) ) ;
#6305 = CIRCLE ( 'NONE', #61599, 0.1749999999999998224 ) ;
#6306 = CIRCLE ( 'NONE', #45819, 0.2500000000000002220 ) ;
#6307 = VECTOR ( 'NONE', #63746, 1000.000000000000000 ) ;
#6308 = CARTESIAN_POINT ( 'NONE',  ( 283.0000000000000568, -42.50000000000000000, -7.500000000000000000 ) ) ;
#6309 = ORIENTED_EDGE ( 'NONE', *, *, #26893, .T. ) ;
#6310 = CARTESIAN_POINT ( 'NONE',  ( 24.00000000000000000, -15.50000000000000000, 19.33772233983200195 ) ) ;
#6311 = LINE ( 'NONE', #17254, #56443 ) ;
#6312 = ORIENTED_EDGE ( 'NONE', *, *, #25907, .T. ) ;
#6313 = DIRECTION ( 'NONE',  ( -1.000000000000000000, 0.000000000000000000, 0.000000000000000000 ) ) ;
#6314 = CARTESIAN_POINT ( 'NONE',  ( -5.242976262117280406, -5.257023737882805747, 54.00000000000000711 ) ) ;
#6315 = CIRCLE ( 'NONE', #66113, 1.000000000000000000 ) ;
#6316 = CARTESIAN_POINT ( 'NONE',  ( 3.682023737882818892, 9.897976262117202495, 54.00000000000000711 ) ) ;
#6317 = EDGE_CURVE ( 'NONE', #36489, #14072, #24348, .T. ) ;
#6318 = DIRECTION ( 'NONE',  ( -1.000000000000000000, 0.000000000000000000, 0.000000000000000000 ) ) ;
#6319 = PLANE ( 'NONE',  #26008 ) ;
#6320 = CARTESIAN_POINT ( 'NONE',  ( 11.08848345035341687, 9.791916549646563439, 455.0000000000000568 ) ) ;
#6321 = AXIS2_PLACEMENT_3D ( 'NONE', #18639, #61415, #29242 ) ;
#6322 = VERTEX_POINT ( 'NONE', #30359 ) ;
#6323 = CARTESIAN_POINT ( 'NONE',  ( -4.135079735113167843, 3.663616288757005623, 26.00000000000000711 ) ) ;
#6324 = CARTESIAN_POINT ( 'NONE',  ( 41.09999999999999432, -21.00000000000000000, 13.86939075806900057 ) ) ;
#6325 = ORIENTED_EDGE ( 'NONE', *, *, #36199, .T. ) ;
#6326 =( GEOMETRIC_REPRESENTATION_CONTEXT ( 3 ) GLOBAL_UNCERTAINTY_ASSIGNED_CONTEXT ( ( #4112 ) ) GLOBAL_UNIT_ASSIGNED_CONTEXT ( ( #36386, #14827, #14479 ) ) REPRESENTATION_CONTEXT ( 'NONE', 'WORKASPACE' ) );
#6327 = LINE ( 'NONE', #43106, #67528 ) ;
#6328 = CARTESIAN_POINT ( 'NONE',  ( 16.89999999999999858, 20.60000000000000142, -13.86939075806900057 ) ) ;
#6329 = CARTESIAN_POINT ( 'NONE',  ( 49.00000000000000000, -0.2000000000089119934, 8.909539772616881237E-12 ) ) ;
#6330 = ORIENTED_EDGE ( 'NONE', *, *, #39436, .F. ) ;
#6331 = VERTEX_POINT ( 'NONE', #52274 ) ;
#6332 = DIRECTION ( 'NONE',  ( 0.000000000000000000, -1.000000000000000000, 0.000000000000000000 ) ) ;
#6333 = ORIENTED_EDGE ( 'NONE', *, *, #46640, .T. ) ;
#6334 = ORIENTED_EDGE ( 'NONE', *, *, #18482, .T. ) ;
#6335 = EDGE_CURVE ( 'NONE', #33050, #61094, #3833, .T. ) ;
#6336 = DIRECTION ( 'NONE',  ( -0.000000000000000000, 0.000000000000000000, -1.000000000000000000 ) ) ;
#6337 = DIRECTION ( 'NONE',  ( -1.000000000000000000, 0.000000000000000000, 0.000000000000000000 ) ) ;
#6338 = CARTESIAN_POINT ( 'NONE',  ( 29.25000000000000000, -5.000000000000000000, 26.25000000000000000 ) ) ;
#6339 = ADVANCED_FACE ( 'NONE', ( #45553 ), #18687, .T. ) ;
#6340 = ADVANCED_FACE ( 'NONE', ( #57576 ), #19045, .F. ) ;
#6341 = VECTOR ( 'NONE', #13315, 1000.000000000000114 ) ;
#6342 = ORIENTED_EDGE ( 'NONE', *, *, #37220, .T. ) ;
#6343 = DIRECTION ( 'NONE',  ( -1.000000000000000000, 0.000000000000000000, 0.000000000000000000 ) ) ;
#6345 = LINE ( 'NONE', #22606, #69356 ) ;
#6344 = CARTESIAN_POINT ( 'NONE',  ( 7.250000000000005329, 7.250000000000000888, -26.00000000000001066 ) ) ;
#6346 = VERTEX_POINT ( 'NONE', #8421 ) ;
#6347 = ORIENTED_EDGE ( 'NONE', *, *, #68038, .T. ) ;
#6350 = VERTEX_POINT ( 'NONE', #3146 ) ;
#6349 = EDGE_CURVE ( 'NONE', #65495, #38703, #19387, .T. ) ;
#6348 = DIRECTION ( 'NONE',  ( -0.000000000000000000, -0.000000000000000000, -1.000000000000000000 ) ) ;
#6351 = EDGE_LOOP ( 'NONE', ( #42752, #64723, #59451, #44875 ) ) ;
#6352 = AXIS2_PLACEMENT_3D ( 'NONE', #58523, #41886, #19971 ) ;
#6353 = EDGE_CURVE ( 'NONE', #18984, #33218, #4629, .T. ) ;
#6354 = DIRECTION ( 'NONE',  ( 0.000000000000000000, -0.1111111111108836896, 0.9938079899999319178 ) ) ;
#6355 = EDGE_CURVE ( 'NONE', #17879, #43197, #24702, .T. ) ;
#6356 = VECTOR ( 'NONE', #131, 1000.000000000000114 ) ;
#6357 = CIRCLE ( 'NONE', #43604, 0.5000000000004236611 ) ;
#6358 = CIRCLE ( 'NONE', #51522, 1.000000000000001776 ) ;
#6359 = CARTESIAN_POINT ( 'NONE',  ( -2.752095193409509033, -9.955011587777317317, 455.0000000000000568 ) ) ;
#6360 = ORIENTED_EDGE ( 'NONE', *, *, #62996, .F. ) ;
#6361 = ORIENTED_EDGE ( 'NONE', *, *, #65721, .T. ) ;
#6362 = CIRCLE ( 'NONE', #52717, 4.000000000000001776 ) ;
#6363 = AXIS2_PLACEMENT_3D ( 'NONE', #65146, #16703, #54531 ) ;
#6364 = VECTOR ( 'NONE', #18314, 1000.000000000000114 ) ;
#6365 = LINE ( 'NONE', #4973, #58362 ) ;
#6366 = DIRECTION ( 'NONE',  ( -1.000000000000000000, 0.000000000000000000, 0.000000000000000000 ) ) ;
#6367 = EDGE_LOOP ( 'NONE', ( #56548, #6962, #7208, #31046 ) ) ;
#6368 = DIRECTION ( 'NONE',  ( 0.000000000000000000, -1.000000000000000000, 0.000000000000000000 ) ) ;
#6370 = VECTOR ( 'NONE', #27754, 1000.000000000000114 ) ;
#6369 = DIRECTION ( 'NONE',  ( 0.000000000000000000, 0.000000000000000000, -1.000000000000000000 ) ) ;
#6371 = PLANE ( 'NONE',  #16998 ) ;
#6372 = ORIENTED_EDGE ( 'NONE', *, *, #3015, .F. ) ;
#6373 = VECTOR ( 'NONE', #57527, 1000.000000000000000 ) ;
#6374 = DIRECTION ( 'NONE',  ( -0.7671651518153065341, 0.6414496315691495809, 2.356647714346224881E-16 ) ) ;
#6375 = ADVANCED_FACE ( 'NONE', ( #57227 ), #20446, .F. ) ;
#6376 = CARTESIAN_POINT ( 'NONE',  ( 6.006483450353379716, -6.006483450353490738, 455.0000000000000568 ) ) ;
#6377 = ORIENTED_EDGE ( 'NONE', *, *, #32816, .T. ) ;
#6379 = VERTEX_POINT ( 'NONE', #59320 ) ;
#6378 = CARTESIAN_POINT ( 'NONE',  ( 39.00000000000000000, -0.2000000000000000111, 0.000000000000000000 ) ) ;
#6380 = DIRECTION ( 'NONE',  ( 0.000000000000000000, 0.000000000000000000, 1.000000000000000000 ) ) ;
#6381 = DIRECTION ( 'NONE',  ( -0.000000000000000000, -0.000000000000000000, -1.000000000000000000 ) ) ;
#6382 = CARTESIAN_POINT ( 'NONE',  ( -16.75000000000000000, -0.2038245569916330158, -21.77831216351300014 ) ) ;
#6383 = CARTESIAN_POINT ( 'NONE',  ( 12.00648345035338238, 4.173516549646515195, 455.0000000000000568 ) ) ;
#6384 = DIRECTION ( 'NONE',  ( 0.000000000000000000, 0.000000000000000000, 1.000000000000000000 ) ) ;
#6385 = DIRECTION ( 'NONE',  ( 0.000000000000000000, -1.000000000000000000, 0.000000000000000000 ) ) ;
#6386 = ORIENTED_EDGE ( 'NONE', *, *, #28368, .F. ) ;
#6387 = CARTESIAN_POINT ( 'NONE',  ( 9.912023737882815766, -3.857023737882816050, 26.00000000000000711 ) ) ;
#6389 = VERTEX_POINT ( 'NONE', #41660 ) ;
#6388 = PLANE ( 'NONE',  #68362 ) ;
#6391 = ORIENTED_EDGE ( 'NONE', *, *, #23226, .T. ) ;
#6390 = LINE ( 'NONE', #65776, #38951 ) ;
#6392 = LINE ( 'NONE', #5005, #60589 ) ;
#6393 = VECTOR ( 'NONE', #23069, 1000.000000000000000 ) ;
#6394 = DIRECTION ( 'NONE',  ( 0.000000000000000000, 0.6857142857142869419, -0.7278708115918273158 ) ) ;
#6395 = CIRCLE ( 'NONE', #7484, 0.5249999999999990230 ) ;
#6396 = ORIENTED_EDGE ( 'NONE', *, *, #60764, .T. ) ;
#6397 = DIRECTION ( 'NONE',  ( 0.000000000000000000, 1.000000000000000000, 0.000000000000000000 ) ) ;
#6398 = CARTESIAN_POINT ( 'NONE',  ( 3.857023737882817827, 10.30047626211720413, 54.00000000000000711 ) ) ;
#6399 = ORIENTED_EDGE ( 'NONE', *, *, #3863, .T. ) ;
#6400 = FACE_OUTER_BOUND ( 'NONE', #8282, .T. ) ;
#6401 = CARTESIAN_POINT ( 'NONE',  ( 28.90000000000000213, -21.00000000000000000, 13.86939075806900057 ) ) ;
#6402 = VECTOR ( 'NONE', #24020, 1000.000000000000000 ) ;
#6403 = VECTOR ( 'NONE', #40361, 1000.000000000000000 ) ;
#6404 = CARTESIAN_POINT ( 'NONE',  ( 275.0000000000000000, -25.50000000000000355, -14.74860679774999994 ) ) ;
#6405 = EDGE_CURVE ( 'NONE', #41004, #59963, #21491, .T. ) ;
#6406 = DIRECTION ( 'NONE',  ( -1.000000000000000000, 0.000000000000000000, 0.000000000000000000 ) ) ;
#6408 = PLANE ( 'NONE',  #47797 ) ;
#6407 = AXIS2_PLACEMENT_3D ( 'NONE', #50865, #39897, #1393 ) ;
#6409 = ORIENTED_EDGE ( 'NONE', *, *, #44016, .T. ) ;
#6410 = AXIS2_PLACEMENT_3D ( 'NONE', #29190, #13287, #34843 ) ;
#6411 = CARTESIAN_POINT ( 'NONE',  ( 30.00000000000000000, -5.599999999999999645, 9.400000000000000355 ) ) ;
#6412 = ORIENTED_EDGE ( 'NONE', *, *, #34510, .F. ) ;
#6413 = EDGE_CURVE ( 'NONE', #8950, #47029, #26114, .T. ) ;
#6414 = EDGE_LOOP ( 'NONE', ( #65391, #65149, #56337, #15100 ) ) ;
#6415 = DIRECTION ( 'NONE',  ( 0.000000000000000000, -0.9921567416492215186, 0.1249999999999996531 ) ) ;
#6416 = CARTESIAN_POINT ( 'NONE',  ( 30.00000000000000000, -14.04000000000000092, -14.80000000000000071 ) ) ;
#6417 = CIRCLE ( 'NONE', #1914, 24.99999999998784972 ) ;
#6418 = ADVANCED_FACE ( 'NONE', ( #15507 ), #53338, .F. ) ;
#6419 = ADVANCED_FACE ( 'NONE', ( #64626 ), #14801, .T. ) ;
#6420 = VECTOR ( 'NONE', #27248, 1000.000000000000000 ) ;
#6421 = CYLINDRICAL_SURFACE ( 'NONE', #18559, 0.2999999999998732569 ) ;
#6422 = DIRECTION ( 'NONE',  ( 0.7071067811865474617, 0.7071067811865474617, 0.000000000000000000 ) ) ;
#6423 = EDGE_LOOP ( 'NONE', ( #10747, #15510, #54733, #52394 ) ) ;
#6424 = ORIENTED_EDGE ( 'NONE', *, *, #9020, .T. ) ;
#6426 = EDGE_LOOP ( 'NONE', ( #55242, #65312, #42684, #54565 ) ) ;
#6425 = LINE ( 'NONE', #1119, #47596 ) ;
#6427 = ORIENTED_EDGE ( 'NONE', *, *, #38103, .T. ) ;
#6428 = VECTOR ( 'NONE', #9601, 1000.000000000000000 ) ;
#6429 = DIRECTION ( 'NONE',  ( 0.000000000000000000, 1.000000000000000000, 0.000000000000000000 ) ) ;
#6430 = DIRECTION ( 'NONE',  ( -1.000000000000000000, 0.000000000000000000, 0.000000000000000000 ) ) ;
#6431 = EDGE_CURVE ( 'NONE', #54584, #2465, #53198, .T. ) ;
#6432 = FACE_OUTER_BOUND ( 'NONE', #36332, .T. ) ;
#6433 = LINE ( 'NONE', #59480, #36812 ) ;
#6435 = LINE ( 'NONE', #44241, #68449 ) ;
#6434 = CARTESIAN_POINT ( 'NONE',  ( 11.00000000000000000, -11.50000000000100009, -15.00000000000084910 ) ) ;
#6436 = ORIENTED_EDGE ( 'NONE', *, *, #39576, .T. ) ;
#6438 = EDGE_LOOP ( 'NONE', ( #51740, #42016, #26144, #4938 ) ) ;
#6437 = LINE ( 'NONE', #1131, #43189 ) ;
#6439 = ORIENTED_EDGE ( 'NONE', *, *, #32797, .F. ) ;
#6440 = ORIENTED_EDGE ( 'NONE', *, *, #28472, .T. ) ;
#6441 = CARTESIAN_POINT ( 'NONE',  ( -3.834182069070765309, 7.342976262117170805, 54.00000000000000711 ) ) ;
#6442 = EDGE_CURVE ( 'NONE', #60266, #6963, #4887, .T. ) ;
#6443 = LINE ( 'NONE', #50605, #30983 ) ;
#6444 = EDGE_CURVE ( 'NONE', #35366, #2217, #47316, .T. ) ;
#6445 = DIRECTION ( 'NONE',  ( -1.794541526872559352E-16, -1.000000000000000000, 0.000000000000000000 ) ) ;
#6446 = CARTESIAN_POINT ( 'NONE',  ( 7.000000000000000000, -25.60000000000000142, 17.60000000000000142 ) ) ;
#6447 = VERTEX_POINT ( 'NONE', #32103 ) ;
#6448 = MECHANICAL_DESIGN_GEOMETRIC_PRESENTATION_REPRESENTATION (  '', ( #51559 ), #45951 ) ;
#6449 = ORIENTED_EDGE ( 'NONE', *, *, #56689, .F. ) ;
#6450 = CARTESIAN_POINT ( 'NONE',  ( -7.250000000000001776, -7.249999999999998224, -14.00000000000000000 ) ) ;
#6451 = CARTESIAN_POINT ( 'NONE',  ( 6.006483450353401921, 5.993516549646582092, 455.0000000000000568 ) ) ;
#6452 = EDGE_CURVE ( 'NONE', #30313, #45034, #68892, .T. ) ;
#6453 = ORIENTED_EDGE ( 'NONE', *, *, #69575, .F. ) ;
#6454 = ORIENTED_EDGE ( 'NONE', *, *, #53190, .F. ) ;
#6455 = CIRCLE ( 'NONE', #45962, 0.3500000000002719824 ) ;
#6457 = DIRECTION ( 'NONE',  ( 1.000000000000000000, -1.356437060717834379E-15, -1.836970198721032646E-16 ) ) ;
#6456 = VECTOR ( 'NONE', #62530, 1000.000000000000000 ) ;
#6458 = CARTESIAN_POINT ( 'NONE',  ( 48.66598694767480993, -0.7500000000000044409, -3.588632928360947272 ) ) ;
#6459 = ORIENTED_EDGE ( 'NONE', *, *, #39229, .T. ) ;
#6460 = CIRCLE ( 'NONE', #39199, 4.000000000000000888 ) ;
#6461 = CIRCLE ( 'NONE', #57273, 0.7499999999999997780 ) ;
#6462 =( GEOMETRIC_REPRESENTATION_CONTEXT ( 3 ) GLOBAL_UNCERTAINTY_ASSIGNED_CONTEXT ( ( #11137 ) ) GLOBAL_UNIT_ASSIGNED_CONTEXT ( ( #48189, #41121, #14605 ) ) REPRESENTATION_CONTEXT ( 'NONE', 'WORKASPACE' ) );
#6463 = CARTESIAN_POINT ( 'NONE',  ( 29.25000000000000000, -5.200000000000001066, -11.75000000000000000 ) ) ;
#6465 = EDGE_LOOP ( 'NONE', ( #5333, #41674, #8885, #7385 ) ) ;
#6464 = LINE ( 'NONE', #48552, #69033 ) ;
#6466 = ORIENTED_EDGE ( 'NONE', *, *, #34229, .F. ) ;
#6467 = LINE ( 'NONE', #49927, #12953 ) ;
#6468 = VECTOR ( 'NONE', #4823, 1000.000000000000000 ) ;
#6469 = LINE ( 'NONE', #48218, #69606 ) ;
#6470 = VECTOR ( 'NONE', #6337, 1000.000000000000000 ) ;
#6471 = FACE_OUTER_BOUND ( 'NONE', #27537, .T. ) ;
#6472 = LINE ( 'NONE', #22723, #34602 ) ;
#6473 = EDGE_CURVE ( 'NONE', #27668, #63779, #28324, .T. ) ;
#6474 = DIRECTION ( 'NONE',  ( 1.000000000000000000, -0.000000000000000000, 0.000000000000000000 ) ) ;
#6475 = ORIENTED_EDGE ( 'NONE', *, *, #35780, .T. ) ;
#6476 = LINE ( 'NONE', #28370, #15706 ) ;
#6477 = EDGE_CURVE ( 'NONE', #29553, #67310, #21154, .T. ) ;
#6479 = ORIENTED_EDGE ( 'NONE', *, *, #57259, .T. ) ;
#6478 = LINE ( 'NONE', #22727, #44606 ) ;
#6480 = AXIS2_PLACEMENT_3D ( 'NONE', #24375, #29313, #45575 ) ;
#6481 = CARTESIAN_POINT ( 'NONE',  ( -15.50000000000000000, -1.037157890325000054, 18.50000000000000000 ) ) ;
#6482 = LINE ( 'NONE', #5454, #4128 ) ;
#6484 = EDGE_CURVE ( 'NONE', #48934, #20922, #63318, .T. ) ;
#6483 = DIRECTION ( 'NONE',  ( 1.000000000000000000, 0.000000000000000000, 0.000000000000000000 ) ) ;
#6485 = DIRECTION ( 'NONE',  ( 0.000000000000000000, 0.000000000000000000, -1.000000000000000000 ) ) ;
#6486 = CARTESIAN_POINT ( 'NONE',  ( 10.31452373788280674, 6.835476262117182067, 54.00000000000000711 ) ) ;
#6487 = EDGE_CURVE ( 'NONE', #22188, #63555, #58973, .T. ) ;
#6488 = VERTEX_POINT ( 'NONE', #57924 ) ;
#6489 = ORIENTED_EDGE ( 'NONE', *, *, #1650, .F. ) ;
#6490 = FACE_OUTER_BOUND ( 'NONE', #5808, .T. ) ;
#6491 = EDGE_CURVE ( 'NONE', #10855, #16950, #54036, .T. ) ;
#6492 = CARTESIAN_POINT ( 'NONE',  ( 46.39999999999999858, 33.00000000000000000, -1.250000000000000000 ) ) ;
#6493 = ORIENTED_EDGE ( 'NONE', *, *, #17658, .F. ) ;
#6494 = CARTESIAN_POINT ( 'NONE',  ( 154.0064834503532722, -29.01119750012554732, 5.000000000000000000 ) ) ;
#6495 = DIRECTION ( 'NONE',  ( 0.000000000000000000, 0.000000000000000000, -1.000000000000000000 ) ) ;
#6496 =( GEOMETRIC_REPRESENTATION_CONTEXT ( 3 ) GLOBAL_UNCERTAINTY_ASSIGNED_CONTEXT ( ( #15414 ) ) GLOBAL_UNIT_ASSIGNED_CONTEXT ( ( #53713, #59701, #38150 ) ) REPRESENTATION_CONTEXT ( 'NONE', 'WORKASPACE' ) );
#6497 = EDGE_CURVE ( 'NONE', #2624, #17564, #43055, .T. ) ;
#6498 = ORIENTED_EDGE ( 'NONE', *, *, #3296, .F. ) ;
#6499 = EDGE_CURVE ( 'NONE', #11348, #54703, #48715, .T. ) ;
#6500 = DIRECTION ( 'NONE',  ( 0.000000000000000000, 0.000000000000000000, 1.000000000000000000 ) ) ;
#6501 = LINE ( 'NONE', #26675, #66932 ) ;
#6502 = VERTEX_POINT ( 'NONE', #52636 ) ;
#6503 = CARTESIAN_POINT ( 'NONE',  ( -25.50000000000000355, -15.50000000000000000, -22.50000000000000000 ) ) ;
#6504 = CARTESIAN_POINT ( 'NONE',  ( 30.00000000000000000, -17.50000000000000000, 15.70500000000000007 ) ) ;
#6505 = ADVANCED_FACE ( 'NONE', ( #25772 ), #63592, .F. ) ;
#6506 = EDGE_CURVE ( 'NONE', #50486, #14586, #5793, .T. ) ;
#6507 = VECTOR ( 'NONE', #59618, 1000.000000000000000 ) ;
#6508 = AXIS2_PLACEMENT_3D ( 'NONE', #24638, #56793, #19318 ) ;
#6509 = CYLINDRICAL_SURFACE ( 'NONE', #49018, 0.1749999999999989342 ) ;
#6510 = CYLINDRICAL_SURFACE ( 'NONE', #40775, 0.3999999999999993006 ) ;
#6511 = ORIENTED_EDGE ( 'NONE', *, *, #60640, .T. ) ;
#6513 = VERTEX_POINT ( 'NONE', #11900 ) ;
#6512 = DIRECTION ( 'NONE',  ( 0.000000000000000000, 1.000000000000000000, 0.000000000000000000 ) ) ;
#6514 = EDGE_CURVE ( 'NONE', #38926, #12, #43397, .T. ) ;
#6515 = CIRCLE ( 'NONE', #5420, 0.4000000000000600298 ) ;
#6516 = AXIS2_PLACEMENT_3D ( 'NONE', #32289, #22382, #17063 ) ;
#6517 = DIRECTION ( 'NONE',  ( 1.000000000000000000, -3.491481338843133355E-15, -1.836970198721036344E-16 ) ) ;
#6518 = DIRECTION ( 'NONE',  ( 0.000000000000000000, -1.000000000000000000, 0.000000000000000000 ) ) ;
#6519 = DIRECTION ( 'NONE',  ( -1.671920889371702854E-15, 1.000000000000000000, 3.673940397442059868E-16 ) ) ;
#6520 = ORIENTED_EDGE ( 'NONE', *, *, #27290, .F. ) ;
#6521 = AXIS2_PLACEMENT_3D ( 'NONE', #2898, #29763, #51336 ) ;
#6523 = FACE_OUTER_BOUND ( 'NONE', #51360, .T. ) ;
#6522 = AXIS2_PLACEMENT_3D ( 'NONE', #43379, #21820, #32776 ) ;
#6524 = LINE ( 'NONE', #22086, #31905 ) ;
#6525 = VERTEX_POINT ( 'NONE', #626 ) ;
#6526 = ORIENTED_EDGE ( 'NONE', *, *, #42402, .T. ) ;
#6527 = VERTEX_POINT ( 'NONE', #22193 ) ;
#6528 = DIRECTION ( 'NONE',  ( -1.000000000000000000, 0.000000000000000000, 0.000000000000000000 ) ) ;
#6529 = EDGE_CURVE ( 'NONE', #39629, #51302, #14761, .T. ) ;
#6530 = CARTESIAN_POINT ( 'NONE',  ( 6.344579767990853547, 8.393516549646580671, 455.0000000000000568 ) ) ;
#6531 = FACE_OUTER_BOUND ( 'NONE', #35145, .T. ) ;
#6532 = ADVANCED_FACE ( 'NONE', ( #49419 ), #49059, .F. ) ;
#6533 = CIRCLE ( 'NONE', #46035, 0.3499999999998879008 ) ;
#6534 = VERTEX_POINT ( 'NONE', #38786 ) ;
#6535 = ORIENTED_EDGE ( 'NONE', *, *, #61737, .T. ) ;
#6536 = ORIENTED_EDGE ( 'NONE', *, *, #15119, .F. ) ;
#6537 = FACE_OUTER_BOUND ( 'NONE', #56877, .T. ) ;
#6538 = VERTEX_POINT ( 'NONE', #60004 ) ;
#6539 = ORIENTED_EDGE ( 'NONE', *, *, #57894, .F. ) ;
#6540 = ORIENTED_EDGE ( 'NONE', *, *, #29145, .F. ) ;
#6541 = ORIENTED_EDGE ( 'NONE', *, *, #59084, .T. ) ;
#6542 = CARTESIAN_POINT ( 'NONE',  ( 289.7499999999998863, -42.24999999999996447, 26.75000000000004619 ) ) ;
#6544 = ORIENTED_EDGE ( 'NONE', *, *, #19900, .T. ) ;
#6543 = PLANE ( 'NONE',  #37913 ) ;
#6545 = LINE ( 'NONE', #200, #6370 ) ;
#6546 = LINE ( 'NONE', #39394, #53244 ) ;
#6547 = CARTESIAN_POINT ( 'NONE',  ( 49.00000000000000000, -0.1999999999911430404, -8.864436962241481021E-12 ) ) ;
#6548 = AXIS2_PLACEMENT_3D ( 'NONE', #54586, #17427, #66223 ) ;
#6549 = VERTEX_POINT ( 'NONE', #17216 ) ;
#6550 = PLANE ( 'NONE',  #5754 ) ;
#6551 = FACE_OUTER_BOUND ( 'NONE', #54617, .T. ) ;
#6552 = DIRECTION ( 'NONE',  ( 1.000000000000000000, 0.000000000000000000, 0.000000000000000000 ) ) ;
#6553 = ORIENTED_EDGE ( 'NONE', *, *, #42173, .T. ) ;
#6554 = CARTESIAN_POINT ( 'NONE',  ( 83.77321854994620765, 47.95351654967443977, 25.00000000000000000 ) ) ;
#6555 = VECTOR ( 'NONE', #16238, 1000.000000000000000 ) ;
#6556 = EDGE_CURVE ( 'NONE', #23985, #6050, #46394, .T. ) ;
#6557 = DIRECTION ( 'NONE',  ( 0.000000000000000000, -1.000000000000000000, 0.000000000000000000 ) ) ;
#6558 = CARTESIAN_POINT ( 'NONE',  ( 28.00000000000000000, -15.50000000000000000, 20.05051025721700242 ) ) ;
#6559 = EDGE_LOOP ( 'NONE', ( #4717, #8847, #22737, #28260 ) ) ;
#6561 = EDGE_CURVE ( 'NONE', #34396, #2518, #24951, .T. ) ;
#6560 = CARTESIAN_POINT ( 'NONE',  ( -7.250000000000001776, -7.249999999999998224, -21.00000000000000000 ) ) ;
#6562 = VECTOR ( 'NONE', #12669, 1000.000000000000000 ) ;
#6563 = VECTOR ( 'NONE', #63837, 1000.000000000000000 ) ;
#6564 = CARTESIAN_POINT ( 'NONE',  ( 7.428221114744993692, 2.993516549646566105, 455.0000000000000568 ) ) ;
#6565 = DIRECTION ( 'NONE',  ( -1.000000000000000000, 0.000000000000000000, 0.000000000000000000 ) ) ;
#6566 = EDGE_CURVE ( 'NONE', #57899, #2479, #66723, .T. ) ;
#6567 = EDGE_CURVE ( 'NONE', #61001, #1782, #22539, .T. ) ;
#6568 =( REPRESENTATION_RELATIONSHIP ('NONE','NONE', #33057, #64253 ) REPRESENTATION_RELATIONSHIP_WITH_TRANSFORMATION ( #58625 )SHAPE_REPRESENTATION_RELATIONSHIP( ) );
#6569 = CARTESIAN_POINT ( 'NONE',  ( -8.250000000000001776, -8.249999999999998224, -26.00000000000001066 ) ) ;
#6570 = EDGE_CURVE ( 'NONE', #48126, #13530, #43756, .T. ) ;
#6571 = CARTESIAN_POINT ( 'NONE',  ( 15.50000000000000000, -0.2000000000000000111, -25.80000000297970075 ) ) ;
#6572 = EDGE_CURVE ( 'NONE', #3924, #64205, #65995, .T. ) ;
#6573 = PLANE ( 'NONE',  #60989 ) ;
#6574 = DIRECTION ( 'NONE',  ( -1.000000000000000000, -2.135044278125301343E-15, 0.000000000000000000 ) ) ;
#6575 = DIRECTION ( 'NONE',  ( 0.000000000000000000, 0.000000000000000000, 1.000000000000000000 ) ) ;
#6576 = VECTOR ( 'NONE', #35148, 1000.000000000000000 ) ;
#6577 = EDGE_LOOP ( 'NONE', ( #56751, #53889, #60130, #9657, #28682, #22718, #64286, #31868, #53854, #3333, #31565, #59999 ) ) ;
#6578 = CARTESIAN_POINT ( 'NONE',  ( 11.00000000000000000, -9.200000000000120082, 17.64999999999993108 ) ) ;
#6579 = CARTESIAN_POINT ( 'NONE',  ( 17.00000000000000000, -15.50000000000000000, 19.33772233983200195 ) ) ;
#6580 = DIRECTION ( 'NONE',  ( -1.000000000000000000, 0.000000000000000000, 0.000000000000000000 ) ) ;
#6581 = CARTESIAN_POINT ( 'NONE',  ( -5.993516549646728642, -6.006483450353378828, 195.0000000000000284 ) ) ;
#6582 = VERTEX_POINT ( 'NONE', #17563 ) ;
#6583 = FACE_OUTER_BOUND ( 'NONE', #15741, .T. ) ;
#6584 = LINE ( 'NONE', #22830, #45182 ) ;
#6585 = CARTESIAN_POINT ( 'NONE',  ( 41.09999999999999432, 13.66939075806899950, -20.80000000000000426 ) ) ;
#6586 = DIRECTION ( 'NONE',  ( -1.000000000000000000, 0.000000000000000000, 0.000000000000000000 ) ) ;
#6587 = DIRECTION ( 'NONE',  ( -0.8660254037844358210, 0.5000000000000049960, 2.509347957447882735E-16 ) ) ;
#6588 = ORIENTED_EDGE ( 'NONE', *, *, #69097, .T. ) ;
#6589 = CARTESIAN_POINT ( 'NONE',  ( 39.90000000000000568, 13.66939075806899240, -20.79999999999999361 ) ) ;
#6590 = CARTESIAN_POINT ( 'NONE',  ( 7.250000000000005329, -8.249999999999998224, -21.50000000000000000 ) ) ;
#6591 = ORIENTED_EDGE ( 'NONE', *, *, #51541, .F. ) ;
#6592 = PLANE ( 'NONE',  #51010 ) ;
#6593 = ORIENTED_EDGE ( 'NONE', *, *, #56527, .T. ) ;
#6594 = DIRECTION ( 'NONE',  ( 0.000000000000000000, 0.000000000000000000, -1.000000000000000000 ) ) ;
#6595 = ORIENTED_EDGE ( 'NONE', *, *, #54510, .T. ) ;
#6596 = ORIENTED_EDGE ( 'NONE', *, *, #51394, .T. ) ;
#6597 = DIRECTION ( 'NONE',  ( 1.000000000000000000, 0.000000000000000000, 0.000000000000000000 ) ) ;
#6598 = EDGE_LOOP ( 'NONE', ( #22313, #5031, #8604, #40979 ) ) ;
#6599 = DIRECTION ( 'NONE',  ( -1.000000000000000000, 0.000000000000000000, 0.000000000000000000 ) ) ;
#6600 = AXIS2_PLACEMENT_3D ( 'NONE', #41273, #62852, #4856 ) ;
#6601 = DIRECTION ( 'NONE',  ( 1.000000000000000000, -0.000000000000000000, 0.000000000000000000 ) ) ;
#6603 = EDGE_CURVE ( 'NONE', #52415, #32145, #64492, .T. ) ;
#6602 = CARTESIAN_POINT ( 'NONE',  ( -4.393516549646835578, -11.78648345035344214, 455.0000000000000568 ) ) ;
#6604 = ORIENTED_EDGE ( 'NONE', *, *, #57462, .T. ) ;
#6606 = EDGE_CURVE ( 'NONE', #47718, #38359, #33968, .T. ) ;
#6605 = EDGE_LOOP ( 'NONE', ( #39383, #25112, #13655, #32409 ) ) ;
#6607 = DIRECTION ( 'NONE',  ( -0.000000000000000000, 3.673940397442059868E-16, -1.000000000000000000 ) ) ;
#6608 = LINE ( 'NONE', #1301, #68343 ) ;
#6609 = VERTEX_POINT ( 'NONE', #65335 ) ;
#6610 = EDGE_LOOP ( 'NONE', ( #65830, #30027, #58651, #15113 ) ) ;
#6611 = ORIENTED_EDGE ( 'NONE', *, *, #62221, .T. ) ;
#6612 = DIRECTION ( 'NONE',  ( 1.000000000000000000, 0.000000000000000000, 0.000000000000000000 ) ) ;
#6614 = ORIENTED_EDGE ( 'NONE', *, *, #54108, .T. ) ;
#6613 = DIRECTION ( 'NONE',  ( 0.000000000000000000, 0.000000000000000000, 1.000000000000000000 ) ) ;
#6615 = AXIS2_PLACEMENT_3D ( 'NONE', #37450, #36753, #19509 ) ;
#6616 = DIRECTION ( 'NONE',  ( -1.000000000000000000, 0.000000000000000000, 0.000000000000000000 ) ) ;
#6617 = CARTESIAN_POINT ( 'NONE',  ( -7.813516549646711162, 11.99351654964660341, 195.0000000000000284 ) ) ;
#6618 = ORIENTED_EDGE ( 'NONE', *, *, #43178, .T. ) ;
#6619 = VERTEX_POINT ( 'NONE', #50440 ) ;
#6620 = CARTESIAN_POINT ( 'NONE',  ( 39.90000000000000568, -21.00000000000000000, 16.96999999999999886 ) ) ;
#6621 = CARTESIAN_POINT ( 'NONE',  ( 8.241237374594303944, -1.634292677759877854, 26.00000000000000711 ) ) ;
#6622 = EDGE_CURVE ( 'NONE', #44394, #68236, #55747, .T. ) ;
#6623 = CARTESIAN_POINT ( 'NONE',  ( 14.24999999999999822, -0.3152037684892576297, 22.74589050208021845 ) ) ;
#6624 = DIRECTION ( 'NONE',  ( 0.000000000000000000, 0.000000000000000000, -1.000000000000000000 ) ) ;
#6626 = ORIENTED_EDGE ( 'NONE', *, *, #60490, .T. ) ;
#6625 = CARTESIAN_POINT ( 'NONE',  ( -9.897976262117246904, -3.857023737882716574, 26.00000000000000000 ) ) ;
#6627 = EDGE_LOOP ( 'NONE', ( #67079, #14290, #12799, #17636 ) ) ;
#6628 = DIRECTION ( 'NONE',  ( 1.000000000000000000, -1.047444401652940007E-14, 1.836970198721010706E-16 ) ) ;
#6629 = DIRECTION ( 'NONE',  ( -0.8660254037844363761, 0.5000000000000038858, 0.000000000000000000 ) ) ;
#6630 = CARTESIAN_POINT ( 'NONE',  ( 11.00000000000000000, -11.50000000000000000, 11.00000000000000000 ) ) ;
#6631 = CARTESIAN_POINT ( 'NONE',  ( -3.834182069070765309, 7.342976262117170805, 54.00000000000000711 ) ) ;
#6632 = AXIS2_PLACEMENT_3D ( 'NONE', #15042, #4094, #53241 ) ;
#6633 = DIRECTION ( 'NONE',  ( 0.000000000000000000, 0.000000000000000000, 1.000000000000000000 ) ) ;
#6635 = ORIENTED_EDGE ( 'NONE', *, *, #29698, .T. ) ;
#6634 = ADVANCED_FACE ( 'NONE', ( #38123 ), #1641, .F. ) ;
#6636 = DIRECTION ( 'NONE',  ( 0.000000000000000000, 1.000000000000000000, 0.000000000000000000 ) ) ;
#6637 = EDGE_CURVE ( 'NONE', #67306, #5737, #11223, .T. ) ;
#6638 = DIRECTION ( 'NONE',  ( 0.7071067811865401342, -0.7071067811865550112, -1.365336182113289717E-30 ) ) ;
#6639 = CIRCLE ( 'NONE', #43943, 0.1999999999999996503 ) ;
#6640 = DIRECTION ( 'NONE',  ( 0.000000000000000000, 0.7071067811865474617, -0.7071067811865474617 ) ) ;
#6641 = EDGE_CURVE ( 'NONE', #60888, #5423, #17910, .T. ) ;
#6642 = DIRECTION ( 'NONE',  ( -0.000000000000000000, 1.000000000000000000, -0.000000000000000000 ) ) ;
#6643 = DIRECTION ( 'NONE',  ( 0.000000000000000000, 1.000000000000000000, 0.000000000000000000 ) ) ;
#6644 = AXIS2_PLACEMENT_3D ( 'NONE', #47517, #4738, #43251 ) ;
#6645 = DIRECTION ( 'NONE',  ( -0.000000000000000000, -0.000000000000000000, 1.000000000000000000 ) ) ;
#6646 = ORIENTED_EDGE ( 'NONE', *, *, #58802, .F. ) ;
#6647 = CARTESIAN_POINT ( 'NONE',  ( 6.832023737882818359, -9.912023737882810437, 26.00000000000000000 ) ) ;
#6648 = DIRECTION ( 'NONE',  ( 0.000000000000000000, 0.000000000000000000, -1.000000000000000000 ) ) ;
#6649 = VERTEX_POINT ( 'NONE', #54373 ) ;
#6650 = FACE_OUTER_BOUND ( 'NONE', #57124, .T. ) ;
#6651 = CARTESIAN_POINT ( 'NONE',  ( 6.849523737882818430, 10.30047626211719169, 54.00000000000000711 ) ) ;
#6652 = AXIS2_PLACEMENT_3D ( 'NONE', #55877, #55536, #7080 ) ;
#6653 = DIRECTION ( 'NONE',  ( 1.000000000000000000, -0.000000000000000000, 0.000000000000000000 ) ) ;
#6654 = DIRECTION ( 'NONE',  ( 0.000000000000000000, -1.000000000000000000, 0.000000000000000000 ) ) ;
#6655 = DIRECTION ( 'NONE',  ( 1.000000000000000000, 0.000000000000000000, 0.000000000000000000 ) ) ;
#6656 = VECTOR ( 'NONE', #67075, 1000.000000000000000 ) ;
#6657 = LINE ( 'NONE', #7335, #36390 ) ;
#6658 = ORIENTED_EDGE ( 'NONE', *, *, #46528, .T. ) ;
#6659 = DIRECTION ( 'NONE',  ( -0.000000000000000000, -0.000000000000000000, -1.000000000000000000 ) ) ;
#6660 = VERTEX_POINT ( 'NONE', #5926 ) ;
#6661 = CARTESIAN_POINT ( 'NONE',  ( 283.0000000000000568, -32.44999999999905071, 14.49999999999906031 ) ) ;
#6662 = CIRCLE ( 'NONE', #46181, 0.4000000000000010214 ) ;
#6663 = DIRECTION ( 'NONE',  ( 0.000000000000000000, 0.000000000000000000, -1.000000000000000000 ) ) ;
#6664 = DIRECTION ( 'NONE',  ( 0.000000000000000000, 0.000000000000000000, 1.000000000000000000 ) ) ;
#6665 = ORIENTED_EDGE ( 'NONE', *, *, #60331, .F. ) ;
#6666 = VERTEX_POINT ( 'NONE', #27488 ) ;
#6667 = LINE ( 'NONE', #22933, #116 ) ;
#6668 = ORIENTED_EDGE ( 'NONE', *, *, #20241, .T. ) ;
#6669 = ORIENTED_EDGE ( 'NONE', *, *, #27336, .F. ) ;
#6670 = PLANE ( 'NONE',  #21393 ) ;
#6671 = CARTESIAN_POINT ( 'NONE',  ( 11.18999999999999950, 11.18999999999999950, 0.000000000000000000 ) ) ;
#6672 = CYLINDRICAL_SURFACE ( 'NONE', #41136, 2.458500000000000796 ) ;
#6673 = ORIENTED_EDGE ( 'NONE', *, *, #26344, .T. ) ;
#6674 = ADVANCED_FACE ( 'NONE', ( #33135 ), #40871, .T. ) ;
#6675 = EDGE_CURVE ( 'NONE', #9656, #1005, #9053, .T. ) ;
#6676 = PLANE ( 'NONE',  #4105 ) ;
#6677 = EDGE_CURVE ( 'NONE', #66827, #49333, #2003, .T. ) ;
#6679 = CARTESIAN_POINT ( 'NONE',  ( -9.390476262117259054, 1.466476262117183627, 26.00000000000000711 ) ) ;
#6678 = LINE ( 'NONE', #61444, #42307 ) ;
#6680 = VERTEX_POINT ( 'NONE', #2689 ) ;
#6682 = EDGE_LOOP ( 'NONE', ( #26285, #52428, #66221, #34161 ) ) ;
#6681 = CARTESIAN_POINT ( 'NONE',  ( -7.450000000000001954, 7.250000000000000000, -21.00000000000000000 ) ) ;
#6683 = EDGE_LOOP ( 'NONE', ( #56005, #49913, #69060, #41127 ) ) ;
#6684 = EDGE_CURVE ( 'NONE', #35206, #53942, #24265, .T. ) ;
#6685 = VECTOR ( 'NONE', #32591, 1000.000000000000000 ) ;
#6686 = DIRECTION ( 'NONE',  ( 0.000000000000000000, 0.000000000000000000, 1.000000000000000000 ) ) ;
#6687 = DIRECTION ( 'NONE',  ( 1.000000000000000000, 0.000000000000000000, 0.000000000000000000 ) ) ;
#6688 = AXIS2_PLACEMENT_3D ( 'NONE', #29023, #3205, #24770 ) ;
#6689 = LINE ( 'NONE', #50171, #51733 ) ;
#6690 = EDGE_LOOP ( 'NONE', ( #35826, #66377, #14501, #26171 ) ) ;
#6691 = EDGE_LOOP ( 'NONE', ( #63135, #45173, #49523, #4829 ) ) ;
#6692 = VECTOR ( 'NONE', #38231, 1000.000000000000114 ) ;
#6693 = CYLINDRICAL_SURFACE ( 'NONE', #68545, 0.1749999999999998224 ) ;
#6694 = CARTESIAN_POINT ( 'NONE',  ( 29.50000000000000355, -15.97213595500069871, -14.50000000000000000 ) ) ;
#6695 = VERTEX_POINT ( 'NONE', #18250 ) ;
#6696 = VECTOR ( 'NONE', #51854, 1000.000000000000000 ) ;
#6697 = DIRECTION ( 'NONE',  ( 0.000000000000000000, 0.000000000000000000, 1.000000000000000000 ) ) ;
#6698 = DIRECTION ( 'NONE',  ( 1.836970198721029934E-16, -1.836970198721036344E-16, 1.000000000000000000 ) ) ;
#6699 = DIRECTION ( 'NONE',  ( 0.000000000000000000, 1.000000000000000000, 0.000000000000000000 ) ) ;
#6700 = ORIENTED_EDGE ( 'NONE', *, *, #44058, .F. ) ;
#6701 = FACE_OUTER_BOUND ( 'NONE', #443, .T. ) ;
#6702 = DIRECTION ( 'NONE',  ( 1.000000000000000000, 0.000000000000000000, 0.000000000000000000 ) ) ;
#6704 = ORIENTED_EDGE ( 'NONE', *, *, #46232, .F. ) ;
#6703 = DIRECTION ( 'NONE',  ( -1.000000000000000000, 0.000000000000000000, 0.000000000000000000 ) ) ;
#6706 = ORIENTED_EDGE ( 'NONE', *, *, #7197, .F. ) ;
#6705 = CARTESIAN_POINT ( 'NONE',  ( 48.50000000000000000, -0.7500000000000000000, 3.418698582794335028 ) ) ;
#6707 = CARTESIAN_POINT ( 'NONE',  ( 41.09999999999999432, 20.60000000000000142, 13.86939075806900057 ) ) ;
#6708 = CIRCLE ( 'NONE', #39461, 0.1749999999999998224 ) ;
#6709 = LINE ( 'NONE', #60800, #40851 ) ;
#6710 = PLANE ( 'NONE',  #15521 ) ;
#6711 = DIRECTION ( 'NONE',  ( 0.000000000000000000, 0.000000000000000000, 1.000000000000000000 ) ) ;
#6712 = CARTESIAN_POINT ( 'NONE',  ( -13.00000000000000178, -15.50000000000000000, 20.05051025721700242 ) ) ;
#6713 = LINE ( 'NONE', #5364, #7811 ) ;
#6714 = ORIENTED_EDGE ( 'NONE', *, *, #56971, .T. ) ;
#6715 = DIRECTION ( 'NONE',  ( -1.794541526872559352E-16, -1.000000000000000000, 0.000000000000000000 ) ) ;
#6716 = EDGE_CURVE ( 'NONE', #67892, #7660, #48727, .T. ) ;
#6717 = CARTESIAN_POINT ( 'NONE',  ( 283.0000000000000568, -38.65000000000095781, -13.20000000000094253 ) ) ;
#6719 = ORIENTED_EDGE ( 'NONE', *, *, #9055, .F. ) ;
#6718 = DIRECTION ( 'NONE',  ( 0.7071067811865391350, -0.7071067811865560104, 0.000000000000000000 ) ) ;
#6720 = DIRECTION ( 'NONE',  ( 0.000000000000000000, -1.000000000000000000, 0.000000000000000000 ) ) ;
#6721 = ADVANCED_FACE ( 'NONE', ( #13652 ), #30623, .F. ) ;
#6722 = EDGE_CURVE ( 'NONE', #27877, #39887, #45831, .T. ) ;
#6723 = FACE_OUTER_BOUND ( 'NONE', #28964, .T. ) ;
#6724 = EDGE_CURVE ( 'NONE', #12315, #57464, #13302, .T. ) ;
#6725 = ORIENTED_EDGE ( 'NONE', *, *, #26979, .F. ) ;
#6726 = CARTESIAN_POINT ( 'NONE',  ( 8.250000000000005329, 7.250000000000000888, -26.00000000000001066 ) ) ;
#6727 = DIRECTION ( 'NONE',  ( -0.000000000000000000, -0.000000000000000000, 1.000000000000000000 ) ) ;
#6728 = ORIENTED_EDGE ( 'NONE', *, *, #38752, .T. ) ;
#6729 = CYLINDRICAL_SURFACE ( 'NONE', #25600, 0.2000000000000005107 ) ;
#6730 = CARTESIAN_POINT ( 'NONE',  ( 7.250000000000005329, 7.250000000000000888, -12.50000000000000000 ) ) ;
#6731 = DIRECTION ( 'NONE',  ( -1.000000000000000000, 5.120954910632640039E-15, 1.881408311965255020E-30 ) ) ;
#6732 = EDGE_CURVE ( 'NONE', #39723, #33795, #39811, .T. ) ;
#6733 = CARTESIAN_POINT ( 'NONE',  ( -8.250000000000001776, -7.249999999999998224, -26.00000000000001066 ) ) ;
#6734 = VECTOR ( 'NONE', #21116, 1000.000000000000000 ) ;
#6735 = EDGE_CURVE ( 'NONE', #55886, #29102, #2349, .T. ) ;
#6736 = VECTOR ( 'NONE', #12230, 1000.000000000000000 ) ;
#6737 = DIRECTION ( 'NONE',  ( -1.836970198721029934E-16, 1.836970198721036344E-16, -1.000000000000000000 ) ) ;
#6738 = ORIENTED_EDGE ( 'NONE', *, *, #56242, .T. ) ;
#6739 = DIRECTION ( 'NONE',  ( 0.000000000000000000, 0.7840980155806945850, 0.6206370130458033207 ) ) ;
#6740 = ORIENTED_EDGE ( 'NONE', *, *, #1405, .F. ) ;
#6741 = VERTEX_POINT ( 'NONE', #30280 ) ;
#6742 = CIRCLE ( 'NONE', #33793, 2.204799999999996540 ) ;
#6743 = LINE ( 'NONE', #28312, #20077 ) ;
#6744 = PLANE ( 'NONE',  #10134 ) ;
#6745 = AXIS2_PLACEMENT_3D ( 'NONE', #63802, #57785, #41529 ) ;
#6746 = DIRECTION ( 'NONE',  ( 1.000000000000000000, -0.000000000000000000, -0.000000000000000000 ) ) ;
#6747 = DIRECTION ( 'NONE',  ( 1.000000000000000000, -0.000000000000000000, 0.000000000000000000 ) ) ;
#6748 = ORIENTED_EDGE ( 'NONE', *, *, #62548, .F. ) ;
#6749 = ORIENTED_EDGE ( 'NONE', *, *, #13085, .T. ) ;
#6751 = ORIENTED_EDGE ( 'NONE', *, *, #19308, .T. ) ;
#6750 = DIRECTION ( 'NONE',  ( 0.7071067811865361374, -0.7071067811865588970, 0.000000000000000000 ) ) ;
#6752 = EDGE_LOOP ( 'NONE', ( #63552, #30088, #30966, #66334 ) ) ;
#6753 = VECTOR ( 'NONE', #2558, 1000.000000000000000 ) ;
#6754 = DIRECTION ( 'NONE',  ( -1.836970198721029934E-16, 1.836970198721036590E-16, -1.000000000000000000 ) ) ;
#6755 = CARTESIAN_POINT ( 'NONE',  ( -7.259684009079930611, 4.188533722949235205, 455.0000000000000568 ) ) ;
#6756 = CARTESIAN_POINT ( 'NONE',  ( -8.250000000000001776, -8.249999999999998224, -26.00000000000001066 ) ) ;
#6757 = FACE_OUTER_BOUND ( 'NONE', #44291, .T. ) ;
#6758 = VECTOR ( 'NONE', #18895, 1000.000000000000000 ) ;
#6760 = CYLINDRICAL_SURFACE ( 'NONE', #8625, 5.000000000000000000 ) ;
#6759 = FACE_OUTER_BOUND ( 'NONE', #60773, .T. ) ;
#6761 = ORIENTED_EDGE ( 'NONE', *, *, #17626, .F. ) ;
#6763 = ORIENTED_EDGE ( 'NONE', *, *, #21267, .T. ) ;
#6762 = DIRECTION ( 'NONE',  ( -1.000000000000000000, 0.000000000000000000, 0.000000000000000000 ) ) ;
#6764 = ORIENTED_EDGE ( 'NONE', *, *, #6778, .F. ) ;
#6765 = VERTEX_POINT ( 'NONE', #51491 ) ;
#6766 = DIRECTION ( 'NONE',  ( 0.7071067811865451302, -0.7071067811865500152, -2.597868168706485527E-16 ) ) ;
#6767 = CARTESIAN_POINT ( 'NONE',  ( -8.250000000000001776, -7.249999999999998224, -26.00000000000001066 ) ) ;
#6768 = AXIS2_PLACEMENT_3D ( 'NONE', #37844, #23908, #34506 ) ;
#6769 = LINE ( 'NONE', #44253, #65841 ) ;
#6770 = ORIENTED_EDGE ( 'NONE', *, *, #28912, .F. ) ;
#6771 = ORIENTED_EDGE ( 'NONE', *, *, #26779, .F. ) ;
#6772 = EDGE_CURVE ( 'NONE', #43371, #8459, #10323, .T. ) ;
#6773 = DIRECTION ( 'NONE',  ( 1.000000000000000000, -0.000000000000000000, 0.000000000000000000 ) ) ;
#6774 = CARTESIAN_POINT ( 'NONE',  ( 15.91242688423647600, -0.3152598339557935447, -21.29473909966096556 ) ) ;
#6775 = VERTEX_POINT ( 'NONE', #40169 ) ;
#6776 = EDGE_LOOP ( 'NONE', ( #40063, #55180, #40792, #33571 ) ) ;
#6777 = CARTESIAN_POINT ( 'NONE',  ( 9.737023737882816832, -3.682023737882826886, 54.00000000000000711 ) ) ;
#6778 = EDGE_CURVE ( 'NONE', #54080, #29125, #29486, .T. ) ;
#6779 = CARTESIAN_POINT ( 'NONE',  ( 48.50000000000000000, -0.7500000000000000000, -3.418698582794335028 ) ) ;
#6780 = AXIS2_PLACEMENT_3D ( 'NONE', #41550, #31655, #25651 ) ;
#6781 = ORIENTED_EDGE ( 'NONE', *, *, #12990, .F. ) ;
#6782 = CIRCLE ( 'NONE', #65553, 0.1999999999999996503 ) ;
#6783 = FACE_OUTER_BOUND ( 'NONE', #36535, .T. ) ;
#6785 = EDGE_LOOP ( 'NONE', ( #40661, #26020, #58476, #17000 ) ) ;
#6784 = DIRECTION ( 'NONE',  ( 1.000000000000000000, 0.000000000000000000, 0.000000000000000000 ) ) ;
#6786 = ORIENTED_EDGE ( 'NONE', *, *, #67366, .T. ) ;
#6787 = CIRCLE ( 'NONE', #13560, 0.5000000000000000000 ) ;
#6788 = LINE ( 'NONE', #22387, #36716 ) ;
#6789 = CYLINDRICAL_SURFACE ( 'NONE', #68488, 0.1999999999999987899 ) ;
#6790 = FACE_OUTER_BOUND ( 'NONE', #20477, .T. ) ;
#6791 = CARTESIAN_POINT ( 'NONE',  ( 46.39999999999999858, 33.00000000000000000, 2.250000000000000444 ) ) ;
#6792 = ADVANCED_FACE ( 'NONE', ( #35929 ), #18965, .F. ) ;
#6793 = DIRECTION ( 'NONE',  ( 1.836970198721029934E-16, 1.836970198721010706E-16, -1.000000000000000000 ) ) ;
#6794 = AXIS2_PLACEMENT_3D ( 'NONE', #2733, #25014, #45874 ) ;
#6795 = DIRECTION ( 'NONE',  ( -1.000000000000000000, 1.794541526872559352E-16, 0.000000000000000000 ) ) ;
#6796 = ORIENTED_EDGE ( 'NONE', *, *, #20653, .F. ) ;
#6797 = CARTESIAN_POINT ( 'NONE',  ( 8.250000000000005329, -7.249999999999998224, -26.00000000000001066 ) ) ;
#6798 = CIRCLE ( 'NONE', #40516, 4.000000000000000000 ) ;
#6800 = ORIENTED_EDGE ( 'NONE', *, *, #195, .T. ) ;
#6799 = DIRECTION ( 'NONE',  ( 1.000000000000000000, -0.000000000000000000, 0.000000000000000000 ) ) ;
#6801 = DIRECTION ( 'NONE',  ( 1.000000000000000000, 0.000000000000000000, 0.000000000000000000 ) ) ;
#6802 = DIRECTION ( 'NONE',  ( 0.000000000000000000, 0.000000000000000000, 1.000000000000000000 ) ) ;
#6803 = EDGE_CURVE ( 'NONE', #27638, #35258, #50931, .T. ) ;
#6804 = CARTESIAN_POINT ( 'NONE',  ( 283.0000000000000568, -31.30000000000045191, 8.400000000000000355 ) ) ;
#6805 = DIRECTION ( 'NONE',  ( 1.000000000000000000, 0.000000000000000000, 0.000000000000000000 ) ) ;
#6806 = VECTOR ( 'NONE', #6040, 1000.000000000000000 ) ;
#6807 = CIRCLE ( 'NONE', #35017, 1.000000000000000000 ) ;
#6808 = CARTESIAN_POINT ( 'NONE',  ( 41.09999999999999432, 20.60000000000000142, -13.86939075806900057 ) ) ;
#6809 = ORIENTED_EDGE ( 'NONE', *, *, #52798, .T. ) ;
#6810 = EDGE_LOOP ( 'NONE', ( #29839, #1979, #65178, #37240 ) ) ;
#6811 = DIRECTION ( 'NONE',  ( 0.000000000000000000, -0.7096009616570518874, 0.7046037717862339012 ) ) ;
#6812 = ADVANCED_FACE ( 'NONE', ( #41220 ), #46524, .F. ) ;
#6813 = DIRECTION ( 'NONE',  ( -0.7071067811865451302, 0.7071067811865500152, 2.597868168706484541E-16 ) ) ;
#6814 = EDGE_CURVE ( 'NONE', #60569, #64371, #8337, .T. ) ;
#6815 = ORIENTED_EDGE ( 'NONE', *, *, #64387, .T. ) ;
#6816 = CARTESIAN_POINT ( 'NONE',  ( 10.92648345035337520, -2.906483450353395614, 195.0000000000000284 ) ) ;
#6817 = ORIENTED_EDGE ( 'NONE', *, *, #41922, .T. ) ;
#6818 = ORIENTED_EDGE ( 'NONE', *, *, #59179, .F. ) ;
#6819 = FACE_OUTER_BOUND ( 'NONE', #12217, .T. ) ;
#6820 = DIRECTION ( 'NONE',  ( 0.000000000000000000, 0.7071067811865076047, -0.7071067811865875408 ) ) ;
#6821 = ORIENTED_EDGE ( 'NONE', *, *, #26234, .T. ) ;
#6822 = CARTESIAN_POINT ( 'NONE',  ( 6.849523737882818430, 10.30047626211719169, 54.00000000000000711 ) ) ;
#6823 = EDGE_CURVE ( 'NONE', #39506, #6502, #62427, .T. ) ;
#6824 = DIRECTION ( 'NONE',  ( -0.000000000000000000, 3.673940397442059868E-16, -1.000000000000000000 ) ) ;
#6825 = LINE ( 'NONE', #29437, #17056 ) ;
#6826 = VERTEX_POINT ( 'NONE', #68100 ) ;
#6827 = AXIS2_PLACEMENT_3D ( 'NONE', #40703, #25508, #52742 ) ;
#6829 = EDGE_LOOP ( 'NONE', ( #3905, #1059, #27044, #21559 ) ) ;
#6828 = LINE ( 'NONE', #18476, #27222 ) ;
#6830 = LINE ( 'NONE', #37729, #23544 ) ;
#6831 = CARTESIAN_POINT ( 'NONE',  ( 283.0000000000000568, -20.50000000000000000, -13.00000000000000178 ) ) ;
#6832 = FACE_OUTER_BOUND ( 'NONE', #47492, .T. ) ;
#6833 = PLANE ( 'NONE',  #18340 ) ;
#6834 = VERTEX_POINT ( 'NONE', #69850 ) ;
#6835 = AXIS2_PLACEMENT_3D ( 'NONE', #57699, #57350, #8904 ) ;
#6836 = DIRECTION ( 'NONE',  ( 1.000000000000000000, -1.047444401652940007E-14, 1.836970198721010706E-16 ) ) ;
#6837 = PLANE ( 'NONE',  #12676 ) ;
#6838 = ORIENTED_EDGE ( 'NONE', *, *, #43361, .F. ) ;
#6839 = VERTEX_POINT ( 'NONE', #63147 ) ;
#6840 = VECTOR ( 'NONE', #18217, 1000.000000000000000 ) ;
#6841 = EDGE_CURVE ( 'NONE', #32973, #53390, #58886, .T. ) ;
#6842 = ORIENTED_EDGE ( 'NONE', *, *, #14984, .T. ) ;
#6843 = CARTESIAN_POINT ( 'NONE',  ( 283.0000000000000568, -26.50000000000000000, 0.5000000000000000000 ) ) ;
#6844 = CARTESIAN_POINT ( 'NONE',  ( -28.00000000000000000, -16.28999999999710369, 14.50000000000000000 ) ) ;
#6845 = VECTOR ( 'NONE', #36581, 1000.000000000000000 ) ;
#6846 = EDGE_CURVE ( 'NONE', #3987, #7713, #64212, .T. ) ;
#6847 = LINE ( 'NONE', #66941, #3310 ) ;
#6848 = CARTESIAN_POINT ( 'NONE',  ( 5.257023737882819070, -3.157023737882815428, 26.00000000000000711 ) ) ;
#6849 = ORIENTED_EDGE ( 'NONE', *, *, #36414, .T. ) ;
#6850 = ORIENTED_EDGE ( 'NONE', *, *, #6246, .T. ) ;
#6851 = ORIENTED_EDGE ( 'NONE', *, *, #62341, .F. ) ;
#6852 = ADVANCED_FACE ( 'NONE', ( #68808 ), #41581, .T. ) ;
#6854 = PLANE ( 'NONE',  #42961 ) ;
#6853 = AXIS2_PLACEMENT_3D ( 'NONE', #31791, #69260, #53359 ) ;
#6855 = ORIENTED_EDGE ( 'NONE', *, *, #30649, .F. ) ;
#6856 = EDGE_CURVE ( 'NONE', #54090, #66376, #15977, .T. ) ;
#6857 = ORIENTED_EDGE ( 'NONE', *, *, #20458, .T. ) ;
#6858 = ORIENTED_EDGE ( 'NONE', *, *, #37352, .T. ) ;
#6859 = ORIENTED_EDGE ( 'NONE', *, *, #39692, .T. ) ;
#6860 = FACE_OUTER_BOUND ( 'NONE', #50682, .T. ) ;
#6861 = EDGE_CURVE ( 'NONE', #6534, #35816, #69502, .T. ) ;
#6863 = ORIENTED_EDGE ( 'NONE', *, *, #3698, .T. ) ;
#6862 = DIRECTION ( 'NONE',  ( -1.000000000000000000, -1.301042606982605321E-16, -0.000000000000000000 ) ) ;
#6864 = CARTESIAN_POINT ( 'NONE',  ( 1.690483450353418737, 10.73351654964659652, 455.0000000000000568 ) ) ;
#6865 = CARTESIAN_POINT ( 'NONE',  ( 283.0000000000000568, -42.50000000000000000, 9.950000000000001066 ) ) ;
#6866 = VECTOR ( 'NONE', #58282, 1000.000000000000000 ) ;
#6867 = DIRECTION ( 'NONE',  ( -1.000000000000000000, 0.000000000000000000, 0.000000000000000000 ) ) ;
#6868 = EDGE_CURVE ( 'NONE', #38183, #59292, #6916, .T. ) ;
#6870 = VERTEX_POINT ( 'NONE', #14711 ) ;
#6869 = DIRECTION ( 'NONE',  ( -0.000000000000000000, 1.000000000000000000, -0.000000000000000000 ) ) ;
#6871 = EDGE_CURVE ( 'NONE', #24957, #55829, #63511, .T. ) ;
#6872 = EDGE_CURVE ( 'NONE', #44485, #11292, #26369, .T. ) ;
#6873 = DIRECTION ( 'NONE',  ( 2.135044278125299371E-15, 1.000000000000000000, 0.000000000000000000 ) ) ;
#6874 = ADVANCED_FACE ( 'NONE', ( #36275 ), #57840, .F. ) ;
#6875 = EDGE_CURVE ( 'NONE', #34406, #28873, #52110, .T. ) ;
#6876 = CARTESIAN_POINT ( 'NONE',  ( 11.00000000000000000, -11.50000000000000000, -19.00000000000000000 ) ) ;
#6877 = CYLINDRICAL_SURFACE ( 'NONE', #1080, 5.250000000000000000 ) ;
#6878 = VECTOR ( 'NONE', #58644, 1000.000000000000000 ) ;
#6879 = ORIENTED_EDGE ( 'NONE', *, *, #52090, .T. ) ;
#6880 = DIRECTION ( 'NONE',  ( 0.000000000000000000, 0.000000000000000000, 1.000000000000000000 ) ) ;
#6881 = EDGE_CURVE ( 'NONE', #54084, #17940, #52188, .T. ) ;
#6882 = DIRECTION ( 'NONE',  ( 1.000000000000000000, 1.570596175624152290E-15, 0.000000000000000000 ) ) ;
#6883 = AXIS2_PLACEMENT_3D ( 'NONE', #29054, #50625, #50970 ) ;
#6884 = DIRECTION ( 'NONE',  ( 0.000000000000000000, 3.673940397442059868E-16, -1.000000000000000000 ) ) ;
#6885 = EDGE_CURVE ( 'NONE', #29779, #3392, #25686, .T. ) ;
#6886 = ORIENTED_EDGE ( 'NONE', *, *, #32454, .T. ) ;
#6888 = CARTESIAN_POINT ( 'NONE',  ( -7.250000000000000888, -8.249999999999998224, -26.00000000000001066 ) ) ;
#6887 = VECTOR ( 'NONE', #8827, 1000.000000000000000 ) ;
#6889 = CARTESIAN_POINT ( 'NONE',  ( 7.450000000000006395, 7.250000000000000888, -22.50000000000000000 ) ) ;
#6890 = CARTESIAN_POINT ( 'NONE',  ( -9.915476262117259409, 0.9414762621171833823, 54.00000000000000711 ) ) ;
#6891 = VECTOR ( 'NONE', #21721, 1000.000000000000000 ) ;
#6892 = VECTOR ( 'NONE', #29540, 1000.000000000000000 ) ;
#6893 = ORIENTED_EDGE ( 'NONE', *, *, #50578, .F. ) ;
#6894 = CARTESIAN_POINT ( 'NONE',  ( 7.249999999999995559, 8.250000000000001776, -5.000000000000000000 ) ) ;
#6895 = CARTESIAN_POINT ( 'NONE',  ( 49.00000000000000000, 20.60000000000000142, -13.86939075806900057 ) ) ;
#6896 = EDGE_CURVE ( 'NONE', #33218, #381, #63854, .T. ) ;
#6897 = CIRCLE ( 'NONE', #53266, 0.2000000000000005107 ) ;
#6898 = FACE_OUTER_BOUND ( 'NONE', #24860, .T. ) ;
#6899 = EDGE_CURVE ( 'NONE', #20240, #46397, #48290, .T. ) ;
#6900 = VERTEX_POINT ( 'NONE', #21065 ) ;
#6901 = PLANE ( 'NONE',  #1071 ) ;
#6902 = CARTESIAN_POINT ( 'NONE',  ( -29.25000000000000000, -5.000000000000000000, -11.75000000000000000 ) ) ;
#6903 = LINE ( 'NONE', #16489, #311 ) ;
#6904 = AXIS2_PLACEMENT_3D ( 'NONE', #41866, #63441, #36559 ) ;
#6905 = LINE ( 'NONE', #50039, #27852 ) ;
#6906 = DIRECTION ( 'NONE',  ( 0.000000000000000000, 1.000000000000000000, 0.000000000000000000 ) ) ;
#6907 = ORIENTED_EDGE ( 'NONE', *, *, #62170, .T. ) ;
#6908 = CARTESIAN_POINT ( 'NONE',  ( 8.250000000000005329, 8.250000000000001776, -26.00000000000001066 ) ) ;
#6909 = DIRECTION ( 'NONE',  ( -0.7671651518153065341, 0.6414496315691495809, 2.356647714346224881E-16 ) ) ;
#6910 = DIRECTION ( 'NONE',  ( 1.836970198721029934E-16, 1.836970198721010706E-16, -1.000000000000000000 ) ) ;
#6911 = CARTESIAN_POINT ( 'NONE',  ( 7.450000000000003730, -7.249999999999997335, -17.50000000000000000 ) ) ;
#6912 = CARTESIAN_POINT ( 'NONE',  ( 6.358413763958958853, 5.779227145995223580, 54.00000000000000711 ) ) ;
#6913 = ORIENTED_EDGE ( 'NONE', *, *, #19735, .F. ) ;
#6914 = EDGE_LOOP ( 'NONE', ( #61146, #42562, #29777, #67228 ) ) ;
#6915 = FACE_OUTER_BOUND ( 'NONE', #18829, .T. ) ;
#6916 = CIRCLE ( 'NONE', #46448, 2.250000000000001776 ) ;
#6917 = CYLINDRICAL_SURFACE ( 'NONE', #16495, 2.458500000000000796 ) ;
#6918 = EDGE_LOOP ( 'NONE', ( #60617, #6588, #22039, #42468 ) ) ;
#6919 = CARTESIAN_POINT ( 'NONE',  ( -11.11351654964668612, 8.693516549646636449, 455.0000000000000568 ) ) ;
#6920 = VERTEX_POINT ( 'NONE', #9768 ) ;
#6921 = CARTESIAN_POINT ( 'NONE',  ( 25.90000000000000213, 0.000000000000000000, -0.5540281690140901327 ) ) ;
#6922 = ORIENTED_EDGE ( 'NONE', *, *, #65268, .T. ) ;
#6923 = ORIENTED_EDGE ( 'NONE', *, *, #48349, .F. ) ;
#6924 = DIRECTION ( 'NONE',  ( 0.000000000000000000, -0.000000000000000000, -1.000000000000000000 ) ) ;
#6925 = AXIS2_PLACEMENT_3D ( 'NONE', #62714, #31613, #53188 ) ;
#6926 = DIRECTION ( 'NONE',  ( 0.000000000000000000, -1.000000000000000000, 0.000000000000000000 ) ) ;
#6927 = EDGE_CURVE ( 'NONE', #50486, #25888, #58901, .T. ) ;
#6928 = DIRECTION ( 'NONE',  ( -1.000000000000000000, 0.000000000000000000, 0.000000000000000000 ) ) ;
#6929 = DIRECTION ( 'NONE',  ( 0.7071067811865487940, 0.7071067811865463515, 0.000000000000000000 ) ) ;
#6930 = VERTEX_POINT ( 'NONE', #52914 ) ;
#6931 = ORIENTED_EDGE ( 'NONE', *, *, #41406, .T. ) ;
#6932 = EDGE_CURVE ( 'NONE', #24609, #58795, #63422, .T. ) ;
#6933 = FACE_OUTER_BOUND ( 'NONE', #20918, .T. ) ;
#6934 = DIRECTION ( 'NONE',  ( 0.000000000000000000, 0.000000000000000000, 1.000000000000000000 ) ) ;
#6935 = VERTEX_POINT ( 'NONE', #10451 ) ;
#6936 = EDGE_CURVE ( 'NONE', #18478, #35648, #20708, .T. ) ;
#6937 = VERTEX_POINT ( 'NONE', #32030 ) ;
#6938 = AXIS2_PLACEMENT_3D ( 'NONE', #1789, #62853, #55544 ) ;
#6939 = CLOSED_SHELL ( 'NONE', ( #28752, #14437, #2017, #66865, #35373, #14211, #25258, #19018, #7757, #65169, #59861, #47669 ) ) ;
#6941 = ORIENTED_EDGE ( 'NONE', *, *, #68215, .T. ) ;
#6940 = ITEM_DEFINED_TRANSFORMATION ( 'NONE', 'NONE', #4201,  #45918 ) ;
#6942 = DIRECTION ( 'NONE',  ( -0.000000000000000000, -1.000000000000000000, -0.000000000000000000 ) ) ;
#6943 = EDGE_CURVE ( 'NONE', #34215, #15393, #8015, .T. ) ;
#6944 = CARTESIAN_POINT ( 'NONE',  ( 3.682023737882786918, -9.737023737882809726, 54.00000000000000711 ) ) ;
#6946 = ORIENTED_EDGE ( 'NONE', *, *, #7740, .F. ) ;
#6945 = LINE ( 'NONE', #29202, #43937 ) ;
#6947 = VECTOR ( 'NONE', #42073, 1000.000000000000000 ) ;
#6948 = FACE_OUTER_BOUND ( 'NONE', #23254, .T. ) ;
#6949 = DIRECTION ( 'NONE',  ( -1.836970198721029934E-16, 1.836970198721036344E-16, -1.000000000000000000 ) ) ;
#6950 = VERTEX_POINT ( 'NONE', #44008 ) ;
#6951 = ORIENTED_EDGE ( 'NONE', *, *, #55273, .T. ) ;
#6952 = CIRCLE ( 'NONE', #17157, 1.224999999999999423 ) ;
#6953 = EDGE_CURVE ( 'NONE', #9826, #51301, #34018, .T. ) ;
#6954 = DIRECTION ( 'NONE',  ( 0.000000000000000000, 0.000000000000000000, -1.000000000000000000 ) ) ;
#6955 = DIRECTION ( 'NONE',  ( -1.000000000000000000, 0.000000000000000000, 0.000000000000000000 ) ) ;
#6956 =( REPRESENTATION_RELATIONSHIP ('NONE','NONE', #4299, #26379 ) REPRESENTATION_RELATIONSHIP_WITH_TRANSFORMATION ( #54706 )SHAPE_REPRESENTATION_RELATIONSHIP( ) );
#6957 = CARTESIAN_POINT ( 'NONE',  ( -12.00000000000000000, -11.18999999999999950, 0.000000000000000000 ) ) ;
#6958 = CARTESIAN_POINT ( 'NONE',  ( 2.290483450353415495, 9.828310488885934504, 455.0000000000000568 ) ) ;
#6959 = FACE_OUTER_BOUND ( 'NONE', #54193, .T. ) ;
#6960 = VECTOR ( 'NONE', #30543, 1000.000000000000000 ) ;
#6962 = ORIENTED_EDGE ( 'NONE', *, *, #56752, .T. ) ;
#6961 = DIRECTION ( 'NONE',  ( -1.000000000000000000, 0.000000000000000000, 0.000000000000000000 ) ) ;
#6963 = VERTEX_POINT ( 'NONE', #54997 ) ;
#6964 = CARTESIAN_POINT ( 'NONE',  ( -10.49297626211729551, -6.849523737882748264, 54.00000000000000711 ) ) ;
#6965 = DIRECTION ( 'NONE',  ( 0.000000000000000000, 0.000000000000000000, 1.000000000000000000 ) ) ;
#6966 = CARTESIAN_POINT ( 'NONE',  ( 7.250000000000005329, 8.250000000000001776, -26.00000000000001066 ) ) ;
#6967 = DIRECTION ( 'NONE',  ( -1.000000000000000000, 0.000000000000000000, 0.000000000000000000 ) ) ;
#6968 = DIRECTION ( 'NONE',  ( 0.000000000000000000, -0.1249999999999996531, -0.9921567416492215186 ) ) ;
#6969 = ORIENTED_EDGE ( 'NONE', *, *, #14227, .T. ) ;
#6970 = DIRECTION ( 'NONE',  ( 0.000000000000000000, -3.673940397442059868E-16, 1.000000000000000000 ) ) ;
#6971 = CARTESIAN_POINT ( 'NONE',  ( 6.364920264886884560, 6.822336235477388655, 26.00000000000000711 ) ) ;
#6972 = EDGE_CURVE ( 'NONE', #35692, #2415, #59594, .T. ) ;
#6973 = CYLINDRICAL_SURFACE ( 'NONE', #569, 0.1749999999999998224 ) ;
#6974 = CARTESIAN_POINT ( 'NONE',  ( 275.0000000000000000, -25.60000000000000142, -17.60000000000000142 ) ) ;
#6975 = PRODUCT ( '5537T808_T-Slotted Framing_5537T808', '5537T808_T-Slotted Framing_5537T808', '', ( #40946 ) ) ;
#6976 = EDGE_CURVE ( 'NONE', #24784, #64534, #32381, .T. ) ;
#6977 = LINE ( 'NONE', #49449, #36035 ) ;
#6978 = EDGE_CURVE ( 'NONE', #13295, #29848, #6546, .T. ) ;
#6979 = FACE_OUTER_BOUND ( 'NONE', #6423, .T. ) ;
#6980 = CARTESIAN_POINT ( 'NONE',  ( -9.791916549646867196, -11.08848345035335115, 455.0000000000000568 ) ) ;
#6981 = VERTEX_POINT ( 'NONE', #59931 ) ;
#6982 = DIRECTION ( 'NONE',  ( -1.836970198721029934E-16, -1.836970198721010706E-16, 1.000000000000000000 ) ) ;
#6983 = CARTESIAN_POINT ( 'NONE',  ( -9.689726262117314803, -8.580623737882756785, 54.00000000000000711 ) ) ;
#6984 = ORIENTED_EDGE ( 'NONE', *, *, #67464, .T. ) ;
#6985 = DIRECTION ( 'NONE',  ( 0.000000000000000000, 1.000000000000000000, 0.000000000000000000 ) ) ;
#6986 = VECTOR ( 'NONE', #12910, 1000.000000000000000 ) ;
#6987 = AXIS2_PLACEMENT_3D ( 'NONE', #13268, #12902, #35524 ) ;
#6988 = DIRECTION ( 'NONE',  ( -0.4999999999989371835, 0.000000000000000000, -0.8660254037850523279 ) ) ;
#6989 = FACE_OUTER_BOUND ( 'NONE', #17742, .T. ) ;
#6990 = CARTESIAN_POINT ( 'NONE',  ( 50.83090410532631864, 63.65740854044500452, 2.000000000000000000 ) ) ;
#6991 = DIRECTION ( 'NONE',  ( 0.000000000000000000, 0.000000000000000000, 1.000000000000000000 ) ) ;
#6992 = AXIS2_PLACEMENT_3D ( 'NONE', #59386, #64013, #38182 ) ;
#6993 = VERTEX_POINT ( 'NONE', #50006 ) ;
#6994 = DIRECTION ( 'NONE',  ( 1.000000000000000000, -0.000000000000000000, -0.000000000000000000 ) ) ;
#6995 = ORIENTED_EDGE ( 'NONE', *, *, #34646, .F. ) ;
#6996 = PLANE ( 'NONE',  #25484 ) ;
#6997 = ORIENTED_EDGE ( 'NONE', *, *, #6896, .T. ) ;
#6998 = CARTESIAN_POINT ( 'NONE',  ( 10.92648345035335922, 9.293516549646611224, 195.0000000000000284 ) ) ;
#6999 = AXIS2_PLACEMENT_3D ( 'NONE', #48751, #25800, #21191 ) ;
#7000 = FILL_AREA_STYLE ('',( #45171 ) ) ;
#7001 = FACE_OUTER_BOUND ( 'NONE', #12507, .T. ) ;
#7002 = VERTEX_POINT ( 'NONE', #542 ) ;
#7003 = ORIENTED_EDGE ( 'NONE', *, *, #26485, .F. ) ;
#7004 = DIRECTION ( 'NONE',  ( -1.000000000000000000, 0.000000000000000000, 0.000000000000000000 ) ) ;
#7005 = ORIENTED_EDGE ( 'NONE', *, *, #9461, .T. ) ;
#7006 = VERTEX_POINT ( 'NONE', #33059 ) ;
#7008 = ADVANCED_FACE ( 'NONE', ( #60268 ), #49341, .F. ) ;
#7007 = PRODUCT_DEFINITION_CONTEXT ( 'detailed design', #40428, 'design' ) ;
#7009 = DIRECTION ( 'NONE',  ( 1.836970198721029934E-16, 1.836970198721010706E-16, -1.000000000000000000 ) ) ;
#7010 = LINE ( 'NONE', #65732, #56115 ) ;
#7011 = DIRECTION ( 'NONE',  ( 0.000000000000000000, -3.673940397442059868E-16, 1.000000000000000000 ) ) ;
#7012 = VERTEX_POINT ( 'NONE', #32715 ) ;
#7013 = EDGE_CURVE ( 'NONE', #66290, #26713, #1279, .T. ) ;
#7014 = CARTESIAN_POINT ( 'NONE',  ( 18.85410196625000268, -15.50000000000000000, -21.50000000000000000 ) ) ;
#7016 = DIRECTION ( 'NONE',  ( 0.000000000000000000, 0.000000000000000000, -1.000000000000000000 ) ) ;
#7015 = DIRECTION ( 'NONE',  ( 0.000000000000000000, 1.000000000000000000, 0.000000000000000000 ) ) ;
#7017 = VERTEX_POINT ( 'NONE', #38709 ) ;
#7019 = ORIENTED_EDGE ( 'NONE', *, *, #9734, .F. ) ;
#7018 = CARTESIAN_POINT ( 'NONE',  ( -3.842976262117224984, 9.897976262117168744, 54.00000000000000711 ) ) ;
#7020 = EDGE_CURVE ( 'NONE', #21729, #40956, #43321, .T. ) ;
#7021 = TOROIDAL_SURFACE ( 'NONE', #5929, 0.06000000000000080963, 0.7500000000000000000 ) ;
#7022 = VERTEX_POINT ( 'NONE', #28104 ) ;
#7023 = EDGE_CURVE ( 'NONE', #27652, #40990, #22461, .T. ) ;
#7024 = EDGE_CURVE ( 'NONE', #52964, #3924, #22797, .T. ) ;
#7025 = EDGE_CURVE ( 'NONE', #7104, #14185, #66282, .T. ) ;
#7026 = LINE ( 'NONE', #50167, #59253 ) ;
#7027 = CIRCLE ( 'NONE', #46548, 0.1999999999999987899 ) ;
#7028 = VERTEX_POINT ( 'NONE', #60955 ) ;
#7029 = DIRECTION ( 'NONE',  ( -0.7071067811865464625, 0.7071067811865486830, 0.000000000000000000 ) ) ;
#7030 = EDGE_CURVE ( 'NONE', #13690, #66560, #39055, .T. ) ;
#7031 = CARTESIAN_POINT ( 'NONE',  ( 24.90000000000000213, 20.60000000000000142, -13.86939075806900057 ) ) ;
#7032 = ORIENTED_EDGE ( 'NONE', *, *, #12680, .T. ) ;
#7033 = ORIENTED_EDGE ( 'NONE', *, *, #32037, .T. ) ;
#7034 = DIRECTION ( 'NONE',  ( 0.000000000000000000, 0.000000000000000000, 1.000000000000000000 ) ) ;
#7035 = FACE_OUTER_BOUND ( 'NONE', #49035, .T. ) ;
#7036 = CIRCLE ( 'NONE', #26247, 0.1749999999999998224 ) ;
#7037 = ORIENTED_EDGE ( 'NONE', *, *, #52038, .F. ) ;
#7038 = CARTESIAN_POINT ( 'NONE',  ( -4.173516549646669738, 11.77351654964658678, 455.0000000000000568 ) ) ;
#7039 = CARTESIAN_POINT ( 'NONE',  ( -6.835476262117333057, -10.31452373788278543, 54.00000000000000711 ) ) ;
#7040 = CARTESIAN_POINT ( 'NONE',  ( 11.50000000000000000, -11.50000000000000000, -11.00000000000000000 ) ) ;
#7041 = ORIENTED_EDGE ( 'NONE', *, *, #58586, .F. ) ;
#7042 = DIRECTION ( 'NONE',  ( 0.000000000000000000, 0.000000000000000000, 1.000000000000000000 ) ) ;
#7043 = CARTESIAN_POINT ( 'NONE',  ( 11.50000000000000000, -12.00000000000000000, 10.69999999999999929 ) ) ;
#7045 = ORIENTED_EDGE ( 'NONE', *, *, #60157, .F. ) ;
#7044 =( NAMED_UNIT ( * ) SI_UNIT ( $, .STERADIAN. ) SOLID_ANGLE_UNIT ( ) );
#7047 = VERTEX_POINT ( 'NONE', #38375 ) ;
#7046 = CARTESIAN_POINT ( 'NONE',  ( 10.92648345035335922, 2.693516549646528091, 455.0000000000000568 ) ) ;
#7049 = LINE ( 'NONE', #1751, #34754 ) ;
#7048 = VECTOR ( 'NONE', #42660, 1000.000000000000000 ) ;
#7050 = VECTOR ( 'NONE', #35741, 1000.000000000000114 ) ;
#7051 = FACE_OUTER_BOUND ( 'NONE', #16173, .T. ) ;
#7052 = CARTESIAN_POINT ( 'NONE',  ( 8.250000000000005329, -8.249999999999998224, -26.00000000000001066 ) ) ;
#7053 = DIRECTION ( 'NONE',  ( 0.6414496315691565753, -0.7671651518153006499, -2.818519042764004597E-16 ) ) ;
#7054 = CIRCLE ( 'NONE', #13878, 0.5999999999999989786 ) ;
#7055 = DIRECTION ( 'NONE',  ( 0.000000000000000000, 1.000000000000000000, 0.000000000000000000 ) ) ;
#7056 = VERTEX_POINT ( 'NONE', #60625 ) ;
#7057 = DIRECTION ( 'NONE',  ( 1.000000000000000000, -1.130039751537442024E-14, -1.836970198721050642E-16 ) ) ;
#7058 = DIRECTION ( 'NONE',  ( 1.000000000000000000, 0.000000000000000000, 0.000000000000000000 ) ) ;
#7059 = PLANE ( 'NONE',  #4013 ) ;
#7061 = VERTEX_POINT ( 'NONE', #27759 ) ;
#7060 = FACE_OUTER_BOUND ( 'NONE', #64004, .T. ) ;
#7062 = DIRECTION ( 'NONE',  ( 0.000000000000000000, 0.000000000000000000, 1.000000000000000000 ) ) ;
#7063 = VECTOR ( 'NONE', #46353, 1000.000000000000000 ) ;
#7064 = EDGE_CURVE ( 'NONE', #11694, #21614, #27064, .T. ) ;
#7065 = DIRECTION ( 'NONE',  ( 0.000000000000000000, -0.000000000000000000, 1.000000000000000000 ) ) ;
#7066 = EDGE_CURVE ( 'NONE', #30690, #3076, #69067, .T. ) ;
#7067 = VERTEX_POINT ( 'NONE', #12176 ) ;
#7068 = DIRECTION ( 'NONE',  ( -0.7071067811865529018, -0.7071067811865422437, 0.000000000000000000 ) ) ;
#7069 = CARTESIAN_POINT ( 'NONE',  ( -7.955476262117322506, -9.737023737882765317, 26.00000000000000000 ) ) ;
#7070 = AXIS2_PLACEMENT_3D ( 'NONE', #17871, #13955, #60991 ) ;
#7072 = ORIENTED_EDGE ( 'NONE', *, *, #54508, .F. ) ;
#7071 = ADVANCED_FACE ( 'NONE', ( #911 ), #28434, .T. ) ;
#7073 = DIRECTION ( 'NONE',  ( 0.000000000000000000, 0.000000000000000000, 1.000000000000000000 ) ) ;
#7074 = FACE_OUTER_BOUND ( 'NONE', #4115, .T. ) ;
#7075 = LINE ( 'NONE', #40652, #17840 ) ;
#7076 = AXIS2_PLACEMENT_3D ( 'NONE', #37694, #32044, #5177 ) ;
#7077 = CARTESIAN_POINT ( 'NONE',  ( 23.75054448485400016, -17.50000000000000000, -25.53140320652400064 ) ) ;
#7078 = CARTESIAN_POINT ( 'NONE',  ( -8.513516549646713116, 11.29351654964659701, 455.0000000000000568 ) ) ;
#7079 = EDGE_LOOP ( 'NONE', ( #9092, #31609, #40649, #12720 ) ) ;
#7080 = DIRECTION ( 'NONE',  ( -1.048062100069321163E-14, -1.000000000000000000, 0.000000000000000000 ) ) ;
#7081 = ORIENTED_EDGE ( 'NONE', *, *, #37969, .T. ) ;
#7082 = VERTEX_POINT ( 'NONE', #54643 ) ;
#7083 = VECTOR ( 'NONE', #16261, 1000.000000000000000 ) ;
#7084 = CARTESIAN_POINT ( 'NONE',  ( 4.186483450353335023, -12.00648345035347830, 455.0000000000000568 ) ) ;
#7085 = DIRECTION ( 'NONE',  ( -0.000000000000000000, -0.000000000000000000, -1.000000000000000000 ) ) ;
#7086 = FACE_OUTER_BOUND ( 'NONE', #50925, .T. ) ;
#7087 = CARTESIAN_POINT ( 'NONE',  ( 25.50000000000000355, 0.000000000000000000, -24.75000000000000000 ) ) ;
#7088 = ORIENTED_EDGE ( 'NONE', *, *, #22135, .T. ) ;
#7089 = ORIENTED_EDGE ( 'NONE', *, *, #11221, .F. ) ;
#7090 = DIRECTION ( 'NONE',  ( 0.000000000000000000, 0.000000000000000000, -1.000000000000000000 ) ) ;
#7091 = EDGE_LOOP ( 'NONE', ( #44941, #6704, #46570, #48537 ) ) ;
#7092 = DIRECTION ( 'NONE',  ( 0.000000000000000000, 0.000000000000000000, -1.000000000000000000 ) ) ;
#7093 = VECTOR ( 'NONE', #15654, 1000.000000000000000 ) ;
#7094 = CARTESIAN_POINT ( 'NONE',  ( 1.866219381641485375, 9.404046420174006826, 455.0000000000000568 ) ) ;
#7095 = LINE ( 'NONE', #12060, #18393 ) ;
#7096 = FACE_BOUND ( 'NONE', #16177, .T. ) ;
#7098 = CARTESIAN_POINT ( 'NONE',  ( 7.250000000000005329, 7.250000000000000888, -12.00000000000000000 ) ) ;
#7097 = FACE_OUTER_BOUND ( 'NONE', #30050, .T. ) ;
#7099 = VECTOR ( 'NONE', #7331, 1000.000000000000000 ) ;
#7100 = ORIENTED_EDGE ( 'NONE', *, *, #56609, .F. ) ;
#7102 = ORIENTED_EDGE ( 'NONE', *, *, #14352, .T. ) ;
#7101 = CARTESIAN_POINT ( 'NONE',  ( 69.92576880110416937, 10.00000000000000000, 335.4830310981152479 ) ) ;
#7103 = VERTEX_POINT ( 'NONE', #23131 ) ;
#7104 = VERTEX_POINT ( 'NONE', #35479 ) ;
#7105 = CIRCLE ( 'NONE', #43263, 0.1999999999999996503 ) ;
#7106 = EDGE_CURVE ( 'NONE', #18604, #36864, #40448, .T. ) ;
#7107 = CARTESIAN_POINT ( 'NONE',  ( -14.25000000000000000, -0.2038245569916330158, -21.77831216351300014 ) ) ;
#7108 = DIRECTION ( 'NONE',  ( 1.000000000000000000, -0.000000000000000000, 0.000000000000000000 ) ) ;
#7109 = VECTOR ( 'NONE', #43486, 1000.000000000000000 ) ;
#7110 = EDGE_CURVE ( 'NONE', #67414, #3728, #14917, .T. ) ;
#7111 = DIRECTION ( 'NONE',  ( -1.000000000000000000, 7.665540703601096574E-15, 0.000000000000000000 ) ) ;
#7112 = ORIENTED_EDGE ( 'NONE', *, *, #12025, .F. ) ;
#7113 = EDGE_CURVE ( 'NONE', #57421, #20590, #56644, .T. ) ;
#7114 = ORIENTED_EDGE ( 'NONE', *, *, #58238, .F. ) ;
#7115 = LINE ( 'NONE', #12758, #20751 ) ;
#7116 = CARTESIAN_POINT ( 'NONE',  ( 15.50000000000000000, -0.2038245569916604938, -21.05662432702600029 ) ) ;
#7117 = CIRCLE ( 'NONE', #47770, 0.1749999999999989342 ) ;
#7118 = ORIENTED_EDGE ( 'NONE', *, *, #1487, .T. ) ;
#7119 = ORIENTED_EDGE ( 'NONE', *, *, #61058, .F. ) ;
#7120 = DIRECTION ( 'NONE',  ( 1.000000000000000000, -0.000000000000000000, 0.000000000000000000 ) ) ;
#7121 = VECTOR ( 'NONE', #38621, 1000.000000000000000 ) ;
#7122 = PLANE ( 'NONE',  #37964 ) ;
#7124 = VERTEX_POINT ( 'NONE', #50700 ) ;
#7123 = EDGE_CURVE ( 'NONE', #10609, #52775, #62006, .T. ) ;
#7125 = DIRECTION ( 'NONE',  ( -0.000000000000000000, -0.000000000000000000, -1.000000000000000000 ) ) ;
#7126 = VECTOR ( 'NONE', #34586, 1000.000000000000000 ) ;
#7128 = ORIENTED_EDGE ( 'NONE', *, *, #50695, .T. ) ;
#7127 =( NAMED_UNIT ( * ) PLANE_ANGLE_UNIT ( ) SI_UNIT ( $, .RADIAN. ) );
#7129 = ORIENTED_EDGE ( 'NONE', *, *, #19563, .T. ) ;
#7130 = CARTESIAN_POINT ( 'NONE',  ( -7.750000000000001776, -7.348062532927999158, 5.000000000000000000 ) ) ;
#7131 = DIRECTION ( 'NONE',  ( -1.000000000000000000, 0.000000000000000000, 0.000000000000000000 ) ) ;
#7132 = DIRECTION ( 'NONE',  ( 0.000000000000000000, 1.000000000000000000, 0.000000000000000000 ) ) ;
#7133 = CARTESIAN_POINT ( 'NONE',  ( 7.616533956692197016, 8.393516549646621527, 195.0000000000000284 ) ) ;
#7134 = CARTESIAN_POINT ( 'NONE',  ( -3.667976262117330410, -9.912023737882817542, 54.00000000000000711 ) ) ;
#7135 = CARTESIAN_POINT ( 'NONE',  ( 283.0000000000000568, -20.85424868893542083, 17.35424868893542083 ) ) ;
#7136 = ORIENTED_EDGE ( 'NONE', *, *, #38484, .T. ) ;
#7137 = CARTESIAN_POINT ( 'NONE',  ( -7.593516549646711411, 11.77351654964660277, 455.0000000000000568 ) ) ;
#7139 = VERTEX_POINT ( 'NONE', #34079 ) ;
#7138 = CARTESIAN_POINT ( 'NONE',  ( 0.5000000000000000000, 0.000000000000000000, 30.00000000000000000 ) ) ;
#7140 = DIRECTION ( 'NONE',  ( 0.000000000000000000, 0.000000000000000000, 1.000000000000000000 ) ) ;
#7141 = AXIS2_PLACEMENT_3D ( 'NONE', #65782, #6055, #55181 ) ;
#7142 = VECTOR ( 'NONE', #34137, 1000.000000000000000 ) ;
#7143 = FACE_OUTER_BOUND ( 'NONE', #67127, .T. ) ;
#7144 = CARTESIAN_POINT ( 'NONE',  ( 10.05377373788281226, 9.689726262117156708, 26.00000000000000711 ) ) ;
#7146 = FACE_OUTER_BOUND ( 'NONE', #25978, .T. ) ;
#7145 = VECTOR ( 'NONE', #18035, 1000.000000000000000 ) ;
#7147 = AXIS2_PLACEMENT_3D ( 'NONE', #5472, #68415, #15022 ) ;
#7148 = DIRECTION ( 'NONE',  ( 0.9375000000000004441, 0.000000000000000000, -0.3479852726768752902 ) ) ;
#7149 = AXIS2_PLACEMENT_3D ( 'NONE', #30175, #3653, #61632 ) ;
#7150 = VERTEX_POINT ( 'NONE', #19575 ) ;
#7152 = VERTEX_POINT ( 'NONE', #18888 ) ;
#7151 = EDGE_CURVE ( 'NONE', #31478, #51178, #13576, .T. ) ;
#7153 = STYLED_ITEM ( 'NONE', ( #37775 ), #43035 ) ;
#7154 = DIRECTION ( 'NONE',  ( -1.084202172485504434E-16, 1.000000000000000000, 0.000000000000000000 ) ) ;
#7155 = AXIS2_PLACEMENT_3D ( 'NONE', #23156, #60977, #7232 ) ;
#7156 = LINE ( 'NONE', #39683, #24385 ) ;
#7157 = CARTESIAN_POINT ( 'NONE',  ( 5.257023737882819070, -5.257023737882825287, 54.00000000000000711 ) ) ;
#7158 = ORIENTED_EDGE ( 'NONE', *, *, #58638, .F. ) ;
#7159 = CARTESIAN_POINT ( 'NONE',  ( 11.75000000000000000, -5.000000000000000000, -26.25000000000000000 ) ) ;
#7160 = ORIENTED_EDGE ( 'NONE', *, *, #25476, .T. ) ;
#7161 = ORIENTED_EDGE ( 'NONE', *, *, #55642, .T. ) ;
#7162 = DIRECTION ( 'NONE',  ( 0.000000000000000000, 3.673940397442059868E-16, -1.000000000000000000 ) ) ;
#7163 = FACE_OUTER_BOUND ( 'NONE', #11478, .T. ) ;
#7165 = EDGE_LOOP ( 'NONE', ( #9178, #68433, #39645, #38401 ) ) ;
#7164 = EDGE_CURVE ( 'NONE', #5551, #37065, #40076, .T. ) ;
#7166 = FACE_OUTER_BOUND ( 'NONE', #19143, .T. ) ;
#7167 = DIRECTION ( 'NONE',  ( 0.000000000000000000, 0.000000000000000000, -1.000000000000000000 ) ) ;
#7168 = EDGE_CURVE ( 'NONE', #11406, #23447, #61658, .T. ) ;
#7169 = DIRECTION ( 'NONE',  ( 0.000000000000000000, 0.000000000000000000, 1.000000000000000000 ) ) ;
#7170 = ORIENTED_EDGE ( 'NONE', *, *, #12463, .T. ) ;
#7172 = ORIENTED_EDGE ( 'NONE', *, *, #63043, .T. ) ;
#7171 = DIRECTION ( 'NONE',  ( 0.000000000000000000, 0.000000000000000000, -1.000000000000000000 ) ) ;
#7173 = DIRECTION ( 'NONE',  ( 1.000000000000000000, 0.000000000000000000, 0.000000000000000000 ) ) ;
#7174 = LINE ( 'NONE', #19193, #64348 ) ;
#7175 = CARTESIAN_POINT ( 'NONE',  ( -30.00000000000000000, -5.599999999999999645, -27.00000000000000000 ) ) ;
#7176 = CARTESIAN_POINT ( 'NONE',  ( 9.562023737882812569, -2.369523737882825998, 54.00000000000000711 ) ) ;
#7177 = DIRECTION ( 'NONE',  ( 0.9375000000000004441, 0.000000000000000000, 0.3479852726768752902 ) ) ;
#7178 = DIRECTION ( 'NONE',  ( -0.000000000000000000, -0.000000000000000000, -1.000000000000000000 ) ) ;
#7179 = ORIENTED_EDGE ( 'NONE', *, *, #61740, .F. ) ;
#7180 = ORIENTED_EDGE ( 'NONE', *, *, #1238, .F. ) ;
#7181 = ORIENTED_EDGE ( 'NONE', *, *, #67951, .T. ) ;
#7182 = CARTESIAN_POINT ( 'NONE',  ( 4.046023737882819660, -3.157023737882815873, 26.00000000000000711 ) ) ;
#7183 = DIRECTION ( 'NONE',  ( -0.000000000000000000, -0.000000000000000000, -1.000000000000000000 ) ) ;
#7185 = EDGE_CURVE ( 'NONE', #63319, #7047, #7571, .T. ) ;
#7184 = LINE ( 'NONE', #55310, #31545 ) ;
#7186 = SHAPE_REPRESENTATION_RELATIONSHIP ( 'NONE' , 'NONE' ,  #25847, #25951 ) ;
#7187 = AXIS2_PLACEMENT_3D ( 'NONE', #19770, #52316, #57264 ) ;
#7188 = EDGE_CURVE ( 'NONE', #29997, #6582, #18518, .T. ) ;
#7189 = ORIENTED_EDGE ( 'NONE', *, *, #2117, .T. ) ;
#7190 = ORIENTED_EDGE ( 'NONE', *, *, #63477, .F. ) ;
#7191 = ADVANCED_FACE ( 'NONE', ( #45042, #51763, #66619 ), #30193, .F. ) ;
#7192 = VERTEX_POINT ( 'NONE', #18172 ) ;
#7193 = DIRECTION ( 'NONE',  ( -0.7071067811865550112, -0.7071067811865401342, -2.597868168706466299E-16 ) ) ;
#7194 = ORIENTED_EDGE ( 'NONE', *, *, #26304, .F. ) ;
#7195 = AXIS2_PLACEMENT_3D ( 'NONE', #2572, #24498, #35794 ) ;
#7196 = AXIS2_PLACEMENT_3D ( 'NONE', #34617, #50880, #8808 ) ;
#7197 = EDGE_CURVE ( 'NONE', #30907, #29553, #23834, .T. ) ;
#7198 = ORIENTED_EDGE ( 'NONE', *, *, #19421, .F. ) ;
#7200 = ORIENTED_EDGE ( 'NONE', *, *, #43405, .T. ) ;
#7199 = ADVANCED_FACE ( 'NONE', ( #39734 ), #56359, .T. ) ;
#7201 = ORIENTED_EDGE ( 'NONE', *, *, #8252, .T. ) ;
#7202 = VECTOR ( 'NONE', #6628, 1000.000000000000000 ) ;
#7203 = FACE_OUTER_BOUND ( 'NONE', #67307, .T. ) ;
#7204 = VECTOR ( 'NONE', #49894, 1000.000000000000000 ) ;
#7205 = CIRCLE ( 'NONE', #51123, 0.1749999999999998224 ) ;
#7206 = EDGE_CURVE ( 'NONE', #69116, #35743, #62354, .T. ) ;
#7208 = ORIENTED_EDGE ( 'NONE', *, *, #66270, .T. ) ;
#7207 = FACE_OUTER_BOUND ( 'NONE', #31511, .T. ) ;
#7209 = EDGE_CURVE ( 'NONE', #17361, #8765, #29485, .T. ) ;
#7210 = FACE_OUTER_BOUND ( 'NONE', #6351, .T. ) ;
#7211 = DIRECTION ( 'NONE',  ( -1.000000000000000000, 0.000000000000000000, 0.000000000000000000 ) ) ;
#7212 = CARTESIAN_POINT ( 'NONE',  ( -7.250000000000001776, -7.249999999999998224, -10.00000000000000000 ) ) ;
#7214 = ORIENTED_EDGE ( 'NONE', *, *, #20688, .T. ) ;
#7213 = CARTESIAN_POINT ( 'NONE',  ( -7.250000000000001776, -7.249999999999998224, -26.00000000000001066 ) ) ;
#7215 = VECTOR ( 'NONE', #797, 1000.000000000000000 ) ;
#7216 = DIRECTION ( 'NONE',  ( 0.000000000000000000, 0.000000000000000000, 1.000000000000000000 ) ) ;
#7217 = DIRECTION ( 'NONE',  ( -0.000000000000000000, -0.000000000000000000, -1.000000000000000000 ) ) ;
#7218 = DIRECTION ( 'NONE',  ( -1.000000000000000000, 0.000000000000000000, 0.000000000000000000 ) ) ;
#7219 = ORIENTED_EDGE ( 'NONE', *, *, #23038, .F. ) ;
#7220 = FACE_OUTER_BOUND ( 'NONE', #68173, .T. ) ;
#7221 =( BOUNDED_CURVE ( )  B_SPLINE_CURVE ( 3, ( #38405, #33092, #55362, #27789 ),
 .UNSPECIFIED., .F., .F. ) 
 B_SPLINE_CURVE_WITH_KNOTS ( ( 4, 4 ),
 ( 5.435123228198102119, 5.560451059366170234 ),
 .UNSPECIFIED. ) 
 CURVE ( )  GEOMETRIC_REPRESENTATION_ITEM ( )  RATIONAL_B_SPLINE_CURVE ( ( 1.000000000000000000, 0.9986915061577686936, 0.9986915061577686936, 1.000000000000000000 ) ) 
 REPRESENTATION_ITEM ( '' )  );
#7222 = CARTESIAN_POINT ( 'NONE',  ( -29.25000000000000000, -5.000000000000000000, -11.75000000000000000 ) ) ;
#7223 = CARTESIAN_POINT ( 'NONE',  ( 49.49874101024862227, 0.7500000000000000000, -4.436434848928188401 ) ) ;
#7224 = ADVANCED_FACE ( 'NONE', ( #45739 ), #67328, .T. ) ;
#7225 = ORIENTED_EDGE ( 'NONE', *, *, #65832, .T. ) ;
#7226 = DIRECTION ( 'NONE',  ( -1.000000000000000000, 0.000000000000000000, 0.000000000000000000 ) ) ;
#7227 = DIRECTION ( 'NONE',  ( 0.000000000000000000, -1.000000000000000000, 0.000000000000000000 ) ) ;
#7228 = DIRECTION ( 'NONE',  ( 0.000000000000000000, -0.6787500000000000755, -0.7343694148723788340 ) ) ;
#7229 = AXIS2_PLACEMENT_3D ( 'NONE', #55785, #1354, #7330 ) ;
#7230 = EDGE_CURVE ( 'NONE', #749, #62902, #57054, .T. ) ;
#7231 = EDGE_LOOP ( 'NONE', ( #37845, #3062, #64497, #58324 ) ) ;
#7232 = DIRECTION ( 'NONE',  ( 1.000000000000000000, 0.000000000000000000, 0.000000000000000000 ) ) ;
#7233 = LINE ( 'NONE', #47100, #31703 ) ;
#7234 = CARTESIAN_POINT ( 'NONE',  ( -7.450000000000001954, 0.000000000000000000, -13.50000000000000178 ) ) ;
#7235 = CARTESIAN_POINT ( 'NONE',  ( 4.406483450353373854, 11.31351654964663211, 195.0000000000000284 ) ) ;
#7236 = AXIS2_PLACEMENT_3D ( 'NONE', #20659, #3356, #52146 ) ;
#7237 = AXIS2_PLACEMENT_3D ( 'NONE', #21316, #64799, #27657 ) ;
#7238 = ORIENTED_EDGE ( 'NONE', *, *, #46194, .T. ) ;
#7239 = CARTESIAN_POINT ( 'NONE',  ( 49.00000000000000000, -0.2000000000089119934, -8.913009219568841313E-12 ) ) ;
#7240 = LINE ( 'NONE', #45074, #67045 ) ;
#7241 = CARTESIAN_POINT ( 'NONE',  ( -10.03972626211732155, -9.703773737882716688, 26.00000000000000000 ) ) ;
#7242 = DIRECTION ( 'NONE',  ( 1.836970198721029934E-16, 1.836970198721010706E-16, -1.000000000000000000 ) ) ;
#7243 = DIRECTION ( 'NONE',  ( 0.000000000000000000, 0.000000000000000000, 1.000000000000000000 ) ) ;
#7244 = VECTOR ( 'NONE', #46319, 1000.000000000000114 ) ;
#7245 = ORIENTED_EDGE ( 'NONE', *, *, #48956, .T. ) ;
#7246 = AXIS2_PLACEMENT_3D ( 'NONE', #65525, #38986, #39668 ) ;
#7247 = DIRECTION ( 'NONE',  ( -0.4999999999989410693, 0.000000000000000000, -0.8660254037850499964 ) ) ;
#7248 = PLANE ( 'NONE',  #11338 ) ;
#7249 = CARTESIAN_POINT ( 'NONE',  ( -24.00000000000000000, -16.28999999999999915, 14.50000000000000000 ) ) ;
#7250 = DIRECTION ( 'NONE',  ( 0.000000000000000000, 0.000000000000000000, -1.000000000000000000 ) ) ;
#7251 = EDGE_CURVE ( 'NONE', #414, #35831, #19231, .T. ) ;
#7252 = DIRECTION ( 'NONE',  ( 0.000000000000000000, 0.000000000000000000, 1.000000000000000000 ) ) ;
#7253 = VERTEX_POINT ( 'NONE', #42193 ) ;
#7254 = ORIENTED_EDGE ( 'NONE', *, *, #61101, .T. ) ;
#7255 = DIRECTION ( 'NONE',  ( -1.000000000000000000, 0.000000000000000000, 0.000000000000000000 ) ) ;
#7256 = DIRECTION ( 'NONE',  ( 0.000000000000000000, 0.000000000000000000, 1.000000000000000000 ) ) ;
#7257 = AXIS2_PLACEMENT_3D ( 'NONE', #19145, #24096, #57678 ) ;
#7259 = ORIENTED_EDGE ( 'NONE', *, *, #63855, .F. ) ;
#7258 = EDGE_CURVE ( 'NONE', #15497, #13690, #14287, .T. ) ;
#7260 = EDGE_CURVE ( 'NONE', #17425, #39081, #47166, .T. ) ;
#7261 = DIRECTION ( 'NONE',  ( 1.836970198721029934E-16, 1.836970198721010706E-16, -1.000000000000000000 ) ) ;
#7262 = EDGE_CURVE ( 'NONE', #63019, #21681, #4029, .T. ) ;
#7263 = EDGE_LOOP ( 'NONE', ( #24941, #10656, #33634, #63029 ) ) ;
#7264 = ADVANCED_FACE ( 'NONE', ( #57760 ), #52109, .F. ) ;
#7265 = EDGE_CURVE ( 'NONE', #48513, #45585, #65679, .T. ) ;
#7266 = LINE ( 'NONE', #56413, #11987 ) ;
#7267 = ORIENTED_EDGE ( 'NONE', *, *, #30649, .T. ) ;
#7268 = ORIENTED_EDGE ( 'NONE', *, *, #16070, .F. ) ;
#7269 = LINE ( 'NONE', #28157, #57733 ) ;
#7270 = LINE ( 'NONE', #28493, #45552 ) ;
#7271 = EDGE_CURVE ( 'NONE', #12301, #57153, #30893, .T. ) ;
#7272 = CARTESIAN_POINT ( 'NONE',  ( 6.500000000000000888, -6.500000000000002665, 0.000000000000000000 ) ) ;
#7273 = CARTESIAN_POINT ( 'NONE',  ( 27.90000000000000213, 13.66939075806899240, -20.79999999999999361 ) ) ;
#7274 = EDGE_CURVE ( 'NONE', #42593, #37725, #35175, .T. ) ;
#7275 = VERTEX_POINT ( 'NONE', #25952 ) ;
#7276 = AXIS2_PLACEMENT_3D ( 'NONE', #4607, #30768, #21552 ) ;
#7277 = ORIENTED_EDGE ( 'NONE', *, *, #5785, .F. ) ;
#7278 = PLANE ( 'NONE',  #47044 ) ;
#7279 = DIRECTION ( 'NONE',  ( 1.836970198721029934E-16, -1.836970198721036344E-16, 1.000000000000000000 ) ) ;
#7280 = ORIENTED_EDGE ( 'NONE', *, *, #25528, .F. ) ;
#7281 = VECTOR ( 'NONE', #19343, 1000.000000000000000 ) ;
#7282 = ORIENTED_EDGE ( 'NONE', *, *, #63437, .T. ) ;
#7283 = ORIENTED_EDGE ( 'NONE', *, *, #16189, .F. ) ;
#7284 = LINE ( 'NONE', #34153, #9054 ) ;
#7285 = EDGE_CURVE ( 'NONE', #62767, #22867, #44217, .T. ) ;
#7287 = ORIENTED_EDGE ( 'NONE', *, *, #51239, .F. ) ;
#7286 = CYLINDRICAL_SURFACE ( 'NONE', #16402, 0.1749999999999998224 ) ;
#7288 = ADVANCED_FACE ( 'NONE', ( #46794, #36186 ), #20277, .T. ) ;
#7289 = DIRECTION ( 'NONE',  ( 0.000000000000000000, 0.000000000000000000, 1.000000000000000000 ) ) ;
#7290 = AXIS2_PLACEMENT_3D ( 'NONE', #69539, #59964, #15794 ) ;
#7291 = DIRECTION ( 'NONE',  ( 0.000000000000000000, 0.000000000000000000, 1.000000000000000000 ) ) ;
#7292 = ORIENTED_EDGE ( 'NONE', *, *, #4067, .T. ) ;
#7293 = ORIENTED_EDGE ( 'NONE', *, *, #34820, .F. ) ;
#7294 = VECTOR ( 'NONE', #50143, 1000.000000000000114 ) ;
#7295 = ADVANCED_FACE ( 'NONE', ( #47843 ), #63421, .T. ) ;
#7296 = CARTESIAN_POINT ( 'NONE',  ( 41.09999999999999432, -0.2000000000000000111, 0.000000000000000000 ) ) ;
#7297 = DIRECTION ( 'NONE',  ( -0.000000000000000000, -0.000000000000000000, 1.000000000000000000 ) ) ;
#7298 = CIRCLE ( 'NONE', #15212, 0.4999999999945534124 ) ;
#7299 = DIRECTION ( 'NONE',  ( -1.000000000000000000, 0.000000000000000000, 0.000000000000000000 ) ) ;
#7300 = MECHANICAL_DESIGN_GEOMETRIC_PRESENTATION_REPRESENTATION (  '', ( #35526 ), #52511 ) ;
#7301 = CYLINDRICAL_SURFACE ( 'NONE', #58399, 0.5999999999999998668 ) ;
#7302 = FACE_OUTER_BOUND ( 'NONE', #57459, .T. ) ;
#7304 = ORIENTED_EDGE ( 'NONE', *, *, #12600, .F. ) ;
#7303 = CARTESIAN_POINT ( 'NONE',  ( -17.51999999999999957, -15.50000000000000000, 26.00000000000000355 ) ) ;
#7305 = ORIENTED_EDGE ( 'NONE', *, *, #8843, .T. ) ;
#7306 = VECTOR ( 'NONE', #7494, 1000.000000000000000 ) ;
#7307 = FACE_OUTER_BOUND ( 'NONE', #28004, .T. ) ;
#7308 = DIRECTION ( 'NONE',  ( -0.7071067811865475727, -0.7071067811865475727, 0.000000000000000000 ) ) ;
#7309 = FACE_OUTER_BOUND ( 'NONE', #20979, .T. ) ;
#7310 = EDGE_CURVE ( 'NONE', #15923, #26457, #35843, .T. ) ;
#7311 = CARTESIAN_POINT ( 'NONE',  ( 11.50000000000000000, -11.50000000000000000, 15.00000000000000000 ) ) ;
#7312 = ORIENTED_EDGE ( 'NONE', *, *, #22615, .T. ) ;
#7313 = DIRECTION ( 'NONE',  ( 0.000000000000000000, 0.000000000000000000, -1.000000000000000000 ) ) ;
#7314 = FACE_OUTER_BOUND ( 'NONE', #29015, .T. ) ;
#7315 = DIRECTION ( 'NONE',  ( 0.000000000000000000, 1.000000000000000000, 0.000000000000000000 ) ) ;
#7316 = EDGE_CURVE ( 'NONE', #44206, #16386, #41502, .T. ) ;
#7317 = DIRECTION ( 'NONE',  ( 0.000000000000000000, 0.000000000000000000, 1.000000000000000000 ) ) ;
#7318 = CARTESIAN_POINT ( 'NONE',  ( -6.749999999999998224, -7.348062532927999158, -5.000000000000000000 ) ) ;
#7319 = LINE ( 'NONE', #38818, #5915 ) ;
#7320 = EDGE_CURVE ( 'NONE', #63385, #55203, #69423, .T. ) ;
#7321 = FACE_OUTER_BOUND ( 'NONE', #19121, .T. ) ;
#7322 = ORIENTED_EDGE ( 'NONE', *, *, #56224, .F. ) ;
#7323 = CARTESIAN_POINT ( 'NONE',  ( 176.4833316329832940, 9.000000000000001776, 280.6301873289890523 ) ) ;
#7324 = EDGE_CURVE ( 'NONE', #63611, #54102, #20621, .T. ) ;
#7325 = CARTESIAN_POINT ( 'NONE',  ( 25.50000000000000355, 0.000000000000000000, -20.24999999999999645 ) ) ;
#7326 = AXIS2_PLACEMENT_3D ( 'NONE', #42931, #26325, #26678 ) ;
#7327 = ORIENTED_EDGE ( 'NONE', *, *, #22311, .F. ) ;
#7328 = FACE_OUTER_BOUND ( 'NONE', #27836, .T. ) ;
#7329 = CARTESIAN_POINT ( 'NONE',  ( 39.00000000000000000, -14.48845687959340012, -21.00000000000000000 ) ) ;
#7330 = DIRECTION ( 'NONE',  ( 1.000000000000000000, 0.000000000000000000, 0.000000000000000000 ) ) ;
#7331 = DIRECTION ( 'NONE',  ( -0.000000000000000000, -0.000000000000000000, -1.000000000000000000 ) ) ;
#7332 = EDGE_CURVE ( 'NONE', #13327, #56322, #62707, .T. ) ;
#7333 = DIRECTION ( 'NONE',  ( 0.000000000000000000, 0.000000000000000000, -1.000000000000000000 ) ) ;
#7334 = EDGE_LOOP ( 'NONE', ( #47679, #1629, #62047, #11974, #13571, #39295, #43893, #49096 ) ) ;
#7335 = CARTESIAN_POINT ( 'NONE',  ( -7.605476262117258024, 9.722976262117178692, 54.00000000000000711 ) ) ;
#7336 = CIRCLE ( 'NONE', #24263, 2.204799999999997873 ) ;
#7337 = VECTOR ( 'NONE', #6265, 1000.000000000000000 ) ;
#7338 = EDGE_LOOP ( 'NONE', ( #7978, #33174, #7785, #29976 ) ) ;
#7339 = AXIS2_PLACEMENT_3D ( 'NONE', #34673, #62244, #30431 ) ;
#7340 = DIRECTION ( 'NONE',  ( 1.000000000000000000, 0.000000000000000000, 0.000000000000000000 ) ) ;
#7341 = ORIENTED_EDGE ( 'NONE', *, *, #15534, .F. ) ;
#7342 = CARTESIAN_POINT ( 'NONE',  ( 23.48000000000000043, -15.50000000000000000, 26.00000000000000355 ) ) ;
#7343 = EDGE_CURVE ( 'NONE', #42524, #32112, #23732, .T. ) ;
#7344 = VECTOR ( 'NONE', #51563, 1000.000000000000000 ) ;
#7345 = AXIS2_PLACEMENT_3D ( 'NONE', #53840, #36509, #52436 ) ;
#7346 = EDGE_CURVE ( 'NONE', #69782, #15754, #67576, .T. ) ;
#7347 = DIRECTION ( 'NONE',  ( 1.836970198721029934E-16, 1.836970198721010706E-16, -1.000000000000000000 ) ) ;
#7348 = VECTOR ( 'NONE', #49235, 1000.000000000000000 ) ;
#7349 = FACE_OUTER_BOUND ( 'NONE', #58254, .T. ) ;
#7350 = ORIENTED_EDGE ( 'NONE', *, *, #32909, .F. ) ;
#7351 = ORIENTED_EDGE ( 'NONE', *, *, #61263, .F. ) ;
#7352 = CARTESIAN_POINT ( 'NONE',  ( 30.00000000000000000, -9.487228132326899654, 12.50000000000000000 ) ) ;
#7353 = VERTEX_POINT ( 'NONE', #45999 ) ;
#7354 = EDGE_LOOP ( 'NONE', ( #11850, #66864, #39928, #526 ) ) ;
#7355 = DIRECTION ( 'NONE',  ( -1.000000000000000000, 1.047444401652940007E-14, -1.836970198721010706E-16 ) ) ;
#7356 = CARTESIAN_POINT ( 'NONE',  ( -7.955476262117259445, 9.547976262117179758, 54.00000000000000711 ) ) ;
#7357 = VECTOR ( 'NONE', #55354, 1000.000000000000000 ) ;
#7358 = DIRECTION ( 'NONE',  ( -1.000000000000000000, 0.000000000000000000, 0.000000000000000000 ) ) ;
#7359 = ORIENTED_EDGE ( 'NONE', *, *, #10273, .T. ) ;
#7360 = VECTOR ( 'NONE', #39923, 1000.000000000000000 ) ;
#7361 = LINE ( 'NONE', #2070, #54933 ) ;
#7363 = DIRECTION ( 'NONE',  ( 9.912705577010344285E-15, 1.000000000000000000, 0.000000000000000000 ) ) ;
#7362 = DIRECTION ( 'NONE',  ( -1.000000000000000000, 0.000000000000000000, 0.000000000000000000 ) ) ;
#7364 = ORIENTED_EDGE ( 'NONE', *, *, #56136, .T. ) ;
#7366 = VERTEX_POINT ( 'NONE', #61194 ) ;
#7365 = DIRECTION ( 'NONE',  ( -0.7071067811865500152, -0.7071067811865451302, 4.683861624749757595E-31 ) ) ;
#7367 = VERTEX_POINT ( 'NONE', #7465 ) ;
#7368 = DIRECTION ( 'NONE',  ( 0.000000000000000000, 0.000000000000000000, 1.000000000000000000 ) ) ;
#7369 = CARTESIAN_POINT ( 'NONE',  ( -11.00000000000000000, -14.04000000000000092, -14.80000000000000071 ) ) ;
#7370 = ADVANCED_FACE ( 'NONE', ( #41039 ), #3221, .T. ) ;
#7371 = ORIENTED_EDGE ( 'NONE', *, *, #1700, .T. ) ;
#7372 = EDGE_CURVE ( 'NONE', #2050, #19031, #66856, .T. ) ;
#7373 = CARTESIAN_POINT ( 'NONE',  ( -30.00000000000000000, -5.000000000000000000, -27.00000000000000000 ) ) ;
#7374 = CARTESIAN_POINT ( 'NONE',  ( 283.0000000000000568, -31.99999999999889866, 7.899999999997660893 ) ) ;
#7375 = ORIENTED_EDGE ( 'NONE', *, *, #21697, .T. ) ;
#7376 = ORIENTED_EDGE ( 'NONE', *, *, #47587, .T. ) ;
#7377 = CARTESIAN_POINT ( 'NONE',  ( 7.357023737882817827, -6.665817930929303969, 54.00000000000000711 ) ) ;
#7378 = CARTESIAN_POINT ( 'NONE',  ( -11.00000000000000000, -14.33999999999999986, -14.50000000000000000 ) ) ;
#7379 = CIRCLE ( 'NONE', #69488, 1.224999999999998757 ) ;
#7380 = ORIENTED_EDGE ( 'NONE', *, *, #66432, .T. ) ;
#7381 = LINE ( 'NONE', #14093, #20023 ) ;
#7382 = LINE ( 'NONE', #34609, #51535 ) ;
#7383 = VECTOR ( 'NONE', #1964, 1000.000000000000000 ) ;
#7384 = CARTESIAN_POINT ( 'NONE',  ( -15.50000000000129852, -17.50000000000000000, 22.50000000000000000 ) ) ;
#7385 = ORIENTED_EDGE ( 'NONE', *, *, #49909, .T. ) ;
#7386 = VECTOR ( 'NONE', #58555, 1000.000000000000000 ) ;
#7387 = VECTOR ( 'NONE', #58666, 1000.000000000000000 ) ;
#7388 = CIRCLE ( 'NONE', #46921, 1.399999999999999245 ) ;
#7389 = CARTESIAN_POINT ( 'NONE',  ( 25.57999999999999829, 0.000000000000000000, 5.250000000000000000 ) ) ;
#7390 = FACE_BOUND ( 'NONE', #47949, .T. ) ;
#7392 = ORIENTED_EDGE ( 'NONE', *, *, #739, .T. ) ;
#7391 = DIRECTION ( 'NONE',  ( 0.000000000000000000, 3.673940397442059868E-16, -1.000000000000000000 ) ) ;
#7394 = ORIENTED_EDGE ( 'NONE', *, *, #49660, .F. ) ;
#7393 = DIRECTION ( 'NONE',  ( 0.000000000000000000, -1.000000000000000000, -3.673940397442059868E-16 ) ) ;
#7395 = DIRECTION ( 'NONE',  ( -1.000000000000000000, 0.000000000000000000, 0.000000000000000000 ) ) ;
#7396 = CIRCLE ( 'NONE', #22281, 4.000000000000000888 ) ;
#7397 = AXIS2_PLACEMENT_3D ( 'NONE', #16516, #6242, #11531 ) ;
#7398 = VECTOR ( 'NONE', #3914, 1000.000000000000000 ) ;
#7399 = DIRECTION ( 'NONE',  ( -0.000000000000000000, 3.673940397442059868E-16, -1.000000000000000000 ) ) ;
#7400 = DIRECTION ( 'NONE',  ( 1.000000000000000000, -0.000000000000000000, 0.000000000000000000 ) ) ;
#7401 = CARTESIAN_POINT ( 'NONE',  ( -10.30047626211725742, 6.642976262117184838, 54.00000000000000711 ) ) ;
#7402 = AXIS2_PLACEMENT_3D ( 'NONE', #67744, #24262, #7289 ) ;
#7403 = LINE ( 'NONE', #28979, #25147 ) ;
#7404 = ORIENTED_EDGE ( 'NONE', *, *, #21881, .T. ) ;
#7405 = CARTESIAN_POINT ( 'NONE',  ( 7.250000000000005329, -7.249999999999998224, -7.500000000000000000 ) ) ;
#7406 = CYLINDRICAL_SURFACE ( 'NONE', #43995, 0.3499999999999302558 ) ;
#7407 = CARTESIAN_POINT ( 'NONE',  ( 4.720772854004765762, 6.344366288193357128, 26.00000000000000711 ) ) ;
#7408 = EDGE_CURVE ( 'NONE', #27819, #52415, #8508, .T. ) ;
#7410 = ORIENTED_EDGE ( 'NONE', *, *, #42673, .F. ) ;
#7409 = CARTESIAN_POINT ( 'NONE',  ( 25.50000000000000355, -5.200000000000001066, 22.50000000000000000 ) ) ;
#7411 = AXIS2_PLACEMENT_3D ( 'NONE', #44465, #34196, #39177 ) ;
#7412 = CARTESIAN_POINT ( 'NONE',  ( 8.093267424590464998, -8.711985858128699078, 54.00000000000000711 ) ) ;
#7413 = VECTOR ( 'NONE', #53365, 1000.000000000000000 ) ;
#7414 = PLANE ( 'NONE',  #56679 ) ;
#7415 = ADVANCED_FACE ( 'NONE', ( #12753 ), #61911, .T. ) ;
#7416 = ORIENTED_EDGE ( 'NONE', *, *, #1366, .F. ) ;
#7417 = DIRECTION ( 'NONE',  ( 0.000000000000000000, 0.000000000000000000, 1.000000000000000000 ) ) ;
#7418 = ADVANCED_FACE ( 'NONE', ( #39632 ), #55910, .F. ) ;
#7419 = CARTESIAN_POINT ( 'NONE',  ( 28.00000000000000000, -17.50000000000000000, 15.70499999999969809 ) ) ;
#7420 = EDGE_CURVE ( 'NONE', #22431, #11380, #8157, .T. ) ;
#7421 = ORIENTED_EDGE ( 'NONE', *, *, #45959, .F. ) ;
#7422 = DIRECTION ( 'NONE',  ( 8.994862468027880808E-15, 0.000000000000000000, 1.000000000000000000 ) ) ;
#7423 = CARTESIAN_POINT ( 'NONE',  ( 111.9257688011037146, 0.000000000000000000, 335.4830310981152479 ) ) ;
#7424 = FACE_BOUND ( 'NONE', #1427, .T. ) ;
#7425 = EDGE_CURVE ( 'NONE', #45642, #47767, #16886, .T. ) ;
#7426 = EDGE_CURVE ( 'NONE', #17601, #35918, #40693, .T. ) ;
#7427 = LINE ( 'NONE', #66480, #62058 ) ;
#7428 = DIRECTION ( 'NONE',  ( -1.794541526872559352E-16, -1.000000000000000000, 0.000000000000000000 ) ) ;
#7429 = ADVANCED_FACE ( 'NONE', ( #13819 ), #45285, .T. ) ;
#7430 = ORIENTED_EDGE ( 'NONE', *, *, #4273, .F. ) ;
#7431 = CARTESIAN_POINT ( 'NONE',  ( -8.693516549646711056, 11.11351654964659730, 194.9999952000000292 ) ) ;
#7432 = ORIENTED_EDGE ( 'NONE', *, *, #51264, .F. ) ;
#7433 = AXIS2_PLACEMENT_3D ( 'NONE', #44705, #21772, #54303 ) ;
#7434 = EDGE_LOOP ( 'NONE', ( #42087, #69786, #16376, #52830 ) ) ;
#7435 = LINE ( 'NONE', #67893, #16712 ) ;
#7436 = DIRECTION ( 'NONE',  ( -0.000000000000000000, -0.000000000000000000, -1.000000000000000000 ) ) ;
#7437 = CIRCLE ( 'NONE', #17642, 0.3500000000009988455 ) ;
#7439 = CARTESIAN_POINT ( 'NONE',  ( -5.655420232009359616, -8.406483450353428921, 455.0000000000000568 ) ) ;
#7438 = DIRECTION ( 'NONE',  ( 8.673617379884087537E-15, 1.000000000000000000, 0.000000000000000000 ) ) ;
#7440 = ORIENTED_EDGE ( 'NONE', *, *, #29181, .F. ) ;
#7441 = ORIENTED_EDGE ( 'NONE', *, *, #41456, .T. ) ;
#7442 = DIRECTION ( 'NONE',  ( -0.7071067811865588970, -0.7071067811865361374, -2.597868168706466792E-16 ) ) ;
#7443 = ORIENTED_EDGE ( 'NONE', *, *, #4756, .T. ) ;
#7444 = VECTOR ( 'NONE', #61557, 1000.000000000000000 ) ;
#7445 = VECTOR ( 'NONE', #67074, 1000.000000000000000 ) ;
#7446 = AXIS2_PLACEMENT_3D ( 'NONE', #42017, #68187, #41663 ) ;
#7447 = CARTESIAN_POINT ( 'NONE',  ( -10.50612335864048674, 6.822329165593977507, 26.00000000000000711 ) ) ;
#7448 = DIRECTION ( 'NONE',  ( 1.000000000000000000, -0.000000000000000000, 0.000000000000000000 ) ) ;
#7449 = PLANE ( 'NONE',  #21802 ) ;
#7450 = CARTESIAN_POINT ( 'NONE',  ( -15.50000000000000000, -5.000000000000000000, -18.50000000000000000 ) ) ;
#7451 = VECTOR ( 'NONE', #27419, 1000.000000000000000 ) ;
#7452 = VECTOR ( 'NONE', #8145, 1000.000000000000000 ) ;
#7453 = VECTOR ( 'NONE', #38525, 1000.000000000000000 ) ;
#7455 = CARTESIAN_POINT ( 'NONE',  ( 11.34648345035334671, 1.077516549646521327, 455.0000000000000568 ) ) ;
#7454 = FACE_OUTER_BOUND ( 'NONE', #57145, .T. ) ;
#7456 = ORIENTED_EDGE ( 'NONE', *, *, #20360, .F. ) ;
#7458 = ORIENTED_EDGE ( 'NONE', *, *, #64520, .F. ) ;
#7457 = FACE_OUTER_BOUND ( 'NONE', #34564, .T. ) ;
#7459 = ORIENTED_EDGE ( 'NONE', *, *, #51195, .T. ) ;
#7460 = VERTEX_POINT ( 'NONE', #18778 ) ;
#7461 = VECTOR ( 'NONE', #67324, 1000.000000000000000 ) ;
#7462 = DIRECTION ( 'NONE',  ( 0.000000000000000000, 0.000000000000000000, 1.000000000000000000 ) ) ;
#7463 = EDGE_CURVE ( 'NONE', #43093, #37823, #51299, .T. ) ;
#7464 = CIRCLE ( 'NONE', #36879, 0.3499999999998879008 ) ;
#7465 = CARTESIAN_POINT ( 'NONE',  ( 9.929523737882751888, 0.9414762621171479662, 54.00000000000000711 ) ) ;
#7466 = EDGE_LOOP ( 'NONE', ( #7380, #36277, #64703, #33388, #49833, #45777, #32691, #23631, #64782, #18489, #22258, #62954, #25773, #59063, #32589, #12575, #16345, #21027 ) ) ;
#7467 = VERTEX_POINT ( 'NONE', #56260 ) ;
#7468 = EDGE_CURVE ( 'NONE', #58210, #19830, #23623, .T. ) ;
#7469 = CARTESIAN_POINT ( 'NONE',  ( 75.42576880091934299, 0.000000000000000000, 334.4830310981790831 ) ) ;
#7470 = CARTESIAN_POINT ( 'NONE',  ( 7.899999999999999467, 14.08845687959340331, -21.00000000000000000 ) ) ;
#7471 = EDGE_CURVE ( 'NONE', #16868, #53126, #62253, .T. ) ;
#7472 = VERTEX_POINT ( 'NONE', #29729 ) ;
#7473 = ORIENTED_EDGE ( 'NONE', *, *, #16239, .F. ) ;
#7474 = PLANE ( 'NONE',  #53385 ) ;
#7475 = CYLINDRICAL_SURFACE ( 'NONE', #50354, 0.2000000000000005107 ) ;
#7476 = VERTEX_POINT ( 'NONE', #30087 ) ;
#7477 = CARTESIAN_POINT ( 'NONE',  ( 283.0000000000000568, -32.45000000000000995, 15.00000000000000000 ) ) ;
#7478 = AXIS2_PLACEMENT_3D ( 'NONE', #40012, #62288, #8540 ) ;
#7480 = VERTEX_POINT ( 'NONE', #46344 ) ;
#7479 = LINE ( 'NONE', #29743, #24966 ) ;
#7481 = ORIENTED_EDGE ( 'NONE', *, *, #53672, .T. ) ;
#7482 = CARTESIAN_POINT ( 'NONE',  ( -6.651770455163739548, 7.342976262117183239, 26.00000000000000711 ) ) ;
#7483 = CARTESIAN_POINT ( 'NONE',  ( 39.00000000000000000, 0.000000000000000000, 3.500000000000000000 ) ) ;
#7484 = AXIS2_PLACEMENT_3D ( 'NONE', #62673, #46068, #36153 ) ;
#7485 = DIRECTION ( 'NONE',  ( -1.000000000000000000, 0.000000000000000000, 0.000000000000000000 ) ) ;
#7486 = CARTESIAN_POINT ( 'NONE',  ( 9.690000000000001279, -8.750000000000000000, -7.000000000000000000 ) ) ;
#7487 = DIRECTION ( 'NONE',  ( -0.000000000000000000, -0.000000000000000000, -1.000000000000000000 ) ) ;
#7488 = DIRECTION ( 'NONE',  ( 1.000000000000000000, -0.000000000000000000, -0.000000000000000000 ) ) ;
#7489 = CIRCLE ( 'NONE', #35761, 0.3499999999998875677 ) ;
#7490 = AXIS2_PLACEMENT_3D ( 'NONE', #26908, #6374, #54813 ) ;
#7491 = FACE_OUTER_BOUND ( 'NONE', #57979, .T. ) ;
#7492 = ORIENTED_EDGE ( 'NONE', *, *, #33423, .T. ) ;
#7493 = LINE ( 'NONE', #66885, #8914 ) ;
#7495 = VERTEX_POINT ( 'NONE', #50950 ) ;
#7494 = DIRECTION ( 'NONE',  ( 0.000000000000000000, 1.000000000000000000, 0.000000000000000000 ) ) ;
#7496 = VECTOR ( 'NONE', #60819, 1000.000000000000114 ) ;
#7497 = CIRCLE ( 'NONE', #33453, 1.000000000000000000 ) ;
#7498 = EDGE_CURVE ( 'NONE', #67429, #29771, #40592, .T. ) ;
#7500 = DIRECTION ( 'NONE',  ( 1.000000000000000000, 0.000000000000000000, 0.000000000000000000 ) ) ;
#7499 = CIRCLE ( 'NONE', #10896, 1.000000000000001776 ) ;
#7501 = CARTESIAN_POINT ( 'NONE',  ( 3.430747519065288298, 7.839518282750187694, 195.0000000000000284 ) ) ;
#7502 = CARTESIAN_POINT ( 'NONE',  ( -7.250000000000000888, 7.250000000000001776, -11.50000000000000000 ) ) ;
#7503 = CARTESIAN_POINT ( 'NONE',  ( -4.031976262117257903, -3.157023737882818981, 54.00000000000000711 ) ) ;
#7504 = AXIS2_PLACEMENT_3D ( 'NONE', #30205, #24895, #68030 ) ;
#7505 = VECTOR ( 'NONE', #64275, 1000.000000000000000 ) ;
#7506 = CARTESIAN_POINT ( 'NONE',  ( -7.250000000000001776, -7.249999999999998224, -20.50000000000000000 ) ) ;
#7507 = ORIENTED_EDGE ( 'NONE', *, *, #27325, .T. ) ;
#7508 = ORIENTED_EDGE ( 'NONE', *, *, #50298, .F. ) ;
#7509 = AXIS2_PLACEMENT_3D ( 'NONE', #45562, #62895, #35651 ) ;
#7510 = CYLINDRICAL_SURFACE ( 'NONE', #68631, 1.929199999999997139 ) ;
#7511 = ADVANCED_FACE ( 'NONE', ( #24788 ), #58379, .T. ) ;
#7512 = EDGE_CURVE ( 'NONE', #51926, #16848, #19820, .T. ) ;
#7513 = FACE_OUTER_BOUND ( 'NONE', #21774, .T. ) ;
#7514 = VECTOR ( 'NONE', #51691, 1000.000000000000000 ) ;
#7515 = DIRECTION ( 'NONE',  ( -0.4999999999989417354, 0.000000000000000000, 0.8660254037850495523 ) ) ;
#7516 = EDGE_CURVE ( 'NONE', #50665, #59763, #58686, .T. ) ;
#7517 = ORIENTED_EDGE ( 'NONE', *, *, #54593, .T. ) ;
#7518 = CARTESIAN_POINT ( 'NONE',  ( 12.00000000000000000, -5.000000000000000000, -22.50000000000000000 ) ) ;
#7519 = ORIENTED_EDGE ( 'NONE', *, *, #22070, .F. ) ;
#7520 = ORIENTED_EDGE ( 'NONE', *, *, #45587, .T. ) ;
#7521 = DIRECTION ( 'NONE',  ( -7.304098846218132892E-15, -1.000000000000000000, 0.000000000000000000 ) ) ;
#7522 = FACE_BOUND ( 'NONE', #55162, .T. ) ;
#7523 = ORIENTED_EDGE ( 'NONE', *, *, #53100, .F. ) ;
#7524 = LINE ( 'NONE', #33367, #595 ) ;
#7525 = LINE ( 'NONE', #40032, #65907 ) ;
#7526 = CARTESIAN_POINT ( 'NONE',  ( -7.250000000000000888, 7.450000000000003730, -7.000000000000000000 ) ) ;
#7527 = ORIENTED_EDGE ( 'NONE', *, *, #4897, .T. ) ;
#7528 = ORIENTED_EDGE ( 'NONE', *, *, #18541, .F. ) ;
#7530 = ORIENTED_EDGE ( 'NONE', *, *, #8843, .F. ) ;
#7529 = FACE_OUTER_BOUND ( 'NONE', #8938, .T. ) ;
#7531 = ORIENTED_EDGE ( 'NONE', *, *, #57006, .F. ) ;
#7532 = DIRECTION ( 'NONE',  ( 0.000000000000000000, 0.000000000000000000, -1.000000000000000000 ) ) ;
#7533 = CARTESIAN_POINT ( 'NONE',  ( 55.00000000000000000, 6.429395695523604153E-16, -5.250000000000000000 ) ) ;
#7534 = LINE ( 'NONE', #39707, #26692 ) ;
#7535 = FACE_OUTER_BOUND ( 'NONE', #49072, .T. ) ;
#7536 = VECTOR ( 'NONE', #21278, 1000.000000000000000 ) ;
#7537 = DIRECTION ( 'NONE',  ( 0.000000000000000000, 1.000000000000000000, 0.000000000000000000 ) ) ;
#7538 = CARTESIAN_POINT ( 'NONE',  ( -10.08346604330787777, 9.293516549646602343, 195.0000000000000284 ) ) ;
#7539 = VECTOR ( 'NONE', #56107, 1000.000000000000000 ) ;
#7540 = ORIENTED_EDGE ( 'NONE', *, *, #26580, .F. ) ;
#7541 = ORIENTED_EDGE ( 'NONE', *, *, #739, .F. ) ;
#7542 = VECTOR ( 'NONE', #15538, 1000.000000000000000 ) ;
#7543 = VECTOR ( 'NONE', #32120, 1000.000000000000000 ) ;
#7544 = EDGE_LOOP ( 'NONE', ( #25228, #10074, #37006, #41603 ) ) ;
#7545 = LINE ( 'NONE', #23814, #55871 ) ;
#7546 = LINE ( 'NONE', #23470, #39938 ) ;
#7547 = LINE ( 'NONE', #12498, #52997 ) ;
#7548 = VECTOR ( 'NONE', #62384, 1000.000000000000000 ) ;
#7549 = AXIS2_PLACEMENT_3D ( 'NONE', #58637, #20795, #48374 ) ;
#7550 = LINE ( 'NONE', #51746, #20695 ) ;
#7551 = ORIENTED_EDGE ( 'NONE', *, *, #66819, .F. ) ;
#7552 = ORIENTED_EDGE ( 'NONE', *, *, #58852, .T. ) ;
#7553 = ORIENTED_EDGE ( 'NONE', *, *, #34487, .F. ) ;
#7554 = EDGE_CURVE ( 'NONE', #67025, #52765, #26192, .T. ) ;
#7555 = EDGE_CURVE ( 'NONE', #28, #48934, #10276, .T. ) ;
#7556 = ADVANCED_FACE ( 'NONE', ( #31504 ), #14524, .T. ) ;
#7557 = LINE ( 'NONE', #62338, #56524 ) ;
#7558 = VECTOR ( 'NONE', #20032, 1000.000000000000000 ) ;
#7559 = AXIS2_PLACEMENT_3D ( 'NONE', #42078, #59390, #63661 ) ;
#7560 = VERTEX_POINT ( 'NONE', #36086 ) ;
#7561 = ORIENTED_EDGE ( 'NONE', *, *, #52806, .T. ) ;
#7562 = EDGE_CURVE ( 'NONE', #57384, #12410, #31154, .T. ) ;
#7563 = ORIENTED_EDGE ( 'NONE', *, *, #10333, .T. ) ;
#7564 = VERTEX_POINT ( 'NONE', #32186 ) ;
#7565 = VECTOR ( 'NONE', #17914, 999.9999999999998863 ) ;
#7566 = DIRECTION ( 'NONE',  ( 1.000000000000000000, 0.000000000000000000, 0.000000000000000000 ) ) ;
#7568 = VERTEX_POINT ( 'NONE', #57658 ) ;
#7567 = CARTESIAN_POINT ( 'NONE',  ( -5.242976262117259978, 5.242976262117182706, 54.00000000000000711 ) ) ;
#7569 = CARTESIAN_POINT ( 'NONE',  ( 49.00000000000000000, -0.1999999999911430404, -8.864436962241481021E-12 ) ) ;
#7570 = AXIS2_PLACEMENT_3D ( 'NONE', #7052, #16655, #17677 ) ;
#7571 = LINE ( 'NONE', #12855, #62289 ) ;
#7572 = CARTESIAN_POINT ( 'NONE',  ( 11.48848345035341900, 10.19191654964656202, 455.0000000000000568 ) ) ;
#7574 = ORIENTED_EDGE ( 'NONE', *, *, #65412, .T. ) ;
#7573 = DIRECTION ( 'NONE',  ( 1.000000000000000000, -0.000000000000000000, -0.000000000000000000 ) ) ;
#7575 = ORIENTED_EDGE ( 'NONE', *, *, #2429, .F. ) ;
#7576 = CYLINDRICAL_SURFACE ( 'NONE', #39581, 1.000000000000000000 ) ;
#7577 = LINE ( 'NONE', #51771, #1804 ) ;
#7578 = DIRECTION ( 'NONE',  ( 1.836970198721029934E-16, 1.836970198721010706E-16, -1.000000000000000000 ) ) ;
#7579 = VERTEX_POINT ( 'NONE', #25848 ) ;
#7580 = CARTESIAN_POINT ( 'NONE',  ( 24.00000000000000000, -17.50000000000000000, -15.70500000000000007 ) ) ;
#7581 = CARTESIAN_POINT ( 'NONE',  ( 7.811466277050774565, 7.259684009079793832, 455.0000000000000568 ) ) ;
#7582 = CYLINDRICAL_SURFACE ( 'NONE', #2951, 0.4999999999979777288 ) ;
#7583 = MECHANICAL_DESIGN_GEOMETRIC_PRESENTATION_REPRESENTATION (  '', ( #44825 ), #16648 ) ;
#7584 = ORIENTED_EDGE ( 'NONE', *, *, #37136, .T. ) ;
#7585 = DIRECTION ( 'NONE',  ( 0.000000000000000000, 0.000000000000000000, -1.000000000000000000 ) ) ;
#7586 = DIRECTION ( 'NONE',  ( 0.000000000000000000, 0.000000000000000000, -1.000000000000000000 ) ) ;
#7587 = CARTESIAN_POINT ( 'NONE',  ( -1.466476262117230034, 9.390476262117152473, 54.00000000000000711 ) ) ;
#7588 = ORIENTED_EDGE ( 'NONE', *, *, #10733, .F. ) ;
#7589 = AXIS2_PLACEMENT_3D ( 'NONE', #37700, #933, #59263 ) ;
#7590 = AXIS2_PLACEMENT_3D ( 'NONE', #41591, #41231, #14379 ) ;
#7591 = SURFACE_STYLE_USAGE ( .BOTH. , #2637 ) ;
#7592 = CARTESIAN_POINT ( 'NONE',  ( -16.75000000000000000, -2.500000000000000000, -21.77831216351300014 ) ) ;
#7593 = CARTESIAN_POINT ( 'NONE',  ( 8.406483450353405829, 7.603567055985406498, 455.0000000000000568 ) ) ;
#7594 = EDGE_CURVE ( 'NONE', #67224, #55172, #5337, .T. ) ;
#7595 = AXIS2_PLACEMENT_3D ( 'NONE', #14661, #48242, #5467 ) ;
#7596 = VECTOR ( 'NONE', #56360, 1000.000000000000000 ) ;
#7597 = EDGE_CURVE ( 'NONE', #48280, #42663, #31588, .T. ) ;
#7598 = VERTEX_POINT ( 'NONE', #53768 ) ;
#7599 = LINE ( 'NONE', #12886, #2212 ) ;
#7600 = CARTESIAN_POINT ( 'NONE',  ( 5.793274621760843957, -4.155633711806670405, 54.00000000000000711 ) ) ;
#7601 = EDGE_CURVE ( 'NONE', #31478, #6447, #30790, .T. ) ;
#7602 = CARTESIAN_POINT ( 'NONE',  ( 30.00000000000000000, -12.00000000000000000, -12.20000000000000107 ) ) ;
#7603 = CARTESIAN_POINT ( 'NONE',  ( 10.47821035407136314, -25.18021646000299896, -17.31978353999700460 ) ) ;
#7604 = VECTOR ( 'NONE', #4525, 1000.000000000000000 ) ;
#7605 = DIRECTION ( 'NONE',  ( 0.000000000000000000, 0.000000000000000000, 1.000000000000000000 ) ) ;
#7606 = ORIENTED_EDGE ( 'NONE', *, *, #22919, .F. ) ;
#7607 = LINE ( 'NONE', #13261, #9542 ) ;
#7608 = CARTESIAN_POINT ( 'NONE',  ( 7.250000000000005329, -7.249999999999998224, -13.00000000000000178 ) ) ;
#7609 = ADVANCED_FACE ( 'NONE', ( #36808 ), #52364, .T. ) ;
#7610 = CARTESIAN_POINT ( 'NONE',  ( 11.50000000000000000, -12.00000000000000000, 11.03137303340310282 ) ) ;
#7611 = EDGE_CURVE ( 'NONE', #9455, #66129, #3923, .T. ) ;
#7612 = FILL_AREA_STYLE_COLOUR ( '', #47852 ) ;
#7613 = EDGE_CURVE ( 'NONE', #13015, #341, #27036, .T. ) ;
#7614 = DIRECTION ( 'NONE',  ( -1.000000000000000000, 0.000000000000000000, 0.000000000000000000 ) ) ;
#7615 = ORIENTED_EDGE ( 'NONE', *, *, #60050, .F. ) ;
#7617 = ORIENTED_EDGE ( 'NONE', *, *, #50070, .F. ) ;
#7616 = CARTESIAN_POINT ( 'NONE',  ( 283.0000000000000568, -39.80000000000000426, 12.69999999999999929 ) ) ;
#7618 = EDGE_CURVE ( 'NONE', #57546, #64704, #14882, .T. ) ;
#7619 = CYLINDRICAL_SURFACE ( 'NONE', #1102, 0.3999999999993835154 ) ;
#7620 = DIRECTION ( 'NONE',  ( 0.000000000000000000, 0.000000000000000000, -1.000000000000000000 ) ) ;
#7621 = ORIENTED_EDGE ( 'NONE', *, *, #11353, .T. ) ;
#7622 = FACE_OUTER_BOUND ( 'NONE', #13034, .T. ) ;
#7623 = VERTEX_POINT ( 'NONE', #4628 ) ;
#7624 = DIRECTION ( 'NONE',  ( -3.491481338843133355E-15, -1.000000000000000000, 0.000000000000000000 ) ) ;
#7625 = ORIENTED_EDGE ( 'NONE', *, *, #67010, .F. ) ;
#7626 = VERTEX_POINT ( 'NONE', #37155 ) ;
#7627 = CARTESIAN_POINT ( 'NONE',  ( -7.450000000000001954, 0.000000000000000000, -18.50000000000000000 ) ) ;
#7628 = CARTESIAN_POINT ( 'NONE',  ( 39.90000000000000568, -0.000000000000000000, 20.80000000000000426 ) ) ;
#7629 = DIRECTION ( 'NONE',  ( 0.000000000000000000, 1.000000000000000000, -0.000000000000000000 ) ) ;
#7630 = DIRECTION ( 'NONE',  ( 0.000000000000000000, 0.000000000000000000, 1.000000000000000000 ) ) ;
#7631 = VECTOR ( 'NONE', #18457, 1000.000000000000000 ) ;
#7632 = ORIENTED_EDGE ( 'NONE', *, *, #56553, .F. ) ;
#7633 = VERTEX_POINT ( 'NONE', #20180 ) ;
#7634 = CYLINDRICAL_SURFACE ( 'NONE', #22214, 24.99999999998784972 ) ;
#7635 = DIRECTION ( 'NONE',  ( 0.000000000000000000, 1.000000000000000000, 0.000000000000000000 ) ) ;
#7636 = ORIENTED_EDGE ( 'NONE', *, *, #25077, .T. ) ;
#7637 = ORIENTED_EDGE ( 'NONE', *, *, #58322, .F. ) ;
#7638 = VERTEX_POINT ( 'NONE', #42790 ) ;
#7639 = VECTOR ( 'NONE', #49755, 1000.000000000000000 ) ;
#7640 = DIRECTION ( 'NONE',  ( 0.000000000000000000, -1.000000000000000000, 0.000000000000000000 ) ) ;
#7642 = ORIENTED_EDGE ( 'NONE', *, *, #54549, .T. ) ;
#7641 = DIRECTION ( 'NONE',  ( -1.000000000000000000, 0.000000000000000000, 0.000000000000000000 ) ) ;
#7643 = AXIS2_PLACEMENT_3D ( 'NONE', #58823, #47845, #3674 ) ;
#7644 = DIRECTION ( 'NONE',  ( 1.000000000000000000, -5.981805089575194965E-17, 0.000000000000000000 ) ) ;
#7645 = CARTESIAN_POINT ( 'NONE',  ( 49.00000000000000000, -14.06939075806900163, -20.80000000000000426 ) ) ;
#7646 = VECTOR ( 'NONE', #68990, 1000.000000000000000 ) ;
#7647 = ORIENTED_EDGE ( 'NONE', *, *, #3063, .T. ) ;
#7648 = VERTEX_POINT ( 'NONE', #47745 ) ;
#7649 = VECTOR ( 'NONE', #35411, 1000.000000000000114 ) ;
#7650 = EDGE_CURVE ( 'NONE', #41013, #44516, #58719, .T. ) ;
#7651 = CARTESIAN_POINT ( 'NONE',  ( -7.798499376344067535, 7.259684009079840017, 455.0000000000000568 ) ) ;
#7652 = CARTESIAN_POINT ( 'NONE',  ( 49.00000000000000000, -0.1999999999911430404, -8.864436962241481021E-12 ) ) ;
#7653 = EDGE_CURVE ( 'NONE', #68084, #44582, #4971, .T. ) ;
#7654 = DIRECTION ( 'NONE',  ( 8.673617379884051249E-15, 1.000000000000000000, 0.000000000000000000 ) ) ;
#7655 = AXIS2_PLACEMENT_3D ( 'NONE', #35496, #19951, #25624 ) ;
#7656 = FACE_OUTER_BOUND ( 'NONE', #43311, .T. ) ;
#7657 = CARTESIAN_POINT ( 'NONE',  ( -7.250000000000000888, 7.250000000000001776, -26.00000000000001066 ) ) ;
#7658 = EDGE_CURVE ( 'NONE', #7150, #46624, #15927, .T. ) ;
#7660 = VERTEX_POINT ( 'NONE', #61026 ) ;
#7659 = CARTESIAN_POINT ( 'NONE',  ( 6.364920264886851697, 3.663616288756991413, 54.00000000000000711 ) ) ;
#7661 = ORIENTED_EDGE ( 'NONE', *, *, #29226, .F. ) ;
#7662 = PLANE ( 'NONE',  #42257 ) ;
#7663 = LINE ( 'NONE', #44792, #68016 ) ;
#7664 = DIRECTION ( 'NONE',  ( -0.000000000000000000, -0.000000000000000000, -1.000000000000000000 ) ) ;
#7665 = ADVANCED_FACE ( 'NONE', ( #29201 ), #50082, .F. ) ;
#7666 = CARTESIAN_POINT ( 'NONE',  ( -15.50000000000000000, -1.037157890325000054, -22.50000000000000000 ) ) ;
#7667 = ORIENTED_EDGE ( 'NONE', *, *, #14521, .T. ) ;
#7668 = CARTESIAN_POINT ( 'NONE',  ( -6.500000000000002665, -6.500000000000002665, 0.000000000000000000 ) ) ;
#7669 = FACE_OUTER_BOUND ( 'NONE', #33048, .T. ) ;
#7670 = DIRECTION ( 'NONE',  ( 0.000000000000000000, 0.000000000000000000, 1.000000000000000000 ) ) ;
#7671 = CARTESIAN_POINT ( 'NONE',  ( 151.5599459900709860, -10.00000000000000178, 324.6739988703752715 ) ) ;
#7672 = EDGE_CURVE ( 'NONE', #69051, #28084, #24800, .T. ) ;
#7673 = VECTOR ( 'NONE', #32592, 1000.000000000000000 ) ;
#7674 = LINE ( 'NONE', #35230, #31519 ) ;
#7675 = DIRECTION ( 'NONE',  ( -1.836970198721029934E-16, -1.836970198721010706E-16, 1.000000000000000000 ) ) ;
#7676 = DIRECTION ( 'NONE',  ( 0.000000000000000000, 0.1500000000000006328, -0.9886859966642592701 ) ) ;
#7677 = ORIENTED_EDGE ( 'NONE', *, *, #50787, .T. ) ;
#7678 = DIRECTION ( 'NONE',  ( -1.836970198721029934E-16, 1.836970198721036344E-16, -1.000000000000000000 ) ) ;
#7679 = DIRECTION ( 'NONE',  ( -1.836970198721029934E-16, 1.836970198721036344E-16, -1.000000000000000000 ) ) ;
#7680 = ORIENTED_EDGE ( 'NONE', *, *, #16742, .F. ) ;
#7681 = DIRECTION ( 'NONE',  ( -0.7071067811865460184, 0.000000000000000000, -0.7071067811865489050 ) ) ;
#7682 = CARTESIAN_POINT ( 'NONE',  ( 29.50000000000000355, -11.70000000000000284, -11.00000000000000000 ) ) ;
#7683 = CARTESIAN_POINT ( 'NONE',  ( 8.000000000000000000, 7.281754163448145079, 0.000000000000000000 ) ) ;
#7684 = LINE ( 'NONE', #8746, #13876 ) ;
#7685 = EDGE_CURVE ( 'NONE', #46756, #45109, #64709, .T. ) ;
#7686 = DIRECTION ( 'NONE',  ( -1.000000000000000000, 1.047444401652940007E-14, -1.836970198721010706E-16 ) ) ;
#7687 = ORIENTED_EDGE ( 'NONE', *, *, #9247, .F. ) ;
#7688 = EDGE_CURVE ( 'NONE', #45034, #16384, #2342, .T. ) ;
#7689 = AXIS2_PLACEMENT_3D ( 'NONE', #29255, #23609, #56153 ) ;
#7690 = CARTESIAN_POINT ( 'NONE',  ( 2.369523737882786918, -9.562023737882798358, 54.00000000000000711 ) ) ;
#7691 = EDGE_LOOP ( 'NONE', ( #1833, #31271, #4728, #19873, #32014, #32358, #69329, #18586, #42810, #2019, #5110, #8489, #66936, #45028, #41578, #49822, #68741, #32976, #60976, #43725, #1215, #63254, #21573, #46297, #55528, #22805, #33279, #66851, #47135, #25446, #68879, #26343, #45155, #31721, #11547 ) ) ;
#7692 = FACE_OUTER_BOUND ( 'NONE', #63609, .T. ) ;
#7693 = ORIENTED_EDGE ( 'NONE', *, *, #66040, .T. ) ;
#7694 = CARTESIAN_POINT ( 'NONE',  ( 7.250000000000005329, -7.249999999999998224, -7.500000000000000000 ) ) ;
#7695 = VECTOR ( 'NONE', #61475, 1000.000000000000000 ) ;
#7696 = ADVANCED_FACE ( 'NONE', ( #59408 ), #54111, .F. ) ;
#7697 = SURFACE_SIDE_STYLE ('',( #2057 ) ) ;
#7698 = CARTESIAN_POINT ( 'NONE',  ( -6.835476262117334834, -10.50702373788278798, 54.00000000000000711 ) ) ;
#7699 = ORIENTED_EDGE ( 'NONE', *, *, #17158, .F. ) ;
#7700 = ORIENTED_EDGE ( 'NONE', *, *, #37701, .F. ) ;
#7701 = DIRECTION ( 'NONE',  ( 0.000000000000000000, 1.000000000000000000, 8.604228440837611257E-13 ) ) ;
#7702 = ORIENTED_EDGE ( 'NONE', *, *, #67099, .F. ) ;
#7703 = ORIENTED_EDGE ( 'NONE', *, *, #52674, .T. ) ;
#7704 = VECTOR ( 'NONE', #50119, 1000.000000000000000 ) ;
#7705 = PRODUCT_DEFINITION_CONTEXT ( 'detailed design', #35891, 'design' ) ;
#7706 = LINE ( 'NONE', #66759, #16895 ) ;
#7707 = DIRECTION ( 'NONE',  ( 1.000000000000000000, -1.047444401652940007E-14, 1.836970198721010706E-16 ) ) ;
#7708 = DIRECTION ( 'NONE',  ( -0.000000000000000000, 1.000000000000000000, -0.000000000000000000 ) ) ;
#7709 = ORIENTED_EDGE ( 'NONE', *, *, #15273, .T. ) ;
#7710 = DIRECTION ( 'NONE',  ( 0.000000000000000000, -0.000000000000000000, 1.000000000000000000 ) ) ;
#7712 = CYLINDRICAL_SURFACE ( 'NONE', #34440, 0.2000000000000005107 ) ;
#7711 = FACE_OUTER_BOUND ( 'NONE', #51297, .T. ) ;
#7713 = VERTEX_POINT ( 'NONE', #17558 ) ;
#7715 = ORIENTED_EDGE ( 'NONE', *, *, #15311, .F. ) ;
#7714 = LINE ( 'NONE', #66071, #54562 ) ;
#7716 = ORIENTED_EDGE ( 'NONE', *, *, #17896, .F. ) ;
#7717 = EDGE_CURVE ( 'NONE', #29989, #56381, #7284, .T. ) ;
#7718 = DIRECTION ( 'NONE',  ( 1.000000000000000000, 0.000000000000000000, 0.000000000000000000 ) ) ;
#7719 = FACE_OUTER_BOUND ( 'NONE', #55457, .T. ) ;
#7720 = ORIENTED_EDGE ( 'NONE', *, *, #68785, .F. ) ;
#7721 = EDGE_CURVE ( 'NONE', #33806, #11215, #13297, .T. ) ;
#7722 = CARTESIAN_POINT ( 'NONE',  ( 9.737023737882816832, -6.832023737882823688, 54.00000000000000711 ) ) ;
#7723 = DIRECTION ( 'NONE',  ( 1.836970198721029934E-16, -1.836970198721036344E-16, 1.000000000000000000 ) ) ;
#7724 = ORIENTED_EDGE ( 'NONE', *, *, #7260, .T. ) ;
#7725 = VERTEX_POINT ( 'NONE', #48451 ) ;
#7726 = EDGE_CURVE ( 'NONE', #69042, #55314, #1139, .T. ) ;
#7727 = CARTESIAN_POINT ( 'NONE',  ( 5.257023737882801306, 5.242976262117200470, 54.00000000000000711 ) ) ;
#7728 = EDGE_CURVE ( 'NONE', #37811, #65011, #47411, .T. ) ;
#7729 = LINE ( 'NONE', #66778, #35717 ) ;
#7730 = ORIENTED_EDGE ( 'NONE', *, *, #28665, .F. ) ;
#7731 = VECTOR ( 'NONE', #35186, 1000.000000000000000 ) ;
#7732 = DIRECTION ( 'NONE',  ( 0.000000000000000000, -0.9938079899998859545, 0.1111111111112941946 ) ) ;
#7733 = FACE_OUTER_BOUND ( 'NONE', #36382, .T. ) ;
#7734 = EDGE_CURVE ( 'NONE', #29731, #54503, #64389, .T. ) ;
#7735 = DIRECTION ( 'NONE',  ( -0.000000000000000000, 1.000000000000000000, -0.000000000000000000 ) ) ;
#7736 = ORIENTED_EDGE ( 'NONE', *, *, #59190, .F. ) ;
#7737 = VECTOR ( 'NONE', #24851, 1000.000000000000000 ) ;
#7738 = LINE ( 'NONE', #61474, #47085 ) ;
#7739 = LINE ( 'NONE', #35659, #971 ) ;
#7740 = EDGE_CURVE ( 'NONE', #50075, #9129, #45464, .T. ) ;
#7742 = ORIENTED_EDGE ( 'NONE', *, *, #41609, .F. ) ;
#7741 = DIRECTION ( 'NONE',  ( 1.000000000000000000, -0.000000000000000000, 0.000000000000000000 ) ) ;
#7744 = VERTEX_POINT ( 'NONE', #5672 ) ;
#7743 = LINE ( 'NONE', #62187, #42248 ) ;
#7745 = EDGE_CURVE ( 'NONE', #30522, #57627, #48584, .T. ) ;
#7746 = CARTESIAN_POINT ( 'NONE',  ( 25.50000000000000355, -15.50000000000000000, -22.50000000000000000 ) ) ;
#7747 = VECTOR ( 'NONE', #29844, 1000.000000000000000 ) ;
#7748 = DIRECTION ( 'NONE',  ( 2.478176394252608948E-15, 1.000000000000000000, 0.000000000000000000 ) ) ;
#7749 = DIRECTION ( 'NONE',  ( 0.000000000000000000, 1.000000000000000000, 0.000000000000000000 ) ) ;
#7750 = ADVANCED_FACE ( 'NONE', ( #28171 ), #67037, .F. ) ;
#7751 = EDGE_CURVE ( 'NONE', #19830, #52952, #12933, .T. ) ;
#7752 = CARTESIAN_POINT ( 'NONE',  ( 7.450000000000004619, -1.336933437520057563E-15, -11.50000000000000000 ) ) ;
#7753 = CARTESIAN_POINT ( 'NONE',  ( 0.000000000000000000, 8.250000000000001776, -17.50000000000000000 ) ) ;
#7754 = ORIENTED_EDGE ( 'NONE', *, *, #32880, .T. ) ;
#7755 = DIRECTION ( 'NONE',  ( 0.000000000000000000, 1.000000000000000000, 0.000000000000000000 ) ) ;
#7756 = DIRECTION ( 'NONE',  ( -0.000000000000000000, -0.000000000000000000, -1.000000000000000000 ) ) ;
#7757 = ADVANCED_FACE ( 'NONE', ( #32548 ), #33814, .F. ) ;
#7758 = SURFACE_STYLE_USAGE ( .BOTH. , #56211 ) ;
#7760 = AXIS2_PLACEMENT_3D ( 'NONE', #10381, #53879, #42199 ) ;
#7759 = VECTOR ( 'NONE', #5186, 1000.000000000000000 ) ;
#7762 = ORIENTED_EDGE ( 'NONE', *, *, #69483, .F. ) ;
#7761 = DIRECTION ( 'NONE',  ( -1.000000000000000000, 0.000000000000000000, 0.000000000000000000 ) ) ;
#7763 = CARTESIAN_POINT ( 'NONE',  ( 78.77321854994620765, 47.95351654967443977, 43.00000000000000000 ) ) ;
#7764 = CARTESIAN_POINT ( 'NONE',  ( 2.544523737882785852, -9.737023737882799068, 54.00000000000000711 ) ) ;
#7765 = ORIENTED_EDGE ( 'NONE', *, *, #30884, .F. ) ;
#7766 = LINE ( 'NONE', #50900, #21846 ) ;
#7767 = PLANE ( 'NONE',  #4645 ) ;
#7768 = ORIENTED_EDGE ( 'NONE', *, *, #7516, .T. ) ;
#7769 = CARTESIAN_POINT ( 'NONE',  ( 8.900000000000005684, -0.2000000000000000111, 0.000000000000000000 ) ) ;
#7770 = FACE_OUTER_BOUND ( 'NONE', #66607, .T. ) ;
#7771 = EDGE_CURVE ( 'NONE', #1721, #19808, #40163, .T. ) ;
#7772 = DIRECTION ( 'NONE',  ( 0.000000000000000000, -1.000000000000000000, 0.000000000000000000 ) ) ;
#7773 = EDGE_CURVE ( 'NONE', #8637, #36514, #7979, .T. ) ;
#7774 = DIRECTION ( 'NONE',  ( 0.000000000000000000, 0.000000000000000000, -1.000000000000000000 ) ) ;
#7775 = VERTEX_POINT ( 'NONE', #13995 ) ;
#7776 = DIRECTION ( 'NONE',  ( -1.000000000000000000, 0.000000000000000000, 0.000000000000000000 ) ) ;
#7777 = ORIENTED_EDGE ( 'NONE', *, *, #39615, .T. ) ;
#7778 = ORIENTED_EDGE ( 'NONE', *, *, #41448, .T. ) ;
#7779 = CARTESIAN_POINT ( 'NONE',  ( -11.00000000000000000, -12.00000000000000000, -11.03137303340310282 ) ) ;
#7780 = AXIS2_PLACEMENT_3D ( 'NONE', #2331, #63485, #35540 ) ;
#7781 = DIRECTION ( 'NONE',  ( 0.000000000000000000, -1.000000000000000000, 0.000000000000000000 ) ) ;
#7783 = DIRECTION ( 'NONE',  ( 0.000000000000000000, 0.000000000000000000, 1.000000000000000000 ) ) ;
#7782 = DIRECTION ( 'NONE',  ( 0.000000000000000000, -3.673940397442059868E-16, 1.000000000000000000 ) ) ;
#7784 = ORIENTED_EDGE ( 'NONE', *, *, #61279, .T. ) ;
#7785 = ORIENTED_EDGE ( 'NONE', *, *, #17247, .T. ) ;
#7786 = DIRECTION ( 'NONE',  ( 9.912705577010435793E-15, 1.000000000000000000, 0.000000000000000000 ) ) ;
#7787 = ORIENTED_EDGE ( 'NONE', *, *, #18520, .F. ) ;
#7788 = LINE ( 'NONE', #62236, #20275 ) ;
#7789 = DIRECTION ( 'NONE',  ( 1.952517519553884087E-14, 1.000000000000000000, 1.836970198721046451E-16 ) ) ;
#7790 = DIRECTION ( 'NONE',  ( 3.491481338843133355E-15, 1.000000000000000000, 1.836970198721029934E-16 ) ) ;
#7791 = DIRECTION ( 'NONE',  ( 1.000000000000000000, 0.000000000000000000, 0.000000000000000000 ) ) ;
#7792 = EDGE_LOOP ( 'NONE', ( #24601, #43342, #35930, #55525 ) ) ;
#7793 = AXIS2_PLACEMENT_3D ( 'NONE', #13500, #19852, #62634 ) ;
#7794 = DIRECTION ( 'NONE',  ( -1.000000000000000000, 0.000000000000000000, -0.000000000000000000 ) ) ;
#7796 = LINE ( 'NONE', #25479, #50416 ) ;
#7795 = DIRECTION ( 'NONE',  ( 0.000000000000000000, -1.000000000000000000, 0.000000000000000000 ) ) ;
#7797 = ORIENTED_EDGE ( 'NONE', *, *, #38967, .T. ) ;
#7799 = ORIENTED_EDGE ( 'NONE', *, *, #22569, .T. ) ;
#7798 = DIRECTION ( 'NONE',  ( 1.000000000000000000, 0.000000000000000000, 0.000000000000000000 ) ) ;
#7800 = VERTEX_POINT ( 'NONE', #35551 ) ;
#7801 = ORIENTED_EDGE ( 'NONE', *, *, #3359, .T. ) ;
#7802 = VECTOR ( 'NONE', #30288, 1000.000000000000000 ) ;
#7803 = CARTESIAN_POINT ( 'NONE',  ( 283.0000000000000568, -20.50000000000000000, -13.00000000000000178 ) ) ;
#7805 = VECTOR ( 'NONE', #18607, 1000.000000000000000 ) ;
#7804 = AXIS2_PLACEMENT_3D ( 'NONE', #33359, #22412, #48239 ) ;
#7806 = EDGE_CURVE ( 'NONE', #6525, #31517, #36616, .T. ) ;
#7807 = DIRECTION ( 'NONE',  ( 0.000000000000000000, 0.000000000000000000, -1.000000000000000000 ) ) ;
#7808 = ORIENTED_EDGE ( 'NONE', *, *, #64737, .T. ) ;
#7809 = ORIENTED_EDGE ( 'NONE', *, *, #4058, .T. ) ;
#7810 = EDGE_CURVE ( 'NONE', #1819, #66376, #57831, .T. ) ;
#7811 = VECTOR ( 'NONE', #39919, 1000.000000000000000 ) ;
#7812 = DIRECTION ( 'NONE',  ( 0.8660254037844375974, -0.5000000000000019984, 0.000000000000000000 ) ) ;
#7813 = EDGE_CURVE ( 'NONE', #23746, #9687, #46866, .T. ) ;
#7814 = LINE ( 'NONE', #50957, #33412 ) ;
#7815 = VERTEX_POINT ( 'NONE', #8332 ) ;
#7816 = ORIENTED_EDGE ( 'NONE', *, *, #64884, .T. ) ;
#7817 = CARTESIAN_POINT ( 'NONE',  ( 39.00000000000000000, 21.00000000000000000, -16.96999999999999886 ) ) ;
#7818 = EDGE_CURVE ( 'NONE', #36255, #4470, #51485, .T. ) ;
#7819 = CYLINDRICAL_SURFACE ( 'NONE', #48596, 0.1749999999999998224 ) ;
#7820 = VERTEX_POINT ( 'NONE', #62420 ) ;
#7821 = CARTESIAN_POINT ( 'NONE',  ( 7.250000000000005329, -8.249999999999998224, -16.50000000000000000 ) ) ;
#7822 = DIRECTION ( 'NONE',  ( 0.000000000000000000, 0.000000000000000000, 1.000000000000000000 ) ) ;
#7824 = ORIENTED_EDGE ( 'NONE', *, *, #43135, .F. ) ;
#7823 = DIRECTION ( 'NONE',  ( 0.000000000000000000, 0.000000000000000000, 1.000000000000000000 ) ) ;
#7825 = VERTEX_POINT ( 'NONE', #19643 ) ;
#7826 = CARTESIAN_POINT ( 'NONE',  ( -7.250000000000000888, 8.250000000000001776, -26.00000000000001066 ) ) ;
#7827 = LINE ( 'NONE', #55934, #53817 ) ;
#7828 = DIRECTION ( 'NONE',  ( -1.000000000000000000, 0.000000000000000000, 0.000000000000000000 ) ) ;
#7829 = CARTESIAN_POINT ( 'NONE',  ( 275.0000000000000000, -0.5000000000000000000, 26.50000000000000000 ) ) ;
#7830 = DIRECTION ( 'NONE',  ( -1.794541526872559352E-16, -1.000000000000000000, 0.000000000000000000 ) ) ;
#7831 = DIRECTION ( 'NONE',  ( -1.000000000000000000, 0.000000000000000000, 0.000000000000000000 ) ) ;
#7832 = DIRECTION ( 'NONE',  ( -1.000000000000000000, 0.000000000000000000, 0.000000000000000000 ) ) ;
#7833 = VERTEX_POINT ( 'NONE', #19299 ) ;
#7834 = DIRECTION ( 'NONE',  ( -1.000000000000000000, 1.047444401652940007E-14, 0.000000000000000000 ) ) ;
#7835 = AXIS2_PLACEMENT_3D ( 'NONE', #8752, #55541, #60488 ) ;
#7836 = VECTOR ( 'NONE', #34217, 1000.000000000000000 ) ;
#7838 = ORIENTED_EDGE ( 'NONE', *, *, #53709, .F. ) ;
#7837 = CARTESIAN_POINT ( 'NONE',  ( 9.955011587777223170, 2.752095193409229257, 455.0000000000000568 ) ) ;
#7839 = CARTESIAN_POINT ( 'NONE',  ( 8.250000000000005329, 7.250000000000000888, -26.00000000000001066 ) ) ;
#7840 = CARTESIAN_POINT ( 'NONE',  ( 7.250000000000005329, 7.250000000000000888, -24.00000000000000000 ) ) ;
#7841 = CARTESIAN_POINT ( 'NONE',  ( -7.813516549646839948, -12.00648345035340903, 455.0000000000000568 ) ) ;
#7842 = CARTESIAN_POINT ( 'NONE',  ( -30.00000000000000000, -15.97213595500069871, -14.50000000000000000 ) ) ;
#7843 = AXIS2_PLACEMENT_3D ( 'NONE', #66117, #39580, #7058 ) ;
#7844 = DIRECTION ( 'NONE',  ( 0.000000000000000000, 1.000000000000000000, 0.000000000000000000 ) ) ;
#7845 = VERTEX_POINT ( 'NONE', #20356 ) ;
#7846 = LINE ( 'NONE', #62645, #52811 ) ;
#7847 = ORIENTED_EDGE ( 'NONE', *, *, #4942, .F. ) ;
#7848 = VECTOR ( 'NONE', #25266, 1000.000000000000114 ) ;
#7849 = DIRECTION ( 'NONE',  ( -1.000000000000000000, 0.000000000000000000, 0.000000000000000000 ) ) ;
#7850 = EDGE_CURVE ( 'NONE', #15565, #59231, #39520, .T. ) ;
#7851 = DIRECTION ( 'NONE',  ( 1.000000000000000000, 0.000000000000000000, 0.000000000000000000 ) ) ;
#7852 = AXIS2_PLACEMENT_3D ( 'NONE', #7938, #66646, #50035 ) ;
#7853 = EDGE_CURVE ( 'NONE', #58981, #31830, #13644, .T. ) ;
#7854 = DIRECTION ( 'NONE',  ( 0.000000000000000000, -1.000000000000000000, 0.000000000000000000 ) ) ;
#7855 = EDGE_LOOP ( 'NONE', ( #61994, #9078, #29327, #28319 ) ) ;
#7856 = DIRECTION ( 'NONE',  ( 1.000000000000000000, -7.304098846218132892E-15, -2.683482381803073952E-30 ) ) ;
#7857 = ORIENTED_EDGE ( 'NONE', *, *, #45372, .T. ) ;
#7858 = EDGE_CURVE ( 'NONE', #4281, #65753, #62080, .T. ) ;
#7859 = ORIENTED_EDGE ( 'NONE', *, *, #50551, .T. ) ;
#7860 = LINE ( 'NONE', #29783, #50560 ) ;
#7861 = VECTOR ( 'NONE', #58269, 1000.000000000000000 ) ;
#7862 = CARTESIAN_POINT ( 'NONE',  ( 7.250000000000005329, 7.250000000000000888, -26.00000000000001066 ) ) ;
#7863 = VERTEX_POINT ( 'NONE', #45825 ) ;
#7864 = CARTESIAN_POINT ( 'NONE',  ( 23.48000000000000043, -15.50000000000000000, -26.00000000000000355 ) ) ;
#7865 = FACE_OUTER_BOUND ( 'NONE', #40559, .T. ) ;
#7866 = LINE ( 'NONE', #18473, #21609 ) ;
#7867 = ORIENTED_EDGE ( 'NONE', *, *, #63414, .T. ) ;
#7868 = ORIENTED_EDGE ( 'NONE', *, *, #20536, .F. ) ;
#7870 = ORIENTED_EDGE ( 'NONE', *, *, #490, .F. ) ;
#7869 = DIRECTION ( 'NONE',  ( -0.000000000000000000, 3.673940397442059868E-16, -1.000000000000000000 ) ) ;
#7871 = ORIENTED_EDGE ( 'NONE', *, *, #10042, .F. ) ;
#7872 = CARTESIAN_POINT ( 'NONE',  ( 7.250000000000005329, 7.250000000000000888, -15.00000000000000000 ) ) ;
#7873 = LINE ( 'NONE', #29799, #3363 ) ;
#7874 = DIRECTION ( 'NONE',  ( 1.000000000000000000, 0.000000000000000000, 0.000000000000000000 ) ) ;
#7875 = VECTOR ( 'NONE', #50436, 1000.000000000000114 ) ;
#7876 = CARTESIAN_POINT ( 'NONE',  ( -7.450000000000001954, 0.000000000000000000, -18.50000000000000000 ) ) ;
#7877 = SURFACE_SIDE_STYLE ('',( #61265 ) ) ;
#7878 = CARTESIAN_POINT ( 'NONE',  ( -11.00000000000000000, -14.04000000000000092, -17.04524521594300523 ) ) ;
#7879 = ORIENTED_EDGE ( 'NONE', *, *, #28824, .F. ) ;
#7880 = VERTEX_POINT ( 'NONE', #35922 ) ;
#7881 = VERTEX_POINT ( 'NONE', #51126 ) ;
#7882 = ORIENTED_EDGE ( 'NONE', *, *, #7324, .T. ) ;
#7883 = CARTESIAN_POINT ( 'NONE',  ( 9.306483450353372433, 10.91351654964661044, 195.0000000000000284 ) ) ;
#7884 = DIRECTION ( 'NONE',  ( 1.678252938371784572E-14, 1.000000000000000000, 0.000000000000000000 ) ) ;
#7885 = DIRECTION ( 'NONE',  ( -0.000000000000000000, 3.673940397442059868E-16, -1.000000000000000000 ) ) ;
#7886 = EDGE_CURVE ( 'NONE', #32538, #30457, #24621, .T. ) ;
#7887 = DIRECTION ( 'NONE',  ( -1.000000000000000000, 0.000000000000000000, 0.000000000000000000 ) ) ;
#7888 = CIRCLE ( 'NONE', #14674, 2.215251240775983899 ) ;
#7889 = ORIENTED_EDGE ( 'NONE', *, *, #374, .F. ) ;
#7890 = ORIENTED_EDGE ( 'NONE', *, *, #3305, .T. ) ;
#7891 = ORIENTED_EDGE ( 'NONE', *, *, #45330, .F. ) ;
#7892 = AXIS2_PLACEMENT_3D ( 'NONE', #45147, #35226, #28885 ) ;
#7893 = CARTESIAN_POINT ( 'NONE',  ( -9.689726262117227762, 9.689726262117183353, 26.00000000000000711 ) ) ;
#7894 = ORIENTED_EDGE ( 'NONE', *, *, #59371, .T. ) ;
#7895 = ORIENTED_EDGE ( 'NONE', *, *, #61402, .F. ) ;
#7896 = ADVANCED_FACE ( 'NONE', ( #24258 ), #35197, .T. ) ;
#7897 = ADVANCED_FACE ( 'NONE', ( #51839 ), #63502, .T. ) ;
#7898 = VERTEX_POINT ( 'NONE', #46518 ) ;
#7899 = AXIS2_PLACEMENT_3D ( 'NONE', #16928, #55110, #50133 ) ;
#7900 = ORIENTED_EDGE ( 'NONE', *, *, #33146, .F. ) ;
#7901 = DIRECTION ( 'NONE',  ( 0.000000000000000000, -1.000000000000000000, 0.000000000000000000 ) ) ;
#7902 = ADVANCED_FACE ( 'NONE', ( #56778 ), #62789, .F. ) ;
#7903 = EDGE_CURVE ( 'NONE', #29653, #30889, #41214, .T. ) ;
#7905 = VERTEX_POINT ( 'NONE', #36268 ) ;
#7904 = DIRECTION ( 'NONE',  ( 0.000000000000000000, -3.673940397442059868E-16, 1.000000000000000000 ) ) ;
#7906 = ORIENTED_EDGE ( 'NONE', *, *, #4347, .F. ) ;
#7907 = AXIS2_PLACEMENT_3D ( 'NONE', #24134, #13521, #29429 ) ;
#7908 = CARTESIAN_POINT ( 'NONE',  ( -11.19000000000000128, -12.00000000000000000, -4.250000000000000000 ) ) ;
#7909 = CARTESIAN_POINT ( 'NONE',  ( 49.00000000000000000, -0.2000000000089119934, -8.913009219568841313E-12 ) ) ;
#7910 = EDGE_CURVE ( 'NONE', #32512, #38612, #3743, .T. ) ;
#7911 = LINE ( 'NONE', #7572, #41528 ) ;
#7913 = EDGE_LOOP ( 'NONE', ( #68696, #62911, #16531, #33759 ) ) ;
#7912 = CARTESIAN_POINT ( 'NONE',  ( 0.000000000000000000, 0.000000000000000000, -1.000000000000000000 ) ) ;
#7914 = EDGE_LOOP ( 'NONE', ( #51406, #36601, #58545, #62082 ) ) ;
#7915 = VECTOR ( 'NONE', #22392, 1000.000000000000000 ) ;
#7916 = VECTOR ( 'NONE', #27743, 1000.000000000000000 ) ;
#7917 = CARTESIAN_POINT ( 'NONE',  ( 11.00000000000000000, -5.200000000000001066, 26.59999999999999787 ) ) ;
#7918 = FACE_OUTER_BOUND ( 'NONE', #48283, .T. ) ;
#7919 = LINE ( 'NONE', #1933, #14649 ) ;
#7920 = ORIENTED_EDGE ( 'NONE', *, *, #47268, .F. ) ;
#7921 = FACE_OUTER_BOUND ( 'NONE', #3147, .T. ) ;
#7922 = LINE ( 'NONE', #50371, #19625 ) ;
#7923 = DIRECTION ( 'NONE',  ( 0.000000000000000000, 0.000000000000000000, 1.000000000000000000 ) ) ;
#7924 = AXIS2_PLACEMENT_3D ( 'NONE', #40258, #2774, #51929 ) ;
#7925 = VERTEX_POINT ( 'NONE', #4111 ) ;
#7926 = CARTESIAN_POINT ( 'NONE',  ( -5.242976262117275077, -5.257023737882800418, 26.00000000000000711 ) ) ;
#7927 = CARTESIAN_POINT ( 'NONE',  ( 0.000000000000000000, 0.000000000000000000, -14.00000000000000000 ) ) ;
#7928 = DIRECTION ( 'NONE',  ( 0.000000000000000000, 0.000000000000000000, 1.000000000000000000 ) ) ;
#7929 = ORIENTED_EDGE ( 'NONE', *, *, #6622, .T. ) ;
#7930 = VECTOR ( 'NONE', #13488, 1000.000000000000000 ) ;
#7931 = LINE ( 'NONE', #2294, #32445 ) ;
#7932 = VECTOR ( 'NONE', #2095, 1000.000000000000000 ) ;
#7933 = DIRECTION ( 'NONE',  ( 0.000000000000000000, 0.000000000000000000, 1.000000000000000000 ) ) ;
#7934 = CARTESIAN_POINT ( 'NONE',  ( 176.4833316329832940, -10.00000000000000178, 322.4587476295993156 ) ) ;
#7935 = EDGE_CURVE ( 'NONE', #21629, #43736, #25682, .T. ) ;
#7936 = VECTOR ( 'NONE', #60665, 1000.000000000000000 ) ;
#7937 = VERTEX_POINT ( 'NONE', #41921 ) ;
#7938 = CARTESIAN_POINT ( 'NONE',  ( 30.90000000000000213, 0.000000000000000000, 2.370429594502469981E-15 ) ) ;
#7939 = DIRECTION ( 'NONE',  ( 1.836970198721029934E-16, 1.836970198721010706E-16, -1.000000000000000000 ) ) ;
#7940 = CARTESIAN_POINT ( 'NONE',  ( 15.00000000000002132, -0.4999999999999964473, -26.50000000000003197 ) ) ;
#7941 = EDGE_CURVE ( 'NONE', #27762, #9056, #15056, .T. ) ;
#7942 = AXIS2_PLACEMENT_3D ( 'NONE', #3258, #46385, #67965 ) ;
#7943 = EDGE_CURVE ( 'NONE', #46313, #55046, #26716, .T. ) ;
#7944 = CARTESIAN_POINT ( 'NONE',  ( 10.62249899919920004, -25.00000000000000000, -17.50000000000000000 ) ) ;
#7945 = CARTESIAN_POINT ( 'NONE',  ( 30.00000000000000000, -17.35230188589299871, 15.35019951917099945 ) ) ;
#7946 = ORIENTED_EDGE ( 'NONE', *, *, #56164, .F. ) ;
#7947 = DIRECTION ( 'NONE',  ( 1.000000000000000000, -4.121462285523435444E-16, 0.000000000000000000 ) ) ;
#7948 = DIRECTION ( 'NONE',  ( 0.000000000000000000, 0.000000000000000000, 1.000000000000000000 ) ) ;
#7949 = CARTESIAN_POINT ( 'NONE',  ( -7.250000000000001776, -7.249999999999998224, -26.00000000000001066 ) ) ;
#7950 = EDGE_CURVE ( 'NONE', #52765, #43546, #19196, .T. ) ;
#7951 = CARTESIAN_POINT ( 'NONE',  ( 7.250000000000005329, 7.250000000000000888, -7.500000000000000000 ) ) ;
#7952 = DIRECTION ( 'NONE',  ( 0.000000000000000000, 1.000000000000000000, -0.000000000000000000 ) ) ;
#7953 = AXIS2_PLACEMENT_3D ( 'NONE', #459, #28693, #12087 ) ;
#7954 = ORIENTED_EDGE ( 'NONE', *, *, #6872, .T. ) ;
#7956 = ORIENTED_EDGE ( 'NONE', *, *, #45108, .T. ) ;
#7955 = LINE ( 'NONE', #29880, #10400 ) ;
#7957 = CARTESIAN_POINT ( 'NONE',  ( 30.00000000000000000, -5.599999999999379696, -26.60000000000059828 ) ) ;
#7958 = DIRECTION ( 'NONE',  ( 0.000000000000000000, 0.000000000000000000, -1.000000000000000000 ) ) ;
#7959 = EDGE_LOOP ( 'NONE', ( #7808, #24342, #69344, #12258 ) ) ;
#7960 = CIRCLE ( 'NONE', #28262, 0.4000000000000010214 ) ;
#7961 = CIRCLE ( 'NONE', #50864, 4.500000000000190958 ) ;
#7962 = FACE_OUTER_BOUND ( 'NONE', #1558, .T. ) ;
#7963 = EDGE_LOOP ( 'NONE', ( #44618, #14542, #58710, #23753 ) ) ;
#7964 = DIRECTION ( 'NONE',  ( -1.000000000000000000, 0.000000000000000000, 0.000000000000000000 ) ) ;
#7965 = ORIENTED_EDGE ( 'NONE', *, *, #36786, .T. ) ;
#7966 = VERTEX_POINT ( 'NONE', #37674 ) ;
#7967 = CARTESIAN_POINT ( 'NONE',  ( 49.00000000000000000, -21.00000000000000000, 13.86939075806900057 ) ) ;
#7968 = CARTESIAN_POINT ( 'NONE',  ( 34.89999999999999858, 0.000000000000000000, 0.000000000000000000 ) ) ;
#7969 = CARTESIAN_POINT ( 'NONE',  ( 0.000000000000000000, 8.250000000000001776, -21.00000000000000000 ) ) ;
#7970 = CARTESIAN_POINT ( 'NONE',  ( 24.00000000000000000, -15.50000000000000000, -19.33772233983200195 ) ) ;
#7971 = AXIS2_PLACEMENT_3D ( 'NONE', #56434, #46178, #23562 ) ;
#7972 = ORIENTED_EDGE ( 'NONE', *, *, #19333, .T. ) ;
#7973 = ORIENTED_EDGE ( 'NONE', *, *, #56952, .F. ) ;
#7974 = LINE ( 'NONE', #12234, #5326 ) ;
#7975 = DIRECTION ( 'NONE',  ( 0.000000000000000000, 0.000000000000000000, -1.000000000000000000 ) ) ;
#7976 = ORIENTED_EDGE ( 'NONE', *, *, #27621, .T. ) ;
#7977 = ORIENTED_EDGE ( 'NONE', *, *, #14557, .T. ) ;
#7978 = ORIENTED_EDGE ( 'NONE', *, *, #51634, .F. ) ;
#7979 = LINE ( 'NONE', #20, #14657 ) ;
#7980 = EDGE_CURVE ( 'NONE', #7863, #30319, #36154, .T. ) ;
#7981 = VECTOR ( 'NONE', #63243, 1000.000000000000000 ) ;
#7983 = ORIENTED_EDGE ( 'NONE', *, *, #21906, .F. ) ;
#7982 = DIRECTION ( 'NONE',  ( -1.000000000000000000, 0.000000000000000000, 0.000000000000000000 ) ) ;
#7984 = EDGE_CURVE ( 'NONE', #43890, #46512, #10446, .T. ) ;
#7985 = CARTESIAN_POINT ( 'NONE',  ( -4.727349090213552429, -4.201500623656063915, 455.0000000000000568 ) ) ;
#7986 = CARTESIAN_POINT ( 'NONE',  ( -11.77351654964670935, 4.393516549646602876, 455.0000000000000568 ) ) ;
#7987 = EDGE_CURVE ( 'NONE', #29792, #56057, #31633, .T. ) ;
#7988 = ADVANCED_FACE ( 'NONE', ( #20702 ), #16451, .T. ) ;
#7989 = ORIENTED_EDGE ( 'NONE', *, *, #58161, .T. ) ;
#7990 = AXIS2_PLACEMENT_3D ( 'NONE', #56901, #9180, #35324 ) ;
#7991 = ORIENTED_EDGE ( 'NONE', *, *, #53670, .F. ) ;
#7992 = VECTOR ( 'NONE', #35260, 1000.000000000000114 ) ;
#7993 = DIRECTION ( 'NONE',  ( 1.000000000000000000, -0.000000000000000000, 0.000000000000000000 ) ) ;
#7994 = FACE_OUTER_BOUND ( 'NONE', #21298, .T. ) ;
#7995 = EDGE_CURVE ( 'NONE', #60486, #20922, #15413, .T. ) ;
#7996 = LINE ( 'NONE', #12601, #17946 ) ;
#7997 = EDGE_CURVE ( 'NONE', #3545, #68313, #58894, .T. ) ;
#7998 = VECTOR ( 'NONE', #50320, 1000.000000000000000 ) ;
#7999 = DIRECTION ( 'NONE',  ( 1.000000000000000000, 5.013651664672856055E-16, 0.000000000000000000 ) ) ;
#8000 = CARTESIAN_POINT ( 'NONE',  ( -15.50000000000000000, -1.037157890325000054, -18.50000000000000000 ) ) ;
#8002 = EDGE_LOOP ( 'NONE', ( #39884, #61912, #50546 ) ) ;
#8001 = DIRECTION ( 'NONE',  ( 1.000000000000000000, -1.047444401652940007E-14, 1.836970198721010706E-16 ) ) ;
#8003 = ORIENTED_EDGE ( 'NONE', *, *, #2282, .T. ) ;
#8004 = LINE ( 'NONE', #62443, #15163 ) ;
#8005 = DIRECTION ( 'NONE',  ( 0.000000000000000000, 0.000000000000000000, 1.000000000000000000 ) ) ;
#8006 = AXIS2_PLACEMENT_3D ( 'NONE', #62373, #29852, #51782 ) ;
#8007 = CARTESIAN_POINT ( 'NONE',  ( 47.00000000000000000, 4.286263797015736595E-16, -3.500000000000000000 ) ) ;
#8008 = DIRECTION ( 'NONE',  ( -0.000000000000000000, 3.673940397442059868E-16, -1.000000000000000000 ) ) ;
#8009 = LINE ( 'NONE', #29582, #52301 ) ;
#8010 = ORIENTED_EDGE ( 'NONE', *, *, #8666, .F. ) ;
#8011 = CARTESIAN_POINT ( 'NONE',  ( 7.811466277050736373, -4.740315990920255018, 455.0000000000000568 ) ) ;
#8012 = LINE ( 'NONE', #19671, #39489 ) ;
#8013 = CARTESIAN_POINT ( 'NONE',  ( -15.50000000000000000, -2.500000000000000000, -23.94337567297399971 ) ) ;
#8014 = CARTESIAN_POINT ( 'NONE',  ( 13.00000000000000178, -16.64230188589299786, 14.64519951917100116 ) ) ;
#8015 = CIRCLE ( 'NONE', #22731, 24.99999999998784972 ) ;
#8016 = DIRECTION ( 'NONE',  ( 0.000000000000000000, 0.000000000000000000, 1.000000000000000000 ) ) ;
#8017 = DIRECTION ( 'NONE',  ( -1.836970198721029934E-16, 1.836970198721036590E-16, -1.000000000000000000 ) ) ;
#8018 = DIRECTION ( 'NONE',  ( -0.000000000000000000, -0.000000000000000000, -1.000000000000000000 ) ) ;
#8019 = VERTEX_POINT ( 'NONE', #38031 ) ;
#8020 = CARTESIAN_POINT ( 'NONE',  ( -6.858227778582845602, -3.003254798005714488, 54.00000000000000711 ) ) ;
#8021 = CARTESIAN_POINT ( 'NONE',  ( -7.250000000000001776, -7.249999999999998224, -22.00000000000000000 ) ) ;
#8022 = VERTEX_POINT ( 'NONE', #53592 ) ;
#8023 = LINE ( 'NONE', #29597, #26724 ) ;
#8024 = CARTESIAN_POINT ( 'NONE',  ( 27.90000000000000213, -0.1999999999911430404, -8.864436962241481021E-12 ) ) ;
#8025 = ADVANCED_FACE ( 'NONE', ( #16101 ), #69844, .F. ) ;
#8026 = DIRECTION ( 'NONE',  ( 1.000000000000000000, 0.000000000000000000, 0.000000000000000000 ) ) ;
#8027 = CARTESIAN_POINT ( 'NONE',  ( -15.50000000000000000, -2.500000000000000000, 21.05662432702600029 ) ) ;
#8028 = CARTESIAN_POINT ( 'NONE',  ( 8.250000000000005329, 7.250000000000000888, -16.00000000000000000 ) ) ;
#8029 = VECTOR ( 'NONE', #23058, 1000.000000000000114 ) ;
#8030 = ORIENTED_EDGE ( 'NONE', *, *, #44863, .F. ) ;
#8031 = CARTESIAN_POINT ( 'NONE',  ( -8.393516549646768965, -5.668387132715940524, 455.0000000000000568 ) ) ;
#8032 = AXIS2_PLACEMENT_3D ( 'NONE', #66193, #67235, #7823 ) ;
#8033 = ORIENTED_EDGE ( 'NONE', *, *, #1483, .T. ) ;
#8034 = LINE ( 'NONE', #40575, #14161 ) ;
#8035 = VERTEX_POINT ( 'NONE', #27406 ) ;
#8036 = DIRECTION ( 'NONE',  ( -0.000000000000000000, -0.000000000000000000, 1.000000000000000000 ) ) ;
#8037 = EDGE_CURVE ( 'NONE', #52042, #64218, #47927, .T. ) ;
#8038 = VERTEX_POINT ( 'NONE', #48286 ) ;
#8039 = VECTOR ( 'NONE', #30851, 1000.000000000000000 ) ;
#8040 = AXIS2_PLACEMENT_3D ( 'NONE', #63916, #63570, #64955 ) ;
#8041 = DIRECTION ( 'NONE',  ( -1.000000000000000000, 0.000000000000000000, 0.000000000000000000 ) ) ;
#8042 = EDGE_CURVE ( 'NONE', #391, #12677, #54198, .T. ) ;
#8043 = DIRECTION ( 'NONE',  ( 1.000000000000000000, 0.000000000000000000, 0.000000000000000000 ) ) ;
#8044 = ORIENTED_EDGE ( 'NONE', *, *, #45661, .F. ) ;
#8045 = EDGE_LOOP ( 'NONE', ( #15241, #41370, #7625, #7179 ) ) ;
#8046 = FACE_OUTER_BOUND ( 'NONE', #43894, .T. ) ;
#8047 = ORIENTED_EDGE ( 'NONE', *, *, #19650, .T. ) ;
#8048 = AXIS2_PLACEMENT_3D ( 'NONE', #52426, #8924, #20588 ) ;
#8049 = ORIENTED_EDGE ( 'NONE', *, *, #42409, .T. ) ;
#8050 = FACE_OUTER_BOUND ( 'NONE', #53608, .T. ) ;
#8051 = DIRECTION ( 'NONE',  ( -1.000000000000000000, 0.000000000000000000, 0.000000000000000000 ) ) ;
#8052 = FACE_OUTER_BOUND ( 'NONE', #17377, .T. ) ;
#8053 = ORIENTED_EDGE ( 'NONE', *, *, #31082, .T. ) ;
#8054 = DIRECTION ( 'NONE',  ( -1.000000000000000000, 4.121462285523435444E-16, 1.514200678731842937E-31 ) ) ;
#8055 = CIRCLE ( 'NONE', #2417, 0.2999999999994933386 ) ;
#8057 = FACE_OUTER_BOUND ( 'NONE', #63666, .T. ) ;
#8056 = CARTESIAN_POINT ( 'NONE',  ( -30.00000000000000000, -5.000000000000000000, -27.00000000000000000 ) ) ;
#8058 = VERTEX_POINT ( 'NONE', #42966 ) ;
#8060 = ORIENTED_EDGE ( 'NONE', *, *, #30620, .F. ) ;
#8059 = DIRECTION ( 'NONE',  ( 8.540177112501197482E-15, 1.000000000000000000, -0.000000000000000000 ) ) ;
#8061 = ORIENTED_EDGE ( 'NONE', *, *, #13623, .T. ) ;
#8062 = EDGE_CURVE ( 'NONE', #11799, #42510, #32724, .T. ) ;
#8063 = DIRECTION ( 'NONE',  ( 1.000000000000000000, 0.000000000000000000, 0.000000000000000000 ) ) ;
#8064 = DIRECTION ( 'NONE',  ( -1.000000000000000000, 0.000000000000000000, 0.000000000000000000 ) ) ;
#8065 = ORIENTED_EDGE ( 'NONE', *, *, #43626, .F. ) ;
#8066 = DIRECTION ( 'NONE',  ( 1.836970198721029934E-16, -1.836970198721036344E-16, 1.000000000000000000 ) ) ;
#8067 = DIRECTION ( 'NONE',  ( 0.000000000000000000, -0.1249999999999996531, 0.9921567416492215186 ) ) ;
#8068 = AXIS2_PLACEMENT_3D ( 'NONE', #1566, #48632, #202 ) ;
#8069 = EDGE_CURVE ( 'NONE', #67352, #10965, #535, .T. ) ;
#8070 = VERTEX_POINT ( 'NONE', #22104 ) ;
#8071 = EDGE_CURVE ( 'NONE', #49745, #47971, #50778, .T. ) ;
#8072 = VERTEX_POINT ( 'NONE', #27059 ) ;
#8073 = DIRECTION ( 'NONE',  ( 0.000000000000000000, -0.9921567416492215186, 0.1249999999999996531 ) ) ;
#8074 = CARTESIAN_POINT ( 'NONE',  ( -6.651770455163739548, 7.342976262117183239, 54.00000000000000711 ) ) ;
#8075 = ADVANCED_FACE ( 'NONE', ( #26024 ), #47577, .F. ) ;
#8076 = ORIENTED_EDGE ( 'NONE', *, *, #45284, .F. ) ;
#8077 = CARTESIAN_POINT ( 'NONE',  ( 30.00000000000000000, -5.000000000000000000, 27.00000000000000000 ) ) ;
#8078 = DIRECTION ( 'NONE',  ( 1.000000000000000000, -0.000000000000000000, 0.000000000000000000 ) ) ;
#8079 = EDGE_CURVE ( 'NONE', #22759, #37065, #38385, .T. ) ;
#8080 = LINE ( 'NONE', #67507, #29440 ) ;
#8081 = AXIS2_PLACEMENT_3D ( 'NONE', #8888, #52035, #31179 ) ;
#8082 = VERTEX_POINT ( 'NONE', #60619 ) ;
#8083 = EDGE_CURVE ( 'NONE', #66296, #69443, #18050, .T. ) ;
#8084 = VECTOR ( 'NONE', #13041, 1000.000000000000000 ) ;
#8085 = FACE_OUTER_BOUND ( 'NONE', #64906, .T. ) ;
#8086 = DIRECTION ( 'NONE',  ( 1.836970198721029934E-16, -1.836970198721036344E-16, 1.000000000000000000 ) ) ;
#8087 = ORIENTED_EDGE ( 'NONE', *, *, #22093, .T. ) ;
#8089 = ORIENTED_EDGE ( 'NONE', *, *, #34965, .F. ) ;
#8088 = DIRECTION ( 'NONE',  ( 1.000000000000000000, -0.000000000000000000, -0.000000000000000000 ) ) ;
#8090 = DIRECTION ( 'NONE',  ( 0.7071067811865474617, -0.7071067811865474617, 0.000000000000000000 ) ) ;
#8091 = DIRECTION ( 'NONE',  ( 0.000000000000000000, 0.000000000000000000, 1.000000000000000000 ) ) ;
#8092 = EDGE_CURVE ( 'NONE', #27791, #68548, #17834, .T. ) ;
#8093 = CARTESIAN_POINT ( 'NONE',  ( 29.50000000000000355, -11.50000000000100009, -19.50000000000103739 ) ) ;
#8094 = VECTOR ( 'NONE', #37307, 1000.000000000000000 ) ;
#8095 = CLOSED_SHELL ( 'NONE', ( #53061, #59530, #52570, #51828, #19357, #45008, #8879, #67806, #8113, #55752, #43523, #15975, #19612, #14433, #44856, #13090, #27181, #2757 ) ) ;
#8096 = DIRECTION ( 'NONE',  ( 1.000000000000000000, -1.254221251785257574E-14, 0.000000000000000000 ) ) ;
#8097 = LINE ( 'NONE', #23668, #30801 ) ;
#8098 = VERTEX_POINT ( 'NONE', #17478 ) ;
#8099 = CARTESIAN_POINT ( 'NONE',  ( 30.00000000000000000, -11.50000000000100009, -19.50000000000103739 ) ) ;
#8100 = DIRECTION ( 'NONE',  ( -0.4999999999989417354, 0.000000000000000000, -0.8660254037850495523 ) ) ;
#8101 = DIRECTION ( 'NONE',  ( -1.000000000000000000, 0.000000000000000000, 0.000000000000000000 ) ) ;
#8103 = ORIENTED_EDGE ( 'NONE', *, *, #16394, .T. ) ;
#8102 = CARTESIAN_POINT ( 'NONE',  ( 6.836383711243005479, -6.364920264886905876, 54.00000000000000711 ) ) ;
#8104 = DIRECTION ( 'NONE',  ( 1.836970198721029934E-16, 1.836970198721010706E-16, -1.000000000000000000 ) ) ;
#8105 = EDGE_CURVE ( 'NONE', #56996, #26669, #37316, .T. ) ;
#8106 = CARTESIAN_POINT ( 'NONE',  ( 40.90000000000000568, -16.96999999999999886, 21.00000000000000000 ) ) ;
#8107 = CIRCLE ( 'NONE', #47651, 1.000000000000000888 ) ;
#8108 = ORIENTED_EDGE ( 'NONE', *, *, #37525, .T. ) ;
#8109 = ORIENTED_EDGE ( 'NONE', *, *, #54793, .T. ) ;
#8110 = CARTESIAN_POINT ( 'NONE',  ( -11.47551654964667733, 11.07551654964660237, 195.0000000000000284 ) ) ;
#8111 = CARTESIAN_POINT ( 'NONE',  ( 2.420780051175163816, 8.697938382363089360, 26.00000000000000711 ) ) ;
#8112 = ORIENTED_EDGE ( 'NONE', *, *, #27139, .F. ) ;
#8113 = ADVANCED_FACE ( 'NONE', ( #7203 ), #45037, .F. ) ;
#8114 = CYLINDRICAL_SURFACE ( 'NONE', #41372, 0.1749999999999989342 ) ;
#8115 = LINE ( 'NONE', #57621, #40614 ) ;
#8116 = EDGE_CURVE ( 'NONE', #9056, #31600, #59926, .T. ) ;
#8117 = ADVANCED_BREP_SHAPE_REPRESENTATION ( '', ( #21303, #45918 ), #66261 ) ;
#8118 = CARTESIAN_POINT ( 'NONE',  ( -29.25000000000000000, -5.000000000000000000, 26.25000000000000000 ) ) ;
#8119 = ORIENTED_EDGE ( 'NONE', *, *, #17853, .T. ) ;
#8120 = LINE ( 'NONE', #3893, #30381 ) ;
#8121 = ORIENTED_EDGE ( 'NONE', *, *, #67934, .F. ) ;
#8122 = ADVANCED_FACE ( 'NONE', ( #12510 ), #54635, .T. ) ;
#8123 = ORIENTED_EDGE ( 'NONE', *, *, #44976, .T. ) ;
#8124 = LINE ( 'NONE', #29697, #39301 ) ;
#8125 = VECTOR ( 'NONE', #16581, 1000.000000000000114 ) ;
#8126 = CARTESIAN_POINT ( 'NONE',  ( -2.989207322240185594, 6.858227778582772771, 54.00000000000000711 ) ) ;
#8127 = EDGE_CURVE ( 'NONE', #24527, #69756, #50350, .T. ) ;
#8128 = DIRECTION ( 'NONE',  ( 1.000000000000000000, 0.000000000000000000, 0.000000000000000000 ) ) ;
#8129 = ORIENTED_EDGE ( 'NONE', *, *, #35931, .F. ) ;
#8130 = ORIENTED_EDGE ( 'NONE', *, *, #35054, .T. ) ;
#8131 = AXIS2_PLACEMENT_3D ( 'NONE', #297, #43076, #37780 ) ;
#8132 = CARTESIAN_POINT ( 'NONE',  ( 17.00000000000000000, -17.50000000000000000, 15.70499999999969809 ) ) ;
#8133 = ORIENTED_EDGE ( 'NONE', *, *, #11805, .F. ) ;
#8134 = ORIENTED_EDGE ( 'NONE', *, *, #19268, .T. ) ;
#8135 = CARTESIAN_POINT ( 'NONE',  ( 3.677663764522614454, -6.364920264886879231, 54.00000000000000711 ) ) ;
#8136 = DIRECTION ( 'NONE',  ( 0.000000000000000000, 0.000000000000000000, -1.000000000000000000 ) ) ;
#8137 = CARTESIAN_POINT ( 'NONE',  ( -8.250000000000001776, 7.250000000000000888, -26.00000000000001066 ) ) ;
#8138 = CARTESIAN_POINT ( 'NONE',  ( -9.690000000000001279, 8.750000000000000000, -7.000000000000000000 ) ) ;
#8139 = ADVANCED_FACE ( 'NONE', ( #6860 ), #1232, .T. ) ;
#8140 = VERTEX_POINT ( 'NONE', #33406 ) ;
#8141 = AXIS2_PLACEMENT_3D ( 'NONE', #12402, #67570, #40340 ) ;
#8142 = EDGE_CURVE ( 'NONE', #69139, #31900, #66613, .T. ) ;
#8143 = CARTESIAN_POINT ( 'NONE',  ( 11.50000000000000000, -11.50000000000100009, -15.00000000000084910 ) ) ;
#8145 = DIRECTION ( 'NONE',  ( 1.000000000000000000, -0.000000000000000000, 0.000000000000000000 ) ) ;
#8144 = DIRECTION ( 'NONE',  ( 0.000000000000000000, 0.000000000000000000, 1.000000000000000000 ) ) ;
#8146 = ORIENTED_EDGE ( 'NONE', *, *, #15835, .T. ) ;
#8149 = EDGE_CURVE ( 'NONE', #35485, #35045, #34415, .T. ) ;
#8148 = VERTEX_POINT ( 'NONE', #12850 ) ;
#8147 = CARTESIAN_POINT ( 'NONE',  ( 0.5000000000000000000, -18.00000000000000355, -21.00000000000000000 ) ) ;
#8150 = EDGE_LOOP ( 'NONE', ( #8060, #46712, #54920, #42841 ) ) ;
#8151 = ORIENTED_EDGE ( 'NONE', *, *, #41956, .T. ) ;
#8153 = EDGE_CURVE ( 'NONE', #54936, #18065, #60262, .T. ) ;
#8152 = VECTOR ( 'NONE', #16083, 1000.000000000000000 ) ;
#8154 = EDGE_CURVE ( 'NONE', #28954, #56111, #27750, .T. ) ;
#8155 = CARTESIAN_POINT ( 'NONE',  ( -9.093516549646817992, -10.09643294401455904, 455.0000000000000568 ) ) ;
#8156 = EDGE_CURVE ( 'NONE', #1910, #55424, #39728, .T. ) ;
#8157 = LINE ( 'NONE', #50608, #45072 ) ;
#8158 = VECTOR ( 'NONE', #40571, 1000.000000000000000 ) ;
#8159 = EDGE_CURVE ( 'NONE', #32818, #67039, #13569, .T. ) ;
#8160 = VERTEX_POINT ( 'NONE', #66612 ) ;
#8161 = ORIENTED_EDGE ( 'NONE', *, *, #46646, .T. ) ;
#8162 = ADVANCED_FACE ( 'NONE', ( #49336 ), #18168, .T. ) ;
#8163 = VECTOR ( 'NONE', #17937, 1000.000000000000000 ) ;
#8164 = DIRECTION ( 'NONE',  ( -1.000000000000000000, 0.000000000000000000, 0.000000000000000000 ) ) ;
#8165 = FACE_OUTER_BOUND ( 'NONE', #31987, .T. ) ;
#8166 = ORIENTED_EDGE ( 'NONE', *, *, #39820, .F. ) ;
#8167 = ORIENTED_EDGE ( 'NONE', *, *, #58052, .T. ) ;
#8168 = CARTESIAN_POINT ( 'NONE',  ( 10.09643294401454661, -9.306483450353491449, 455.0000000000000568 ) ) ;
#8169 = ADVANCED_FACE ( 'NONE', ( #23828 ), #22454, .F. ) ;
#8170 = DIRECTION ( 'NONE',  ( 0.000000000000000000, 1.000000000000000000, 0.000000000000000000 ) ) ;
#8171 = ORIENTED_EDGE ( 'NONE', *, *, #41775, .F. ) ;
#8172 = EDGE_CURVE ( 'NONE', #50332, #17779, #24832, .T. ) ;
#8173 = CARTESIAN_POINT ( 'NONE',  ( 283.0000000000000568, -42.50000000000000000, -14.50000000000000000 ) ) ;
#8174 = LINE ( 'NONE', #36101, #15892 ) ;
#8176 = VERTEX_POINT ( 'NONE', #51046 ) ;
#8175 = LINE ( 'NONE', #17398, #3521 ) ;
#8177 = ORIENTED_EDGE ( 'NONE', *, *, #49625, .T. ) ;
#8178 = DIRECTION ( 'NONE',  ( -1.000000000000000000, 0.000000000000000000, 0.000000000000000000 ) ) ;
#8179 = LINE ( 'NONE', #24097, #49269 ) ;
#8180 = LINE ( 'NONE', #12103, #17088 ) ;
#8181 = VECTOR ( 'NONE', #47970, 1000.000000000000000 ) ;
#8182 = CARTESIAN_POINT ( 'NONE',  ( 0.000000000000000000, -8.249999999999998224, -9.000000000000001776 ) ) ;
#8183 = DIRECTION ( 'NONE',  ( 0.000000000000000000, -3.673940397442059868E-16, 1.000000000000000000 ) ) ;
#8184 = CARTESIAN_POINT ( 'NONE',  ( 11.00000000000000000, -11.50000000000100009, 19.50000000000103739 ) ) ;
#8185 = DIRECTION ( 'NONE',  ( 0.6414496315691565753, 0.7671651518153006499, 2.818519042764004597E-16 ) ) ;
#8186 = AXIS2_PLACEMENT_3D ( 'NONE', #10815, #15434, #53618 ) ;
#8187 = ORIENTED_EDGE ( 'NONE', *, *, #23177, .F. ) ;
#8188 = CARTESIAN_POINT ( 'NONE',  ( 28.90000000000000213, 13.66939075806899240, -20.79999999999999361 ) ) ;
#8190 = EDGE_LOOP ( 'NONE', ( #26494, #4937, #45455, #8913 ) ) ;
#8189 = DIRECTION ( 'NONE',  ( 0.7142857142857395036, 0.000000000000000000, 0.6998542122237394469 ) ) ;
#8191 = DIRECTION ( 'NONE',  ( -1.000000000000000000, 0.000000000000000000, 0.000000000000000000 ) ) ;
#8192 = CARTESIAN_POINT ( 'NONE',  ( 8.241237374594243548, 1.620245201994235718, 26.00000000000000711 ) ) ;
#8193 = DIRECTION ( 'NONE',  ( -0.000000000000000000, -0.000000000000000000, 1.000000000000000000 ) ) ;
#8194 = VECTOR ( 'NONE', #4624, 1000.000000000000000 ) ;
#8195 = CARTESIAN_POINT ( 'NONE',  ( 8.250000000000005329, 0.000000000000000000, -14.00000000000000000 ) ) ;
#8196 = LINE ( 'NONE', #29766, #13370 ) ;
#8197 = ORIENTED_EDGE ( 'NONE', *, *, #10600, .F. ) ;
#8198 = CARTESIAN_POINT ( 'NONE',  ( 9.417013320880792904, -1.866219381641561315, 455.0000000000000568 ) ) ;
#8199 = ORIENTED_EDGE ( 'NONE', *, *, #9558, .T. ) ;
#8200 = EDGE_CURVE ( 'NONE', #18501, #68804, #3312, .T. ) ;
#8201 = CARTESIAN_POINT ( 'NONE',  ( 49.00000000000000000, -0.1999999999911795112, 8.826273045769999343E-12 ) ) ;
#8202 = EDGE_CURVE ( 'NONE', #43425, #4452, #22617, .T. ) ;
#8203 = DIRECTION ( 'NONE',  ( 0.000000000000000000, -1.000000000000000000, 0.000000000000000000 ) ) ;
#8204 = VECTOR ( 'NONE', #24595, 1000.000000000000114 ) ;
#8205 = ORIENTED_EDGE ( 'NONE', *, *, #34931, .F. ) ;
#8206 = CARTESIAN_POINT ( 'NONE',  ( 9.795823737882805915, -10.50702373788282529, 54.00000000000000711 ) ) ;
#8207 = ORIENTED_EDGE ( 'NONE', *, *, #1848, .F. ) ;
#8208 = EDGE_CURVE ( 'NONE', #20324, #20952, #68728, .T. ) ;
#8209 = ORIENTED_EDGE ( 'NONE', *, *, #46738, .T. ) ;
#8210 = AXIS2_PLACEMENT_3D ( 'NONE', #63176, #68840, #57867 ) ;
#8211 = DIRECTION ( 'NONE',  ( -1.000000000000000000, 0.000000000000000000, 0.000000000000000000 ) ) ;
#8212 = CARTESIAN_POINT ( 'NONE',  ( 283.0000000000000568, -23.65000000000000568, 12.40000000000000213 ) ) ;
#8213 = VERTEX_POINT ( 'NONE', #57048 ) ;
#8214 = CARTESIAN_POINT ( 'NONE',  ( 7.250000000000005329, -7.249999999999998224, -26.00000000000001066 ) ) ;
#8215 = AXIS2_PLACEMENT_3D ( 'NONE', #27534, #6654, #55448 ) ;
#8216 = EDGE_CURVE ( 'NONE', #60418, #20791, #40071, .T. ) ;
#8217 = LINE ( 'NONE', #35084, #59164 ) ;
#8218 = VECTOR ( 'NONE', #65004, 1000.000000000000000 ) ;
#8219 = ADVANCED_FACE ( 'NONE', ( #40793 ), #51396, .T. ) ;
#8220 = DIRECTION ( 'NONE',  ( -1.000000000000000000, 0.000000000000000000, 0.000000000000000000 ) ) ;
#8221 = VERTEX_POINT ( 'NONE', #35836 ) ;
#8222 = ORIENTED_EDGE ( 'NONE', *, *, #18131, .F. ) ;
#8224 = ORIENTED_EDGE ( 'NONE', *, *, #26718, .F. ) ;
#8223 = CARTESIAN_POINT ( 'NONE',  ( -8.249999999999996447, 8.250000000000001776, 0.000000000000000000 ) ) ;
#8225 = VERTEX_POINT ( 'NONE', #30887 ) ;
#8226 = CARTESIAN_POINT ( 'NONE',  ( -9.915476262117259409, 0.9414762621171833823, 26.00000000000000711 ) ) ;
#8227 = LINE ( 'NONE', #30155, #52409 ) ;
#8228 = CARTESIAN_POINT ( 'NONE',  ( 10.14575131106465378, -25.50000000000000355, -17.00000000000000000 ) ) ;
#8229 = DIRECTION ( 'NONE',  ( 0.000000000000000000, 1.000000000000000000, 0.000000000000000000 ) ) ;
#8230 = CARTESIAN_POINT ( 'NONE',  ( 275.0000000000000000, -21.00000000000000000, 0.000000000000000000 ) ) ;
#8231 = DIRECTION ( 'NONE',  ( 1.000000000000000000, 0.000000000000000000, 0.000000000000000000 ) ) ;
#8232 = AXIS2_PLACEMENT_3D ( 'NONE', #68764, #47881, #8656 ) ;
#8233 = VERTEX_POINT ( 'NONE', #24539 ) ;
#8234 = VERTEX_POINT ( 'NONE', #61648 ) ;
#8235 = ORIENTED_EDGE ( 'NONE', *, *, #33503, .T. ) ;
#8236 = EDGE_CURVE ( 'NONE', #5139, #27370, #4023, .T. ) ;
#8237 = ORIENTED_EDGE ( 'NONE', *, *, #69535, .F. ) ;
#8238 = CARTESIAN_POINT ( 'NONE',  ( -12.00854180281612571, 7.798491296477156887, 195.0000000000000284 ) ) ;
#8239 = CIRCLE ( 'NONE', #52324, 1.000000000000000888 ) ;
#8240 = CARTESIAN_POINT ( 'NONE',  ( 6.006483450353353959, 5.993516549646629166, 195.0000000000000284 ) ) ;
#8241 = DIRECTION ( 'NONE',  ( 1.000000000000000000, -1.130039751537442024E-14, -1.836970198721050642E-16 ) ) ;
#8242 = EDGE_LOOP ( 'NONE', ( #13871, #55656, #28396, #15748 ) ) ;
#8243 = ORIENTED_EDGE ( 'NONE', *, *, #5868, .F. ) ;
#8244 = ORIENTED_EDGE ( 'NONE', *, *, #17591, .T. ) ;
#8245 = CARTESIAN_POINT ( 'NONE',  ( 283.0000000000000568, -20.50000000000000000, -17.00000000000000000 ) ) ;
#8246 = ORIENTED_EDGE ( 'NONE', *, *, #31685, .F. ) ;
#8247 = ORIENTED_EDGE ( 'NONE', *, *, #35254, .F. ) ;
#8248 = PLANE ( 'NONE',  #48050 ) ;
#8249 = ORIENTED_EDGE ( 'NONE', *, *, #24748, .F. ) ;
#8250 = ORIENTED_EDGE ( 'NONE', *, *, #62843, .T. ) ;
#8251 = LINE ( 'NONE', #16028, #32800 ) ;
#8252 = EDGE_CURVE ( 'NONE', #62948, #51099, #29480, .T. ) ;
#8254 = ORIENTED_EDGE ( 'NONE', *, *, #20781, .T. ) ;
#8253 = LINE ( 'NONE', #45735, #35604 ) ;
#8255 = ORIENTED_EDGE ( 'NONE', *, *, #15129, .T. ) ;
#8256 = LINE ( 'NONE', #29832, #32372 ) ;
#8257 = EDGE_CURVE ( 'NONE', #59763, #50665, #49710, .T. ) ;
#8259 = CARTESIAN_POINT ( 'NONE',  ( 11.75000000000000000, -5.000000000000000000, -21.10805890929250950 ) ) ;
#8258 = VECTOR ( 'NONE', #795, 1000.000000000000000 ) ;
#8260 = FACE_OUTER_BOUND ( 'NONE', #11676, .T. ) ;
#8262 = ORIENTED_EDGE ( 'NONE', *, *, #25942, .F. ) ;
#8261 = CARTESIAN_POINT ( 'NONE',  ( -25.50000000000000355, -15.50000000000000000, -25.99999999999985079 ) ) ;
#8264 = ORIENTED_EDGE ( 'NONE', *, *, #20682, .F. ) ;
#8263 = CIRCLE ( 'NONE', #44390, 8.000000000000000000 ) ;
#8265 = COLOUR_RGB ( '', 0.08235294, 0.09019608, 0.10196078) ;
#8266 = CIRCLE ( 'NONE', #47800, 24.99999999998784972 ) ;
#8267 = DIRECTION ( 'NONE',  ( -0.000000000000000000, -0.000000000000000000, -1.000000000000000000 ) ) ;
#8268 = LINE ( 'NONE', #13584, #24426 ) ;
#8269 = DIRECTION ( 'NONE',  ( 0.000000000000000000, 0.000000000000000000, 1.000000000000000000 ) ) ;
#8270 = AXIS2_PLACEMENT_3D ( 'NONE', #5261, #15860, #15524 ) ;
#8271 = VECTOR ( 'NONE', #20037, 1000.000000000000000 ) ;
#8272 = EDGE_LOOP ( 'NONE', ( #27221, #63272, #26068, #2513, #38933, #38240, #69156 ) ) ;
#8273 = DIRECTION ( 'NONE',  ( -1.000000000000000000, 0.000000000000000000, 0.000000000000000000 ) ) ;
#8274 = CARTESIAN_POINT ( 'NONE',  ( -8.250000000000001776, 0.000000000000000000, -13.50000000000000178 ) ) ;
#8275 = CARTESIAN_POINT ( 'NONE',  ( -3.667976262117328190, -9.737023737882820384, 54.00000000000000711 ) ) ;
#8276 = VERTEX_POINT ( 'NONE', #8957 ) ;
#8277 = DIRECTION ( 'NONE',  ( 1.000000000000000000, 0.000000000000000000, 0.000000000000000000 ) ) ;
#8278 = CARTESIAN_POINT ( 'NONE',  ( -15.50000000000000000, -1.037157890325000054, 22.50000000000000000 ) ) ;
#8279 = CARTESIAN_POINT ( 'NONE',  ( -10.03972626211731978, -8.930623737882752877, 54.00000000000000711 ) ) ;
#8280 = FACE_OUTER_BOUND ( 'NONE', #7263, .T. ) ;
#8281 = AXIS2_PLACEMENT_3D ( 'NONE', #43536, #10673, #37554 ) ;
#8282 = EDGE_LOOP ( 'NONE', ( #5574, #39725, #9669, #67524, #13706, #42156, #32015, #55094 ) ) ;
#8283 = CARTESIAN_POINT ( 'NONE',  ( 7.000000000000000000, -32.44999999999905071, 13.20000000000091944 ) ) ;
#8284 = ADVANCED_FACE ( 'NONE', ( #56353 ), #24880, .T. ) ;
#8285 = EDGE_LOOP ( 'NONE', ( #2956, #31235, #12427, #6001 ) ) ;
#8286 = CYLINDRICAL_SURFACE ( 'NONE', #56372, 0.8099999999999999423 ) ;
#8287 = DIRECTION ( 'NONE',  ( -0.000000000000000000, 3.673940397442059868E-16, -1.000000000000000000 ) ) ;
#8288 = DIRECTION ( 'NONE',  ( 0.000000000000000000, 0.000000000000000000, -1.000000000000000000 ) ) ;
#8289 = AXIS2_PLACEMENT_3D ( 'NONE', #52140, #30232, #36945 ) ;
#8290 = EDGE_CURVE ( 'NONE', #44995, #5708, #46442, .T. ) ;
#8291 = DIRECTION ( 'NONE',  ( 0.000000000000000000, -0.7046037717859445770, 0.7096009616573392131 ) ) ;
#8292 = LINE ( 'NONE', #51444, #47723 ) ;
#8293 = ORIENTED_EDGE ( 'NONE', *, *, #35773, .F. ) ;
#8294 = PLANE ( 'NONE',  #41166 ) ;
#8295 = FACE_OUTER_BOUND ( 'NONE', #52612, .T. ) ;
#8296 = EDGE_CURVE ( 'NONE', #1150, #23929, #23708, .T. ) ;
#8297 = ADVANCED_FACE ( 'NONE', ( #8608 ), #30534, .F. ) ;
#8298 = CARTESIAN_POINT ( 'NONE',  ( -7.250000000000000888, -8.249999999999998224, -10.00000000000000000 ) ) ;
#8299 = CARTESIAN_POINT ( 'NONE',  ( 105.8309041053263257, 5.657408540445008960, 2.000000000000000000 ) ) ;
#8300 = EDGE_CURVE ( 'NONE', #47005, #21718, #67320, .T. ) ;
#8301 = PLANE ( 'NONE',  #20384 ) ;
#8302 = EDGE_CURVE ( 'NONE', #27839, #28029, #18880, .T. ) ;
#8303 = ORIENTED_EDGE ( 'NONE', *, *, #57259, .F. ) ;
#8305 = EDGE_LOOP ( 'NONE', ( #68304, #69736, #33350, #64408, #26166, #68244, #29730, #36286, #65341, #48698, #62535 ) ) ;
#8304 = CARTESIAN_POINT ( 'NONE',  ( 1.866219381641426533, -9.417013320880872840, 455.0000000000000568 ) ) ;
#8306 = AXIS2_PLACEMENT_3D ( 'NONE', #24029, #2124, #7068 ) ;
#8307 = VECTOR ( 'NONE', #1621, 1000.000000000000000 ) ;
#8308 = ADVANCED_FACE ( 'NONE', ( #62000 ), #40443, .F. ) ;
#8309 = DIRECTION ( 'NONE',  ( 0.000000000000000000, 0.000000000000000000, 1.000000000000000000 ) ) ;
#8310 = PLANE ( 'NONE',  #32298 ) ;
#8311 = ORIENTED_EDGE ( 'NONE', *, *, #31074, .T. ) ;
#8312 = VECTOR ( 'NONE', #22833, 1000.000000000000000 ) ;
#8313 = CARTESIAN_POINT ( 'NONE',  ( -30.00000000000000000, -11.50000000000000000, 15.00000000000000000 ) ) ;
#8314 = AXIS2_PLACEMENT_3D ( 'NONE', #46623, #40970, #62903 ) ;
#8315 = ORIENTED_EDGE ( 'NONE', *, *, #62935, .F. ) ;
#8316 = VECTOR ( 'NONE', #53696, 1000.000000000000000 ) ;
#8318 = ORIENTED_EDGE ( 'NONE', *, *, #37002, .T. ) ;
#8317 = VECTOR ( 'NONE', #3992, 1000.000000000000000 ) ;
#8319 = VECTOR ( 'NONE', #46699, 1000.000000000000000 ) ;
#8320 = ORIENTED_EDGE ( 'NONE', *, *, #33430, .F. ) ;
#8321 = CYLINDRICAL_SURFACE ( 'NONE', #10301, 1.000000000000000000 ) ;
#8322 = DIRECTION ( 'NONE',  ( 0.6414496315691446959, 0.7671651518153106419, -0.000000000000000000 ) ) ;
#8323 = FACE_OUTER_BOUND ( 'NONE', #13520, .T. ) ;
#8324 = DIRECTION ( 'NONE',  ( -0.000000000000000000, -0.000000000000000000, -1.000000000000000000 ) ) ;
#8325 = ORIENTED_EDGE ( 'NONE', *, *, #11548, .T. ) ;
#8326 = ORIENTED_EDGE ( 'NONE', *, *, #42243, .T. ) ;
#8327 = FACE_OUTER_BOUND ( 'NONE', #30881, .T. ) ;
#8328 = CARTESIAN_POINT ( 'NONE',  ( -11.18999999999999950, 12.00000000000000000, 0.000000000000000000 ) ) ;
#8329 = ORIENTED_EDGE ( 'NONE', *, *, #6206, .F. ) ;
#8330 = VERTEX_POINT ( 'NONE', #56703 ) ;
#8331 = ORIENTED_EDGE ( 'NONE', *, *, #29576, .F. ) ;
#8332 = CARTESIAN_POINT ( 'NONE',  ( 36.90000000000000568, 13.66939075806899240, 20.79999999999999361 ) ) ;
#8334 = EDGE_LOOP ( 'NONE', ( #61610, #11368, #39362, #5758, #30982, #22450, #5236, #28060 ) ) ;
#8333 = CARTESIAN_POINT ( 'NONE',  ( -12.00000000000000000, 11.18999999999999950, -4.250000000000000000 ) ) ;
#8335 = CARTESIAN_POINT ( 'NONE',  ( 8.835729544836283367, 2.355476262117166986, 26.00000000000000711 ) ) ;
#8336 = EDGE_CURVE ( 'NONE', #45642, #19180, #8251, .T. ) ;
#8337 = LINE ( 'NONE', #29561, #17081 ) ;
#8338 = ORIENTED_EDGE ( 'NONE', *, *, #50494, .F. ) ;
#8339 = ADVANCED_FACE ( 'NONE', ( #42185 ), #16365, .F. ) ;
#8340 = VERTEX_POINT ( 'NONE', #20616 ) ;
#8341 = EDGE_CURVE ( 'NONE', #20615, #49129, #63299, .T. ) ;
#8342 = VECTOR ( 'NONE', #20834, 1000.000000000000000 ) ;
#8343 = EDGE_CURVE ( 'NONE', #29056, #23638, #20969, .T. ) ;
#8344 = CARTESIAN_POINT ( 'NONE',  ( 17.89999999999999858, -0.1999999999911430404, -8.864436962241481021E-12 ) ) ;
#8345 = CARTESIAN_POINT ( 'NONE',  ( 7.826483450353380000, -11.78648345035339418, 195.0000000000000284 ) ) ;
#8346 = LINE ( 'NONE', #40877, #54120 ) ;
#8347 = VECTOR ( 'NONE', #46650, 1000.000000000000114 ) ;
#8348 = AXIS2_PLACEMENT_3D ( 'NONE', #46079, #62687, #3295 ) ;
#8349 = LINE ( 'NONE', #2698, #7539 ) ;
#8350 = DIRECTION ( 'NONE',  ( 1.000000000000000000, 0.000000000000000000, 0.000000000000000000 ) ) ;
#8352 = ORIENTED_EDGE ( 'NONE', *, *, #3767, .T. ) ;
#8351 = DIRECTION ( 'NONE',  ( 0.000000000000000000, 0.000000000000000000, -1.000000000000000000 ) ) ;
#8353 = ORIENTED_EDGE ( 'NONE', *, *, #54021, .T. ) ;
#8354 = CARTESIAN_POINT ( 'NONE',  ( 15.50000000000000000, 998.9628421096749662, 22.50000000000000000 ) ) ;
#8355 = PLANE ( 'NONE',  #16622 ) ;
#8357 = AXIS2_PLACEMENT_3D ( 'NONE', #68389, #2991, #57773 ) ;
#8356 = CARTESIAN_POINT ( 'NONE',  ( 41.09999999999999432, -0.2000000000000000111, 0.000000000000000000 ) ) ;
#8358 = CARTESIAN_POINT ( 'NONE',  ( 10.70000000000000107, -53.81370849898476649, -17.60000000000000142 ) ) ;
#8359 = VECTOR ( 'NONE', #48438, 1000.000000000000000 ) ;
#8360 = PLANE ( 'NONE',  #57947 ) ;
#8361 = EDGE_LOOP ( 'NONE', ( #31465, #63071, #326, #63301 ) ) ;
#8362 = CARTESIAN_POINT ( 'NONE',  ( -7.342976262117259623, 6.651770455163663165, 26.00000000000000711 ) ) ;
#8363 = PLANE ( 'NONE',  #7892 ) ;
#8364 = DIRECTION ( 'NONE',  ( -0.000000000000000000, 1.000000000000000000, 0.000000000000000000 ) ) ;
#8365 = CARTESIAN_POINT ( 'NONE',  ( 14.05000000000000249, -0.2000000000000000111, 22.50000000000000000 ) ) ;
#8366 = EDGE_CURVE ( 'NONE', #13089, #69122, #63770, .T. ) ;
#8367 = VECTOR ( 'NONE', #24985, 1000.000000000000000 ) ;
#8368 = LINE ( 'NONE', #8736, #23603 ) ;
#8369 = CARTESIAN_POINT ( 'NONE',  ( -11.00000000000000000, -14.33999999999999986, 14.50000000000000000 ) ) ;
#8370 = CIRCLE ( 'NONE', #47917, 1.224999999999999423 ) ;
#8371 = FACE_OUTER_BOUND ( 'NONE', #40411, .T. ) ;
#8372 = ORIENTED_EDGE ( 'NONE', *, *, #49831, .F. ) ;
#8373 = DIRECTION ( 'NONE',  ( -0.000000000000000000, -0.000000000000000000, -1.000000000000000000 ) ) ;
#8374 = CARTESIAN_POINT ( 'NONE',  ( -8.250000000000001776, -7.249999999999998224, -26.00000000000001066 ) ) ;
#8375 = ORIENTED_EDGE ( 'NONE', *, *, #59380, .T. ) ;
#8376 = CARTESIAN_POINT ( 'NONE',  ( 7.250000000000005329, -8.249999999999998224, -26.00000000000001066 ) ) ;
#8377 = CARTESIAN_POINT ( 'NONE',  ( -7.250000000000000888, -8.249999999999998224, -14.50000000000000000 ) ) ;
#8378 = LINE ( 'NONE', #53639, #59246 ) ;
#8379 = CARTESIAN_POINT ( 'NONE',  ( 4.149127210878741145, 3.663616288756999406, 54.00000000000000711 ) ) ;
#8380 = CYLINDRICAL_SURFACE ( 'NONE', #6794, 0.5000000000079367624 ) ;
#8381 = EDGE_CURVE ( 'NONE', #13045, #68965, #69061, .T. ) ;
#8382 = ORIENTED_EDGE ( 'NONE', *, *, #54030, .F. ) ;
#8383 = FACE_OUTER_BOUND ( 'NONE', #23362, .T. ) ;
#8384 = VERTEX_POINT ( 'NONE', #63417 ) ;
#8385 = EDGE_CURVE ( 'NONE', #13221, #39386, #23763, .T. ) ;
#8386 = DIRECTION ( 'NONE',  ( -1.000000000000000000, 0.000000000000000000, 0.000000000000000000 ) ) ;
#8387 = DIRECTION ( 'NONE',  ( 0.000000000000000000, 0.000000000000000000, 1.000000000000000000 ) ) ;
#8388 = ORIENTED_EDGE ( 'NONE', *, *, #18627, .F. ) ;
#8389 = DIRECTION ( 'NONE',  ( -0.000000000000000000, 3.673940397442059868E-16, -1.000000000000000000 ) ) ;
#8390 = CIRCLE ( 'NONE', #42330, 1.000000000000000000 ) ;
#8391 = ORIENTED_EDGE ( 'NONE', *, *, #34416, .F. ) ;
#8392 = LINE ( 'NONE', #18303, #17550 ) ;
#8393 = ORIENTED_EDGE ( 'NONE', *, *, #41393, .F. ) ;
#8394 = ORIENTED_EDGE ( 'NONE', *, *, #27796, .F. ) ;
#8395 = DIRECTION ( 'NONE',  ( 1.000000000000000000, 0.000000000000000000, 0.000000000000000000 ) ) ;
#8396 = VERTEX_POINT ( 'NONE', #15680 ) ;
#8397 = ORIENTED_EDGE ( 'NONE', *, *, #42332, .T. ) ;
#8398 = CARTESIAN_POINT ( 'NONE',  ( -7.839518282750232991, -3.430747519065274531, 195.0000000000000284 ) ) ;
#8399 = LINE ( 'NONE', #14061, #33555 ) ;
#8400 = AXIS2_PLACEMENT_3D ( 'NONE', #41254, #67784, #4499 ) ;
#8401 = VECTOR ( 'NONE', #44586, 1000.000000000000000 ) ;
#8402 = PLANE ( 'NONE',  #50218 ) ;
#8403 = ORIENTED_EDGE ( 'NONE', *, *, #43440, .T. ) ;
#8404 = DIRECTION ( 'NONE',  ( -1.000000000000000000, 0.000000000000000000, 0.000000000000000000 ) ) ;
#8406 = LINE ( 'NONE', #68878, #52553 ) ;
#8405 = DIRECTION ( 'NONE',  ( 0.7071067811865447972, -0.7071067811865502373, 0.000000000000000000 ) ) ;
#8407 = VECTOR ( 'NONE', #350, 1000.000000000000000 ) ;
#8408 = AXIS2_PLACEMENT_3D ( 'NONE', #29012, #66832, #29348 ) ;
#8410 = ORIENTED_EDGE ( 'NONE', *, *, #69729, .T. ) ;
#8409 = CIRCLE ( 'NONE', #47954, 1.399999999999998579 ) ;
#8412 = VERTEX_POINT ( 'NONE', #14978 ) ;
#8411 = DIRECTION ( 'NONE',  ( -1.000000000000000000, 0.000000000000000000, 0.000000000000000000 ) ) ;
#8413 = EDGE_LOOP ( 'NONE', ( #10305, #63925, #60058, #39641 ) ) ;
#8414 = APPLICATION_PROTOCOL_DEFINITION ( 'draft international standard', 'automotive_design', 1998, #21429 ) ;
#8415 = VECTOR ( 'NONE', #20772, 1000.000000000000000 ) ;
#8416 = DIRECTION ( 'NONE',  ( -0.000000000000000000, 3.673940397442059868E-16, -1.000000000000000000 ) ) ;
#8418 = ORIENTED_EDGE ( 'NONE', *, *, #3824, .F. ) ;
#8417 = CARTESIAN_POINT ( 'NONE',  ( -15.50000000000000000, 998.9628421096749662, -22.50000000000000000 ) ) ;
#8419 = DIRECTION ( 'NONE',  ( 1.000000000000000000, -0.000000000000000000, -0.000000000000000000 ) ) ;
#8420 =( GEOMETRIC_REPRESENTATION_CONTEXT ( 3 ) GLOBAL_UNCERTAINTY_ASSIGNED_CONTEXT ( ( #16102 ) ) GLOBAL_UNIT_ASSIGNED_CONTEXT ( ( #29587, #66024, #34882 ) ) REPRESENTATION_CONTEXT ( 'NONE', 'WORKASPACE' ) );
#8421 = CARTESIAN_POINT ( 'NONE',  ( -10.49297626211725998, 9.781776262117173104, 54.00000000000000711 ) ) ;
#8422 = ORIENTED_EDGE ( 'NONE', *, *, #33110, .F. ) ;
#8423 = ORIENTED_EDGE ( 'NONE', *, *, #30090, .T. ) ;
#8424 = EDGE_CURVE ( 'NONE', #15754, #66149, #26634, .T. ) ;
#8425 = VECTOR ( 'NONE', #14156, 1000.000000000000000 ) ;
#8426 = DIRECTION ( 'NONE',  ( 0.000000000000000000, 0.000000000000000000, -1.000000000000000000 ) ) ;
#8427 = ORIENTED_EDGE ( 'NONE', *, *, #20253, .T. ) ;
#8428 = EDGE_CURVE ( 'NONE', #43460, #39509, #58108, .T. ) ;
#8429 = DIRECTION ( 'NONE',  ( 1.000000000000000000, 0.000000000000000000, 0.000000000000000000 ) ) ;
#8430 = DIRECTION ( 'NONE',  ( 0.7071067811865510144, 0.7071067811865441310, -8.088905766426390583E-31 ) ) ;
#8431 = LINE ( 'NONE', #46615, #65594 ) ;
#8432 = ORIENTED_EDGE ( 'NONE', *, *, #7688, .T. ) ;
#8433 = CARTESIAN_POINT ( 'NONE',  ( -9.781776262117309884, -9.795823737882740190, 26.00000000000000000 ) ) ;
#8434 = PLANE ( 'NONE',  #15615 ) ;
#8435 = CIRCLE ( 'NONE', #51350, 2.250000000000001776 ) ;
#8437 = VERTEX_POINT ( 'NONE', #52831 ) ;
#8436 = LINE ( 'NONE', #68200, #24074 ) ;
#8439 = ORIENTED_EDGE ( 'NONE', *, *, #59326, .F. ) ;
#8438 = DIRECTION ( 'NONE',  ( 0.000000000000000000, -1.000000000000000000, 0.000000000000000000 ) ) ;
#8440 = CARTESIAN_POINT ( 'NONE',  ( 78.77321854994620765, 47.95351654967443977, 15.00000000000000000 ) ) ;
#8441 = DIRECTION ( 'NONE',  ( 0.000000000000000000, 0.000000000000000000, 1.000000000000000000 ) ) ;
#8442 = VECTOR ( 'NONE', #13957, 1000.000000000000000 ) ;
#8443 = CARTESIAN_POINT ( 'NONE',  ( 0.000000000000000000, 8.250000000000001776, -16.50000000000000000 ) ) ;
#8444 = LINE ( 'NONE', #30024, #27169 ) ;
#8445 = EDGE_CURVE ( 'NONE', #3293, #26867, #43235, .T. ) ;
#8446 = LINE ( 'NONE', #7753, #27420 ) ;
#8447 = ORIENTED_EDGE ( 'NONE', *, *, #36102, .F. ) ;
#8448 = LINE ( 'NONE', #50197, #48203 ) ;
#8449 = CARTESIAN_POINT ( 'NONE',  ( 17.24945551514599984, -15.50000000000000000, 25.53140320652400064 ) ) ;
#8450 = DIRECTION ( 'NONE',  ( -0.000000000000000000, 1.000000000000000000, -0.000000000000000000 ) ) ;
#8452 = VERTEX_POINT ( 'NONE', #5768 ) ;
#8451 = FACE_OUTER_BOUND ( 'NONE', #33215, .T. ) ;
#8453 = AXIS2_PLACEMENT_3D ( 'NONE', #11298, #32878, #54453 ) ;
#8454 = CARTESIAN_POINT ( 'NONE',  ( -16.75000000000000000, -0.2038245569916330158, -23.22168783648699986 ) ) ;
#8455 = AXIS2_PLACEMENT_3D ( 'NONE', #35019, #13809, #56595 ) ;
#8456 = DIRECTION ( 'NONE',  ( 0.000000000000000000, 1.000000000000000000, 0.000000000000000000 ) ) ;
#8457 = ORIENTED_EDGE ( 'NONE', *, *, #35319, .F. ) ;
#8458 = AXIS2_PLACEMENT_3D ( 'NONE', #19990, #41554, #37306 ) ;
#8459 = VERTEX_POINT ( 'NONE', #37250 ) ;
#8460 = CARTESIAN_POINT ( 'NONE',  ( -4.173516549646666185, 11.99351654964658920, 455.0000000000000568 ) ) ;
#8461 = DIRECTION ( 'NONE',  ( -1.836970198721029934E-16, 1.836970198721036590E-16, -1.000000000000000000 ) ) ;
#8462 = VERTEX_POINT ( 'NONE', #31940 ) ;
#8463 = DIRECTION ( 'NONE',  ( 0.000000000000000000, 0.000000000000000000, 1.000000000000000000 ) ) ;
#8464 = VECTOR ( 'NONE', #16013, 1000.000000000000000 ) ;
#8465 = DIRECTION ( 'NONE',  ( 0.000000000000000000, 0.000000000000000000, 1.000000000000000000 ) ) ;
#8466 = DIRECTION ( 'NONE',  ( -1.000000000000000000, 0.000000000000000000, 0.000000000000000000 ) ) ;
#8467 = EDGE_CURVE ( 'NONE', #9839, #63180, #36905, .T. ) ;
#8468 = DIRECTION ( 'NONE',  ( 1.000000000000000000, -0.000000000000000000, 0.000000000000000000 ) ) ;
#8469 = VECTOR ( 'NONE', #18987, 1000.000000000000000 ) ;
#8470 = ORIENTED_EDGE ( 'NONE', *, *, #65563, .T. ) ;
#8471 = ADVANCED_FACE ( 'NONE', ( #21328 ), #4718, .T. ) ;
#8472 = CARTESIAN_POINT ( 'NONE',  ( -7.793516549646712477, 11.11351654964660085, 195.0000000000000284 ) ) ;
#8473 = VERTEX_POINT ( 'NONE', #26280 ) ;
#8474 = ORIENTED_EDGE ( 'NONE', *, *, #66512, .T. ) ;
#8475 = ADVANCED_FACE ( 'NONE', ( #10710 ), #27334, .T. ) ;
#8476 = ORIENTED_EDGE ( 'NONE', *, *, #27950, .F. ) ;
#8477 = DIRECTION ( 'NONE',  ( -1.000000000000000000, 0.000000000000000000, 0.000000000000000000 ) ) ;
#8478 = EDGE_CURVE ( 'NONE', #68313, #1298, #26987, .T. ) ;
#8479 = ADVANCED_FACE ( 'NONE', ( #11067 ), #53868, .F. ) ;
#8480 = CARTESIAN_POINT ( 'NONE',  ( 49.00000000000000000, 20.60000000000000142, -13.86939075806900057 ) ) ;
#8481 = EDGE_CURVE ( 'NONE', #67890, #37232, #60999, .T. ) ;
#8482 = LINE ( 'NONE', #68243, #47937 ) ;
#8483 = ORIENTED_EDGE ( 'NONE', *, *, #12475, .T. ) ;
#8484 = ADVANCED_FACE ( 'NONE', ( #55921 ), #22711, .F. ) ;
#8485 = ORIENTED_EDGE ( 'NONE', *, *, #56455, .T. ) ;
#8486 = DIRECTION ( 'NONE',  ( -0.000000000000000000, -0.000000000000000000, 1.000000000000000000 ) ) ;
#8488 = ORIENTED_EDGE ( 'NONE', *, *, #65667, .T. ) ;
#8487 = EDGE_CURVE ( 'NONE', #48502, #245, #29408, .T. ) ;
#8489 = ORIENTED_EDGE ( 'NONE', *, *, #11009, .F. ) ;
#8490 = DIRECTION ( 'NONE',  ( 0.000000000000000000, -3.673940397442059868E-16, 1.000000000000000000 ) ) ;
#8491 = CARTESIAN_POINT ( 'NONE',  ( -7.798499376344157241, -7.272650909786626983, 455.0000000000000568 ) ) ;
#8492 = CARTESIAN_POINT ( 'NONE',  ( -15.91434062215688350, -0.3156604612129211285, -21.29584399676446793 ) ) ;
#8493 = DIRECTION ( 'NONE',  ( -1.000000000000000000, 0.000000000000000000, 0.000000000000000000 ) ) ;
#8494 = ORIENTED_EDGE ( 'NONE', *, *, #59179, .T. ) ;
#8495 = LINE ( 'NONE', #30072, #17599 ) ;
#8497 = PLANE ( 'NONE',  #7339 ) ;
#8496 = CARTESIAN_POINT ( 'NONE',  ( 15.50000000000000000, -0.4000000000000000222, 25.99999999999999645 ) ) ;
#8498 = VERTEX_POINT ( 'NONE', #12763 ) ;
#8500 = ORIENTED_EDGE ( 'NONE', *, *, #18068, .T. ) ;
#8499 = PLANE ( 'NONE',  #52277 ) ;
#8501 = CIRCLE ( 'NONE', #24353, 0.3500000000009988455 ) ;
#8502 = EDGE_LOOP ( 'NONE', ( #27662, #41831, #11526, #23538 ) ) ;
#8503 = ORIENTED_EDGE ( 'NONE', *, *, #47724, .T. ) ;
#8504 = CARTESIAN_POINT ( 'NONE',  ( 39.00000000000000000, -21.00000000000000000, -16.96999999999999886 ) ) ;
#8505 = VECTOR ( 'NONE', #10788, 1000.000000000000000 ) ;
#8506 = VECTOR ( 'NONE', #37790, 1000.000000000000000 ) ;
#8508 = LINE ( 'NONE', #2859, #19140 ) ;
#8507 = AXIS2_PLACEMENT_3D ( 'NONE', #58277, #9847, #47660 ) ;
#8509 = ORIENTED_EDGE ( 'NONE', *, *, #15425, .T. ) ;
#8510 = EDGE_LOOP ( 'NONE', ( #55154, #35024, #10865, #15061 ) ) ;
#8511 = VECTOR ( 'NONE', #68155, 1000.000000000000000 ) ;
#8512 = AXIS2_PLACEMENT_3D ( 'NONE', #14256, #35808, #9651 ) ;
#8513 = DIRECTION ( 'NONE',  ( 0.000000000000000000, 0.000000000000000000, 1.000000000000000000 ) ) ;
#8514 = DIRECTION ( 'NONE',  ( 1.000000000000000000, -0.000000000000000000, -0.000000000000000000 ) ) ;
#8515 = EDGE_LOOP ( 'NONE', ( #13883, #6267, #57039, #64298 ) ) ;
#8516 = ORIENTED_EDGE ( 'NONE', *, *, #59187, .F. ) ;
#8517 = CARTESIAN_POINT ( 'NONE',  ( 9.900000000000000355, 18.00000000000000355, -21.00000000000000000 ) ) ;
#8518 = VECTOR ( 'NONE', #53680, 1000.000000000000000 ) ;
#8519 = CARTESIAN_POINT ( 'NONE',  ( 30.00000000000000000, -9.454754784057099570, -17.53999999999999915 ) ) ;
#8520 = ORIENTED_EDGE ( 'NONE', *, *, #45954, .T. ) ;
#8521 = PRESENTATION_LAYER_ASSIGNMENT (  '', '', ( #14134 ) ) ;
#8522 = DIRECTION ( 'NONE',  ( 1.000000000000000000, 0.000000000000000000, 0.000000000000000000 ) ) ;
#8523 = FACE_OUTER_BOUND ( 'NONE', #4381, .T. ) ;
#8525 = ORIENTED_EDGE ( 'NONE', *, *, #53658, .F. ) ;
#8524 =( LENGTH_UNIT ( ) NAMED_UNIT ( * ) SI_UNIT ( .MILLI., .METRE. ) );
#8526 = ORIENTED_EDGE ( 'NONE', *, *, #51003, .F. ) ;
#8527 = DIRECTION ( 'NONE',  ( 0.000000000000000000, 0.000000000000000000, -1.000000000000000000 ) ) ;
#8528 = ADVANCED_FACE ( 'NONE', ( #50267 ), #38293, .F. ) ;
#8529 = DIRECTION ( 'NONE',  ( 0.000000000000000000, 0.000000000000000000, 1.000000000000000000 ) ) ;
#8530 = LINE ( 'NONE', #48133, #15470 ) ;
#8531 = DIRECTION ( 'NONE',  ( -1.000000000000000000, 0.000000000000000000, 0.000000000000000000 ) ) ;
#8532 = CARTESIAN_POINT ( 'NONE',  ( -8.393516549646792058, -7.616533956692236096, 455.0000000000000568 ) ) ;
#8533 = EDGE_CURVE ( 'NONE', #67686, #22473, #61205, .T. ) ;
#8534 = CARTESIAN_POINT ( 'NONE',  ( 7.749999999999998224, -7.348062532928000934, -5.000000000000000000 ) ) ;
#8535 = VERTEX_POINT ( 'NONE', #65168 ) ;
#8536 = DIRECTION ( 'NONE',  ( 0.000000000000000000, -0.000000000000000000, 1.000000000000000000 ) ) ;
#8538 = VERTEX_POINT ( 'NONE', #43922 ) ;
#8537 = CARTESIAN_POINT ( 'NONE',  ( 6.364920264886885448, -6.836383711243011696, 26.00000000000000000 ) ) ;
#8539 = DIRECTION ( 'NONE',  ( -0.000000000000000000, -0.000000000000000000, -1.000000000000000000 ) ) ;
#8540 = DIRECTION ( 'NONE',  ( 0.000000000000000000, 0.000000000000000000, 1.000000000000000000 ) ) ;
#8541 = ADVANCED_FACE ( 'NONE', ( #33994 ), #66186, .F. ) ;
#8542 = AXIS2_PLACEMENT_3D ( 'NONE', #58207, #26040, #47597 ) ;
#8543 = CARTESIAN_POINT ( 'NONE',  ( 283.0000000000000568, -30.45000000000000639, 15.00000000000000000 ) ) ;
#8544 = LINE ( 'NONE', #3254, #32968 ) ;
#8545 = DIRECTION ( 'NONE',  ( -1.000000000000000000, 0.000000000000000000, 0.000000000000000000 ) ) ;
#8546 = CIRCLE ( 'NONE', #48100, 0.5000000000079362072 ) ;
#8547 = EDGE_LOOP ( 'NONE', ( #7322, #54692, #12201, #21917 ) ) ;
#8548 = DIRECTION ( 'NONE',  ( -0.7142857142857395036, 0.000000000000000000, -0.6998542122237394469 ) ) ;
#8549 = DIRECTION ( 'NONE',  ( 0.000000000000000000, -0.7071067811865474617, 0.7071067811865474617 ) ) ;
#8550 = EDGE_CURVE ( 'NONE', #64676, #64879, #54902, .T. ) ;
#8551 = EDGE_LOOP ( 'NONE', ( #66177, #48081 ) ) ;
#8552 = AXIS2_PLACEMENT_3D ( 'NONE', #10145, #53988, #58235 ) ;
#8553 = FACE_OUTER_BOUND ( 'NONE', #39527, .T. ) ;
#8554 = AXIS2_PLACEMENT_3D ( 'NONE', #14619, #24882, #35837 ) ;
#8555 = VECTOR ( 'NONE', #53976, 1000.000000000000000 ) ;
#8556 = VECTOR ( 'NONE', #38960, 1000.000000000000000 ) ;
#8557 = DIRECTION ( 'NONE',  ( -1.000000000000000000, -0.000000000000000000, -0.000000000000000000 ) ) ;
#8558 = VERTEX_POINT ( 'NONE', #1147 ) ;
#8559 = ADVANCED_FACE ( 'NONE', ( #17749 ), #65502, .F. ) ;
#8560 = CARTESIAN_POINT ( 'NONE',  ( -7.259684009079930611, 7.798499376343971612, 455.0000000000000568 ) ) ;
#8561 = ORIENTED_EDGE ( 'NONE', *, *, #26984, .T. ) ;
#8562 = ORIENTED_EDGE ( 'NONE', *, *, #14633, .F. ) ;
#8563 = LINE ( 'NONE', #50656, #26810 ) ;
#8565 = DIRECTION ( 'NONE',  ( -1.836970198721029934E-16, 1.836970198721036590E-16, -1.000000000000000000 ) ) ;
#8564 = CIRCLE ( 'NONE', #46987, 0.1999999999999987899 ) ;
#8566 = CIRCLE ( 'NONE', #61664, 24.99999999998794920 ) ;
#8567 = CARTESIAN_POINT ( 'NONE',  ( -10.91351654964666373, -2.706483450353290632, 195.0000000000000284 ) ) ;
#8568 = CIRCLE ( 'NONE', #15412, 0.7500000000000006661 ) ;
#8569 = CARTESIAN_POINT ( 'NONE',  ( 25.50000000000000355, -15.50000000000000000, -20.49999999999999645 ) ) ;
#8570 = LINE ( 'NONE', #47458, #18196 ) ;
#8571 = VERTEX_POINT ( 'NONE', #39314 ) ;
#8572 = EDGE_CURVE ( 'NONE', #33487, #51627, #47497, .T. ) ;
#8573 = VERTEX_POINT ( 'NONE', #27669 ) ;
#8575 = ORIENTED_EDGE ( 'NONE', *, *, #50576, .F. ) ;
#8574 = DIRECTION ( 'NONE',  ( 0.000000000000000000, 0.000000000000000000, 1.000000000000000000 ) ) ;
#8577 = ORIENTED_EDGE ( 'NONE', *, *, #43183, .F. ) ;
#8576 = EDGE_CURVE ( 'NONE', #67636, #62094, #30537, .T. ) ;
#8578 = PRODUCT ( 'Actuator  Carriage Assembly', 'Actuator  Carriage Assembly', '', ( #40601 ) ) ;
#8579 = AXIS2_PLACEMENT_3D ( 'NONE', #33691, #29085, #66563 ) ;
#8580 = CARTESIAN_POINT ( 'NONE',  ( 10.31452373788277654, 3.650476262117150483, 26.00000000000000711 ) ) ;
#8581 = DIRECTION ( 'NONE',  ( 0.000000000000000000, 1.000000000000000000, 0.000000000000000000 ) ) ;
#8582 = CARTESIAN_POINT ( 'NONE',  ( 30.00000000000000000, -8.959999999999999076, 17.04524521594300523 ) ) ;
#8583 = FACE_BOUND ( 'NONE', #35696, .T. ) ;
#8584 = AXIS2_PLACEMENT_3D ( 'NONE', #57255, #53020, #8818 ) ;
#8585 = CARTESIAN_POINT ( 'NONE',  ( 0.5000000000000000000, -42.00000000000000000, 27.00000000000000000 ) ) ;
#8586 = DIRECTION ( 'NONE',  ( -0.5773502691896257311, -0.5773502691896257311, 0.5773502691896257311 ) ) ;
#8587 = VERTEX_POINT ( 'NONE', #32974 ) ;
#8588 = EDGE_CURVE ( 'NONE', #7713, #31930, #21501, .T. ) ;
#8589 = EDGE_LOOP ( 'NONE', ( #18182, #24753, #28771, #60524 ) ) ;
#8590 = ORIENTED_EDGE ( 'NONE', *, *, #56994, .F. ) ;
#8591 = ORIENTED_EDGE ( 'NONE', *, *, #46172, .T. ) ;
#8592 = CARTESIAN_POINT ( 'NONE',  ( 289.7500000000000000, -0.2499999999999944766, 26.75000000000000000 ) ) ;
#8593 = DIRECTION ( 'NONE',  ( -0.000000000000000000, 3.673940397442059868E-16, -1.000000000000000000 ) ) ;
#8594 = CARTESIAN_POINT ( 'NONE',  ( -15.91434062215689060, -0.3156604612129251808, 23.70415600323552852 ) ) ;
#8595 = ORIENTED_EDGE ( 'NONE', *, *, #6160, .F. ) ;
#8596 = EDGE_LOOP ( 'NONE', ( #50610, #48439, #27548, #68368 ) ) ;
#8597 = VECTOR ( 'NONE', #66554, 1000.000000000000000 ) ;
#8598 = ORIENTED_EDGE ( 'NONE', *, *, #44019, .T. ) ;
#8599 = FACE_OUTER_BOUND ( 'NONE', #23475, .T. ) ;
#8600 = ORIENTED_EDGE ( 'NONE', *, *, #69921, .F. ) ;
#8601 = VECTOR ( 'NONE', #37727, 1000.000000000000000 ) ;
#8602 = VERTEX_POINT ( 'NONE', #23045 ) ;
#8603 = LINE ( 'NONE', #25590, #57070 ) ;
#8604 = ORIENTED_EDGE ( 'NONE', *, *, #50935, .T. ) ;
#8605 = EDGE_CURVE ( 'NONE', #12591, #51101, #17391, .T. ) ;
#8606 = ORIENTED_EDGE ( 'NONE', *, *, #44467, .T. ) ;
#8607 = VECTOR ( 'NONE', #22751, 1000.000000000000114 ) ;
#8608 = FACE_OUTER_BOUND ( 'NONE', #58835, .T. ) ;
#8610 = ORIENTED_EDGE ( 'NONE', *, *, #68341, .T. ) ;
#8609 = LINE ( 'NONE', #35474, #65012 ) ;
#8611 = EDGE_LOOP ( 'NONE', ( #40784, #57202, #37961, #42521 ) ) ;
#8612 = EDGE_CURVE ( 'NONE', #11541, #2395, #64672, .T. ) ;
#8613 = PLANE ( 'NONE',  #19885 ) ;
#8614 = VECTOR ( 'NONE', #43593, 1000.000000000000000 ) ;
#8615 = AXIS2_PLACEMENT_3D ( 'NONE', #54842, #28640, #61157 ) ;
#8616 = CIRCLE ( 'NONE', #57172, 0.1999999999999987899 ) ;
#8617 = CARTESIAN_POINT ( 'NONE',  ( -25.50000000000000355, 0.000000000000000000, -24.75000000000000000 ) ) ;
#8618 = DIRECTION ( 'NONE',  ( 0.000000000000000000, 0.000000000000000000, -1.000000000000000000 ) ) ;
#8619 = ADVANCED_FACE ( 'NONE', ( #60869 ), #12417, .F. ) ;
#8621 = VERTEX_POINT ( 'NONE', #39646 ) ;
#8620 = LINE ( 'NONE', #57056, #14353 ) ;
#8622 = ORIENTED_EDGE ( 'NONE', *, *, #1585, .F. ) ;
#8623 = VECTOR ( 'NONE', #29750, 1000.000000000000114 ) ;
#8624 = CARTESIAN_POINT ( 'NONE',  ( 12.00648345035338060, -7.826483450353395988, 195.0000000000000284 ) ) ;
#8625 = AXIS2_PLACEMENT_3D ( 'NONE', #17729, #33643, #61184 ) ;
#8626 = ADVANCED_FACE ( 'NONE', ( #34330 ), #7474, .F. ) ;
#8627 = CARTESIAN_POINT ( 'NONE',  ( -11.00000000000000000, -15.97213595500069871, -14.50000000000000000 ) ) ;
#8628 = PLANE ( 'NONE',  #7504 ) ;
#8629 = CARTESIAN_POINT ( 'NONE',  ( -7.259684009080030975, -7.811466277050769236, 455.0000000000000568 ) ) ;
#8630 = AXIS2_PLACEMENT_3D ( 'NONE', #30366, #40961, #67138 ) ;
#8631 = EDGE_CURVE ( 'NONE', #4384, #62416, #11736, .T. ) ;
#8632 = ORIENTED_EDGE ( 'NONE', *, *, #13805, .F. ) ;
#8633 = DIRECTION ( 'NONE',  ( 0.000000000000000000, 3.673940397442059868E-16, -1.000000000000000000 ) ) ;
#8634 = VECTOR ( 'NONE', #31269, 1000.000000000000114 ) ;
#8635 = DIRECTION ( 'NONE',  ( 0.000000000000000000, 1.000000000000000000, 0.000000000000000000 ) ) ;
#8636 = CARTESIAN_POINT ( 'NONE',  ( 7.000000000000000000, -20.40000000000000213, -12.40000000000000213 ) ) ;
#8637 = VERTEX_POINT ( 'NONE', #35384 ) ;
#8638 = EDGE_CURVE ( 'NONE', #61820, #63196, #3584, .T. ) ;
#8639 = CARTESIAN_POINT ( 'NONE',  ( -11.07551654964667520, 9.791916549646639822, 195.0000000000000284 ) ) ;
#8640 = ADVANCED_FACE ( 'NONE', ( #39981 ), #2178, .F. ) ;
#8641 = FACE_OUTER_BOUND ( 'NONE', #61846, .T. ) ;
#8642 = FACE_OUTER_BOUND ( 'NONE', #39029, .T. ) ;
#8643 = EDGE_CURVE ( 'NONE', #34571, #15298, #56956, .T. ) ;
#8644 = EDGE_CURVE ( 'NONE', #17879, #42683, #41402, .T. ) ;
#8645 = VERTEX_POINT ( 'NONE', #8517 ) ;
#8646 = CARTESIAN_POINT ( 'NONE',  ( 7.272650909786554152, 4.188533722949247640, 195.0000000000000284 ) ) ;
#8647 = CARTESIAN_POINT ( 'NONE',  ( 41.09999999999999432, 20.60000000000000142, 13.86939075806900057 ) ) ;
#8648 = EDGE_CURVE ( 'NONE', #5578, #27416, #56619, .T. ) ;
#8649 = CARTESIAN_POINT ( 'NONE',  ( 275.0000000000000000, -23.70411739045900390, -12.50000000000000000 ) ) ;
#8650 = ORIENTED_EDGE ( 'NONE', *, *, #11174, .T. ) ;
#8651 = CARTESIAN_POINT ( 'NONE',  ( 10.62249899919920004, -25.00000000000000000, -17.50000000000000000 ) ) ;
#8652 = DIRECTION ( 'NONE',  ( -1.000000000000000000, 0.000000000000000000, 0.000000000000000000 ) ) ;
#8653 = CIRCLE ( 'NONE', #44769, 24.99999999998784972 ) ;
#8654 = LINE ( 'NONE', #24576, #56772 ) ;
#8655 = DIRECTION ( 'NONE',  ( 0.000000000000000000, 0.000000000000000000, -1.000000000000000000 ) ) ;
#8656 = DIRECTION ( 'NONE',  ( 0.000000000000000000, 0.000000000000000000, 1.000000000000000000 ) ) ;
#8657 = ORIENTED_EDGE ( 'NONE', *, *, #50945, .F. ) ;
#8658 = CARTESIAN_POINT ( 'NONE',  ( -2.893516549646675706, 10.91351654964657669, 455.0000000000000568 ) ) ;
#8659 = CARTESIAN_POINT ( 'NONE',  ( 50.83090410532631864, 3.657408540445007628, 10.00000000000000000 ) ) ;
#8660 = AXIS2_PLACEMENT_3D ( 'NONE', #59563, #28076, #53566 ) ;
#8661 = LINE ( 'NONE', #45788, #34530 ) ;
#8662 = AXIS2_PLACEMENT_3D ( 'NONE', #56549, #7755, #61487 ) ;
#8663 = CIRCLE ( 'NONE', #15438, 2.215251240775983899 ) ;
#8664 = DIRECTION ( 'NONE',  ( -0.7071067811865474617, -0.7071067811865474617, 0.000000000000000000 ) ) ;
#8665 = CARTESIAN_POINT ( 'NONE',  ( 25.57999999999999829, 3.010794155703768650E-16, -2.458500000000000796 ) ) ;
#8666 = EDGE_CURVE ( 'NONE', #34716, #47806, #35266, .T. ) ;
#8667 = ORIENTED_EDGE ( 'NONE', *, *, #47840, .T. ) ;
#8669 = VERTEX_POINT ( 'NONE', #8168 ) ;
#8668 = LINE ( 'NONE', #41184, #17062 ) ;
#8670 = EDGE_CURVE ( 'NONE', #12490, #21729, #68280, .T. ) ;
#8671 = AXIS2_PLACEMENT_3D ( 'NONE', #34115, #7242, #50391 ) ;
#8672 = CIRCLE ( 'NONE', #6407, 0.1999999999999987899 ) ;
#8673 = DIRECTION ( 'NONE',  ( 1.000000000000000000, 0.000000000000000000, 0.000000000000000000 ) ) ;
#8674 = LINE ( 'NONE', #26336, #62766 ) ;
#8675 = CARTESIAN_POINT ( 'NONE',  ( 4.396432944014527777, -8.406483450353478659, 455.0000000000000568 ) ) ;
#8676 = ORIENTED_EDGE ( 'NONE', *, *, #42746, .F. ) ;
#8677 = VECTOR ( 'NONE', #47772, 1000.000000000000000 ) ;
#8678 = VECTOR ( 'NONE', #14782, 1000.000000000000000 ) ;
#8679 = DIRECTION ( 'NONE',  ( 1.000000000000000000, 0.000000000000000000, 0.000000000000000000 ) ) ;
#8680 = EDGE_LOOP ( 'NONE', ( #33374, #4377, #6761, #10881 ) ) ;
#8681 = VECTOR ( 'NONE', #9059, 1000.000000000000114 ) ;
#8682 = ORIENTED_EDGE ( 'NONE', *, *, #54108, .F. ) ;
#8683 = ORIENTED_EDGE ( 'NONE', *, *, #67515, .F. ) ;
#8684 = FACE_OUTER_BOUND ( 'NONE', #11055, .T. ) ;
#8685 = LINE ( 'NONE', #14689, #62509 ) ;
#8686 = DIRECTION ( 'NONE',  ( 1.000000000000000000, 0.000000000000000000, 0.000000000000000000 ) ) ;
#8687 = CARTESIAN_POINT ( 'NONE',  ( -9.781776262117313436, -9.795823737882745519, 54.00000000000000711 ) ) ;
#8688 = CIRCLE ( 'NONE', #22228, 4.500000000000191847 ) ;
#8689 = ORIENTED_EDGE ( 'NONE', *, *, #61233, .F. ) ;
#8690 = ORIENTED_EDGE ( 'NONE', *, *, #38049, .F. ) ;
#8691 = DIRECTION ( 'NONE',  ( -1.000000000000000000, 0.000000000000000000, 0.000000000000000000 ) ) ;
#8692 = DIRECTION ( 'NONE',  ( -1.000000000000000000, 0.000000000000000000, 0.000000000000000000 ) ) ;
#8693 = EDGE_LOOP ( 'NONE', ( #38367, #32430, #7376, #60810 ) ) ;
#8694 = ORIENTED_EDGE ( 'NONE', *, *, #57895, .F. ) ;
#8695 = ORIENTED_EDGE ( 'NONE', *, *, #25340, .T. ) ;
#8696 = ORIENTED_EDGE ( 'NONE', *, *, #48703, .F. ) ;
#8697 = DIRECTION ( 'NONE',  ( -1.000000000000000000, 3.491481338843133355E-15, 1.836970198721036344E-16 ) ) ;
#8699 = VERTEX_POINT ( 'NONE', #14533 ) ;
#8698 = CARTESIAN_POINT ( 'NONE',  ( 282.6457513110646005, -20.50000000000000000, 17.00000000000000000 ) ) ;
#8700 = EDGE_CURVE ( 'NONE', #14045, #40926, #51672, .T. ) ;
#8701 = CARTESIAN_POINT ( 'NONE',  ( 8.250000000000005329, -7.249999999999998224, -11.00000000000000000 ) ) ;
#8702 = DIRECTION ( 'NONE',  ( 0.000000000000000000, 1.000000000000000000, 0.000000000000000000 ) ) ;
#8703 = AXIS2_PLACEMENT_3D ( 'NONE', #58668, #10222, #31802 ) ;
#8704 = EDGE_LOOP ( 'NONE', ( #35944, #35427, #7364, #49048, #60616, #64898, #11915, #60921, #50079, #37427, #48515, #36675, #16470, #46376, #23361, #50711 ) ) ;
#8705 = EDGE_CURVE ( 'NONE', #40067, #43546, #56268, .T. ) ;
#8706 = ORIENTED_EDGE ( 'NONE', *, *, #54384, .T. ) ;
#8707 = ADVANCED_FACE ( 'NONE', ( #51309, #24087 ), #25146, .F. ) ;
#8708 = ADVANCED_FACE ( 'NONE', ( #19831 ), #57667, .T. ) ;
#8709 = CYLINDRICAL_SURFACE ( 'NONE', #11204, 25.39999999999999858 ) ;
#8710 = CARTESIAN_POINT ( 'NONE',  ( 283.0000000000000568, -32.95000000000000284, -13.19999999999999929 ) ) ;
#8711 = VECTOR ( 'NONE', #49771, 1000.000000000000000 ) ;
#8712 = AXIS2_PLACEMENT_3D ( 'NONE', #9868, #30722, #41319 ) ;
#8713 = EDGE_CURVE ( 'NONE', #3514, #17105, #2869, .T. ) ;
#8714 = ADVANCED_FACE ( 'NONE', ( #34693, #41050, #9236, #66867, #14181 ), #46011, .T. ) ;
#8715 = CARTESIAN_POINT ( 'NONE',  ( -9.828310488886053520, 2.277516549646603661, 195.0000000000000284 ) ) ;
#8716 = AXIS2_PLACEMENT_3D ( 'NONE', #57362, #8915, #45691 ) ;
#8717 = AXIS2_PLACEMENT_3D ( 'NONE', #43681, #16810, #6192 ) ;
#8718 = DIRECTION ( 'NONE',  ( 0.4285714285711678118, 0.000000000000000000, 0.9035079029053749711 ) ) ;
#8719 = CARTESIAN_POINT ( 'NONE',  ( 1.480523737882788238, -9.404523737882794165, 54.00000000000000711 ) ) ;
#8721 = ORIENTED_EDGE ( 'NONE', *, *, #46386, .F. ) ;
#8720 = DIRECTION ( 'NONE',  ( 1.000000000000000000, -0.000000000000000000, 0.000000000000000000 ) ) ;
#8722 = VERTEX_POINT ( 'NONE', #45643 ) ;
#8723 = CARTESIAN_POINT ( 'NONE',  ( 39.00000000000000000, 14.08845687959340331, 21.00000000000000000 ) ) ;
#8724 = CARTESIAN_POINT ( 'NONE',  ( 1.090483450353338268, -11.34648345035345329, 455.0000000000000568 ) ) ;
#8725 = CIRCLE ( 'NONE', #57282, 0.1999999999999996503 ) ;
#8726 = AXIS2_PLACEMENT_3D ( 'NONE', #41725, #62237, #36426 ) ;
#8727 = CARTESIAN_POINT ( 'NONE',  ( 29.89999999999999858, -14.06939075806900874, 20.80000000000001137 ) ) ;
#8728 = DIRECTION ( 'NONE',  ( 0.000000000000000000, 0.7278708115913771204, 0.6857142857147648929 ) ) ;
#8729 = CARTESIAN_POINT ( 'NONE',  ( 2.544523737882812942, 9.722976262117210666, 26.00000000000000711 ) ) ;
#8730 = ORIENTED_EDGE ( 'NONE', *, *, #35927, .T. ) ;
#8731 = LINE ( 'NONE', #35583, #4191 ) ;
#8732 = CARTESIAN_POINT ( 'NONE',  ( 48.50000000000000000, 0.000000000000000000, 0.000000000000000000 ) ) ;
#8733 = CARTESIAN_POINT ( 'NONE',  ( -30.00000000000000000, -17.50000000000000000, 26.64999999999999858 ) ) ;
#8734 = DIRECTION ( 'NONE',  ( 0.000000000000000000, 1.000000000000000000, 0.000000000000000000 ) ) ;
#8735 = VECTOR ( 'NONE', #9876, 1000.000000000000000 ) ;
#8736 = CARTESIAN_POINT ( 'NONE',  ( -28.00000000000000000, -16.64230188589299786, 14.64519951917100116 ) ) ;
#8737 = DIRECTION ( 'NONE',  ( 0.000000000000000000, -1.000000000000000000, 0.000000000000000000 ) ) ;
#8738 = DIRECTION ( 'NONE',  ( -1.000000000000000000, 0.000000000000000000, 0.000000000000000000 ) ) ;
#8739 = ORIENTED_EDGE ( 'NONE', *, *, #37552, .T. ) ;
#8740 = DIRECTION ( 'NONE',  ( -1.000000000000000000, 0.000000000000000000, 0.000000000000000000 ) ) ;
#8741 = LINE ( 'NONE', #13689, #27089 ) ;
#8742 = EDGE_LOOP ( 'NONE', ( #26271, #7456, #15910, #38300, #43490, #29809, #18499 ) ) ;
#8743 = DIRECTION ( 'NONE',  ( 0.000000000000000000, 0.000000000000000000, 1.000000000000000000 ) ) ;
#8744 = CARTESIAN_POINT ( 'NONE',  ( 75.42576880091937142, 0.000000000000000000, 285.9830310981789125 ) ) ;
#8745 = LINE ( 'NONE', #4158, #53603 ) ;
#8746 = CARTESIAN_POINT ( 'NONE',  ( 10.00000000000000000, -18.00000000000000355, 21.00000000000000000 ) ) ;
#8747 = CARTESIAN_POINT ( 'NONE',  ( -6.486996718459931088, 3.142976262117182173, 54.00000000000000711 ) ) ;
#8748 = ORIENTED_EDGE ( 'NONE', *, *, #69075, .T. ) ;
#8749 = DIRECTION ( 'NONE',  ( 1.000000000000000000, 0.000000000000000000, 0.000000000000000000 ) ) ;
#8750 = EDGE_CURVE ( 'NONE', #23746, #67816, #62264, .T. ) ;
#8751 = ORIENTED_EDGE ( 'NONE', *, *, #53520, .F. ) ;
#8752 = CARTESIAN_POINT ( 'NONE',  ( 8.900000000000005684, -0.1999999999911795112, 8.826273045769999343E-12 ) ) ;
#8753 = FACE_OUTER_BOUND ( 'NONE', #68269, .T. ) ;
#8754 = AXIS2_PLACEMENT_3D ( 'NONE', #65867, #44631, #27012 ) ;
#8755 = ORIENTED_EDGE ( 'NONE', *, *, #39297, .T. ) ;
#8756 = EDGE_CURVE ( 'NONE', #2123, #59802, #18786, .T. ) ;
#8757 = FACE_OUTER_BOUND ( 'NONE', #45641, .T. ) ;
#8758 = ORIENTED_EDGE ( 'NONE', *, *, #16929, .T. ) ;
#8759 = CIRCLE ( 'NONE', #43747, 0.2000000000000005107 ) ;
#8760 = CIRCLE ( 'NONE', #35870, 5.000000000000000000 ) ;
#8761 = LINE ( 'NONE', #3112, #24372 ) ;
#8762 = ORIENTED_EDGE ( 'NONE', *, *, #12600, .T. ) ;
#8763 = VERTEX_POINT ( 'NONE', #47066 ) ;
#8764 = DIRECTION ( 'NONE',  ( 1.836970198721029934E-16, 1.836970198721010706E-16, -1.000000000000000000 ) ) ;
#8765 = VERTEX_POINT ( 'NONE', #4298 ) ;
#8766 = ORIENTED_EDGE ( 'NONE', *, *, #39432, .T. ) ;
#8767 = CIRCLE ( 'NONE', #32507, 3.999999999999993339 ) ;
#8768 = VECTOR ( 'NONE', #32637, 1000.000000000000000 ) ;
#8769 = FACE_OUTER_BOUND ( 'NONE', #59374, .T. ) ;
#8770 = DIRECTION ( 'NONE',  ( 1.000000000000000000, 0.000000000000000000, 0.000000000000000000 ) ) ;
#8771 = DIRECTION ( 'NONE',  ( -1.794541526872559352E-16, -1.000000000000000000, 0.000000000000000000 ) ) ;
#8772 = ORIENTED_EDGE ( 'NONE', *, *, #11300, .T. ) ;
#8773 = CYLINDRICAL_SURFACE ( 'NONE', #62889, 0.2000000000000000944 ) ;
#8774 = VECTOR ( 'NONE', #55260, 1000.000000000000000 ) ;
#8775 = AXIS2_PLACEMENT_3D ( 'NONE', #5567, #20424, #10862 ) ;
#8777 = DIRECTION ( 'NONE',  ( 0.000000000000000000, 0.000000000000000000, -1.000000000000000000 ) ) ;
#8776 = PLANE ( 'NONE',  #69970 ) ;
#8778 = ORIENTED_EDGE ( 'NONE', *, *, #42655, .T. ) ;
#8780 = ORIENTED_EDGE ( 'NONE', *, *, #13491, .F. ) ;
#8779 = DIRECTION ( 'NONE',  ( 1.000000000000000000, -0.000000000000000000, 0.000000000000000000 ) ) ;
#8781 = ORIENTED_EDGE ( 'NONE', *, *, #20057, .T. ) ;
#8782 = PRODUCT_CONTEXT ( 'NONE', #2010, 'mechanical' ) ;
#8783 = DIRECTION ( 'NONE',  ( 1.836970198721029934E-16, 1.836970198721010706E-16, -1.000000000000000000 ) ) ;
#8785 = ORIENTED_EDGE ( 'NONE', *, *, #47251, .F. ) ;
#8784 = CARTESIAN_POINT ( 'NONE',  ( 39.00000000000000000, 21.00000000000000000, 13.98999642601811999 ) ) ;
#8786 = VECTOR ( 'NONE', #56118, 1000.000000000000000 ) ;
#8787 = EDGE_CURVE ( 'NONE', #1825, #64092, #25151, .T. ) ;
#8788 = LINE ( 'NONE', #45550, #41584 ) ;
#8789 = CARTESIAN_POINT ( 'NONE',  ( 10.00000000000000000, 18.00000000000000355, 21.00000000000000000 ) ) ;
#8790 = VERTEX_POINT ( 'NONE', #10282 ) ;
#8791 = ORIENTED_EDGE ( 'NONE', *, *, #2316, .T. ) ;
#8792 = EDGE_CURVE ( 'NONE', #4531, #32705, #56734, .T. ) ;
#8793 = CARTESIAN_POINT ( 'NONE',  ( 41.09999999999999432, 13.66939075806899950, -20.80000000000000426 ) ) ;
#8794 = EDGE_CURVE ( 'NONE', #41582, #15537, #47754, .T. ) ;
#8795 = EDGE_CURVE ( 'NONE', #61811, #22725, #48115, .T. ) ;
#8796 = EDGE_LOOP ( 'NONE', ( #7128, #12540, #18429, #32700, #15017 ) ) ;
#8797 = LINE ( 'NONE', #13742, #59070 ) ;
#8798 = PLANE ( 'NONE',  #9812 ) ;
#8799 = EDGE_CURVE ( 'NONE', #25281, #40029, #45469, .T. ) ;
#8800 = DIRECTION ( 'NONE',  ( 0.000000000000000000, 0.000000000000000000, 1.000000000000000000 ) ) ;
#8801 = EDGE_CURVE ( 'NONE', #34713, #3293, #68638, .T. ) ;
#8802 = VERTEX_POINT ( 'NONE', #9584 ) ;
#8803 = EDGE_CURVE ( 'NONE', #17833, #51724, #20649, .T. ) ;
#8804 = LINE ( 'NONE', #62899, #6456 ) ;
#8805 = CARTESIAN_POINT ( 'NONE',  ( 283.0000000000000568, -20.85424868893542083, 17.35424868893542083 ) ) ;
#8807 = ORIENTED_EDGE ( 'NONE', *, *, #24679, .T. ) ;
#8806 = DIRECTION ( 'NONE',  ( 0.000000000000000000, 0.000000000000000000, 1.000000000000000000 ) ) ;
#8809 = ORIENTED_EDGE ( 'NONE', *, *, #12390, .F. ) ;
#8808 = DIRECTION ( 'NONE',  ( -1.000000000000000000, 0.000000000000000000, 0.000000000000000000 ) ) ;
#8810 = LINE ( 'NONE', #66793, #64521 ) ;
#8811 = DIRECTION ( 'NONE',  ( 0.000000000000000000, 1.000000000000000000, 0.000000000000000000 ) ) ;
#8812 = CARTESIAN_POINT ( 'NONE',  ( -7.250000000000001776, -7.249999999999998224, -24.00000000000000000 ) ) ;
#8813 = CARTESIAN_POINT ( 'NONE',  ( -25.50000000000000355, -17.50000000000000000, -25.99999999999985079 ) ) ;
#8814 = DIRECTION ( 'NONE',  ( -0.000000000000000000, 1.000000000000000000, -0.000000000000000000 ) ) ;
#8815 = ORIENTED_EDGE ( 'NONE', *, *, #19497, .F. ) ;
#8816 = DIRECTION ( 'NONE',  ( 0.000000000000000000, 0.000000000000000000, 1.000000000000000000 ) ) ;
#8817 = CARTESIAN_POINT ( 'NONE',  ( -2.893516549646820035, -10.09643294401462654, 455.0000000000000568 ) ) ;
#8818 = DIRECTION ( 'NONE',  ( -1.000000000000000000, 0.000000000000000000, 0.000000000000000000 ) ) ;
#8819 = VECTOR ( 'NONE', #67548, 1000.000000000000000 ) ;
#8821 = ORIENTED_EDGE ( 'NONE', *, *, #66951, .F. ) ;
#8820 = DIRECTION ( 'NONE',  ( 0.000000000000000000, 0.000000000000000000, -1.000000000000000000 ) ) ;
#8822 = DIRECTION ( 'NONE',  ( -0.000000000000000000, 3.673940397442059868E-16, -1.000000000000000000 ) ) ;
#8823 = CARTESIAN_POINT ( 'NONE',  ( 41.09999999999999432, 13.66939075806899950, 20.80000000000000426 ) ) ;
#8824 = VECTOR ( 'NONE', #9747, 1000.000000000000114 ) ;
#8825 = ORIENTED_EDGE ( 'NONE', *, *, #57844, .F. ) ;
#8826 = DIRECTION ( 'NONE',  ( 0.000000000000000000, 0.000000000000000000, 1.000000000000000000 ) ) ;
#8827 = DIRECTION ( 'NONE',  ( 1.000000000000000000, -6.308085367188447236E-15, -2.317552966102676720E-30 ) ) ;
#8828 = ORIENTED_EDGE ( 'NONE', *, *, #8062, .T. ) ;
#8829 = DIRECTION ( 'NONE',  ( 0.000000000000000000, 0.000000000000000000, -1.000000000000000000 ) ) ;
#8830 = DIRECTION ( 'NONE',  ( 1.000000000000000000, 0.000000000000000000, -0.000000000000000000 ) ) ;
#8831 = PLANE ( 'NONE',  #14 ) ;
#8832 = AXIS2_PLACEMENT_3D ( 'NONE', #6890, #18905, #45769 ) ;
#8833 = DIRECTION ( 'NONE',  ( 1.000000000000000000, -0.000000000000000000, -0.000000000000000000 ) ) ;
#8834 = VERTEX_POINT ( 'NONE', #26199 ) ;
#8835 = LINE ( 'NONE', #67889, #33750 ) ;
#8836 = ORIENTED_EDGE ( 'NONE', *, *, #65005, .T. ) ;
#8837 = DIRECTION ( 'NONE',  ( 0.000000000000000000, 0.000000000000000000, 1.000000000000000000 ) ) ;
#8838 = ORIENTED_EDGE ( 'NONE', *, *, #69950, .T. ) ;
#8839 = ADVANCED_FACE ( 'NONE', ( #53776 ), #41749, .T. ) ;
#8840 = EDGE_CURVE ( 'NONE', #59731, #27989, #36817, .T. ) ;
#8841 = DIRECTION ( 'NONE',  ( -8.994862468027880808E-15, 0.000000000000000000, -1.000000000000000000 ) ) ;
#8842 = ADVANCED_FACE ( 'NONE', ( #26903 ), #30, .T. ) ;
#8843 = EDGE_CURVE ( 'NONE', #29771, #22437, #14893, .T. ) ;
#8844 = LINE ( 'NONE', #4946, #62625 ) ;
#8845 = DIRECTION ( 'NONE',  ( -1.000000000000000000, 0.000000000000000000, 0.000000000000000000 ) ) ;
#8846 = ORIENTED_EDGE ( 'NONE', *, *, #40456, .T. ) ;
#8847 = ORIENTED_EDGE ( 'NONE', *, *, #13767, .T. ) ;
#8848 = DIRECTION ( 'NONE',  ( 0.000000000000000000, 0.000000000000000000, 1.000000000000000000 ) ) ;
#8849 = ORIENTED_EDGE ( 'NONE', *, *, #56069, .T. ) ;
#8850 = ORIENTED_EDGE ( 'NONE', *, *, #52435, .F. ) ;
#8851 = FACE_OUTER_BOUND ( 'NONE', #69820, .T. ) ;
#8852 = PLANE ( 'NONE',  #57231 ) ;
#8853 = CARTESIAN_POINT ( 'NONE',  ( -9.547976262117304103, -7.969523737882760805, 54.00000000000000711 ) ) ;
#8854 = CARTESIAN_POINT ( 'NONE',  ( -11.77351654964674310, -4.406483450353321452, 455.0000000000000568 ) ) ;
#8855 = ORIENTED_EDGE ( 'NONE', *, *, #59425, .F. ) ;
#8856 = DIRECTION ( 'NONE',  ( 1.000000000000000000, -0.000000000000000000, 0.000000000000000000 ) ) ;
#8858 = DIRECTION ( 'NONE',  ( -4.336808689942025625E-15, -1.000000000000000000, 0.000000000000000000 ) ) ;
#8857 = CARTESIAN_POINT ( 'NONE',  ( -7.517976262117288755, -6.665817930929256008, 26.00000000000000000 ) ) ;
#8859 = VERTEX_POINT ( 'NONE', #42102 ) ;
#8861 = ORIENTED_EDGE ( 'NONE', *, *, #6285, .F. ) ;
#8860 = CARTESIAN_POINT ( 'NONE',  ( -6.835476262117330393, -10.50702373788278265, 26.00000000000000000 ) ) ;
#8862 = ORIENTED_EDGE ( 'NONE', *, *, #59185, .F. ) ;
#8863 = ORIENTED_EDGE ( 'NONE', *, *, #65964, .F. ) ;
#8864 = CARTESIAN_POINT ( 'NONE',  ( 151.5599459900709860, -10.00000000000000178, 280.6301873289890523 ) ) ;
#8865 = AXIS2_PLACEMENT_3D ( 'NONE', #7872, #2932, #18843 ) ;
#8866 = DIRECTION ( 'NONE',  ( -1.000000000000000000, 0.000000000000000000, 0.000000000000000000 ) ) ;
#8867 = ORIENTED_EDGE ( 'NONE', *, *, #10403, .F. ) ;
#8868 = VERTEX_POINT ( 'NONE', #3934 ) ;
#8869 = VECTOR ( 'NONE', #48993, 1000.000000000000000 ) ;
#8870 = LINE ( 'NONE', #14176, #42097 ) ;
#8871 = DIRECTION ( 'NONE',  ( 0.000000000000000000, -3.673940397442059868E-16, 1.000000000000000000 ) ) ;
#8872 = EDGE_LOOP ( 'NONE', ( #29556, #69671 ) ) ;
#8873 = ORIENTED_EDGE ( 'NONE', *, *, #42578, .T. ) ;
#8874 = CARTESIAN_POINT ( 'NONE',  ( 8.250000000000005329, 7.250000000000000888, -26.00000000000001066 ) ) ;
#8875 = DIRECTION ( 'NONE',  ( 0.000000000000000000, 0.000000000000000000, 1.000000000000000000 ) ) ;
#8876 = VERTEX_POINT ( 'NONE', #30800 ) ;
#8877 = ADVANCED_FACE ( 'NONE', ( #68977 ), #20884, .F. ) ;
#8878 = VECTOR ( 'NONE', #41077, 1000.000000000000000 ) ;
#8879 = ADVANCED_FACE ( 'NONE', ( #36448 ), #15935, .F. ) ;
#8880 = DIRECTION ( 'NONE',  ( 0.000000000000000000, 1.000000000000000000, 0.000000000000000000 ) ) ;
#8881 = CARTESIAN_POINT ( 'NONE',  ( 30.00000000000000000, -13.54524521594299991, -17.53999999999999915 ) ) ;
#8882 = EDGE_CURVE ( 'NONE', #12, #31689, #15243, .T. ) ;
#8884 = EDGE_LOOP ( 'NONE', ( #24503, #58183, #25365, #6593 ) ) ;
#8883 = DIRECTION ( 'NONE',  ( -1.000000000000000000, -0.000000000000000000, -0.000000000000000000 ) ) ;
#8885 = ORIENTED_EDGE ( 'NONE', *, *, #69508, .T. ) ;
#8886 = PLANE ( 'NONE',  #40653 ) ;
#8887 = EDGE_CURVE ( 'NONE', #3656, #48554, #42456, .T. ) ;
#8888 = CARTESIAN_POINT ( 'NONE',  ( 49.00000000000000000, -14.06939075806900163, -20.80000000000000426 ) ) ;
#8889 = DIRECTION ( 'NONE',  ( 1.000000000000000000, 0.000000000000000000, 0.000000000000000000 ) ) ;
#8890 = CARTESIAN_POINT ( 'NONE',  ( -22.14589803375000088, -17.50000000000000000, -21.50000000000000000 ) ) ;
#8891 = CARTESIAN_POINT ( 'NONE',  ( 7.900000000000003908, -21.00000000000000000, -18.00000000000000355 ) ) ;
#8892 = EDGE_CURVE ( 'NONE', #14806, #39018, #52311, .T. ) ;
#8893 = LINE ( 'NONE', #36113, #24739 ) ;
#8894 = ORIENTED_EDGE ( 'NONE', *, *, #24471, .T. ) ;
#8895 = DIRECTION ( 'NONE',  ( 0.000000000000000000, -1.000000000000000000, 0.000000000000000000 ) ) ;
#8896 = EDGE_CURVE ( 'NONE', #45446, #55340, #46645, .T. ) ;
#8898 = ORIENTED_EDGE ( 'NONE', *, *, #50003, .T. ) ;
#8897 = CARTESIAN_POINT ( 'NONE',  ( -2.406732575409590069, 8.697938382363036069, 26.00000000000000711 ) ) ;
#8899 = CARTESIAN_POINT ( 'NONE',  ( 283.0000000000000568, -26.50000000000000000, 9.080000000000000071 ) ) ;
#8900 = DIRECTION ( 'NONE',  ( -1.000000000000000000, 0.000000000000000000, 0.000000000000000000 ) ) ;
#8901 = DIRECTION ( 'NONE',  ( 0.000000000000000000, 0.000000000000000000, 1.000000000000000000 ) ) ;
#8902 = ORIENTED_EDGE ( 'NONE', *, *, #68714, .F. ) ;
#8903 = CARTESIAN_POINT ( 'NONE',  ( -4.193516549646675529, 11.11351654964658664, 455.0000000000000568 ) ) ;
#8904 = DIRECTION ( 'NONE',  ( 0.000000000000000000, 0.000000000000000000, -1.000000000000000000 ) ) ;
#8905 = ORIENTED_EDGE ( 'NONE', *, *, #56076, .F. ) ;
#8906 = AXIS2_PLACEMENT_3D ( 'NONE', #15744, #59574, #59225 ) ;
#8907 = CARTESIAN_POINT ( 'NONE',  ( 21.90000000000000213, -0.1999999999911795112, 8.826273045769999343E-12 ) ) ;
#8908 = AXIS2_PLACEMENT_3D ( 'NONE', #64437, #53485, #42515 ) ;
#8909 = DIRECTION ( 'NONE',  ( 0.000000000000000000, 0.000000000000000000, 1.000000000000000000 ) ) ;
#8910 = VERTEX_POINT ( 'NONE', #27580 ) ;
#8911 = FACE_OUTER_BOUND ( 'NONE', #1105, .T. ) ;
#8912 = ORIENTED_EDGE ( 'NONE', *, *, #29764, .F. ) ;
#8913 = ORIENTED_EDGE ( 'NONE', *, *, #59914, .T. ) ;
#8914 = VECTOR ( 'NONE', #49597, 1000.000000000000000 ) ;
#8915 = DIRECTION ( 'NONE',  ( 1.000000000000000000, -3.491481338843132961E-15, -1.836970198721036344E-16 ) ) ;
#8916 = CARTESIAN_POINT ( 'NONE',  ( -11.18999999999999950, -11.18999999999999950, 0.000000000000000000 ) ) ;
#8917 = LINE ( 'NONE', #67280, #60381 ) ;
#8918 = EDGE_CURVE ( 'NONE', #47489, #33326, #23312, .T. ) ;
#8919 = AXIS2_PLACEMENT_3D ( 'NONE', #62087, #28526, #12948 ) ;
#8920 = DIRECTION ( 'NONE',  ( 1.000000000000000000, 0.000000000000000000, 0.000000000000000000 ) ) ;
#8921 = CARTESIAN_POINT ( 'NONE',  ( 8.250000000000005329, -8.249999999999998224, -26.00000000000001066 ) ) ;
#8922 = ORIENTED_EDGE ( 'NONE', *, *, #10008, .T. ) ;
#8923 = ORIENTED_EDGE ( 'NONE', *, *, #31560, .F. ) ;
#8925 = ORIENTED_EDGE ( 'NONE', *, *, #3887, .F. ) ;
#8924 = DIRECTION ( 'NONE',  ( -0.000000000000000000, -0.000000000000000000, 1.000000000000000000 ) ) ;
#8926 = ORIENTED_EDGE ( 'NONE', *, *, #40367, .F. ) ;
#8928 = CIRCLE ( 'NONE', #48464, 24.99999999998789946 ) ;
#8927 = VECTOR ( 'NONE', #46552, 1000.000000000000000 ) ;
#8929 = DIRECTION ( 'NONE',  ( -0.8660254037844482555, 0.000000000000000000, 0.4999999999999831801 ) ) ;
#8930 = CARTESIAN_POINT ( 'NONE',  ( 11.50000000000000000, -12.00000000000000000, -10.52786404500095863 ) ) ;
#8931 = DIRECTION ( 'NONE',  ( -0.000000000000000000, -0.000000000000000000, 1.000000000000000000 ) ) ;
#8932 = CARTESIAN_POINT ( 'NONE',  ( 29.89999999999999858, -0.000000000000000000, 20.80000000000000426 ) ) ;
#8933 = CARTESIAN_POINT ( 'NONE',  ( -9.942044687070527687, -2.765062094115999791, 195.0000000000000284 ) ) ;
#8934 = AXIS2_PLACEMENT_3D ( 'NONE', #29070, #7832, #50981 ) ;
#8935 = ADVANCED_FACE ( 'NONE', ( #28609 ), #33575, .F. ) ;
#8936 = CARTESIAN_POINT ( 'NONE',  ( 4.149127210878726935, -6.836383711243002814, 54.00000000000000711 ) ) ;
#8937 = ORIENTED_EDGE ( 'NONE', *, *, #67141, .T. ) ;
#8938 = EDGE_LOOP ( 'NONE', ( #23030, #26324, #43991, #48099 ) ) ;
#8939 = EDGE_LOOP ( 'NONE', ( #32461, #3615, #51696, #65233 ) ) ;
#8940 = EDGE_LOOP ( 'NONE', ( #42303, #22298, #38215, #34282 ) ) ;
#8941 = EDGE_CURVE ( 'NONE', #30522, #58172, #44872, .T. ) ;
#8942 = DIRECTION ( 'NONE',  ( 0.000000000000000000, 0.000000000000000000, -1.000000000000000000 ) ) ;
#8943 = CARTESIAN_POINT ( 'NONE',  ( 5.257023737882819070, -5.257023737882825287, 54.00000000000000711 ) ) ;
#8944 = DIRECTION ( 'NONE',  ( 1.000000000000000000, 0.000000000000000000, 0.000000000000000000 ) ) ;
#8945 = DIRECTION ( 'NONE',  ( 1.000000000000000000, 0.000000000000000000, 0.000000000000000000 ) ) ;
#8946 = ORIENTED_EDGE ( 'NONE', *, *, #50529, .T. ) ;
#8947 = EDGE_LOOP ( 'NONE', ( #5966, #13, #68988, #35731 ) ) ;
#8948 = VERTEX_POINT ( 'NONE', #21930 ) ;
#8949 = CARTESIAN_POINT ( 'NONE',  ( -29.50000000000000355, -11.50000000000000000, -15.00000000000000000 ) ) ;
#8950 = VERTEX_POINT ( 'NONE', #32556 ) ;
#8951 = ORIENTED_EDGE ( 'NONE', *, *, #47460, .T. ) ;
#8952 = CARTESIAN_POINT ( 'NONE',  ( 14.25000000000000000, -2.500000000000000000, -21.77831216351300014 ) ) ;
#8953 = EDGE_CURVE ( 'NONE', #57125, #28928, #33909, .T. ) ;
#8954 = ORIENTED_EDGE ( 'NONE', *, *, #32529, .F. ) ;
#8955 = CIRCLE ( 'NONE', #1055, 0.3499999999999996447 ) ;
#8956 = ORIENTED_EDGE ( 'NONE', *, *, #17971, .T. ) ;
#8957 = CARTESIAN_POINT ( 'NONE',  ( 11.12648345035336028, 9.093516549646610159, 195.0000000000000284 ) ) ;
#8959 = ORIENTED_EDGE ( 'NONE', *, *, #9596, .T. ) ;
#8958 = LINE ( 'NONE', #52105, #23244 ) ;
#8960 = AXIS2_PLACEMENT_3D ( 'NONE', #12219, #39104, #54685 ) ;
#8961 = ORIENTED_EDGE ( 'NONE', *, *, #59025, .F. ) ;
#8962 = AXIS2_PLACEMENT_3D ( 'NONE', #54778, #6336, #33547 ) ;
#8963 = DIRECTION ( 'NONE',  ( 0.000000000000000000, 0.7071067811865474617, -0.7071067811865474617 ) ) ;
#8964 = DIRECTION ( 'NONE',  ( 0.000000000000000000, -1.000000000000000000, 0.000000000000000000 ) ) ;
#8965 = EDGE_CURVE ( 'NONE', #29539, #8221, #27247, .T. ) ;
#8966 = DIRECTION ( 'NONE',  ( -7.665540703601096574E-15, -1.000000000000000000, -3.673940397442059868E-16 ) ) ;
#8968 = VERTEX_POINT ( 'NONE', #11992 ) ;
#8967 = CARTESIAN_POINT ( 'NONE',  ( 7.250000000000005329, -7.249999999999998224, -15.50000000000000000 ) ) ;
#8969 = ORIENTED_EDGE ( 'NONE', *, *, #7425, .F. ) ;
#8970 = VECTOR ( 'NONE', #5366, 1000.000000000000000 ) ;
#8971 = LINE ( 'NONE', #8624, #17437 ) ;
#8972 = CARTESIAN_POINT ( 'NONE',  ( 16.89194109070750116, -5.000000000000000000, 26.25000000000000000 ) ) ;
#8973 = DIRECTION ( 'NONE',  ( 0.000000000000000000, -1.000000000000000000, 0.000000000000000000 ) ) ;
#8974 = AXIS2_PLACEMENT_3D ( 'NONE', #25628, #31631, #25977 ) ;
#8975 = DIRECTION ( 'NONE',  ( 0.000000000000000000, 0.000000000000000000, 1.000000000000000000 ) ) ;
#8976 = EDGE_CURVE ( 'NONE', #7863, #21985, #17305, .T. ) ;
#8977 = ORIENTED_EDGE ( 'NONE', *, *, #18550, .F. ) ;
#8978 = DIRECTION ( 'NONE',  ( -1.836970198721029934E-16, 1.836970198721036344E-16, -1.000000000000000000 ) ) ;
#8979 = EDGE_CURVE ( 'NONE', #26426, #19122, #66444, .T. ) ;
#8980 = AXIS2_PLACEMENT_3D ( 'NONE', #63100, #47875, #14658 ) ;
#8981 = CARTESIAN_POINT ( 'NONE',  ( -7.249999999999995559, -7.848062532927998269, -1.000000000000000000 ) ) ;
#8982 = FACE_OUTER_BOUND ( 'NONE', #11510, .T. ) ;
#8983 = ORIENTED_EDGE ( 'NONE', *, *, #64572, .F. ) ;
#8984 = DIRECTION ( 'NONE',  ( -1.000000000000000000, 0.000000000000000000, 0.000000000000000000 ) ) ;
#8985 = CARTESIAN_POINT ( 'NONE',  ( 283.0000000000000568, -20.50000000000000000, 17.00000000000000000 ) ) ;
#8986 = VECTOR ( 'NONE', #48005, 1000.000000000000114 ) ;
#8987 = DIRECTION ( 'NONE',  ( 0.000000000000000000, 1.000000000000000000, -0.000000000000000000 ) ) ;
#8988 = ORIENTED_EDGE ( 'NONE', *, *, #22127, .F. ) ;
#8989 = DIRECTION ( 'NONE',  ( 0.7071067811865401342, -0.7071067811865550112, -1.355854680848614216E-30 ) ) ;
#8990 = DIRECTION ( 'NONE',  ( 1.000000000000000000, 0.000000000000000000, 0.000000000000000000 ) ) ;
#8991 = CARTESIAN_POINT ( 'NONE',  ( 11.00000000000000000, -11.85423089348099879, -9.852125413066602277 ) ) ;
#8992 = ORIENTED_EDGE ( 'NONE', *, *, #22597, .F. ) ;
#8993 = AXIS2_PLACEMENT_3D ( 'NONE', #37500, #59055, #63680 ) ;
#8994 = CYLINDRICAL_SURFACE ( 'NONE', #49615, 24.99999999998784972 ) ;
#8995 = DIRECTION ( 'NONE',  ( -0.4999999999999832356, 0.000000000000000000, -0.8660254037844483666 ) ) ;
#8996 = DIRECTION ( 'NONE',  ( 0.000000000000000000, 0.000000000000000000, 1.000000000000000000 ) ) ;
#8997 = DIRECTION ( 'NONE',  ( 1.000000000000000000, 0.000000000000000000, 0.000000000000000000 ) ) ;
#8998 = DIRECTION ( 'NONE',  ( 0.000000000000000000, 1.000000000000000000, 0.000000000000000000 ) ) ;
#8999 = EDGE_LOOP ( 'NONE', ( #1053, #19055, #69925, #11746 ) ) ;
#9000 = CARTESIAN_POINT ( 'NONE',  ( 283.0000000000000568, -23.50007830495750127, 12.58007262201399890 ) ) ;
#9001 = DIRECTION ( 'NONE',  ( -1.000000000000000000, 0.000000000000000000, 0.000000000000000000 ) ) ;
#9002 = LINE ( 'NONE', #25276, #20987 ) ;
#9003 = EDGE_CURVE ( 'NONE', #56939, #67203, #17997, .T. ) ;
#9004 = DIRECTION ( 'NONE',  ( 0.000000000000000000, 0.6857142857142869419, -0.7278708115918273158 ) ) ;
#9005 = DIRECTION ( 'NONE',  ( 0.000000000000000000, 0.7071067811865475727, -0.7071067811865475727 ) ) ;
#9006 = ORIENTED_EDGE ( 'NONE', *, *, #63531, .T. ) ;
#9007 = VECTOR ( 'NONE', #8581, 1000.000000000000000 ) ;
#9009 = ORIENTED_EDGE ( 'NONE', *, *, #45983, .F. ) ;
#9008 = LINE ( 'NONE', #31311, #63354 ) ;
#9010 = CIRCLE ( 'NONE', #10185, 1.224999999999998757 ) ;
#9011 = EDGE_CURVE ( 'NONE', #49703, #22032, #39560, .T. ) ;
#9012 = AXIS2_PLACEMENT_3D ( 'NONE', #8021, #46211, #35236 ) ;
#9013 = FACE_OUTER_BOUND ( 'NONE', #56048, .T. ) ;
#9014 = CARTESIAN_POINT ( 'NONE',  ( -7.250000000000001776, -7.249999999999998224, -25.50000000000000355 ) ) ;
#9015 = LINE ( 'NONE', #47218, #17245 ) ;
#9016 = VERTEX_POINT ( 'NONE', #16640 ) ;
#9017 = EDGE_CURVE ( 'NONE', #27679, #29817, #49838, .T. ) ;
#9018 = CIRCLE ( 'NONE', #42898, 0.5249999999999994671 ) ;
#9019 = CARTESIAN_POINT ( 'NONE',  ( 15.50000000000000000, -5.000000000000000000, -26.00000000000000000 ) ) ;
#9020 = EDGE_CURVE ( 'NONE', #34472, #57523, #44513, .T. ) ;
#9021 = ORIENTED_EDGE ( 'NONE', *, *, #69508, .F. ) ;
#9022 = ORIENTED_EDGE ( 'NONE', *, *, #44084, .T. ) ;
#9023 = AXIS2_PLACEMENT_3D ( 'NONE', #20142, #64670, #31815 ) ;
#9024 = VERTEX_POINT ( 'NONE', #22627 ) ;
#9025 = EDGE_CURVE ( 'NONE', #28622, #7275, #26316, .T. ) ;
#9026 = EDGE_LOOP ( 'NONE', ( #11233, #50337, #64364, #59153 ) ) ;
#9027 = DIRECTION ( 'NONE',  ( 0.000000000000000000, 0.000000000000000000, -1.000000000000000000 ) ) ;
#9028 = PLANE ( 'NONE',  #6109 ) ;
#9029 = VECTOR ( 'NONE', #17092, 1000.000000000000000 ) ;
#9030 = CARTESIAN_POINT ( 'NONE',  ( 7.250000000000005329, -7.249999999999998224, -24.50000000000000000 ) ) ;
#9031 = CYLINDRICAL_SURFACE ( 'NONE', #48358, 2.458500000000000796 ) ;
#9032 = VERTEX_POINT ( 'NONE', #6022 ) ;
#9033 = EDGE_CURVE ( 'NONE', #33133, #28048, #64724, .T. ) ;
#9034 = ORIENTED_EDGE ( 'NONE', *, *, #21107, .F. ) ;
#9035 = PLANE ( 'NONE',  #49330 ) ;
#9036 = EDGE_CURVE ( 'NONE', #36263, #22451, #66087, .T. ) ;
#9038 = DIRECTION ( 'NONE',  ( -0.7071067811865476838, 0.4999999999999997780, 0.4999999999999997780 ) ) ;
#9037 = VECTOR ( 'NONE', #23061, 1000.000000000000000 ) ;
#9039 = VECTOR ( 'NONE', #53586, 1000.000000000000000 ) ;
#9040 = ORIENTED_EDGE ( 'NONE', *, *, #33081, .F. ) ;
#9041 = EDGE_CURVE ( 'NONE', #67467, #18151, #12332, .T. ) ;
#9042 = ORIENTED_EDGE ( 'NONE', *, *, #65667, .F. ) ;
#9043 = ADVANCED_FACE ( 'NONE', ( #16976 ), #44356, .F. ) ;
#9044 = EDGE_CURVE ( 'NONE', #67807, #50438, #49499, .T. ) ;
#9045 = ORIENTED_EDGE ( 'NONE', *, *, #1620, .F. ) ;
#9046 = ORIENTED_EDGE ( 'NONE', *, *, #19743, .F. ) ;
#9047 = CARTESIAN_POINT ( 'NONE',  ( 41.09999999999999432, -21.00000000000000000, 13.86939075806900057 ) ) ;
#9048 = UNCERTAINTY_MEASURE_WITH_UNIT (LENGTH_MEASURE( 1.000000000000000082E-05 ), #29858, 'distance_accuracy_value', 'NONE');
#9050 = EDGE_LOOP ( 'NONE', ( #53591, #11337, #62448, #29903, #26503, #26775, #15815, #26952, #39979, #3603, #27634, #18877, #39339, #8956, #59144, #15584, #19016, #52333 ) ) ;
#9049 = CARTESIAN_POINT ( 'NONE',  ( 41.09999999999999432, -21.00000000000000000, 13.86939075806900057 ) ) ;
#9051 = ADVANCED_FACE ( 'NONE', ( #34607 ), #24355, .T. ) ;
#9052 = CARTESIAN_POINT ( 'NONE',  ( -1.620245201994301665, 8.227189898828640935, 26.00000000000000711 ) ) ;
#9053 = LINE ( 'NONE', #45120, #17035 ) ;
#9054 = VECTOR ( 'NONE', #49740, 1000.000000000000000 ) ;
#9055 = EDGE_CURVE ( 'NONE', #40737, #5474, #8797, .T. ) ;
#9056 = VERTEX_POINT ( 'NONE', #28960 ) ;
#9057 = ORIENTED_EDGE ( 'NONE', *, *, #11824, .F. ) ;
#9058 = EDGE_CURVE ( 'NONE', #21659, #26808, #61843, .T. ) ;
#9059 = DIRECTION ( 'NONE',  ( 0.000000000000000000, -0.7071067811865474617, 0.7071067811865474617 ) ) ;
#9060 = AXIS2_PLACEMENT_3D ( 'NONE', #24807, #41759, #29746 ) ;
#9061 = ADVANCED_FACE ( 'NONE', ( #46612 ), #40266, .F. ) ;
#9062 = PLANE ( 'NONE',  #41682 ) ;
#9063 = VECTOR ( 'NONE', #39227, 1000.000000000000000 ) ;
#9064 = VERTEX_POINT ( 'NONE', #61121 ) ;
#9065 = EDGE_CURVE ( 'NONE', #18073, #6054, #2438, .T. ) ;
#9066 = AXIS2_PLACEMENT_3D ( 'NONE', #54676, #6909, #38743 ) ;
#9067 =( LENGTH_UNIT ( ) NAMED_UNIT ( * ) SI_UNIT ( .MILLI., .METRE. ) );
#9068 = CARTESIAN_POINT ( 'NONE',  ( 5.257023737882819070, -5.257023737882825287, 54.00000000000000711 ) ) ;
#9069 = DIRECTION ( 'NONE',  ( 0.000000000000000000, 1.000000000000000000, 0.000000000000000000 ) ) ;
#9070 = VERTEX_POINT ( 'NONE', #35650 ) ;
#9071 = CARTESIAN_POINT ( 'NONE',  ( 7.000000000000000000, -38.65000000000095781, -13.20000000000094253 ) ) ;
#9073 = DIRECTION ( 'NONE',  ( 0.000000000000000000, 0.000000000000000000, 1.000000000000000000 ) ) ;
#9072 = CIRCLE ( 'NONE', #48605, 5.000000000000004441 ) ;
#9074 = DIRECTION ( 'NONE',  ( 0.000000000000000000, -1.000000000000000000, 0.000000000000000000 ) ) ;
#9075 = CARTESIAN_POINT ( 'NONE',  ( 105.8309041053263257, 63.65740854044500452, 10.00000000000000000 ) ) ;
#9076 = CIRCLE ( 'NONE', #14684, 0.1749999999999993783 ) ;
#9077 = LINE ( 'NONE', #57858, #9402 ) ;
#9078 = ORIENTED_EDGE ( 'NONE', *, *, #29541, .T. ) ;
#9079 = DIRECTION ( 'NONE',  ( 0.000000000000000000, 0.000000000000000000, -1.000000000000000000 ) ) ;
#9080 = CARTESIAN_POINT ( 'NONE',  ( 9.955011587777223170, 9.234937905883922937, 195.0000000000000284 ) ) ;
#9081 = DIRECTION ( 'NONE',  ( -0.000000000000000000, 1.000000000000000000, -0.000000000000000000 ) ) ;
#9082 = DIRECTION ( 'NONE',  ( -0.000000000000000000, -0.000000000000000000, -1.000000000000000000 ) ) ;
#9083 = DIRECTION ( 'NONE',  ( 0.000000000000000000, 3.673940397442059868E-16, -1.000000000000000000 ) ) ;
#9084 = PLANE ( 'NONE',  #28546 ) ;
#9085 = VECTOR ( 'NONE', #1084, 1000.000000000000000 ) ;
#9086 = CYLINDRICAL_SURFACE ( 'NONE', #38015, 0.2000000000000005107 ) ;
#9087 = CIRCLE ( 'NONE', #52004, 0.3499999999999996447 ) ;
#9088 = LINE ( 'NONE', #69188, #16084 ) ;
#9089 = EDGE_LOOP ( 'NONE', ( #63569, #68005, #55821, #3683, #38319, #32559, #62038, #14291 ) ) ;
#9090 = CARTESIAN_POINT ( 'NONE',  ( 6.836383711243002814, 6.350872789121261519, 54.00000000000000711 ) ) ;
#9091 = CARTESIAN_POINT ( 'NONE',  ( -9.915476262117259409, 0.9414762621171833823, 26.00000000000000711 ) ) ;
#9092 = ORIENTED_EDGE ( 'NONE', *, *, #4775, .F. ) ;
#9093 = LINE ( 'NONE', #30662, #5279 ) ;
#9094 = DIRECTION ( 'NONE',  ( 1.000000000000000000, 0.000000000000000000, 0.000000000000000000 ) ) ;
#9095 = DIRECTION ( 'NONE',  ( 1.000000000000000000, 0.000000000000000000, 0.000000000000000000 ) ) ;
#9096 = DIRECTION ( 'NONE',  ( 0.000000000000000000, 1.000000000000000000, 0.000000000000000000 ) ) ;
#9097 = CARTESIAN_POINT ( 'NONE',  ( 30.00000000000000000, -17.14999999999900027, 26.64999999999900027 ) ) ;
#9098 = ORIENTED_EDGE ( 'NONE', *, *, #24940, .T. ) ;
#9099 = EDGE_CURVE ( 'NONE', #68671, #67553, #52810, .T. ) ;
#9100 = CARTESIAN_POINT ( 'NONE',  ( -7.342976262117273833, -4.961189459950004377, 54.00000000000000711 ) ) ;
#9101 = EDGE_LOOP ( 'NONE', ( #31589, #66443, #22278, #7606 ) ) ;
#9102 = LINE ( 'NONE', #22673, #53492 ) ;
#9103 = AXIS2_PLACEMENT_3D ( 'NONE', #31246, #41128, #4379 ) ;
#9104 = DIRECTION ( 'NONE',  ( -1.000000000000000000, 0.000000000000000000, 0.000000000000000000 ) ) ;
#9105 = ORIENTED_EDGE ( 'NONE', *, *, #35608, .T. ) ;
#9106 = EDGE_CURVE ( 'NONE', #27584, #26198, #60645, .T. ) ;
#9107 = CARTESIAN_POINT ( 'NONE',  ( 4.186483450353422953, 11.77351654964658501, 455.0000000000000568 ) ) ;
#9108 = PLANE ( 'NONE',  #6938 ) ;
#9109 = ADVANCED_FACE ( 'NONE', ( #18695 ), #66781, .F. ) ;
#9110 = VERTEX_POINT ( 'NONE', #2093 ) ;
#9111 = CIRCLE ( 'NONE', #55398, 1.399999999999999245 ) ;
#9112 = DIRECTION ( 'NONE',  ( 0.000000000000000000, -1.000000000000000000, 0.000000000000000000 ) ) ;
#9113 = VERTEX_POINT ( 'NONE', #68190 ) ;
#9114 = EDGE_CURVE ( 'NONE', #40740, #33225, #30166, .T. ) ;
#9115 = EDGE_LOOP ( 'NONE', ( #44719, #67166, #18119, #13546 ) ) ;
#9116 = LINE ( 'NONE', #13712, #45246 ) ;
#9117 = AXIS2_PLACEMENT_3D ( 'NONE', #30367, #14809, #2784 ) ;
#9118 = EDGE_LOOP ( 'NONE', ( #56618, #11410, #57057, #11860 ) ) ;
#9119 = ORIENTED_EDGE ( 'NONE', *, *, #34568, .F. ) ;
#9120 = FACE_OUTER_BOUND ( 'NONE', #46597, .T. ) ;
#9121 = FACE_OUTER_BOUND ( 'NONE', #26367, .T. ) ;
#9123 = DIRECTION ( 'NONE',  ( 1.836970198721029934E-16, 1.836970198721010706E-16, -1.000000000000000000 ) ) ;
#9122 = VECTOR ( 'NONE', #46018, 1000.000000000000000 ) ;
#9124 = ORIENTED_EDGE ( 'NONE', *, *, #14564, .T. ) ;
#9125 = VECTOR ( 'NONE', #64083, 1000.000000000000114 ) ;
#9126 = PLANE ( 'NONE',  #5266 ) ;
#9128 = DIRECTION ( 'NONE',  ( -0.000000000000000000, -0.000000000000000000, -1.000000000000000000 ) ) ;
#9127 = DIRECTION ( 'NONE',  ( 0.000000000000000000, 0.000000000000000000, -1.000000000000000000 ) ) ;
#9129 = VERTEX_POINT ( 'NONE', #13394 ) ;
#9131 = ORIENTED_EDGE ( 'NONE', *, *, #14840, .T. ) ;
#9130 = DIRECTION ( 'NONE',  ( 0.000000000000000000, 0.000000000000000000, -1.000000000000000000 ) ) ;
#9132 = EDGE_LOOP ( 'NONE', ( #63084, #58815, #69239, #14345 ) ) ;
#9133 = AXIS2_PLACEMENT_3D ( 'NONE', #57101, #2311, #24231 ) ;
#9134 = ADVANCED_FACE ( 'NONE', ( #61470 ), #29297, .F. ) ;
#9135 = VECTOR ( 'NONE', #40231, 1000.000000000000000 ) ;
#9136 = SHAPE_DEFINITION_REPRESENTATION ( #2347, #33057 ) ;
#9137 = CYLINDRICAL_SURFACE ( 'NONE', #22057, 0.2000000000000005107 ) ;
#9139 = VERTEX_POINT ( 'NONE', #67844 ) ;
#9138 = FACE_OUTER_BOUND ( 'NONE', #26548, .T. ) ;
#9140 = VECTOR ( 'NONE', #49630, 999.9999999999998863 ) ;
#9141 = CARTESIAN_POINT ( 'NONE',  ( -5.993516549646711766, 5.993516549646603409, 455.0000000000000568 ) ) ;
#9142 = CARTESIAN_POINT ( 'NONE',  ( -2.355476262117229158, 9.547976262117156665, 54.00000000000000711 ) ) ;
#9143 = VERTEX_POINT ( 'NONE', #23650 ) ;
#9144 = ORIENTED_EDGE ( 'NONE', *, *, #58778, .F. ) ;
#9145 = VECTOR ( 'NONE', #44445, 1000.000000000000000 ) ;
#9146 = DIRECTION ( 'NONE',  ( -1.000000000000000000, 0.000000000000000000, 0.000000000000000000 ) ) ;
#9147 = ORIENTED_EDGE ( 'NONE', *, *, #69936, .F. ) ;
#9148 = DIRECTION ( 'NONE',  ( 1.000000000000000000, 0.000000000000000000, 0.000000000000000000 ) ) ;
#9149 = CARTESIAN_POINT ( 'NONE',  ( -8.750000000000003553, -7.348062532927999158, 0.000000000000000000 ) ) ;
#9150 = CARTESIAN_POINT ( 'NONE',  ( -11.50000000000000000, -12.00000000000000000, -10.52786404500095863 ) ) ;
#9151 = EDGE_CURVE ( 'NONE', #938, #51166, #2782, .T. ) ;
#9152 = ORIENTED_EDGE ( 'NONE', *, *, #64526, .T. ) ;
#9153 = EDGE_CURVE ( 'NONE', #42535, #59658, #7381, .T. ) ;
#9154 = DIRECTION ( 'NONE',  ( -0.000000000000000000, -0.000000000000000000, -1.000000000000000000 ) ) ;
#9155 = AXIS2_PLACEMENT_3D ( 'NONE', #10533, #69237, #15838 ) ;
#9156 = CARTESIAN_POINT ( 'NONE',  ( 282.6457513110646005, -25.50000000000000355, -17.00000000000000000 ) ) ;
#9159 = ORIENTED_EDGE ( 'NONE', *, *, #8976, .T. ) ;
#9158 = EDGE_CURVE ( 'NONE', #48640, #21736, #51669, .T. ) ;
#9157 = DIRECTION ( 'NONE',  ( -0.4999999999989410693, 0.000000000000000000, 0.8660254037850499964 ) ) ;
#9161 = ORIENTED_EDGE ( 'NONE', *, *, #28411, .F. ) ;
#9160 = CARTESIAN_POINT ( 'NONE',  ( 0.000000000000000000, 8.250000000000001776, -19.00000000000000000 ) ) ;
#9162 = CARTESIAN_POINT ( 'NONE',  ( 6.501044194225450212, 3.142976262117187058, 54.00000000000000711 ) ) ;
#9163 = DIRECTION ( 'NONE',  ( 0.000000000000000000, 3.673940397442059868E-16, -1.000000000000000000 ) ) ;
#9164 = CARTESIAN_POINT ( 'NONE',  ( 10.92648345035335922, 9.293516549646611224, 195.0000000000000284 ) ) ;
#9165 = CARTESIAN_POINT ( 'NONE',  ( 2.369523737882817116, 9.547976262117204627, 54.00000000000000711 ) ) ;
#9166 = DIRECTION ( 'NONE',  ( -3.491481338843132961E-15, -1.000000000000000000, 0.000000000000000000 ) ) ;
#9167 = EDGE_LOOP ( 'NONE', ( #38706, #55004, #19211, #10524 ) ) ;
#9168 = DIRECTION ( 'NONE',  ( 0.000000000000000000, -1.000000000000000000, 0.000000000000000000 ) ) ;
#9169 = LINE ( 'NONE', #40639, #25957 ) ;
#9170 = AXIS2_PLACEMENT_3D ( 'NONE', #55246, #28364, #55935 ) ;
#9171 = LINE ( 'NONE', #52307, #60525 ) ;
#9173 = ORIENTED_EDGE ( 'NONE', *, *, #2626, .T. ) ;
#9172 = CARTESIAN_POINT ( 'NONE',  ( -6.350872789121327244, 6.822336235477381550, 26.00000000000000711 ) ) ;
#9174 = DIRECTION ( 'NONE',  ( 0.000000000000000000, 0.7071067811865495711, -0.7071067811865455743 ) ) ;
#9175 = CARTESIAN_POINT ( 'NONE',  ( 41.09999999999999432, -0.2000000000000000111, 0.000000000000000000 ) ) ;
#9176 = VECTOR ( 'NONE', #26070, 1000.000000000000000 ) ;
#9177 = CARTESIAN_POINT ( 'NONE',  ( -9.897976262117259338, 3.842976262117183683, 26.00000000000000711 ) ) ;
#9178 = ORIENTED_EDGE ( 'NONE', *, *, #51736, .F. ) ;
#9179 = LINE ( 'NONE', #25094, #63710 ) ;
#9180 = DIRECTION ( 'NONE',  ( 0.000000000000000000, 0.000000000000000000, 1.000000000000000000 ) ) ;
#9181 = EDGE_LOOP ( 'NONE', ( #21172, #51234, #3717, #13637 ) ) ;
#9182 = CARTESIAN_POINT ( 'NONE',  ( 13.90000000000000213, -0.1999999999911795112, 8.826273045769999343E-12 ) ) ;
#9183 = CIRCLE ( 'NONE', #23854, 0.1749999999999998224 ) ;
#9184 = VECTOR ( 'NONE', #32770, 1000.000000000000000 ) ;
#9185 = DIRECTION ( 'NONE',  ( 1.836970198721029934E-16, 1.836970198721010706E-16, -1.000000000000000000 ) ) ;
#9186 = LINE ( 'NONE', #41349, #17388 ) ;
#9187 = DIRECTION ( 'NONE',  ( 0.000000000000000000, -0.7096009616570518874, 0.7046037717862339012 ) ) ;
#9188 = AXIS2_PLACEMENT_3D ( 'NONE', #26596, #32940, #54521 ) ;
#9189 = EDGE_CURVE ( 'NONE', #47124, #67875, #42631, .T. ) ;
#9190 = DIRECTION ( 'NONE',  ( 0.000000000000000000, 0.000000000000000000, -1.000000000000000000 ) ) ;
#9191 = AXIS2_PLACEMENT_3D ( 'NONE', #57594, #40281, #19063 ) ;
#9192 = ORIENTED_EDGE ( 'NONE', *, *, #20583, .F. ) ;
#9193 = FACE_OUTER_BOUND ( 'NONE', #64329, .T. ) ;
#9194 = VERTEX_POINT ( 'NONE', #30006 ) ;
#9195 = DIRECTION ( 'NONE',  ( 0.000000000000000000, 0.000000000000000000, 1.000000000000000000 ) ) ;
#9196 = ORIENTED_EDGE ( 'NONE', *, *, #52227, .T. ) ;
#9197 = ADVANCED_FACE ( 'NONE', ( #51586 ), #3151, .F. ) ;
#9198 = DIRECTION ( 'NONE',  ( -3.491481338843133355E-15, -1.000000000000000000, 0.000000000000000000 ) ) ;
#9199 = VECTOR ( 'NONE', #64495, 1000.000000000000114 ) ;
#9200 = EDGE_CURVE ( 'NONE', #9204, #16876, #52281, .T. ) ;
#9201 = ADVANCED_FACE ( 'NONE', ( #10539 ), #58983, .T. ) ;
#9202 = CARTESIAN_POINT ( 'NONE',  ( 7.250000000000005329, -8.249999999999998224, -10.50000000000000000 ) ) ;
#9203 = FACE_BOUND ( 'NONE', #49730, .T. ) ;
#9204 = VERTEX_POINT ( 'NONE', #26120 ) ;
#9205 = EDGE_CURVE ( 'NONE', #24682, #23628, #41311, .T. ) ;
#9206 = ORIENTED_EDGE ( 'NONE', *, *, #31827, .T. ) ;
#9207 = EDGE_CURVE ( 'NONE', #7648, #14823, #65214, .T. ) ;
#9208 = LINE ( 'NONE', #40671, #56671 ) ;
#9209 = ORIENTED_EDGE ( 'NONE', *, *, #17923, .F. ) ;
#9210 = ORIENTED_EDGE ( 'NONE', *, *, #36412, .F. ) ;
#9211 = PLANE ( 'NONE',  #59800 ) ;
#9212 = CARTESIAN_POINT ( 'NONE',  ( 15.50000000000000000, -5.000000000000000000, 26.00000000000000000 ) ) ;
#9213 = DIRECTION ( 'NONE',  ( 0.000000000000000000, 0.000000000000000000, -1.000000000000000000 ) ) ;
#9214 = EDGE_CURVE ( 'NONE', #5750, #19510, #29044, .T. ) ;
#9215 = CARTESIAN_POINT ( 'NONE',  ( 11.00000000000000000, -12.00000000000000000, 12.20000000000000107 ) ) ;
#9216 = ORIENTED_EDGE ( 'NONE', *, *, #64726, .T. ) ;
#9217 = CARTESIAN_POINT ( 'NONE',  ( 15.89999999999999680, 13.66939075806899240, 20.79999999999999361 ) ) ;
#9219 = DIRECTION ( 'NONE',  ( 0.000000000000000000, -1.000000000000000000, 0.000000000000000000 ) ) ;
#9218 = CARTESIAN_POINT ( 'NONE',  ( -7.813516549646711162, 11.77351654964660277, 455.0000000000000568 ) ) ;
#9220 = VERTEX_POINT ( 'NONE', #42020 ) ;
#9222 = EDGE_LOOP ( 'NONE', ( #13000, #12226, #32531, #57985 ) ) ;
#9221 = DIRECTION ( 'NONE',  ( -0.7071067811865451302, 0.7071067811865500152, 2.597868168706485527E-16 ) ) ;
#9223 = ORIENTED_EDGE ( 'NONE', *, *, #65201, .F. ) ;
#9224 = LINE ( 'NONE', #13818, #60390 ) ;
#9225 = AXIS2_PLACEMENT_3D ( 'NONE', #15257, #3595, #46026 ) ;
#9226 = DIRECTION ( 'NONE',  ( -1.000000000000000000, 0.000000000000000000, 0.000000000000000000 ) ) ;
#9227 = VECTOR ( 'NONE', #32896, 1000.000000000000000 ) ;
#9228 = ORIENTED_EDGE ( 'NONE', *, *, #37499, .F. ) ;
#9229 = EDGE_LOOP ( 'NONE', ( #47069, #2468, #53993, #28332 ) ) ;
#9230 = CARTESIAN_POINT ( 'NONE',  ( -24.00000000000000000, -17.50000000000000000, -19.33772233983200195 ) ) ;
#9231 = CARTESIAN_POINT ( 'NONE',  ( 4.046023737882819660, -3.157023737882826087, 54.00000000000000711 ) ) ;
#9232 = ORIENTED_EDGE ( 'NONE', *, *, #33138, .F. ) ;
#9233 = CIRCLE ( 'NONE', #36327, 0.1749999999999989342 ) ;
#9234 = AXIS2_PLACEMENT_3D ( 'NONE', #48071, #26504, #5296 ) ;
#9235 = EDGE_LOOP ( 'NONE', ( #7181, #491, #48697, #13238 ) ) ;
#9236 = FACE_BOUND ( 'NONE', #3148, .T. ) ;
#9237 = CARTESIAN_POINT ( 'NONE',  ( 11.50000000000000000, -11.50000000000100009, -19.50000000000103739 ) ) ;
#9238 = ORIENTED_EDGE ( 'NONE', *, *, #32802, .T. ) ;
#9239 = EDGE_CURVE ( 'NONE', #7660, #7047, #52645, .T. ) ;
#9240 = ADVANCED_FACE ( 'NONE', ( #57582 ), #63598, .T. ) ;
#9241 = CYLINDRICAL_SURFACE ( 'NONE', #19922, 2.250000000000001776 ) ;
#9242 = LINE ( 'NONE', #39989, #9122 ) ;
#9245 = ORIENTED_EDGE ( 'NONE', *, *, #17921, .F. ) ;
#9244 = EDGE_CURVE ( 'NONE', #16044, #45304, #26821, .T. ) ;
#9243 = DIRECTION ( 'NONE',  ( 1.000000000000000000, -0.000000000000000000, 0.000000000000000000 ) ) ;
#9246 = VERTEX_POINT ( 'NONE', #42715 ) ;
#9247 = EDGE_CURVE ( 'NONE', #24243, #8233, #20113, .T. ) ;
#9249 = DIRECTION ( 'NONE',  ( 0.000000000000000000, 0.000000000000000000, -1.000000000000000000 ) ) ;
#9248 = AXIS2_PLACEMENT_3D ( 'NONE', #28635, #17004, #66125 ) ;
#9250 = CYLINDRICAL_SURFACE ( 'NONE', #49889, 2.458500000000000796 ) ;
#9251 = LINE ( 'NONE', #36464, #6428 ) ;
#9252 = DIRECTION ( 'NONE',  ( -1.047444401652939849E-14, -1.000000000000000000, 0.000000000000000000 ) ) ;
#9253 = EDGE_CURVE ( 'NONE', #26084, #50433, #21202, .T. ) ;
#9254 = DIRECTION ( 'NONE',  ( -1.047444401652940007E-14, -1.000000000000000000, -1.836970198721029934E-16 ) ) ;
#9255 = APPLICATION_CONTEXT ( 'automotive_design' ) ;
#9256 = DIRECTION ( 'NONE',  ( 0.000000000000000000, 0.000000000000000000, 1.000000000000000000 ) ) ;
#9257 = EDGE_LOOP ( 'NONE', ( #23106, #68263, #33112, #65740 ) ) ;
#9258 = LINE ( 'NONE', #30818, #59755 ) ;
#9260 = ORIENTED_EDGE ( 'NONE', *, *, #50619, .T. ) ;
#9259 = DIRECTION ( 'NONE',  ( -1.794541526872559352E-16, -1.000000000000000000, 0.000000000000000000 ) ) ;
#9261 = DIRECTION ( 'NONE',  ( 0.000000000000000000, 0.000000000000000000, 1.000000000000000000 ) ) ;
#9262 = CARTESIAN_POINT ( 'NONE',  ( 7.000000000000000000, -25.93000000000544958, -9.412893218815410634 ) ) ;
#9263 = AXIS2_PLACEMENT_3D ( 'NONE', #6865, #16459, #27413 ) ;
#9264 = CARTESIAN_POINT ( 'NONE',  ( 69.92576880110368620, 10.00000000000000000, 281.4830310981151911 ) ) ;
#9265 = ORIENTED_EDGE ( 'NONE', *, *, #6011, .F. ) ;
#9266 = CARTESIAN_POINT ( 'NONE',  ( 9.929523737882751888, 0.9414762621171479662, 54.00000000000000711 ) ) ;
#9267 = CARTESIAN_POINT ( 'NONE',  ( 25.90000000000000213, 20.60000000000000142, 13.86939075806899702 ) ) ;
#9268 = CIRCLE ( 'NONE', #61171, 0.3499999999999996447 ) ;
#9269 = ORIENTED_EDGE ( 'NONE', *, *, #9681, .T. ) ;
#9270 = PLANE ( 'NONE',  #36859 ) ;
#9271 = VECTOR ( 'NONE', #36377, 1000.000000000000000 ) ;
#9272 = DIRECTION ( 'NONE',  ( -0.000000000000000000, -0.000000000000000000, -1.000000000000000000 ) ) ;
#9273 = EDGE_LOOP ( 'NONE', ( #816, #59814, #8224, #56427 ) ) ;
#9274 = DIRECTION ( 'NONE',  ( 1.836970198721029934E-16, 1.836970198721010706E-16, -1.000000000000000000 ) ) ;
#9275 = ORIENTED_EDGE ( 'NONE', *, *, #23032, .T. ) ;
#9276 = ORIENTED_EDGE ( 'NONE', *, *, #68677, .T. ) ;
#9277 = CARTESIAN_POINT ( 'NONE',  ( 11.48848345035334617, -11.08848345035349148, 455.0000000000000568 ) ) ;
#9278 = LINE ( 'NONE', #31559, #3711 ) ;
#9279 = CARTESIAN_POINT ( 'NONE',  ( -11.00000000000000000, -17.14999999999900027, 26.64999999999900027 ) ) ;
#9280 = VECTOR ( 'NONE', #43021, 1000.000000000000000 ) ;
#9281 = DIRECTION ( 'NONE',  ( 1.000000000000000000, -0.000000000000000000, -0.000000000000000000 ) ) ;
#9282 = DIRECTION ( 'NONE',  ( -1.000000000000000000, 0.000000000000000000, 0.000000000000000000 ) ) ;
#9283 = VERTEX_POINT ( 'NONE', #68899 ) ;
#9284 = ORIENTED_EDGE ( 'NONE', *, *, #2100, .F. ) ;
#9285 = EDGE_CURVE ( 'NONE', #54102, #51111, #32504, .T. ) ;
#9287 = ORIENTED_EDGE ( 'NONE', *, *, #7209, .F. ) ;
#9286 = CARTESIAN_POINT ( 'NONE',  ( -11.50000000000000000, -11.50000000000100009, 15.00000000000084910 ) ) ;
#9288 = VECTOR ( 'NONE', #54775, 1000.000000000000000 ) ;
#9289 = ORIENTED_EDGE ( 'NONE', *, *, #58903, .T. ) ;
#9290 = CYLINDRICAL_SURFACE ( 'NONE', #37154, 0.5249999999999990230 ) ;
#9291 = VECTOR ( 'NONE', #28562, 1000.000000000000114 ) ;
#9292 = DIRECTION ( 'NONE',  ( -1.000000000000000000, 0.000000000000000000, 0.000000000000000000 ) ) ;
#9293 = ADVANCED_FACE ( 'NONE', ( #36723 ), #3842, .F. ) ;
#9294 = LINE ( 'NONE', #52432, #28989 ) ;
#9295 = FACE_BOUND ( 'NONE', #19070, .T. ) ;
#9296 = AXIS2_PLACEMENT_3D ( 'NONE', #9175, #25440, #16580 ) ;
#9297 = DIRECTION ( 'NONE',  ( 0.000000000000000000, 1.000000000000000000, 0.000000000000000000 ) ) ;
#9299 = CARTESIAN_POINT ( 'NONE',  ( -14.25000000000000000, -0.2038245569916330158, -21.77831216351300014 ) ) ;
#9298 = DIRECTION ( 'NONE',  ( 0.000000000000000000, -3.673940397442059868E-16, 1.000000000000000000 ) ) ;
#9300 = ORIENTED_EDGE ( 'NONE', *, *, #14781, .T. ) ;
#9301 = ORIENTED_EDGE ( 'NONE', *, *, #725, .F. ) ;
#9302 = VERTEX_POINT ( 'NONE', #25411 ) ;
#9303 = ORIENTED_EDGE ( 'NONE', *, *, #12776, .T. ) ;
#9304 = CYLINDRICAL_SURFACE ( 'NONE', #55922, 24.99999999998794920 ) ;
#9305 = DIRECTION ( 'NONE',  ( -1.000000000000000000, -0.000000000000000000, -0.000000000000000000 ) ) ;
#9306 = ADVANCED_FACE ( 'NONE', ( #63240 ), #69243, .T. ) ;
#9307 = DIRECTION ( 'NONE',  ( -8.673617379884035472E-19, 0.000000000000000000, 0.9999999999999998890 ) ) ;
#9308 = EDGE_CURVE ( 'NONE', #3375, #2041, #15849, .T. ) ;
#9309 = DIRECTION ( 'NONE',  ( 0.000000000000000000, 0.000000000000000000, 1.000000000000000000 ) ) ;
#9310 = EDGE_LOOP ( 'NONE', ( #32981, #8509, #43663, #33807, #58784 ) ) ;
#9311 = ORIENTED_EDGE ( 'NONE', *, *, #9446, .T. ) ;
#9312 = VERTEX_POINT ( 'NONE', #47673 ) ;
#9313 = PLANE ( 'NONE',  #9103 ) ;
#9314 = ORIENTED_EDGE ( 'NONE', *, *, #47587, .F. ) ;
#9315 = VERTEX_POINT ( 'NONE', #31778 ) ;
#9316 = CARTESIAN_POINT ( 'NONE',  ( -7.955476262117324282, -9.562023737882771712, 54.00000000000000711 ) ) ;
#9317 = AXIS2_PLACEMENT_3D ( 'NONE', #41964, #47618, #31006 ) ;
#9318 = ORIENTED_EDGE ( 'NONE', *, *, #20893, .T. ) ;
#9319 = VERTEX_POINT ( 'NONE', #37424 ) ;
#9320 = CARTESIAN_POINT ( 'NONE',  ( 7.428221114745003462, -3.006483450353395259, 195.0000000000000284 ) ) ;
#9321 = AXIS2_PLACEMENT_3D ( 'NONE', #62191, #13755, #35306 ) ;
#9323 = ORIENTED_EDGE ( 'NONE', *, *, #27139, .T. ) ;
#9322 = DIRECTION ( 'NONE',  ( 1.000000000000000000, -0.000000000000000000, 0.000000000000000000 ) ) ;
#9324 = ORIENTED_EDGE ( 'NONE', *, *, #11954, .F. ) ;
#9325 = DIRECTION ( 'NONE',  ( -1.000000000000000000, 0.000000000000000000, -0.000000000000000000 ) ) ;
#9326 = CARTESIAN_POINT ( 'NONE',  ( 4.149127210878725158, 6.822336235477391320, 54.00000000000000711 ) ) ;
#9327 = AXIS2_PLACEMENT_3D ( 'NONE', #64792, #16705, #11041 ) ;
#9329 = ORIENTED_EDGE ( 'NONE', *, *, #49906, .T. ) ;
#9328 = LINE ( 'NONE', #46797, #48175 ) ;
#9330 = EDGE_LOOP ( 'NONE', ( #38935, #7194, #6185, #64805 ) ) ;
#9331 = DIRECTION ( 'NONE',  ( 1.000000000000000000, 0.000000000000000000, 0.000000000000000000 ) ) ;
#9332 = DIRECTION ( 'NONE',  ( 0.000000000000000000, 0.000000000000000000, 1.000000000000000000 ) ) ;
#9333 = CARTESIAN_POINT ( 'NONE',  ( 39.00000000000000000, 21.00000000000000000, -16.96999999999999886 ) ) ;
#9334 = ADVANCED_FACE ( 'NONE', ( #53344 ), #4895, .T. ) ;
#9335 = DIRECTION ( 'NONE',  ( 0.000000000000000000, 0.000000000000000000, -1.000000000000000000 ) ) ;
#9336 = B_SPLINE_CURVE_WITH_KNOTS ( 'NONE', 3,
 ( #60183, #32285, #5065, #16030, #6106, #48206 ),
 .UNSPECIFIED., .F., .F.,
 ( 4, 2, 4 ),
 ( 0.0002380763768129734448, 0.7291065797294589146, 1.457975083082104995 ),
 .UNSPECIFIED. ) ;
#9337 = VERTEX_POINT ( 'NONE', #6620 ) ;
#9338 = DIRECTION ( 'NONE',  ( -1.836970198721029934E-16, 1.836970198721036344E-16, -1.000000000000000000 ) ) ;
#9339 = CARTESIAN_POINT ( 'NONE',  ( 8.711985858128693749, -8.093267424590459669, 26.00000000000000000 ) ) ;
#9340 = CIRCLE ( 'NONE', #59007, 5.000000000000004441 ) ;
#9341 =( LENGTH_UNIT ( ) NAMED_UNIT ( * ) SI_UNIT ( .MILLI., .METRE. ) );
#9342 = ORIENTED_EDGE ( 'NONE', *, *, #33177, .T. ) ;
#9343 = DIRECTION ( 'NONE',  ( 0.5773502691896298389, -0.5773502691896257311, 0.5773502691896216232 ) ) ;
#9345 = CARTESIAN_POINT ( 'NONE',  ( 3.848229544836323512, -7.357023737882811609, 54.00000000000000711 ) ) ;
#9344 = VECTOR ( 'NONE', #55695, 1000.000000000000000 ) ;
#9346 = EDGE_CURVE ( 'NONE', #14806, #39001, #11228, .T. ) ;
#9347 = DIRECTION ( 'NONE',  ( 0.000000000000000000, 0.000000000000000000, -1.000000000000000000 ) ) ;
#9348 = ORIENTED_EDGE ( 'NONE', *, *, #44380, .F. ) ;
#9349 = ADVANCED_FACE ( 'NONE', ( #27155 ), #17221, .F. ) ;
#9350 = DIRECTION ( 'NONE',  ( 0.000000000000000000, -0.8320000000000487006, -0.5547756303226729635 ) ) ;
#9351 = CIRCLE ( 'NONE', #11600, 3.499999999999849454 ) ;
#9352 = DIRECTION ( 'NONE',  ( 0.000000000000000000, 0.000000000000000000, -1.000000000000000000 ) ) ;
#9353 = LINE ( 'NONE', #3699, #5556 ) ;
#9354 = EDGE_LOOP ( 'NONE', ( #52981, #17790, #56277, #21850 ) ) ;
#9355 = DIRECTION ( 'NONE',  ( -5.981805089575196197E-17, -1.000000000000000000, 0.000000000000000000 ) ) ;
#9356 = DIRECTION ( 'NONE',  ( 0.000000000000000000, 0.000000000000000000, 1.000000000000000000 ) ) ;
#9357 = LINE ( 'NONE', #21009, #27461 ) ;
#9358 = CARTESIAN_POINT ( 'NONE',  ( -14.24999999999999822, -0.3152037684892594616, 22.25410949791978510 ) ) ;
#9359 = CARTESIAN_POINT ( 'NONE',  ( -7.250000000000001776, -7.249999999999998224, -26.00000000000001066 ) ) ;
#9360 = ORIENTED_EDGE ( 'NONE', *, *, #37564, .F. ) ;
#9361 = CARTESIAN_POINT ( 'NONE',  ( 8.000000000000001776, -8.000000000000000000, -1.000000000000000000 ) ) ;
#9362 = PLANE ( 'NONE',  #56502 ) ;
#9363 = VECTOR ( 'NONE', #9719, 1000.000000000000000 ) ;
#9364 = CARTESIAN_POINT ( 'NONE',  ( -29.50000000000000355, -11.50000000000000000, -19.00000000000000000 ) ) ;
#9365 = FACE_OUTER_BOUND ( 'NONE', #26787, .T. ) ;
#9366 = AXIS2_PLACEMENT_3D ( 'NONE', #63528, #59614, #68824 ) ;
#9367 = VERTEX_POINT ( 'NONE', #11907 ) ;
#9369 = EDGE_LOOP ( 'NONE', ( #4697, #47631, #40366, #64002 ) ) ;
#9368 = LINE ( 'NONE', #20326, #49758 ) ;
#9370 = ADVANCED_FACE ( 'NONE', ( #55415 ), #59679, .T. ) ;
#9371 = CARTESIAN_POINT ( 'NONE',  ( 24.00000000000000000, -17.50000000000000000, 15.70499999999969809 ) ) ;
#9372 = EDGE_CURVE ( 'NONE', #33051, #37343, #66349, .T. ) ;
#9373 = DIRECTION ( 'NONE',  ( 0.000000000000000000, 1.000000000000000000, 0.000000000000000000 ) ) ;
#9374 = CARTESIAN_POINT ( 'NONE',  ( 40.90000000000000568, 21.00000000000000000, 16.96999999999999886 ) ) ;
#9375 = ORIENTED_EDGE ( 'NONE', *, *, #43440, .F. ) ;
#9376 = EDGE_CURVE ( 'NONE', #20422, #61702, #14421, .T. ) ;
#9377 = AXIS2_PLACEMENT_3D ( 'NONE', #4965, #59399, #64701 ) ;
#9378 = DIRECTION ( 'NONE',  ( -1.000000000000000000, -3.016910393003147986E-15, -0.000000000000000000 ) ) ;
#9379 = EDGE_CURVE ( 'NONE', #15862, #20689, #62977, .T. ) ;
#9380 = ORIENTED_EDGE ( 'NONE', *, *, #45389, .F. ) ;
#9381 = EDGE_LOOP ( 'NONE', ( #44418, #15834, #34747, #21670 ) ) ;
#9382 = ADVANCED_FACE ( 'NONE', ( #22198 ), #38790, .T. ) ;
#9383 = ORIENTED_EDGE ( 'NONE', *, *, #18158, .F. ) ;
#9385 = EDGE_CURVE ( 'NONE', #29039, #16772, #68637, .T. ) ;
#9384 = CARTESIAN_POINT ( 'NONE',  ( 34.89999999999999858, -21.00000000000000000, 13.86939075806900057 ) ) ;
#9386 = DIRECTION ( 'NONE',  ( 0.000000000000000000, -0.7096009616570518874, 0.7046037717862339012 ) ) ;
#9387 = EDGE_CURVE ( 'NONE', #67890, #41002, #60010, .T. ) ;
#9388 = LINE ( 'NONE', #25670, #13393 ) ;
#9389 = CARTESIAN_POINT ( 'NONE',  ( 10.90000000000000036, 20.60000000000000142, -13.86939075806900057 ) ) ;
#9390 = CIRCLE ( 'NONE', #39838, 0.2000000000000005107 ) ;
#9391 = VERTEX_POINT ( 'NONE', #44098 ) ;
#9392 = ORIENTED_EDGE ( 'NONE', *, *, #46118, .T. ) ;
#9393 = FACE_OUTER_BOUND ( 'NONE', #64101, .T. ) ;
#9394 = CIRCLE ( 'NONE', #54579, 3.499999999999999556 ) ;
#9395 = DIRECTION ( 'NONE',  ( -0.000000000000000000, -0.000000000000000000, 1.000000000000000000 ) ) ;
#9396 = ORIENTED_EDGE ( 'NONE', *, *, #64847, .F. ) ;
#9397 = PRESENTATION_LAYER_ASSIGNMENT (  '', '', ( #68089 ) ) ;
#9398 = VERTEX_POINT ( 'NONE', #27496 ) ;
#9399 = ORIENTED_EDGE ( 'NONE', *, *, #63992, .T. ) ;
#9400 = ORIENTED_EDGE ( 'NONE', *, *, #40983, .T. ) ;
#9401 = DIRECTION ( 'NONE',  ( -0.000000000000000000, -0.000000000000000000, -1.000000000000000000 ) ) ;
#9402 = VECTOR ( 'NONE', #30644, 1000.000000000000000 ) ;
#9404 = VERTEX_POINT ( 'NONE', #10890 ) ;
#9403 = DIRECTION ( 'NONE',  ( -3.304235192336778667E-15, -1.000000000000000000, 0.000000000000000000 ) ) ;
#9405 = LINE ( 'NONE', #37335, #21001 ) ;
#9406 = DIRECTION ( 'NONE',  ( -1.000000000000000000, 0.000000000000000000, 0.000000000000000000 ) ) ;
#9407 = EDGE_CURVE ( 'NONE', #14976, #4599, #16549, .T. ) ;
#9408 = CYLINDRICAL_SURFACE ( 'NONE', #60653, 24.99999999998794920 ) ;
#9409 = ORIENTED_EDGE ( 'NONE', *, *, #15667, .T. ) ;
#9410 = ORIENTED_EDGE ( 'NONE', *, *, #7258, .F. ) ;
#9411 = VECTOR ( 'NONE', #63023, 1000.000000000000000 ) ;
#9412 = ADVANCED_FACE ( 'NONE', ( #66002 ), #37768, .F. ) ;
#9413 = DIRECTION ( 'NONE',  ( -4.336808689942025625E-15, -1.000000000000000000, 0.000000000000000000 ) ) ;
#9414 = VECTOR ( 'NONE', #21149, 1000.000000000000000 ) ;
#9415 = DIRECTION ( 'NONE',  ( 0.6414496315691592399, 0.7671651518152985405, 2.309356642088728176E-17 ) ) ;
#9416 = ORIENTED_EDGE ( 'NONE', *, *, #64770, .F. ) ;
#9417 = CARTESIAN_POINT ( 'NONE',  ( -2.530476262117229425, 9.547976262117158441, 54.00000000000000711 ) ) ;
#9418 = DIRECTION ( 'NONE',  ( 0.000000000000000000, 0.000000000000000000, -1.000000000000000000 ) ) ;
#9419 = DIRECTION ( 'NONE',  ( 1.000000000000000000, 0.000000000000000000, 0.000000000000000000 ) ) ;
#9420 = ORIENTED_EDGE ( 'NONE', *, *, #51400, .T. ) ;
#9421 = CARTESIAN_POINT ( 'NONE',  ( 18.85410196625000268, -17.50000000000000000, -21.50000000000000000 ) ) ;
#9422 = FACE_OUTER_BOUND ( 'NONE', #37927, .T. ) ;
#9423 = LINE ( 'NONE', #57156, #14981 ) ;
#9424 = LINE ( 'NONE', #30992, #66372 ) ;
#9425 = EDGE_CURVE ( 'NONE', #20373, #50555, #22544, .T. ) ;
#9426 = FACE_OUTER_BOUND ( 'NONE', #69733, .T. ) ;
#9427 = ORIENTED_EDGE ( 'NONE', *, *, #12560, .F. ) ;
#9428 = CARTESIAN_POINT ( 'NONE',  ( 6.665817930929297752, -7.357023737882824044, 54.00000000000000711 ) ) ;
#9429 = DIRECTION ( 'NONE',  ( -1.901462112903059913E-14, -1.000000000000000000, 0.000000000000000000 ) ) ;
#9430 = CARTESIAN_POINT ( 'NONE',  ( 7.250000000000004441, 7.450000000000001954, -14.00000000000000000 ) ) ;
#9431 = CARTESIAN_POINT ( 'NONE',  ( 7.250000000000005329, 8.250000000000001776, -22.00000000000000000 ) ) ;
#9432 = VECTOR ( 'NONE', #60815, 1000.000000000000000 ) ;
#9433 = DIRECTION ( 'NONE',  ( -1.836970198721029934E-16, -1.836970198721010706E-16, 1.000000000000000000 ) ) ;
#9434 = ADVANCED_FACE ( 'NONE', ( #33140, #55081 ), #22881, .T. ) ;
#9435 = PLANE ( 'NONE',  #39798 ) ;
#9436 = EDGE_CURVE ( 'NONE', #68196, #46286, #5589, .T. ) ;
#9437 = DIRECTION ( 'NONE',  ( 1.047444401652939849E-14, 1.000000000000000000, 1.836970198721029934E-16 ) ) ;
#9438 = CYLINDRICAL_SURFACE ( 'NONE', #9317, 25.39999999999999858 ) ;
#9439 = CIRCLE ( 'NONE', #33153, 0.3000000000005412781 ) ;
#9440 = ORIENTED_EDGE ( 'NONE', *, *, #50782, .F. ) ;
#9441 = AXIS2_PLACEMENT_3D ( 'NONE', #41485, #56343, #7887 ) ;
#9442 = DIRECTION ( 'NONE',  ( 0.000000000000000000, 0.000000000000000000, 1.000000000000000000 ) ) ;
#9443 = DIRECTION ( 'NONE',  ( 1.836970198721029934E-16, -1.836970198721036344E-16, 1.000000000000000000 ) ) ;
#9444 = EDGE_CURVE ( 'NONE', #57368, #24330, #43406, .T. ) ;
#9445 = CARTESIAN_POINT ( 'NONE',  ( -7.342976262117247188, -3.848229544836283100, 26.00000000000000711 ) ) ;
#9446 = EDGE_CURVE ( 'NONE', #51551, #41185, #69909, .T. ) ;
#9447 = EDGE_CURVE ( 'NONE', #30907, #33465, #54126, .T. ) ;
#9448 = CARTESIAN_POINT ( 'NONE',  ( -7.250000000000000888, 7.250000000000001776, -26.00000000000001066 ) ) ;
#9449 = CARTESIAN_POINT ( 'NONE',  ( 78.77321854994620765, 47.95351654967443977, 25.00000000000000000 ) ) ;
#9451 = VECTOR ( 'NONE', #65161, 1000.000000000000000 ) ;
#9450 = DIRECTION ( 'NONE',  ( 1.836970198721029934E-16, -1.836970198721036344E-16, 1.000000000000000000 ) ) ;
#9452 = DIRECTION ( 'NONE',  ( 1.000000000000000000, 0.000000000000000000, 0.000000000000000000 ) ) ;
#9453 = ORIENTED_EDGE ( 'NONE', *, *, #12936, .F. ) ;
#9454 = EDGE_CURVE ( 'NONE', #68361, #55546, #12597, .T. ) ;
#9455 = VERTEX_POINT ( 'NONE', #2693 ) ;
#9456 = CARTESIAN_POINT ( 'NONE',  ( -7.250000000000001776, -7.249999999999998224, -26.00000000000001066 ) ) ;
#9457 = EDGE_CURVE ( 'NONE', #40436, #56320, #12944, .T. ) ;
#9458 = LINE ( 'NONE', #15115, #38991 ) ;
#9459 = ORIENTED_EDGE ( 'NONE', *, *, #47053, .F. ) ;
#9460 = LINE ( 'NONE', #37045, #47284 ) ;
#9461 = EDGE_CURVE ( 'NONE', #25131, #7744, #68806, .T. ) ;
#9462 = DIRECTION ( 'NONE',  ( 1.000000000000000000, -0.000000000000000000, 0.000000000000000000 ) ) ;
#9463 = ORIENTED_EDGE ( 'NONE', *, *, #54492, .F. ) ;
#9464 = LINE ( 'NONE', #64263, #2921 ) ;
#9465 = ORIENTED_EDGE ( 'NONE', *, *, #2507, .F. ) ;
#9466 = ORIENTED_EDGE ( 'NONE', *, *, #56098, .F. ) ;
#9468 = EDGE_CURVE ( 'NONE', #41511, #69896, #29918, .T. ) ;
#9467 = LINE ( 'NONE', #62858, #5766 ) ;
#9469 = EDGE_LOOP ( 'NONE', ( #48990, #55312, #11434, #52614 ) ) ;
#9470 = ORIENTED_EDGE ( 'NONE', *, *, #3218, .T. ) ;
#9471 = EDGE_CURVE ( 'NONE', #33973, #15671, #66367, .T. ) ;
#9472 = CARTESIAN_POINT ( 'NONE',  ( -6.606374702650211539, -4.747751991980665665, 455.0000000000000568 ) ) ;
#9473 = CARTESIAN_POINT ( 'NONE',  ( -7.250000000000000888, 8.250000000000001776, -26.00000000000001066 ) ) ;
#9474 = LINE ( 'NONE', #41286, #58154 ) ;
#9475 = EDGE_LOOP ( 'NONE', ( #43140, #32942, #24178, #29793 ) ) ;
#9476 = AXIS2_PLACEMENT_3D ( 'NONE', #23165, #8287, #61686 ) ;
#9477 = DIRECTION ( 'NONE',  ( 1.000000000000000000, 0.000000000000000000, 0.000000000000000000 ) ) ;
#9479 = DIRECTION ( 'NONE',  ( 0.000000000000000000, 1.000000000000000000, 0.000000000000000000 ) ) ;
#9478 = CARTESIAN_POINT ( 'NONE',  ( 30.00000000000000000, -17.35230188589299871, 15.35019951917099945 ) ) ;
#9480 = ORIENTED_EDGE ( 'NONE', *, *, #2593, .F. ) ;
#9481 = VERTEX_POINT ( 'NONE', #23220 ) ;
#9482 = VERTEX_POINT ( 'NONE', #14003 ) ;
#9483 = FACE_OUTER_BOUND ( 'NONE', #43480, .T. ) ;
#9485 = ORIENTED_EDGE ( 'NONE', *, *, #32476, .T. ) ;
#9484 = CARTESIAN_POINT ( 'NONE',  ( 9.404523737882817258, -1.480523737882825985, 54.00000000000000711 ) ) ;
#9486 = CARTESIAN_POINT ( 'NONE',  ( 7.272650909786598561, -4.201500623656122535, 455.0000000000000568 ) ) ;
#9487 = VECTOR ( 'NONE', #33523, 1000.000000000000000 ) ;
#9488 = CIRCLE ( 'NONE', #38849, 2.000000000000001776 ) ;
#9489 = CARTESIAN_POINT ( 'NONE',  ( 289.5000000000000000, -0.5000000000000000000, -27.00000000000000000 ) ) ;
#9490 = VERTEX_POINT ( 'NONE', #34164 ) ;
#9491 = VERTEX_POINT ( 'NONE', #1646 ) ;
#9492 = VECTOR ( 'NONE', #49627, 1000.000000000000000 ) ;
#9493 = DIRECTION ( 'NONE',  ( -0.000000000000000000, -0.000000000000000000, -1.000000000000000000 ) ) ;
#9494 = ORIENTED_EDGE ( 'NONE', *, *, #29710, .T. ) ;
#9495 = EDGE_CURVE ( 'NONE', #28592, #54687, #17913, .T. ) ;
#9496 = CARTESIAN_POINT ( 'NONE',  ( 15.50000000000000000, 0.000000000000000000, 22.50000000000000000 ) ) ;
#9497 = CARTESIAN_POINT ( 'NONE',  ( 7.000000000000000000, -38.10000000000000142, 8.400000000000000355 ) ) ;
#9498 = AXIS2_PLACEMENT_3D ( 'NONE', #31080, #69613, #21509 ) ;
#9499 = VECTOR ( 'NONE', #56930, 1000.000000000000000 ) ;
#9500 = CARTESIAN_POINT ( 'NONE',  ( -4.727349090213560423, -7.811466277050794993, 455.0000000000000568 ) ) ;
#9501 = ORIENTED_EDGE ( 'NONE', *, *, #13183, .T. ) ;
#9502 = EDGE_CURVE ( 'NONE', #39173, #26484, #51139, .T. ) ;
#9503 = DIRECTION ( 'NONE',  ( 0.000000000000000000, 0.6857142857146703019, -0.7278708115914659382 ) ) ;
#9504 = CARTESIAN_POINT ( 'NONE',  ( 8.250000000000005329, 0.000000000000000000, -20.00000000000000000 ) ) ;
#9506 = ORIENTED_EDGE ( 'NONE', *, *, #30187, .T. ) ;
#9505 = CARTESIAN_POINT ( 'NONE',  ( 17.51999999999999957, -17.50000000000000000, -26.00000000000000355 ) ) ;
#9508 = VERTEX_POINT ( 'NONE', #61038 ) ;
#9507 = CARTESIAN_POINT ( 'NONE',  ( -8.393516549646712122, 7.603567055985436696, 455.0000000000000568 ) ) ;
#9509 = EDGE_CURVE ( 'NONE', #22867, #54447, #3282, .T. ) ;
#9510 = AXIS2_PLACEMENT_3D ( 'NONE', #37227, #53154, #4695 ) ;
#9511 = CARTESIAN_POINT ( 'NONE',  ( 41.09999999999999432, 13.66939075806899950, -20.80000000000000426 ) ) ;
#9512 = DIRECTION ( 'NONE',  ( 1.000000000000000000, 0.000000000000000000, 0.000000000000000000 ) ) ;
#9513 = EDGE_CURVE ( 'NONE', #56934, #59373, #45836, .T. ) ;
#9514 = LINE ( 'NONE', #30730, #55042 ) ;
#9515 = FACE_OUTER_BOUND ( 'NONE', #41752, .T. ) ;
#9516 = ADVANCED_FACE ( 'NONE', ( #2355 ), #56438, .F. ) ;
#9517 = DIRECTION ( 'NONE',  ( 0.7071067811865550112, 0.7071067811865401342, 0.000000000000000000 ) ) ;
#9518 = ORIENTED_EDGE ( 'NONE', *, *, #32161, .T. ) ;
#9519 = CARTESIAN_POINT ( 'NONE',  ( -11.50000000000000000, -12.00000000000000000, 10.69999999999999929 ) ) ;
#9520 = DIRECTION ( 'NONE',  ( 0.7671651518153043137, -0.6414496315691521344, 0.000000000000000000 ) ) ;
#9521 = FILL_AREA_STYLE_COLOUR ( '', #50374 ) ;
#9523 = ORIENTED_EDGE ( 'NONE', *, *, #42333, .T. ) ;
#9522 = DIRECTION ( 'NONE',  ( 0.000000000000000000, 0.000000000000000000, -1.000000000000000000 ) ) ;
#9524 =( BOUNDED_CURVE ( )  B_SPLINE_CURVE ( 3, ( #59428, #38553, #54815, #69699 ),
 .UNSPECIFIED., .F., .F. ) 
 B_SPLINE_CURVE_WITH_KNOTS ( ( 4, 4 ),
 ( 0.7227342478134280990, 0.8956647938578748969 ),
 .UNSPECIFIED. ) 
 CURVE ( )  GEOMETRIC_REPRESENTATION_ITEM ( )  RATIONAL_B_SPLINE_CURVE ( ( 1.000000000000000000, 0.9975094710839675916, 0.9975094710839675916, 1.000000000000000000 ) ) 
 REPRESENTATION_ITEM ( '' )  );
#9525 = CARTESIAN_POINT ( 'NONE',  ( -6.661338147750939243E-15, -20.50000000000000000, 17.79289321881346808 ) ) ;
#9526 = EDGE_CURVE ( 'NONE', #49662, #34559, #8928, .T. ) ;
#9527 = LINE ( 'NONE', #4924, #61199 ) ;
#9528 = EDGE_CURVE ( 'NONE', #46314, #62186, #17953, .T. ) ;
#9529 = DIRECTION ( 'NONE',  ( -1.000000000000000000, 0.000000000000000000, 0.000000000000000000 ) ) ;
#9530 = VERTEX_POINT ( 'NONE', #18970 ) ;
#9531 = CARTESIAN_POINT ( 'NONE',  ( 4.406483450353340103, -11.32648345035338089, 195.0000000000000284 ) ) ;
#9532 = DIRECTION ( 'NONE',  ( 0.000000000000000000, 0.000000000000000000, 1.000000000000000000 ) ) ;
#9533 = VECTOR ( 'NONE', #45161, 1000.000000000000000 ) ;
#9534 = ORIENTED_EDGE ( 'NONE', *, *, #22320, .F. ) ;
#9535 = ADVANCED_FACE ( 'NONE', ( #40527 ), #19311, .F. ) ;
#9536 = ADVANCED_FACE ( 'NONE', ( #23568 ), #8709, .F. ) ;
#9537 = FACE_OUTER_BOUND ( 'NONE', #13997, .T. ) ;
#9538 = DIRECTION ( 'NONE',  ( 1.000000000000000000, -0.000000000000000000, -0.000000000000000000 ) ) ;
#9539 = FACE_OUTER_BOUND ( 'NONE', #16889, .T. ) ;
#9540 = EDGE_CURVE ( 'NONE', #23385, #20190, #28865, .T. ) ;
#9541 = CYLINDRICAL_SURFACE ( 'NONE', #25244, 2.204799999999997429 ) ;
#9542 = VECTOR ( 'NONE', #39429, 1000.000000000000000 ) ;
#9543 = CIRCLE ( 'NONE', #52447, 0.1750000000000002387 ) ;
#9544 = VERTEX_POINT ( 'NONE', #53524 ) ;
#9545 = ORIENTED_EDGE ( 'NONE', *, *, #24016, .F. ) ;
#9546 = ORIENTED_EDGE ( 'NONE', *, *, #53805, .F. ) ;
#9547 = VERTEX_POINT ( 'NONE', #130 ) ;
#9548 = VERTEX_POINT ( 'NONE', #16736 ) ;
#9549 = CARTESIAN_POINT ( 'NONE',  ( 275.0000000000000000, -31.99999999999889866, 7.899999999997660893 ) ) ;
#9550 = VECTOR ( 'NONE', #7436, 1000.000000000000000 ) ;
#9551 = VECTOR ( 'NONE', #63438, 1000.000000000000000 ) ;
#9552 = CARTESIAN_POINT ( 'NONE',  ( 6.006483450353401921, 5.993516549646582092, 455.0000000000000568 ) ) ;
#9553 = AXIS2_PLACEMENT_3D ( 'NONE', #57294, #46329, #63305 ) ;
#9554 = DIRECTION ( 'NONE',  ( 1.000000000000000000, -0.000000000000000000, -0.000000000000000000 ) ) ;
#9555 = ORIENTED_EDGE ( 'NONE', *, *, #62482, .F. ) ;
#9556 = VERTEX_POINT ( 'NONE', #69788 ) ;
#9558 = EDGE_CURVE ( 'NONE', #5287, #10010, #55224, .T. ) ;
#9557 = CARTESIAN_POINT ( 'NONE',  ( 4.396432944014526889, -8.606483450353477949, 455.0000000000000568 ) ) ;
#9559 = EDGE_LOOP ( 'NONE', ( #11605, #19806, #2655, #30807 ) ) ;
#9560 = VERTEX_POINT ( 'NONE', #32644 ) ;
#9561 = ADVANCED_FACE ( 'NONE', ( #37954 ), #42554, .F. ) ;
#9562 = DIRECTION ( 'NONE',  ( -1.000000000000000000, 0.000000000000000000, 0.000000000000000000 ) ) ;
#9563 = LINE ( 'NONE', #32535, #59567 ) ;
#9564 = CARTESIAN_POINT ( 'NONE',  ( 29.89999999999999858, -21.00000000000000000, 13.86939075806900057 ) ) ;
#9565 = AXIS2_PLACEMENT_3D ( 'NONE', #30459, #62275, #62989 ) ;
#9566 = ORIENTED_EDGE ( 'NONE', *, *, #24675, .F. ) ;
#9567 = VECTOR ( 'NONE', #38527, 1000.000000000000000 ) ;
#9568 = LINE ( 'NONE', #37143, #11988 ) ;
#9570 = DIRECTION ( 'NONE',  ( -1.836970198721029934E-16, 1.836970198721036590E-16, -1.000000000000000000 ) ) ;
#9569 = CARTESIAN_POINT ( 'NONE',  ( 29.50000000000000355, -12.00000000000000000, 11.00000000000000000 ) ) ;
#9571 = ORIENTED_EDGE ( 'NONE', *, *, #36542, .F. ) ;
#9573 = EDGE_LOOP ( 'NONE', ( #52611, #39795, #27333, #38460 ) ) ;
#9572 = FACE_OUTER_BOUND ( 'NONE', #39219, .T. ) ;
#9574 = EDGE_LOOP ( 'NONE', ( #42383, #26185 ) ) ;
#9575 = LINE ( 'NONE', #31149, #35557 ) ;
#9576 = CARTESIAN_POINT ( 'NONE',  ( 283.0000000000000568, -32.46196062927499781, 8.091291340630698770 ) ) ;
#9577 = ORIENTED_EDGE ( 'NONE', *, *, #25288, .T. ) ;
#9578 = ORIENTED_EDGE ( 'NONE', *, *, #21127, .F. ) ;
#9579 = CARTESIAN_POINT ( 'NONE',  ( -6.651770455163775964, -7.357023737882784964, 26.00000000000000000 ) ) ;
#9580 = CARTESIAN_POINT ( 'NONE',  ( 7.250000000000004441, 7.450000000000001954, -16.50000000000000000 ) ) ;
#9581 = VECTOR ( 'NONE', #43718, 1000.000000000000000 ) ;
#9582 = ORIENTED_EDGE ( 'NONE', *, *, #5685, .F. ) ;
#9583 = ORIENTED_EDGE ( 'NONE', *, *, #20014, .F. ) ;
#9584 = CARTESIAN_POINT ( 'NONE',  ( -11.00000000000000000, -17.14999999999999858, -27.00000000000000000 ) ) ;
#9585 = DIRECTION ( 'NONE',  ( 0.000000000000000000, 0.7071067811865475727, -0.7071067811865475727 ) ) ;
#9586 = ORIENTED_EDGE ( 'NONE', *, *, #385, .F. ) ;
#9587 = EDGE_CURVE ( 'NONE', #11595, #27939, #5778, .T. ) ;
#9588 = AXIS2_PLACEMENT_3D ( 'NONE', #37193, #5371, #10644 ) ;
#9589 = AXIS2_PLACEMENT_3D ( 'NONE', #34591, #50855, #2428 ) ;
#9590 = DIRECTION ( 'NONE',  ( -0.5773502691896257311, -0.5773502691896257311, 0.5773502691896257311 ) ) ;
#9591 = CARTESIAN_POINT ( 'NONE',  ( -15.50000000000000000, -0.1999999999999999556, -22.50000000000000000 ) ) ;
#9593 = VERTEX_POINT ( 'NONE', #470 ) ;
#9592 = DIRECTION ( 'NONE',  ( -1.000000000000000000, 0.000000000000000000, 0.000000000000000000 ) ) ;
#9595 = VERTEX_POINT ( 'NONE', #37260 ) ;
#9594 = CARTESIAN_POINT ( 'NONE',  ( 275.0000000000000000, -38.15000000000000568, 13.19999999999999929 ) ) ;
#9596 = EDGE_CURVE ( 'NONE', #6050, #23985, #38324, .T. ) ;
#9597 = DIRECTION ( 'NONE',  ( -0.000000000000000000, 1.000000000000000000, -0.000000000000000000 ) ) ;
#9598 = CIRCLE ( 'NONE', #46830, 0.1749999999999998224 ) ;
#9599 = CARTESIAN_POINT ( 'NONE',  ( -29.50000000000000355, -11.50000000000000000, -15.00000000000000000 ) ) ;
#9600 = EDGE_CURVE ( 'NONE', #25515, #28299, #11413, .T. ) ;
#9601 = DIRECTION ( 'NONE',  ( -1.000000000000000000, 0.000000000000000000, 0.000000000000000000 ) ) ;
#9602 = EDGE_CURVE ( 'NONE', #41191, #58562, #48556, .T. ) ;
#9603 = CARTESIAN_POINT ( 'NONE',  ( 11.50000000000000000, -12.00000000000000000, -10.52786404500095863 ) ) ;
#9604 = CARTESIAN_POINT ( 'NONE',  ( 10.20488345035338007, -11.48848345035339769, 195.0000000000000284 ) ) ;
#9605 = VECTOR ( 'NONE', #52259, 1000.000000000000000 ) ;
#9606 = ADVANCED_FACE ( 'NONE', ( #42899 ), #21687, .T. ) ;
#9607 = EDGE_CURVE ( 'NONE', #50982, #11259, #48910, .T. ) ;
#9608 = CARTESIAN_POINT ( 'NONE',  ( 16.89999999999999858, 13.66939075806899240, 20.79999999999999361 ) ) ;
#9609 = VERTEX_POINT ( 'NONE', #31951 ) ;
#9610 = DIRECTION ( 'NONE',  ( 0.000000000000000000, 1.000000000000000000, 0.000000000000000000 ) ) ;
#9612 = EDGE_LOOP ( 'NONE', ( #34316, #68815, #51307, #55290 ) ) ;
#9611 = LINE ( 'NONE', #47428, #51442 ) ;
#9613 = CARTESIAN_POINT ( 'NONE',  ( 11.78648345035340839, 7.813516549646560172, 455.0000000000000568 ) ) ;
#9614 = VECTOR ( 'NONE', #69180, 1000.000000000000000 ) ;
#9615 = CARTESIAN_POINT ( 'NONE',  ( 13.90000000000000213, 13.66939075806899240, 20.79999999999999361 ) ) ;
#9616 = EDGE_CURVE ( 'NONE', #43669, #47649, #63097, .T. ) ;
#9617 = CARTESIAN_POINT ( 'NONE',  ( 7.000000000000000000, -32.44999999999905071, 14.49999999999906031 ) ) ;
#9618 = VECTOR ( 'NONE', #58209, 1000.000000000000000 ) ;
#9619 = LINE ( 'NONE', #62642, #22813 ) ;
#9620 = VERTEX_POINT ( 'NONE', #58828 ) ;
#9621 = CARTESIAN_POINT ( 'NONE',  ( -16.75000000000000000, -0.2038245569916330158, 21.77831216351300014 ) ) ;
#9622 = DIRECTION ( 'NONE',  ( 1.000000000000000000, 0.000000000000000000, 0.000000000000000000 ) ) ;
#9623 = EDGE_LOOP ( 'NONE', ( #49197, #33738, #24529, #42065, #41156, #21144, #46090, #61890 ) ) ;
#9624 = LINE ( 'NONE', #31199, #61656 ) ;
#9625 = CARTESIAN_POINT ( 'NONE',  ( 19.90000000000000213, 20.60000000000000142, -13.86939075806900057 ) ) ;
#9626 = CARTESIAN_POINT ( 'NONE',  ( -4.135079735113215804, -6.836383711243002814, 54.00000000000000711 ) ) ;
#9627 = ORIENTED_EDGE ( 'NONE', *, *, #21200, .T. ) ;
#9628 = CARTESIAN_POINT ( 'NONE',  ( -4.734785091274035018, -6.619341603356897252, 455.0000000000000568 ) ) ;
#9629 = ORIENTED_EDGE ( 'NONE', *, *, #43323, .T. ) ;
#9630 = ORIENTED_EDGE ( 'NONE', *, *, #22521, .F. ) ;
#9631 = CARTESIAN_POINT ( 'NONE',  ( 1.634292677759859869, -8.241237374594282628, 54.00000000000000711 ) ) ;
#9632 = CARTESIAN_POINT ( 'NONE',  ( -9.942044687070573872, -2.765062094116047309, 455.0000000000000568 ) ) ;
#9633 = LINE ( 'NONE', #3271, #50293 ) ;
#9634 = AXIS2_PLACEMENT_3D ( 'NONE', #16416, #37990, #53218 ) ;
#9635 = FACE_OUTER_BOUND ( 'NONE', #21895, .T. ) ;
#9636 = VECTOR ( 'NONE', #18289, 1000.000000000000114 ) ;
#9637 = LINE ( 'NONE', #42508, #8039 ) ;
#9638 = VERTEX_POINT ( 'NONE', #64823 ) ;
#9639 = ORIENTED_EDGE ( 'NONE', *, *, #69950, .F. ) ;
#9641 = ORIENTED_EDGE ( 'NONE', *, *, #45495, .F. ) ;
#9640 = LINE ( 'NONE', #41805, #50966 ) ;
#9642 = ORIENTED_EDGE ( 'NONE', *, *, #4244, .T. ) ;
#9643 = EDGE_CURVE ( 'NONE', #62060, #27405, #66467, .T. ) ;
#9644 = CIRCLE ( 'NONE', #45757, 0.5999999999999998668 ) ;
#9645 = AXIS2_PLACEMENT_3D ( 'NONE', #14828, #51609, #30032 ) ;
#9646 = AXIS2_PLACEMENT_3D ( 'NONE', #17559, #24535, #40440 ) ;
#9647 = LINE ( 'NONE', #69746, #51821 ) ;
#9648 = DIRECTION ( 'NONE',  ( 1.836970198721029934E-16, 1.836970198721010706E-16, -1.000000000000000000 ) ) ;
#9649 = DIRECTION ( 'NONE',  ( 0.000000000000000000, 0.000000000000000000, 1.000000000000000000 ) ) ;
#9650 = EDGE_CURVE ( 'NONE', #29479, #48363, #16377, .T. ) ;
#9651 = DIRECTION ( 'NONE',  ( 0.000000000000000000, 0.000000000000000000, 1.000000000000000000 ) ) ;
#9652 = VECTOR ( 'NONE', #68531, 1000.000000000000000 ) ;
#9653 = VECTOR ( 'NONE', #3644, 1000.000000000000000 ) ;
#9655 = LINE ( 'NONE', #31921, #24427 ) ;
#9654 = CARTESIAN_POINT ( 'NONE',  ( 31.89999999999999858, 0.000000000000000000, 2.585923194002694273E-15 ) ) ;
#9656 = VERTEX_POINT ( 'NONE', #11077 ) ;
#9657 = ORIENTED_EDGE ( 'NONE', *, *, #12767, .T. ) ;
#9658 = EDGE_CURVE ( 'NONE', #20610, #37207, #26644, .T. ) ;
#9659 = ORIENTED_EDGE ( 'NONE', *, *, #50818, .F. ) ;
#9660 = EDGE_CURVE ( 'NONE', #58661, #53780, #15336, .T. ) ;
#9662 = ORIENTED_EDGE ( 'NONE', *, *, #60407, .T. ) ;
#9661 = VECTOR ( 'NONE', #53848, 1000.000000000000000 ) ;
#9663 = DIRECTION ( 'NONE',  ( 0.000000000000000000, 0.000000000000000000, 1.000000000000000000 ) ) ;
#9664 = LINE ( 'NONE', #31238, #38906 ) ;
#9665 = DIRECTION ( 'NONE',  ( 0.000000000000000000, 0.000000000000000000, 1.000000000000000000 ) ) ;
#9666 = CARTESIAN_POINT ( 'NONE',  ( 9.899999999999998579, -0.2000000000000000111, 0.000000000000000000 ) ) ;
#9667 = ORIENTED_EDGE ( 'NONE', *, *, #13891, .F. ) ;
#9668 = ORIENTED_EDGE ( 'NONE', *, *, #39635, .T. ) ;
#9669 = ORIENTED_EDGE ( 'NONE', *, *, #59209, .T. ) ;
#9670 = AXIS2_PLACEMENT_3D ( 'NONE', #3956, #64071, #67955 ) ;
#9671 = DIRECTION ( 'NONE',  ( 0.6414496315691494699, 0.7671651518153064231, 2.818519042764025305E-16 ) ) ;
#9672 = ORIENTED_EDGE ( 'NONE', *, *, #10320, .F. ) ;
#9673 = ORIENTED_EDGE ( 'NONE', *, *, #42802, .T. ) ;
#9674 = FACE_OUTER_BOUND ( 'NONE', #169, .T. ) ;
#9675 = ORIENTED_EDGE ( 'NONE', *, *, #38577, .T. ) ;
#9676 = ORIENTED_EDGE ( 'NONE', *, *, #63743, .T. ) ;
#9677 = CARTESIAN_POINT ( 'NONE',  ( 280.0000000000000000, -25.50000000000000355, 20.00000000000000000 ) ) ;
#9679 = VERTEX_POINT ( 'NONE', #31611 ) ;
#9678 = CARTESIAN_POINT ( 'NONE',  ( -8.393516549646744096, -4.396432944014549093, 455.0000000000000568 ) ) ;
#9680 = ORIENTED_EDGE ( 'NONE', *, *, #15672, .F. ) ;
#9681 = EDGE_CURVE ( 'NONE', #46263, #11892, #53186, .T. ) ;
#9682 = CARTESIAN_POINT ( 'NONE',  ( -7.250000000000001776, -7.249999999999998224, -13.50000000000000178 ) ) ;
#9683 = CARTESIAN_POINT ( 'NONE',  ( 55.00000000000000000, 0.000000000000000000, 0.000000000000000000 ) ) ;
#9684 = AXIS2_PLACEMENT_3D ( 'NONE', #37086, #47681, #37773 ) ;
#9686 = ORIENTED_EDGE ( 'NONE', *, *, #11091, .T. ) ;
#9685 = LINE ( 'NONE', #52468, #37982 ) ;
#9687 = VERTEX_POINT ( 'NONE', #69429 ) ;
#9688 = DIRECTION ( 'NONE',  ( 0.000000000000000000, 1.000000000000000000, -0.000000000000000000 ) ) ;
#9689 = VECTOR ( 'NONE', #49464, 1000.000000000000000 ) ;
#9690 = CARTESIAN_POINT ( 'NONE',  ( 9.900000000000000355, -0.000000000000000000, 20.80000000000000426 ) ) ;
#9691 = PLANE ( 'NONE',  #42502 ) ;
#9692 = DIRECTION ( 'NONE',  ( -0.000000000000000000, 3.673940397442059868E-16, -1.000000000000000000 ) ) ;
#9693 = CIRCLE ( 'NONE', #15342, 2.204799999999997429 ) ;
#9694 = EDGE_CURVE ( 'NONE', #3757, #46850, #20980, .T. ) ;
#9695 = EDGE_CURVE ( 'NONE', #135, #19031, #63823, .T. ) ;
#9696 = ORIENTED_EDGE ( 'NONE', *, *, #22019, .T. ) ;
#9697 = DIRECTION ( 'NONE',  ( 0.000000000000000000, 0.000000000000000000, -1.000000000000000000 ) ) ;
#9698 = AXIS2_PLACEMENT_3D ( 'NONE', #37025, #9798, #58923 ) ;
#9700 = DIRECTION ( 'NONE',  ( 1.883404846338789915E-14, 1.000000000000000000, 1.836970198721045218E-16 ) ) ;
#9699 = VECTOR ( 'NONE', #49916, 1000.000000000000000 ) ;
#9701 = DIRECTION ( 'NONE',  ( 0.8660254037844482555, 0.000000000000000000, 0.4999999999999831801 ) ) ;
#9702 = ADVANCED_FACE ( 'NONE', ( #831 ), #28705, .F. ) ;
#9703 = CARTESIAN_POINT ( 'NONE',  ( -7.250000000000000888, 7.450000000000003730, -21.50000000000000000 ) ) ;
#9704 = FACE_OUTER_BOUND ( 'NONE', #12138, .T. ) ;
#9705 = AXIS2_PLACEMENT_3D ( 'NONE', #66627, #62715, #1932 ) ;
#9706 = AXIS2_PLACEMENT_3D ( 'NONE', #62483, #3462, #62139 ) ;
#9707 = AXIS2_PLACEMENT_3D ( 'NONE', #50242, #50597, #13458 ) ;
#9708 = CARTESIAN_POINT ( 'NONE',  ( 7.250000000000005329, 7.250000000000000888, -18.50000000000000000 ) ) ;
#9709 = ORIENTED_EDGE ( 'NONE', *, *, #11207, .F. ) ;
#9710 = VECTOR ( 'NONE', #21193, 1000.000000000000000 ) ;
#9711 = DIRECTION ( 'NONE',  ( 0.000000000000000000, 0.000000000000000000, 1.000000000000000000 ) ) ;
#9712 = DIRECTION ( 'NONE',  ( -1.000000000000000000, 0.000000000000000000, 0.000000000000000000 ) ) ;
#9713 = LINE ( 'NONE', #20309, #4502 ) ;
#9714 = ORIENTED_EDGE ( 'NONE', *, *, #25668, .T. ) ;
#9715 = CARTESIAN_POINT ( 'NONE',  ( 41.09999999999999432, -14.06939075806901940, -20.80000000000000426 ) ) ;
#9716 = CYLINDRICAL_SURFACE ( 'NONE', #39975, 4.000000000000000000 ) ;
#9717 = DIRECTION ( 'NONE',  ( 0.000000000000000000, 1.000000000000000000, 0.000000000000000000 ) ) ;
#9718 = DIRECTION ( 'NONE',  ( 1.000000000000000000, -0.000000000000000000, -0.000000000000000000 ) ) ;
#9719 = DIRECTION ( 'NONE',  ( 0.000000000000000000, 0.000000000000000000, 1.000000000000000000 ) ) ;
#9720 = EDGE_LOOP ( 'NONE', ( #51170, #29471, #65429, #11021 ) ) ;
#9721 = LINE ( 'NONE', #62387, #8442 ) ;
#9722 = DIRECTION ( 'NONE',  ( -1.000000000000000000, 0.000000000000000000, -0.000000000000000000 ) ) ;
#9723 = CARTESIAN_POINT ( 'NONE',  ( 30.00000000000000000, -10.85999999999999943, 9.350000000000269651 ) ) ;
#9724 = CARTESIAN_POINT ( 'NONE',  ( 78.77321854994620765, 47.95351654967443977, 29.00000000000000000 ) ) ;
#9725 = PLANE ( 'NONE',  #28300 ) ;
#9726 = ORIENTED_EDGE ( 'NONE', *, *, #46045, .T. ) ;
#9728 = ORIENTED_EDGE ( 'NONE', *, *, #44487, .F. ) ;
#9727 = DIRECTION ( 'NONE',  ( 0.000000000000000000, -1.000000000000000000, 0.000000000000000000 ) ) ;
#9729 = CARTESIAN_POINT ( 'NONE',  ( 7.450000000000006395, 7.250000000000000888, -10.50000000000000000 ) ) ;
#9730 = LINE ( 'NONE', #30944, #65107 ) ;
#9731 = DIRECTION ( 'NONE',  ( -1.000000000000000000, 0.000000000000000000, 0.000000000000000000 ) ) ;
#9732 = EDGE_LOOP ( 'NONE', ( #18251, #64042, #60061, #21885, #19597, #61004, #14508 ) ) ;
#9733 = MECHANICAL_DESIGN_GEOMETRIC_PRESENTATION_REPRESENTATION (  '', ( #53749 ), #23227 ) ;
#9734 = EDGE_CURVE ( 'NONE', #9638, #45723, #6467, .T. ) ;
#9735 = ADVANCED_FACE ( 'NONE', ( #28361 ), #23755, .F. ) ;
#9736 = EDGE_CURVE ( 'NONE', #55561, #52369, #6114, .T. ) ;
#9737 = DIRECTION ( 'NONE',  ( -3.491481338843133355E-15, -1.000000000000000000, -1.836970198721029934E-16 ) ) ;
#9738 = CARTESIAN_POINT ( 'NONE',  ( 7.000000000000000000, -21.00000000000000000, 0.000000000000000000 ) ) ;
#9739 = VECTOR ( 'NONE', #65967, 1000.000000000000000 ) ;
#9740 = VERTEX_POINT ( 'NONE', #60875 ) ;
#9741 = ORIENTED_EDGE ( 'NONE', *, *, #48472, .T. ) ;
#9742 = EDGE_CURVE ( 'NONE', #65973, #34373, #6788, .T. ) ;
#9743 = CIRCLE ( 'NONE', #14277, 24.99999999998784972 ) ;
#9744 = VERTEX_POINT ( 'NONE', #55933 ) ;
#9745 = DIRECTION ( 'NONE',  ( -0.5773502691896257311, 0.5773502691896257311, -0.5773502691896257311 ) ) ;
#9746 = DIRECTION ( 'NONE',  ( -0.000000000000000000, 0.000000000000000000, 1.000000000000000000 ) ) ;
#9747 = DIRECTION ( 'NONE',  ( 0.000000000000000000, 0.7071067811865474617, -0.7071067811865474617 ) ) ;
#9748 = VECTOR ( 'NONE', #45247, 1000.000000000000000 ) ;
#9749 = AXIS2_PLACEMENT_3D ( 'NONE', #49497, #1732, #66442 ) ;
#9750 = ORIENTED_EDGE ( 'NONE', *, *, #14123, .T. ) ;
#9751 = ORIENTED_EDGE ( 'NONE', *, *, #55708, .F. ) ;
#9752 = DIRECTION ( 'NONE',  ( -1.000000000000000000, 1.952517519553884087E-14, 0.000000000000000000 ) ) ;
#9753 = LINE ( 'NONE', #64201, #24 ) ;
#9754 = AXIS2_PLACEMENT_3D ( 'NONE', #13846, #60879, #66543 ) ;
#9755 = AXIS2_PLACEMENT_3D ( 'NONE', #43559, #21655, #48877 ) ;
#9756 = VECTOR ( 'NONE', #348, 1000.000000000000000 ) ;
#9757 = ORIENTED_EDGE ( 'NONE', *, *, #7717, .T. ) ;
#9758 = ORIENTED_EDGE ( 'NONE', *, *, #66000, .F. ) ;
#9759 = ORIENTED_EDGE ( 'NONE', *, *, #49640, .F. ) ;
#9760 = ORIENTED_EDGE ( 'NONE', *, *, #1190, .T. ) ;
#9761 = VECTOR ( 'NONE', #40447, 1000.000000000000000 ) ;
#9762 = DIRECTION ( 'NONE',  ( 1.000000000000000000, 0.000000000000000000, 0.000000000000000000 ) ) ;
#9763 = UNCERTAINTY_MEASURE_WITH_UNIT (LENGTH_MEASURE( 1.000000000000000082E-05 ), #4671, 'distance_accuracy_value', 'NONE');
#9765 = ORIENTED_EDGE ( 'NONE', *, *, #60633, .T. ) ;
#9764 = LINE ( 'NONE', #20704, #41266 ) ;
#9766 = PLANE ( 'NONE',  #33420 ) ;
#9767 = VECTOR ( 'NONE', #51882, 1000.000000000000000 ) ;
#9768 = CARTESIAN_POINT ( 'NONE',  ( -7.450000000000001954, -7.249999999999998224, -17.50000000000000000 ) ) ;
#9769 = DIRECTION ( 'NONE',  ( -0.000000000000000000, -0.000000000000000000, -1.000000000000000000 ) ) ;
#9770 = ORIENTED_EDGE ( 'NONE', *, *, #8670, .T. ) ;
#9771 = ORIENTED_EDGE ( 'NONE', *, *, #16869, .F. ) ;
#9772 = DIRECTION ( 'NONE',  ( 0.000000000000000000, 0.000000000000000000, 1.000000000000000000 ) ) ;
#9773 = CARTESIAN_POINT ( 'NONE',  ( 6.364920264886885448, -6.836383711243021466, 54.00000000000000711 ) ) ;
#9774 = ORIENTED_EDGE ( 'NONE', *, *, #16425, .F. ) ;
#9775 = EDGE_CURVE ( 'NONE', #20378, #15085, #22028, .T. ) ;
#9776 = DIRECTION ( 'NONE',  ( 0.000000000000000000, 0.000000000000000000, -1.000000000000000000 ) ) ;
#9777 = EDGE_CURVE ( 'NONE', #22677, #373, #58165, .T. ) ;
#9778 = EDGE_CURVE ( 'NONE', #67923, #22000, #39656, .T. ) ;
#9779 = AXIS2_PLACEMENT_3D ( 'NONE', #61228, #46037, #12792 ) ;
#9780 = DIRECTION ( 'NONE',  ( -1.000000000000000000, 1.047444401652940007E-14, -1.836970198721010706E-16 ) ) ;
#9781 = ORIENTED_EDGE ( 'NONE', *, *, #28508, .T. ) ;
#9782 = DIRECTION ( 'NONE',  ( 0.000000000000000000, -0.000000000000000000, 1.000000000000000000 ) ) ;
#9783 = CARTESIAN_POINT ( 'NONE',  ( -11.75000000000000000, -5.000000000000000000, -21.10805890929250239 ) ) ;
#9784 = DIRECTION ( 'NONE',  ( 0.4999999999999785727, -0.8660254037844510311, 0.000000000000000000 ) ) ;
#9785 = EDGE_CURVE ( 'NONE', #62156, #1825, #61213, .T. ) ;
#9786 = VECTOR ( 'NONE', #6518, 1000.000000000000000 ) ;
#9787 = DIRECTION ( 'NONE',  ( -1.000000000000000000, 0.000000000000000000, 0.000000000000000000 ) ) ;
#9788 = PRODUCT_DEFINITION ( 'UNKNOWN', '', #34698, #7705 ) ;
#9789 = AXIS2_PLACEMENT_3D ( 'NONE', #44186, #23323, #54817 ) ;
#9790 = AXIS2_PLACEMENT_3D ( 'NONE', #42806, #48820, #10288 ) ;
#9791 = DIRECTION ( 'NONE',  ( -0.000000000000000000, -0.000000000000000000, -1.000000000000000000 ) ) ;
#9792 = EDGE_CURVE ( 'NONE', #22032, #41339, #66009, .T. ) ;
#9793 = ORIENTED_EDGE ( 'NONE', *, *, #60442, .T. ) ;
#9794 = DIRECTION ( 'NONE',  ( 1.000000000000000000, -0.000000000000000000, 0.000000000000000000 ) ) ;
#9795 = DIRECTION ( 'NONE',  ( -0.000000000000000000, -0.000000000000000000, -1.000000000000000000 ) ) ;
#9797 = EDGE_CURVE ( 'NONE', #14276, #52784, #62640, .T. ) ;
#9796 = CARTESIAN_POINT ( 'NONE',  ( 37.90000000000000568, -0.2000000000089119934, 8.909539772616881237E-12 ) ) ;
#9798 = DIRECTION ( 'NONE',  ( 0.000000000000000000, 0.000000000000000000, -1.000000000000000000 ) ) ;
#9799 = VECTOR ( 'NONE', #65290, 1000.000000000000114 ) ;
#9800 = VECTOR ( 'NONE', #62924, 1000.000000000000000 ) ;
#9801 = EDGE_LOOP ( 'NONE', ( #43853, #68201, #12579, #38778 ) ) ;
#9802 = CARTESIAN_POINT ( 'NONE',  ( 7.750000000000001776, 7.750000000000000000, 0.000000000000000000 ) ) ;
#9803 = LINE ( 'NONE', #5533, #64657 ) ;
#9804 = AXIS2_PLACEMENT_3D ( 'NONE', #56285, #23759, #7830 ) ;
#9805 = CARTESIAN_POINT ( 'NONE',  ( 30.00000000000000000, -17.35230188589299871, 15.35019951917099945 ) ) ;
#9806 = AXIS2_PLACEMENT_3D ( 'NONE', #24252, #29901, #34846 ) ;
#9807 = CARTESIAN_POINT ( 'NONE',  ( 11.00000000000000000, -11.50000000000100009, 15.00000000000084910 ) ) ;
#9808 = VERTEX_POINT ( 'NONE', #23414 ) ;
#9809 = DIRECTION ( 'NONE',  ( 0.000000000000000000, -0.000000000000000000, 1.000000000000000000 ) ) ;
#9810 = CARTESIAN_POINT ( 'NONE',  ( 0.000000000000000000, -7.449999999999998401, -12.50000000000000000 ) ) ;
#9811 = CARTESIAN_POINT ( 'NONE',  ( -11.11351654964671098, 4.193516549646605363, 195.0000000000000284 ) ) ;
#9812 = AXIS2_PLACEMENT_3D ( 'NONE', #62177, #8078, #3499 ) ;
#9813 = DIRECTION ( 'NONE',  ( -0.000000000000000000, -0.000000000000000000, 1.000000000000000000 ) ) ;
#9814 = FACE_OUTER_BOUND ( 'NONE', #2851, .T. ) ;
#9815 = FACE_OUTER_BOUND ( 'NONE', #50868, .T. ) ;
#9816 = VERTEX_POINT ( 'NONE', #38639 ) ;
#9817 = AXIS2_PLACEMENT_3D ( 'NONE', #52838, #63425, #14988 ) ;
#9818 = EDGE_LOOP ( 'NONE', ( #58424, #59515, #54866, #59126, #40523, #22058, #39873, #31580, #28158, #5927, #58230, #52114, #2873, #29087 ) ) ;
#9819 = LINE ( 'NONE', #31020, #48500 ) ;
#9820 = DIRECTION ( 'NONE',  ( 0.000000000000000000, 0.000000000000000000, 1.000000000000000000 ) ) ;
#9821 = ORIENTED_EDGE ( 'NONE', *, *, #5310, .T. ) ;
#9822 = CYLINDRICAL_SURFACE ( 'NONE', #67575, 0.1999999999999992339 ) ;
#9823 = CARTESIAN_POINT ( 'NONE',  ( -7.172176262117259782, 5.242976262117182706, 54.00000000000000711 ) ) ;
#9824 = VERTEX_POINT ( 'NONE', #45306 ) ;
#9825 = CARTESIAN_POINT ( 'NONE',  ( 39.90000000000000568, -16.96999999999999886, -21.00000000000000000 ) ) ;
#9826 = VERTEX_POINT ( 'NONE', #17759 ) ;
#9827 = ORIENTED_EDGE ( 'NONE', *, *, #28657, .T. ) ;
#9828 = DIRECTION ( 'NONE',  ( 1.000000000000000000, 0.000000000000000000, 0.000000000000000000 ) ) ;
#9829 = VERTEX_POINT ( 'NONE', #22720 ) ;
#9830 = CARTESIAN_POINT ( 'NONE',  ( -11.07551654964667520, 9.791916549646639822, 455.0000000000000568 ) ) ;
#9831 = DIRECTION ( 'NONE',  ( 0.6414496315691592399, 0.7671651518152985405, 2.309356642088728176E-17 ) ) ;
#9832 = CARTESIAN_POINT ( 'NONE',  ( 7.969523737882818537, -8.835729544836345539, 54.00000000000000711 ) ) ;
#9833 = CIRCLE ( 'NONE', #33488, 24.99999999998794920 ) ;
#9834 = EDGE_LOOP ( 'NONE', ( #25035, #41635, #67390, #26862 ) ) ;
#9835 = DIRECTION ( 'NONE',  ( -0.000000000000000000, -0.000000000000000000, -1.000000000000000000 ) ) ;
#9837 = CARTESIAN_POINT ( 'NONE',  ( 4.961189459950046121, 7.342976262117201003, 54.00000000000000711 ) ) ;
#9836 = CARTESIAN_POINT ( 'NONE',  ( -8.250000000000001776, -8.249999999999998224, -26.00000000000001066 ) ) ;
#9838 = EDGE_CURVE ( 'NONE', #59053, #21746, #18089, .T. ) ;
#9839 = VERTEX_POINT ( 'NONE', #29058 ) ;
#9840 = EDGE_LOOP ( 'NONE', ( #623, #64209, #59837, #68782 ) ) ;
#9841 = CIRCLE ( 'NONE', #58226, 0.5000000000000000000 ) ;
#9842 = VERTEX_POINT ( 'NONE', #34340 ) ;
#9843 = ORIENTED_EDGE ( 'NONE', *, *, #59125, .F. ) ;
#9844 = VECTOR ( 'NONE', #17240, 1000.000000000000000 ) ;
#9845 = VECTOR ( 'NONE', #27855, 1000.000000000000000 ) ;
#9846 = EDGE_CURVE ( 'NONE', #45732, #37491, #33334, .T. ) ;
#9847 = DIRECTION ( 'NONE',  ( 0.000000000000000000, -1.000000000000000000, 0.000000000000000000 ) ) ;
#9849 = VERTEX_POINT ( 'NONE', #7482 ) ;
#9848 = LINE ( 'NONE', #15833, #69233 ) ;
#9850 = VECTOR ( 'NONE', #1239, 1000.000000000000000 ) ;
#9851 = LINE ( 'NONE', #21153, #43566 ) ;
#9852 = CARTESIAN_POINT ( 'NONE',  ( 25.50000000000000355, -15.50000000000000000, -22.50000000000000000 ) ) ;
#9853 = ORIENTED_EDGE ( 'NONE', *, *, #21924, .T. ) ;
#9854 = ADVANCED_FACE ( 'NONE', ( #65848 ), #28030, .F. ) ;
#9855 = ORIENTED_EDGE ( 'NONE', *, *, #31515, .F. ) ;
#9856 = CIRCLE ( 'NONE', #33606, 6.000000000000005329 ) ;
#9857 = VECTOR ( 'NONE', #41017, 1000.000000000000000 ) ;
#9858 = CARTESIAN_POINT ( 'NONE',  ( 0.000000000000000000, -7.449999999999998401, -10.50000000000000000 ) ) ;
#9859 = ADVANCED_FACE ( 'NONE', ( #49589 ), #1161, .T. ) ;
#9860 = ORIENTED_EDGE ( 'NONE', *, *, #37274, .T. ) ;
#9861 = CARTESIAN_POINT ( 'NONE',  ( 28.00000000000000000, -15.50000000000000000, 20.05051025721700242 ) ) ;
#9863 = CYLINDRICAL_SURFACE ( 'NONE', #14344, 0.5999999999999989786 ) ;
#9862 = AXIS2_PLACEMENT_3D ( 'NONE', #57147, #13659, #56439 ) ;
#9864 = DIRECTION ( 'NONE',  ( 0.000000000000000000, 1.000000000000000000, 0.000000000000000000 ) ) ;
#9865 = ORIENTED_EDGE ( 'NONE', *, *, #25883, .F. ) ;
#9866 = VECTOR ( 'NONE', #10212, 1000.000000000000000 ) ;
#9867 = DIRECTION ( 'NONE',  ( 0.000000000000000000, 0.000000000000000000, 1.000000000000000000 ) ) ;
#9868 = CARTESIAN_POINT ( 'NONE',  ( -11.99351654964679526, -7.826483450353362237, 455.0000000000000568 ) ) ;
#9869 = ADVANCED_FACE ( 'NONE', ( #41059 ), #35048, .F. ) ;
#9871 = EDGE_LOOP ( 'NONE', ( #9741, #21259, #52185, #9416 ) ) ;
#9870 = PLANE ( 'NONE',  #41035 ) ;
#9873 = ORIENTED_EDGE ( 'NONE', *, *, #34824, .F. ) ;
#9872 = DIRECTION ( 'NONE',  ( 0.000000000000000000, 0.000000000000000000, 1.000000000000000000 ) ) ;
#9874 = DIRECTION ( 'NONE',  ( -0.7071067811865472397, 0.5000000000000002220, 0.5000000000000002220 ) ) ;
#9875 = LINE ( 'NONE', #47689, #42023 ) ;
#9876 = DIRECTION ( 'NONE',  ( -0.000000000000000000, 1.000000000000000000, -0.000000000000000000 ) ) ;
#9877 = DIRECTION ( 'NONE',  ( 1.000000000000000000, 0.000000000000000000, 0.000000000000000000 ) ) ;
#9878 = CYLINDRICAL_SURFACE ( 'NONE', #39805, 1.399999999999998579 ) ;
#9879 = ADVANCED_FACE ( 'NONE', ( #41412, #62623 ), #52381, .F. ) ;
#9880 = EDGE_LOOP ( 'NONE', ( #44268, #35848, #181, #50187, #48867, #47394, #15245, #27653 ) ) ;
#9881 = FACE_OUTER_BOUND ( 'NONE', #23083, .T. ) ;
#9882 = FACE_OUTER_BOUND ( 'NONE', #60358, .T. ) ;
#9883 = ADVANCED_FACE ( 'NONE', ( #67596 ), #14543, .F. ) ;
#9885 = ORIENTED_EDGE ( 'NONE', *, *, #31572, .F. ) ;
#9884 = DIRECTION ( 'NONE',  ( 0.000000000000000000, 3.673940397442059868E-16, -1.000000000000000000 ) ) ;
#9886 = FACE_BOUND ( 'NONE', #43062, .T. ) ;
#9887 = VECTOR ( 'NONE', #56732, 1000.000000000000000 ) ;
#9888 = CARTESIAN_POINT ( 'NONE',  ( 105.8309041053263257, 5.657408540445008960, 0.000000000000000000 ) ) ;
#9889 = CYLINDRICAL_SURFACE ( 'NONE', #21715, 0.2000000000000005107 ) ;
#9890 = DIRECTION ( 'NONE',  ( -0.000000000000000000, -0.000000000000000000, 1.000000000000000000 ) ) ;
#9891 = EDGE_LOOP ( 'NONE', ( #49428, #67009, #7394, #41708, #69975, #41034, #22385, #16285 ) ) ;
#9892 = DIRECTION ( 'NONE',  ( 1.000000000000000000, 0.000000000000000000, 0.000000000000000000 ) ) ;
#9893 = LINE ( 'NONE', #31808, #61034 ) ;
#9894 = EDGE_CURVE ( 'NONE', #974, #20953, #30809, .T. ) ;
#9895 = ORIENTED_EDGE ( 'NONE', *, *, #66531, .F. ) ;
#9896 = CARTESIAN_POINT ( 'NONE',  ( -28.00000000000000000, -16.28999999999999915, 14.50000000000000000 ) ) ;
#9897 = AXIS2_PLACEMENT_3D ( 'NONE', #45926, #56530, #55834 ) ;
#9898 = AXIS2_PLACEMENT_3D ( 'NONE', #35417, #67263, #24827 ) ;
#9899 = CARTESIAN_POINT ( 'NONE',  ( -11.00000000000000000, -11.10796162543699950, -9.102987789146602893 ) ) ;
#9900 = DIRECTION ( 'NONE',  ( 0.000000000000000000, 0.000000000000000000, 1.000000000000000000 ) ) ;
#9901 = AXIS2_PLACEMENT_3D ( 'NONE', #20926, #19878, #42501 ) ;
#9903 = DIRECTION ( 'NONE',  ( 0.000000000000000000, 1.000000000000000000, 0.000000000000000000 ) ) ;
#9902 = AXIS2_PLACEMENT_3D ( 'NONE', #55240, #38298, #54561 ) ;
#9904 = VERTEX_POINT ( 'NONE', #56965 ) ;
#9905 = PRODUCT_DEFINITION_FORMATION_WITH_SPECIFIED_SOURCE ( 'ANY', '', #44233, .NOT_KNOWN. ) ;
#9906 = ORIENTED_EDGE ( 'NONE', *, *, #20888, .F. ) ;
#9907 = PLANE ( 'NONE',  #11485 ) ;
#9908 = ORIENTED_EDGE ( 'NONE', *, *, #68668, .T. ) ;
#9909 = ORIENTED_EDGE ( 'NONE', *, *, #14601, .F. ) ;
#9910 = DIRECTION ( 'NONE',  ( 0.000000000000000000, 0.000000000000000000, 1.000000000000000000 ) ) ;
#9911 = CONICAL_SURFACE ( 'NONE', #29061, 2.000000000000001776, 0.7853981633974503884 ) ;
#9912 = EDGE_CURVE ( 'NONE', #18037, #51018, #2881, .T. ) ;
#9913 = CARTESIAN_POINT ( 'NONE',  ( 1.866219381641426533, -9.417013320880872840, 455.0000000000000568 ) ) ;
#9914 = DIRECTION ( 'NONE',  ( -1.000000000000000000, 0.000000000000000000, 0.000000000000000000 ) ) ;
#9915 = ORIENTED_EDGE ( 'NONE', *, *, #26053, .F. ) ;
#9916 = VERTEX_POINT ( 'NONE', #13135 ) ;
#9917 = CYLINDRICAL_SURFACE ( 'NONE', #67985, 1.000000000000000000 ) ;
#9918 = ORIENTED_EDGE ( 'NONE', *, *, #30212, .F. ) ;
#9919 = EDGE_CURVE ( 'NONE', #12232, #27294, #58115, .T. ) ;
#9920 = EDGE_LOOP ( 'NONE', ( #31883, #27558, #51214, #48086, #24384, #66220, #15203, #36339 ) ) ;
#9921 = DIRECTION ( 'NONE',  ( 0.5000000000000004441, -0.8660254037844383745, 0.000000000000000000 ) ) ;
#9922 = DIRECTION ( 'NONE',  ( 0.000000000000000000, 1.000000000000000000, 0.000000000000000000 ) ) ;
#9923 = LINE ( 'NONE', #62958, #54679 ) ;
#9924 = ORIENTED_EDGE ( 'NONE', *, *, #64066, .T. ) ;
#9925 = EDGE_CURVE ( 'NONE', #23182, #54436, #2775, .T. ) ;
#9926 = DIRECTION ( 'NONE',  ( 0.000000000000000000, 0.000000000000000000, 1.000000000000000000 ) ) ;
#9928 = CARTESIAN_POINT ( 'NONE',  ( 9.562023737882805463, 7.955476262117186614, 54.00000000000000711 ) ) ;
#9927 = DIRECTION ( 'NONE',  ( 8.659560562354951347E-17, -0.7071067811865460184, 0.7071067811865489050 ) ) ;
#9929 = EDGE_LOOP ( 'NONE', ( #27010, #4634, #16851, #54201 ) ) ;
#9930 = ADVANCED_FACE ( 'NONE', ( #40368 ), #8886, .F. ) ;
#9932 = EDGE_LOOP ( 'NONE', ( #16187, #27195, #4355, #61907 ) ) ;
#9931 = DIRECTION ( 'NONE',  ( 0.000000000000000000, 1.000000000000000000, 0.000000000000000000 ) ) ;
#9933 = ORIENTED_EDGE ( 'NONE', *, *, #17695, .T. ) ;
#9934 = ADVANCED_FACE ( 'NONE', ( #3239 ), #47077, .F. ) ;
#9935 = CARTESIAN_POINT ( 'NONE',  ( 7.000000000000000000, -26.42999999999999972, -9.412893218813501051 ) ) ;
#9936 = CARTESIAN_POINT ( 'NONE',  ( -7.450000000000001954, 0.000000000000000000, -22.00000000000000000 ) ) ;
#9937 = EDGE_LOOP ( 'NONE', ( #21589, #10608, #66683, #26598, #47506, #14145, #58563, #66167 ) ) ;
#9938 = EDGE_CURVE ( 'NONE', #17140, #64203, #29400, .T. ) ;
#9939 = EDGE_CURVE ( 'NONE', #64793, #31474, #67753, .T. ) ;
#9940 = DIRECTION ( 'NONE',  ( 0.000000000000000000, 0.000000000000000000, 1.000000000000000000 ) ) ;
#9941 = CARTESIAN_POINT ( 'NONE',  ( -11.00000000000000000, -11.50000000000000000, -15.00000000000000000 ) ) ;
#9942 = EDGE_CURVE ( 'NONE', #4880, #4176, #3594, .T. ) ;
#9943 = ORIENTED_EDGE ( 'NONE', *, *, #59637, .F. ) ;
#9944 = EDGE_CURVE ( 'NONE', #57776, #12173, #67942, .T. ) ;
#9945 = EDGE_CURVE ( 'NONE', #20689, #62061, #68291, .T. ) ;
#9946 = ORIENTED_EDGE ( 'NONE', *, *, #17970, .T. ) ;
#9947 = DIRECTION ( 'NONE',  ( -0.000000000000000000, -0.000000000000000000, 1.000000000000000000 ) ) ;
#9948 = CARTESIAN_POINT ( 'NONE',  ( -7.450000000000001954, 0.000000000000000000, -19.50000000000000000 ) ) ;
#9949 = ORIENTED_EDGE ( 'NONE', *, *, #20405, .T. ) ;
#9950 = EDGE_CURVE ( 'NONE', #40124, #59933, #42935, .T. ) ;
#9951 = VECTOR ( 'NONE', #48426, 1000.000000000000000 ) ;
#9952 = CYLINDRICAL_SURFACE ( 'NONE', #23295, 4.500000000000189182 ) ;
#9953 = FACE_OUTER_BOUND ( 'NONE', #35550, .T. ) ;
#9955 = VERTEX_POINT ( 'NONE', #67239 ) ;
#9954 = LINE ( 'NONE', #3942, #47630 ) ;
#9957 = EDGE_LOOP ( 'NONE', ( #61449, #8476, #42620, #27165 ) ) ;
#9956 = CARTESIAN_POINT ( 'NONE',  ( -2.500000000000000000, 0.000000000000000000, -29.90000000000000924 ) ) ;
#9958 = CARTESIAN_POINT ( 'NONE',  ( 7.969523737882818537, -9.737023737882820384, 54.00000000000000711 ) ) ;
#9959 = CIRCLE ( 'NONE', #69771, 2.000000000000001776 ) ;
#9960 = CARTESIAN_POINT ( 'NONE',  ( 2.369523737882786918, -9.562023737882787700, 26.00000000000000000 ) ) ;
#9961 = DIRECTION ( 'NONE',  ( 1.000000000000000000, 0.000000000000000000, 0.000000000000000000 ) ) ;
#9962 = FACE_OUTER_BOUND ( 'NONE', #33688, .T. ) ;
#9963 = DIRECTION ( 'NONE',  ( 1.000000000000000000, 0.000000000000000000, 0.000000000000000000 ) ) ;
#9964 = CARTESIAN_POINT ( 'NONE',  ( 9.900000000000000355, 18.00000000000000355, -21.00000000000000000 ) ) ;
#9965 = EDGE_CURVE ( 'NONE', #20590, #57421, #47477, .T. ) ;
#9966 = ORIENTED_EDGE ( 'NONE', *, *, #47243, .F. ) ;
#9967 = DIRECTION ( 'NONE',  ( 0.000000000000000000, 0.000000000000000000, 1.000000000000000000 ) ) ;
#9970 = ORIENTED_EDGE ( 'NONE', *, *, #10236, .T. ) ;
#9969 = EDGE_CURVE ( 'NONE', #44485, #57134, #61928, .T. ) ;
#9968 = CARTESIAN_POINT ( 'NONE',  ( 41.09999999999999432, -14.06939075806900163, 20.80000000000000426 ) ) ;
#9971 = VECTOR ( 'NONE', #45412, 1000.000000000000000 ) ;
#9972 = DIRECTION ( 'NONE',  ( -1.000000000000000000, 1.047444401652940007E-14, -1.836970198721010706E-16 ) ) ;
#9973 = CARTESIAN_POINT ( 'NONE',  ( 0.000000000000000000, 10.00000000000000000, 0.000000000000000000 ) ) ;
#9974 = DIRECTION ( 'NONE',  ( 0.000000000000000000, 1.000000000000000000, 0.000000000000000000 ) ) ;
#9975 = DIRECTION ( 'NONE',  ( -0.6414496315691446959, -0.7671651518153106419, -2.818519042764040589E-16 ) ) ;
#9976 = ORIENTED_EDGE ( 'NONE', *, *, #58468, .F. ) ;
#9977 = DIRECTION ( 'NONE',  ( 8.612436249475772606E-15, 1.000000000000000000, 0.000000000000000000 ) ) ;
#9978 = DIRECTION ( 'NONE',  ( -0.000000000000000000, -0.000000000000000000, -1.000000000000000000 ) ) ;
#9979 = EDGE_LOOP ( 'NONE', ( #65781, #47563, #2325, #36064 ) ) ;
#9980 = CARTESIAN_POINT ( 'NONE',  ( 39.00000000000000000, -14.48845687959340012, 21.00000000000000000 ) ) ;
#9981 = CARTESIAN_POINT ( 'NONE',  ( 283.0000000000000568, -20.40000000000000213, -17.60000000000000142 ) ) ;
#9982 = DIRECTION ( 'NONE',  ( -0.7671651518153105309, -0.6414496315691445849, 0.000000000000000000 ) ) ;
#9983 = ORIENTED_EDGE ( 'NONE', *, *, #62573, .T. ) ;
#9984 = DIRECTION ( 'NONE',  ( 0.000000000000000000, -0.000000000000000000, 1.000000000000000000 ) ) ;
#9985 = EDGE_LOOP ( 'NONE', ( #69109, #1408, #40081, #25859 ) ) ;
#9986 = AXIS2_PLACEMENT_3D ( 'NONE', #12030, #55186, #38247 ) ;
#9987 = ORIENTED_EDGE ( 'NONE', *, *, #48821, .T. ) ;
#9988 = FACE_BOUND ( 'NONE', #12041, .T. ) ;
#9989 = CARTESIAN_POINT ( 'NONE',  ( -10.91351654964670992, -2.706483450353338593, 455.0000000000000568 ) ) ;
#9990 = CARTESIAN_POINT ( 'NONE',  ( 13.00000000000000178, -17.35230188589299871, -15.35019951917099945 ) ) ;
#9991 = DIRECTION ( 'NONE',  ( 1.000000000000000000, -0.000000000000000000, 0.000000000000000000 ) ) ;
#9992 = CARTESIAN_POINT ( 'NONE',  ( 25.50000000000000355, -5.200000000000001066, 20.49999999999999645 ) ) ;
#9993 = ORIENTED_EDGE ( 'NONE', *, *, #40140, .F. ) ;
#9994 = ORIENTED_EDGE ( 'NONE', *, *, #10025, .F. ) ;
#9996 = VERTEX_POINT ( 'NONE', #20898 ) ;
#9995 = CYLINDRICAL_SURFACE ( 'NONE', #11450, 1.929199999999998916 ) ;
#9997 = EDGE_LOOP ( 'NONE', ( #67891, #33109, #61245, #29905 ) ) ;
#9998 = CIRCLE ( 'NONE', #41624, 0.4999999999979497511 ) ;
#9999 = EDGE_CURVE ( 'NONE', #59753, #55220, #56492, .T. ) ;
#10000 = DIRECTION ( 'NONE',  ( 1.000000000000000000, -0.000000000000000000, -0.000000000000000000 ) ) ;
#10001 = DIRECTION ( 'NONE',  ( -1.000000000000000000, 0.000000000000000000, 0.000000000000000000 ) ) ;
#10002 = CARTESIAN_POINT ( 'NONE',  ( 4.255011587777269177, 8.452095193409277840, 455.0000000000000568 ) ) ;
#10003 = EDGE_CURVE ( 'NONE', #47329, #59237, #15888, .T. ) ;
#10004 = VECTOR ( 'NONE', #24005, 1000.000000000000000 ) ;
#10005 = CARTESIAN_POINT ( 'NONE',  ( 8.689999999999999503, 9.750000000000001776, -7.000000000000000000 ) ) ;
#10007 = CARTESIAN_POINT ( 'NONE',  ( 40.90000000000000568, 14.08845687959340154, 20.99999999999999645 ) ) ;
#10006 = DIRECTION ( 'NONE',  ( 1.000000000000000000, 0.000000000000000000, 0.000000000000000000 ) ) ;
#10008 = EDGE_CURVE ( 'NONE', #55374, #16718, #31526, .T. ) ;
#10009 = ORIENTED_EDGE ( 'NONE', *, *, #27499, .T. ) ;
#10010 = VERTEX_POINT ( 'NONE', #9958 ) ;
#10011 = ORIENTED_EDGE ( 'NONE', *, *, #31938, .F. ) ;
#10012 = CARTESIAN_POINT ( 'NONE',  ( 11.78648345035337819, -4.406483450353490205, 455.0000000000000568 ) ) ;
#10013 = EDGE_CURVE ( 'NONE', #26698, #52241, #9111, .T. ) ;
#10014 = DIRECTION ( 'NONE',  ( -0.8660254037844510311, -0.4999999999999785727, 0.000000000000000000 ) ) ;
#10015 = SHAPE_REPRESENTATION_RELATIONSHIP ( 'NONE' , 'NONE' ,  #64253, #67252 ) ;
#10016 = AXIS2_PLACEMENT_3D ( 'NONE', #7506, #12797, #1182 ) ;
#10017 = DIRECTION ( 'NONE',  ( 1.000000000000000000, 0.000000000000000000, 0.000000000000000000 ) ) ;
#10018 = ORIENTED_EDGE ( 'NONE', *, *, #1842, .T. ) ;
#10019 = EDGE_LOOP ( 'NONE', ( #984, #51020, #29032, #6159 ) ) ;
#10020 = ORIENTED_EDGE ( 'NONE', *, *, #36107, .F. ) ;
#10021 = DIRECTION ( 'NONE',  ( 1.047444401652940007E-14, 1.000000000000000000, 1.836970198721029934E-16 ) ) ;
#10022 = ORIENTED_EDGE ( 'NONE', *, *, #52243, .T. ) ;
#10023 = DIRECTION ( 'NONE',  ( 0.000000000000000000, -1.000000000000000000, 0.000000000000000000 ) ) ;
#10024 = ORIENTED_EDGE ( 'NONE', *, *, #63066, .F. ) ;
#10025 = EDGE_CURVE ( 'NONE', #35382, #69020, #64396, .T. ) ;
#10026 = ORIENTED_EDGE ( 'NONE', *, *, #2287, .T. ) ;
#10027 = CARTESIAN_POINT ( 'NONE',  ( 30.00000000000000000, -9.200000000000120082, -17.30000000000000071 ) ) ;
#10029 = EDGE_LOOP ( 'NONE', ( #56562, #5338, #68921, #66696 ) ) ;
#10028 = DIRECTION ( 'NONE',  ( -1.000000000000000000, 0.000000000000000000, 0.000000000000000000 ) ) ;
#10030 = EDGE_LOOP ( 'NONE', ( #16161, #8483, #29888, #49608 ) ) ;
#10031 = DIRECTION ( 'NONE',  ( -0.000000000000000000, -0.000000000000000000, -1.000000000000000000 ) ) ;
#10032 = CARTESIAN_POINT ( 'NONE',  ( 283.0000000000000568, -32.95000000000000284, -7.700000000000000178 ) ) ;
#10034 = ORIENTED_EDGE ( 'NONE', *, *, #12668, .F. ) ;
#10033 = DIRECTION ( 'NONE',  ( -1.000000000000000000, 0.000000000000000000, 0.000000000000000000 ) ) ;
#10035 = ORIENTED_EDGE ( 'NONE', *, *, #15845, .F. ) ;
#10036 = DIRECTION ( 'NONE',  ( -1.000000000000000000, 0.000000000000000000, 0.000000000000000000 ) ) ;
#10037 = FACE_OUTER_BOUND ( 'NONE', #11030, .T. ) ;
#10038 = FACE_OUTER_BOUND ( 'NONE', #47476, .T. ) ;
#10039 = FACE_OUTER_BOUND ( 'NONE', #24448, .T. ) ;
#10040 = CIRCLE ( 'NONE', #36011, 1.929199999999998028 ) ;
#10041 = DIRECTION ( 'NONE',  ( 0.000000000000000000, -1.000000000000000000, -3.673940397442060361E-16 ) ) ;
#10042 = EDGE_CURVE ( 'NONE', #34031, #37597, #42112, .T. ) ;
#10043 = ORIENTED_EDGE ( 'NONE', *, *, #19700, .F. ) ;
#10044 = CARTESIAN_POINT ( 'NONE',  ( -9.722976262117258628, 3.667976262117184749, 54.00000000000000711 ) ) ;
#10045 = VECTOR ( 'NONE', #1528, 1000.000000000000000 ) ;
#10047 = ORIENTED_EDGE ( 'NONE', *, *, #19656, .T. ) ;
#10046 = EDGE_CURVE ( 'NONE', #57233, #1031, #67808, .T. ) ;
#10048 = DIRECTION ( 'NONE',  ( -0.000000000000000000, -0.000000000000000000, 1.000000000000000000 ) ) ;
#10049 = CARTESIAN_POINT ( 'NONE',  ( -8.250000000000001776, -8.249999999999998224, -26.00000000000001066 ) ) ;
#10050 = EDGE_CURVE ( 'NONE', #33306, #66802, #48829, .T. ) ;
#10051 = CARTESIAN_POINT ( 'NONE',  ( -25.50000000000000355, -5.200000000000001066, -22.50000000000000000 ) ) ;
#10052 = DIRECTION ( 'NONE',  ( 0.000000000000000000, 1.000000000000000000, 0.000000000000000000 ) ) ;
#10053 = CIRCLE ( 'NONE', #1014, 1.929199999999997139 ) ;
#10054 = CARTESIAN_POINT ( 'NONE',  ( 8.250000000000005329, 7.250000000000000888, -13.00000000000000178 ) ) ;
#10055 = ORIENTED_EDGE ( 'NONE', *, *, #9214, .F. ) ;
#10056 = VECTOR ( 'NONE', #7299, 1000.000000000000000 ) ;
#10057 = CARTESIAN_POINT ( 'NONE',  ( 5.257023737882795977, 5.242976262117205799, 26.00000000000000711 ) ) ;
#10058 = DIRECTION ( 'NONE',  ( -1.000000000000000000, 2.602085213965213008E-15, 0.000000000000000000 ) ) ;
#10059 = VECTOR ( 'NONE', #58926, 1000.000000000000000 ) ;
#10060 = DIRECTION ( 'NONE',  ( -1.000000000000000000, 0.000000000000000000, 0.000000000000000000 ) ) ;
#10061 = ORIENTED_EDGE ( 'NONE', *, *, #26015, .F. ) ;
#10062 = DIRECTION ( 'NONE',  ( -1.836970198721029934E-16, 1.836970198721036344E-16, -1.000000000000000000 ) ) ;
#10064 = EDGE_CURVE ( 'NONE', #31340, #20149, #48473, .T. ) ;
#10063 = DIRECTION ( 'NONE',  ( -0.000000000000000000, -0.000000000000000000, -1.000000000000000000 ) ) ;
#10065 = DIRECTION ( 'NONE',  ( -1.000000000000000000, 0.000000000000000000, 0.000000000000000000 ) ) ;
#10066 = CYLINDRICAL_SURFACE ( 'NONE', #62931, 1.000000000000000000 ) ;
#10067 = AXIS2_PLACEMENT_3D ( 'NONE', #60803, #1759, #61485 ) ;
#10068 = CARTESIAN_POINT ( 'NONE',  ( 283.0000000000000568, -31.30000000000000071, 12.69999999999999929 ) ) ;
#10069 = VERTEX_POINT ( 'NONE', #26557 ) ;
#10070 = LINE ( 'NONE', #48245, #10737 ) ;
#10071 = DIRECTION ( 'NONE',  ( 1.000000000000000000, -0.000000000000000000, 0.000000000000000000 ) ) ;
#10072 = DIRECTION ( 'NONE',  ( -1.000000000000000000, 0.000000000000000000, 0.000000000000000000 ) ) ;
#10073 = PLANE ( 'NONE',  #15901 ) ;
#10074 = ORIENTED_EDGE ( 'NONE', *, *, #8533, .T. ) ;
#10076 = ORIENTED_EDGE ( 'NONE', *, *, #35912, .T. ) ;
#10075 = CARTESIAN_POINT ( 'NONE',  ( -11.00000000000000000, -5.200000000000001066, -9.400000000000000355 ) ) ;
#10077 = EDGE_CURVE ( 'NONE', #55220, #48338, #37180, .T. ) ;
#10078 = CARTESIAN_POINT ( 'NONE',  ( 8.249999999999996447, -7.848062532927998269, 0.000000000000000000 ) ) ;
#10079 = DIRECTION ( 'NONE',  ( -0.000000000000000000, -0.000000000000000000, -1.000000000000000000 ) ) ;
#10080 = DIRECTION ( 'NONE',  ( 0.000000000000000000, -0.7071067811865474617, -0.7071067811865474617 ) ) ;
#10081 = ORIENTED_EDGE ( 'NONE', *, *, #5160, .F. ) ;
#10082 = DIRECTION ( 'NONE',  ( -0.7071067811865475727, -0.7071067811865475727, 0.000000000000000000 ) ) ;
#10083 = DIRECTION ( 'NONE',  ( -1.836970198721029934E-16, 1.836970198721036344E-16, -1.000000000000000000 ) ) ;
#10084 = ADVANCED_FACE ( 'NONE', ( #31872 ), #5694, .F. ) ;
#10085 = ORIENTED_EDGE ( 'NONE', *, *, #43239, .T. ) ;
#10086 = EDGE_LOOP ( 'NONE', ( #63830, #61491, #16540, #45743 ) ) ;
#10087 = ADVANCED_FACE ( 'NONE', ( #58029 ), #53437, .T. ) ;
#10088 = AXIS2_PLACEMENT_3D ( 'NONE', #40057, #66599, #60939 ) ;
#10089 = ORIENTED_EDGE ( 'NONE', *, *, #60608, .F. ) ;
#10090 = EDGE_CURVE ( 'NONE', #34171, #749, #49739, .T. ) ;
#10091 = ADVANCED_FACE ( 'NONE', ( #382 ), #59432, .F. ) ;
#10092 = CARTESIAN_POINT ( 'NONE',  ( 37.90000000000000568, -0.000000000000000000, 20.80000000000000426 ) ) ;
#10093 = AXIS2_PLACEMENT_3D ( 'NONE', #13185, #19536, #30502 ) ;
#10094 = FACE_OUTER_BOUND ( 'NONE', #48016, .T. ) ;
#10095 = CARTESIAN_POINT ( 'NONE',  ( 5.257023737882819070, -5.257023737882825287, 54.00000000000000711 ) ) ;
#10096 = ADVANCED_FACE ( 'NONE', ( #48131 ), #10991, .T. ) ;
#10097 = ORIENTED_EDGE ( 'NONE', *, *, #52881, .T. ) ;
#10098 = ORIENTED_EDGE ( 'NONE', *, *, #29216, .F. ) ;
#10099 = AXIS2_PLACEMENT_3D ( 'NONE', #64834, #16385, #37962 ) ;
#10100 = CARTESIAN_POINT ( 'NONE',  ( -28.00000000000000000, -15.50000000000000000, 14.49999999999999645 ) ) ;
#10101 = ORIENTED_EDGE ( 'NONE', *, *, #286, .F. ) ;
#10102 = ORIENTED_EDGE ( 'NONE', *, *, #22660, .F. ) ;
#10103 = VERTEX_POINT ( 'NONE', #15254 ) ;
#10104 = AXIS2_PLACEMENT_3D ( 'NONE', #47942, #5513, #44612 ) ;
#10105 = ORIENTED_EDGE ( 'NONE', *, *, #28645, .F. ) ;
#10106 = DIRECTION ( 'NONE',  ( 0.000000000000000000, 1.000000000000000000, 0.000000000000000000 ) ) ;
#10108 = VERTEX_POINT ( 'NONE', #69337 ) ;
#10107 = DIRECTION ( 'NONE',  ( -1.000000000000000000, 0.000000000000000000, 0.000000000000000000 ) ) ;
#10109 = DIRECTION ( 'NONE',  ( -1.000000000000000000, 7.304098846218132892E-15, -0.000000000000000000 ) ) ;
#10110 = CARTESIAN_POINT ( 'NONE',  ( 9.955011587777235604, -9.247904806590801385, 455.0000000000000568 ) ) ;
#10111 = CYLINDRICAL_SURFACE ( 'NONE', #55022, 0.1749999999999998224 ) ;
#10112 = ORIENTED_EDGE ( 'NONE', *, *, #37162, .F. ) ;
#10113 = ORIENTED_EDGE ( 'NONE', *, *, #58936, .T. ) ;
#10114 = VECTOR ( 'NONE', #6552, 1000.000000000000000 ) ;
#10115 = CARTESIAN_POINT ( 'NONE',  ( 7.000000000000000000, -25.56180396883900130, 14.25872597390799967 ) ) ;
#10116 = CARTESIAN_POINT ( 'NONE',  ( 25.57999999999999829, 0.000000000000000000, 2.458500000000000796 ) ) ;
#10117 = VERTEX_POINT ( 'NONE', #4312 ) ;
#10118 = DIRECTION ( 'NONE',  ( 1.000000000000000000, -0.000000000000000000, 0.000000000000000000 ) ) ;
#10119 = CARTESIAN_POINT ( 'NONE',  ( 4.149127210878726935, -6.836383711243002814, 54.00000000000000711 ) ) ;
#10120 = AXIS2_PLACEMENT_3D ( 'NONE', #35027, #14171, #7807 ) ;
#10121 = CARTESIAN_POINT ( 'NONE',  ( -10.91351654964680584, -9.306483450353375986, 455.0000000000000568 ) ) ;
#10122 = ORIENTED_EDGE ( 'NONE', *, *, #17321, .T. ) ;
#10123 = EDGE_CURVE ( 'NONE', #3316, #47101, #47416, .T. ) ;
#10124 = FACE_OUTER_BOUND ( 'NONE', #65370, .T. ) ;
#10125 = DIRECTION ( 'NONE',  ( -1.000000000000000000, 0.000000000000000000, 0.000000000000000000 ) ) ;
#10126 = ADVANCED_FACE ( 'NONE', ( #43 ), #25750, .T. ) ;
#10127 = CARTESIAN_POINT ( 'NONE',  ( -2.355476262117319308, -8.835729544836356197, 54.00000000000000711 ) ) ;
#10128 = CARTESIAN_POINT ( 'NONE',  ( -30.00000000000000000, -13.79999999999979998, 17.30000000000000071 ) ) ;
#10129 = EDGE_CURVE ( 'NONE', #11705, #66129, #22301, .T. ) ;
#10130 = FACE_OUTER_BOUND ( 'NONE', #47731, .T. ) ;
#10131 = ORIENTED_EDGE ( 'NONE', *, *, #54335, .T. ) ;
#10132 = DIRECTION ( 'NONE',  ( 0.000000000000000000, 1.000000000000000000, 0.000000000000000000 ) ) ;
#10133 = CARTESIAN_POINT ( 'NONE',  ( 106.4257688009193430, 0.000000000000000000, 334.4830310981789694 ) ) ;
#10134 = AXIS2_PLACEMENT_3D ( 'NONE', #51544, #19353, #35249 ) ;
#10135 = FACE_OUTER_BOUND ( 'NONE', #23558, .T. ) ;
#10136 = DIRECTION ( 'NONE',  ( 0.7071067811865513475, 0.7071067811865435759, 0.000000000000000000 ) ) ;
#10137 = ORIENTED_EDGE ( 'NONE', *, *, #68210, .T. ) ;
#10138 = LINE ( 'NONE', #15094, #41689 ) ;
#10139 = DIRECTION ( 'NONE',  ( -1.000000000000000000, 0.000000000000000000, 0.000000000000000000 ) ) ;
#10140 = CARTESIAN_POINT ( 'NONE',  ( -6.775514141871385121, 7.394232575409538377, 54.00000000000000711 ) ) ;
#10141 = LINE ( 'NONE', #31720, #4826 ) ;
#10142 = ORIENTED_EDGE ( 'NONE', *, *, #44083, .F. ) ;
#10143 = FACE_OUTER_BOUND ( 'NONE', #23292, .T. ) ;
#10144 = LINE ( 'NONE', #9810, #68939 ) ;
#10145 = CARTESIAN_POINT ( 'NONE',  ( 9.841277389592701041, 2.277516549646538824, 455.0000000000000568 ) ) ;
#10146 = VECTOR ( 'NONE', #8466, 1000.000000000000000 ) ;
#10147 = PLANE ( 'NONE',  #61482 ) ;
#10148 = CARTESIAN_POINT ( 'NONE',  ( 26.90000000000000213, -14.06939075806900874, 20.80000000000001137 ) ) ;
#10149 = EDGE_LOOP ( 'NONE', ( #59284, #49268, #31663, #19293 ) ) ;
#10150 = AXIS2_PLACEMENT_3D ( 'NONE', #42923, #33013, #11097 ) ;
#10151 = ORIENTED_EDGE ( 'NONE', *, *, #36935, .T. ) ;
#10152 = CARTESIAN_POINT ( 'NONE',  ( -7.955476262117259445, 9.722976262117178692, 54.00000000000000711 ) ) ;
#10153 = LINE ( 'NONE', #31735, #24407 ) ;
#10154 = ORIENTED_EDGE ( 'NONE', *, *, #66172, .F. ) ;
#10155 = PLANE ( 'NONE',  #49503 ) ;
#10156 = AXIS2_PLACEMENT_3D ( 'NONE', #4735, #5784, #63787 ) ;
#10157 = DIRECTION ( 'NONE',  ( 0.000000000000000000, 0.000000000000000000, 1.000000000000000000 ) ) ;
#10158 = ORIENTED_EDGE ( 'NONE', *, *, #52280, .T. ) ;
#10159 = DIRECTION ( 'NONE',  ( 1.000000000000000000, 0.000000000000000000, 0.000000000000000000 ) ) ;
#10160 = ORIENTED_EDGE ( 'NONE', *, *, #30172, .T. ) ;
#10161 = VERTEX_POINT ( 'NONE', #39571 ) ;
#10162 = CYLINDRICAL_SURFACE ( 'NONE', #19310, 1.000000000000000000 ) ;
#10163 = EDGE_CURVE ( 'NONE', #33821, #13319, #2004, .T. ) ;
#10164 = ORIENTED_EDGE ( 'NONE', *, *, #10320, .T. ) ;
#10165 = ADVANCED_FACE ( 'NONE', ( #65430 ), #61132, .T. ) ;
#10166 = CARTESIAN_POINT ( 'NONE',  ( 11.32648345035338089, 4.393516549646522051, 455.0000000000000568 ) ) ;
#10167 = FACE_OUTER_BOUND ( 'NONE', #66950, .T. ) ;
#10168 = DIRECTION ( 'NONE',  ( 1.836970198721029934E-16, -1.836970198721036344E-16, 1.000000000000000000 ) ) ;
#10169 = EDGE_CURVE ( 'NONE', #25149, #40605, #68646, .T. ) ;
#10170 = EDGE_CURVE ( 'NONE', #35206, #62636, #55163, .T. ) ;
#10171 = ORIENTED_EDGE ( 'NONE', *, *, #63972, .T. ) ;
#10172 = ORIENTED_EDGE ( 'NONE', *, *, #66369, .T. ) ;
#10173 = DIRECTION ( 'NONE',  ( -0.000000000000000000, -0.000000000000000000, -1.000000000000000000 ) ) ;
#10175 = LINE ( 'NONE', #69222, #51426 ) ;
#10174 = LINE ( 'NONE', #48701, #59825 ) ;
#10176 = VERTEX_POINT ( 'NONE', #44526 ) ;
#10177 = ORIENTED_EDGE ( 'NONE', *, *, #12930, .F. ) ;
#10179 = ORIENTED_EDGE ( 'NONE', *, *, #53802, .F. ) ;
#10178 = APPLICATION_PROTOCOL_DEFINITION ( 'draft international standard', 'automotive_design', 1998, #64814 ) ;
#10180 = AXIS2_PLACEMENT_3D ( 'NONE', #68650, #57329, #34704 ) ;
#10181 =( REPRESENTATION_RELATIONSHIP ('NONE','NONE', #4299, #14183 ) REPRESENTATION_RELATIONSHIP_WITH_TRANSFORMATION ( #39465 )SHAPE_REPRESENTATION_RELATIONSHIP( ) );
#10182 = LINE ( 'NONE', #31763, #49157 ) ;
#10183 = VECTOR ( 'NONE', #12144, 1000.000000000000000 ) ;
#10184 = EDGE_CURVE ( 'NONE', #6447, #12885, #39237, .T. ) ;
#10185 = AXIS2_PLACEMENT_3D ( 'NONE', #67108, #61095, #13715 ) ;
#10187 = ORIENTED_EDGE ( 'NONE', *, *, #61708, .F. ) ;
#10186 = DIRECTION ( 'NONE',  ( -1.000000000000000000, 0.000000000000000000, 0.000000000000000000 ) ) ;
#10188 = DIRECTION ( 'NONE',  ( 1.836970198721029934E-16, -1.836970198721036344E-16, 1.000000000000000000 ) ) ;
#10189 = DIRECTION ( 'NONE',  ( 1.000000000000000000, -0.000000000000000000, 0.000000000000000000 ) ) ;
#10190 = ORIENTED_EDGE ( 'NONE', *, *, #67550, .F. ) ;
#10191 = ORIENTED_EDGE ( 'NONE', *, *, #5120, .F. ) ;
#10192 = VECTOR ( 'NONE', #68573, 1000.000000000000000 ) ;
#10193 = DIRECTION ( 'NONE',  ( 0.000000000000000000, 1.000000000000000000, 1.922073611378672844E-12 ) ) ;
#10194 = ORIENTED_EDGE ( 'NONE', *, *, #12682, .T. ) ;
#10195 = VECTOR ( 'NONE', #23953, 1000.000000000000000 ) ;
#10196 = CARTESIAN_POINT ( 'NONE',  ( 7.532023737882806103, 6.651770455163672047, 54.00000000000000711 ) ) ;
#10197 = CARTESIAN_POINT ( 'NONE',  ( -11.99351654964671354, 4.173516549646604901, 195.0000000000000284 ) ) ;
#10198 = DIRECTION ( 'NONE',  ( 0.000000000000000000, 0.000000000000000000, -1.000000000000000000 ) ) ;
#10199 = VECTOR ( 'NONE', #7901, 1000.000000000000000 ) ;
#10200 = VERTEX_POINT ( 'NONE', #22637 ) ;
#10201 = AXIS2_PLACEMENT_3D ( 'NONE', #18741, #40311, #6739 ) ;
#10202 = FILL_AREA_STYLE_COLOUR ( '', #5302 ) ;
#10203 = CARTESIAN_POINT ( 'NONE',  ( -9.689726262117325462, -9.703773737882725570, 54.00000000000000711 ) ) ;
#10205 = VERTEX_POINT ( 'NONE', #16988 ) ;
#10204 = SURFACE_STYLE_FILL_AREA ( #10899 ) ;
#10207 = ORIENTED_EDGE ( 'NONE', *, *, #37191, .F. ) ;
#10206 = CARTESIAN_POINT ( 'NONE',  ( 283.0000000000000568, -32.45000000000000995, -15.00000000000000000 ) ) ;
#10208 = CARTESIAN_POINT ( 'NONE',  ( 15.00000000000000000, -0.5000000000000000000, -26.50000000000000000 ) ) ;
#10209 = VECTOR ( 'NONE', #21269, 1000.000000000000000 ) ;
#10210 = CIRCLE ( 'NONE', #19237, 24.99999999998784972 ) ;
#10211 = DIRECTION ( 'NONE',  ( 1.836970198721029934E-16, 1.836970198721010706E-16, -1.000000000000000000 ) ) ;
#10212 = DIRECTION ( 'NONE',  ( 1.836970198721029934E-16, 1.836970198721010706E-16, -1.000000000000000000 ) ) ;
#10213 = DIRECTION ( 'NONE',  ( 0.000000000000000000, 1.000000000000000000, 0.000000000000000000 ) ) ;
#10214 = EDGE_CURVE ( 'NONE', #32725, #66079, #34262, .T. ) ;
#10215 = CARTESIAN_POINT ( 'NONE',  ( 7.000000000000000000, -32.00000000000000000, -8.400000000000000355 ) ) ;
#10216 = ORIENTED_EDGE ( 'NONE', *, *, #2106, .T. ) ;
#10217 = LINE ( 'NONE', #67864, #18854 ) ;
#10218 = DIRECTION ( 'NONE',  ( -0.7071067811865503483, -0.7071067811865446862, 0.000000000000000000 ) ) ;
#10219 = DIRECTION ( 'NONE',  ( 1.000000000000000000, -5.981805089575196197E-17, 0.000000000000000000 ) ) ;
#10221 = ORIENTED_EDGE ( 'NONE', *, *, #60089, .T. ) ;
#10220 = CARTESIAN_POINT ( 'NONE',  ( 280.0000000000000000, -53.81370849898476649, -16.00000000000000711 ) ) ;
#10222 = DIRECTION ( 'NONE',  ( -0.000000000000000000, 3.673940397442059868E-16, -1.000000000000000000 ) ) ;
#10223 = AXIS2_PLACEMENT_3D ( 'NONE', #58469, #58809, #68363 ) ;
#10224 = LINE ( 'NONE', #31803, #8878 ) ;
#10225 = CARTESIAN_POINT ( 'NONE',  ( -7.250000000000000888, -8.249999999999998224, -26.00000000000001066 ) ) ;
#10226 = EDGE_CURVE ( 'NONE', #51967, #27626, #28280, .T. ) ;
#10227 = LINE ( 'NONE', #26489, #9710 ) ;
#10228 = ORIENTED_EDGE ( 'NONE', *, *, #9471, .T. ) ;
#10229 = DIRECTION ( 'NONE',  ( -0.4999999999989410693, 0.000000000000000000, 0.8660254037850499964 ) ) ;
#10230 = CARTESIAN_POINT ( 'NONE',  ( 4.206483450353421638, 11.11351654964658486, 455.0000000000000568 ) ) ;
#10231 = ORIENTED_EDGE ( 'NONE', *, *, #13677, .F. ) ;
#10232 = DIRECTION ( 'NONE',  ( 0.000000000000000000, 1.000000000000000000, -0.000000000000000000 ) ) ;
#10233 = LINE ( 'NONE', #21535, #15447 ) ;
#10234 = DIRECTION ( 'NONE',  ( -1.000000000000000000, 0.000000000000000000, 0.000000000000000000 ) ) ;
#10235 = AXIS2_PLACEMENT_3D ( 'NONE', #16288, #25868, #15950 ) ;
#10236 = EDGE_CURVE ( 'NONE', #54829, #26529, #60454, .T. ) ;
#10237 = CARTESIAN_POINT ( 'NONE',  ( -11.00000000000000000, -17.50000000000000000, 26.64999999999999858 ) ) ;
#10238 = VECTOR ( 'NONE', #36450, 1000.000000000000000 ) ;
#10239 = CARTESIAN_POINT ( 'NONE',  ( 29.50000000000000355, -11.50000000000100009, -15.00000000000084910 ) ) ;
#10240 = VECTOR ( 'NONE', #53783, 1000.000000000000000 ) ;
#10241 = VERTEX_POINT ( 'NONE', #60798 ) ;
#10242 = ORIENTED_EDGE ( 'NONE', *, *, #32117, .T. ) ;
#10243 = PLANE ( 'NONE',  #35195 ) ;
#10244 = ORIENTED_EDGE ( 'NONE', *, *, #16062, .T. ) ;
#10245 = VERTEX_POINT ( 'NONE', #44188 ) ;
#10246 = VECTOR ( 'NONE', #21282, 1000.000000000000000 ) ;
#10247 = LINE ( 'NONE', #57281, #48350 ) ;
#10248 = AXIS2_PLACEMENT_3D ( 'NONE', #44383, #49027, #21800 ) ;
#10249 = FACE_OUTER_BOUND ( 'NONE', #9957, .T. ) ;
#10250 = DIRECTION ( 'NONE',  ( 1.000000000000000000, 0.000000000000000000, 0.000000000000000000 ) ) ;
#10251 = ORIENTED_EDGE ( 'NONE', *, *, #29226, .T. ) ;
#10252 = ORIENTED_EDGE ( 'NONE', *, *, #53513, .F. ) ;
#10253 = CYLINDRICAL_SURFACE ( 'NONE', #27363, 24.99999999998784972 ) ;
#10254 = ORIENTED_EDGE ( 'NONE', *, *, #16191, .F. ) ;
#10255 = VECTOR ( 'NONE', #3364, 1000.000000000000000 ) ;
#10256 = VERTEX_POINT ( 'NONE', #12342 ) ;
#10257 = EDGE_CURVE ( 'NONE', #52237, #41185, #60110, .T. ) ;
#10258 = DIRECTION ( 'NONE',  ( 1.000000000000000000, 0.000000000000000000, 0.000000000000000000 ) ) ;
#10259 = DIRECTION ( 'NONE',  ( 8.951101527228104953E-17, -1.000000000000000000, 0.000000000000000000 ) ) ;
#10260 = CARTESIAN_POINT ( 'NONE',  ( 32.89999999999999858, 13.66939075806899240, -20.79999999999999361 ) ) ;
#10261 = ADVANCED_FACE ( 'NONE', ( #738 ), #55509, .F. ) ;
#10262 = EDGE_CURVE ( 'NONE', #39282, #3194, #7049, .T. ) ;
#10263 = ORIENTED_EDGE ( 'NONE', *, *, #63874, .F. ) ;
#10264 = CARTESIAN_POINT ( 'NONE',  ( 7.450000000000004619, -1.336933437520057563E-15, -22.00000000000000000 ) ) ;
#10265 = VECTOR ( 'NONE', #54051, 1000.000000000000000 ) ;
#10267 = PLANE ( 'NONE',  #31101 ) ;
#10266 = CARTESIAN_POINT ( 'NONE',  ( -7.250000000000001776, -7.249999999999998224, -23.50000000000000000 ) ) ;
#10268 = ORIENTED_EDGE ( 'NONE', *, *, #16454, .T. ) ;
#10271 = ORIENTED_EDGE ( 'NONE', *, *, #68670, .T. ) ;
#10270 = EDGE_CURVE ( 'NONE', #38222, #32779, #4307, .T. ) ;
#10269 = CARTESIAN_POINT ( 'NONE',  ( -30.00000000000000000, -11.50000000000000000, 15.00000000000000000 ) ) ;
#10272 = ORIENTED_EDGE ( 'NONE', *, *, #28106, .T. ) ;
#10273 = EDGE_CURVE ( 'NONE', #65734, #48070, #18008, .T. ) ;
#10274 = DIRECTION ( 'NONE',  ( -1.000000000000000000, 0.000000000000000000, 0.000000000000000000 ) ) ;
#10275 = EDGE_CURVE ( 'NONE', #22897, #21838, #38890, .T. ) ;
#10276 = LINE ( 'NONE', #10614, #57500 ) ;
#10277 = VERTEX_POINT ( 'NONE', #2107 ) ;
#10278 = CARTESIAN_POINT ( 'NONE',  ( -30.00000000000000000, -11.70000000000000284, 12.50000000000000000 ) ) ;
#10279 = DIRECTION ( 'NONE',  ( 1.000000000000000000, 0.000000000000000000, 0.000000000000000000 ) ) ;
#10280 = VERTEX_POINT ( 'NONE', #43500 ) ;
#10281 = EDGE_LOOP ( 'NONE', ( #34845, #65716, #17903, #8151 ) ) ;
#10282 = CARTESIAN_POINT ( 'NONE',  ( -11.77351654964674665, -7.826483450353317828, 195.0000000000000284 ) ) ;
#10283 = DIRECTION ( 'NONE',  ( -1.000000000000000000, 0.000000000000000000, 0.000000000000000000 ) ) ;
#10284 = CARTESIAN_POINT ( 'NONE',  ( -10.19191654964671301, 11.07551654964660415, 455.0000000000000568 ) ) ;
#10285 = CIRCLE ( 'NONE', #18135, 0.5249999999999994671 ) ;
#10286 = ORIENTED_EDGE ( 'NONE', *, *, #28527, .T. ) ;
#10287 = STYLED_ITEM ( 'NONE', ( #2877 ), #42462 ) ;
#10288 = DIRECTION ( 'NONE',  ( -1.000000000000000000, 8.540177112501197482E-15, 0.000000000000000000 ) ) ;
#10289 = ADVANCED_FACE ( 'NONE', ( #16653 ), #38557, .F. ) ;
#10290 = CARTESIAN_POINT ( 'NONE',  ( -29.50000000000000355, -11.50000000000100009, -15.00000000000084910 ) ) ;
#10292 = VERTEX_POINT ( 'NONE', #40973 ) ;
#10291 = CARTESIAN_POINT ( 'NONE',  ( -11.00000000000000000, -9.200000000000120082, -17.30000000000000071 ) ) ;
#10294 = ORIENTED_EDGE ( 'NONE', *, *, #11574, .F. ) ;
#10293 = DIRECTION ( 'NONE',  ( 0.000000000000000000, 1.000000000000000000, 0.000000000000000000 ) ) ;
#10295 = AXIS2_PLACEMENT_3D ( 'NONE', #36396, #45593, #40299 ) ;
#10296 = CARTESIAN_POINT ( 'NONE',  ( 0.000000000000000000, 3.959283101643393150E-16, 3.233000000000000096 ) ) ;
#10297 = DIRECTION ( 'NONE',  ( -0.000000000000000000, -0.000000000000000000, -1.000000000000000000 ) ) ;
#10298 = DIRECTION ( 'NONE',  ( 0.000000000000000000, 1.000000000000000000, 0.000000000000000000 ) ) ;
#10299 = CARTESIAN_POINT ( 'NONE',  ( 37.90000000000000568, 13.66939075806899240, 20.79999999999999361 ) ) ;
#10300 = AXIS2_PLACEMENT_3D ( 'NONE', #67283, #45003, #12815 ) ;
#10301 = AXIS2_PLACEMENT_3D ( 'NONE', #68078, #45447, #40850 ) ;
#10302 = ADVANCED_FACE ( 'NONE', ( #24011 ), #30728, .F. ) ;
#10303 = LINE ( 'NONE', #9604, #66671 ) ;
#10304 = LINE ( 'NONE', #58407, #14596 ) ;
#10305 = ORIENTED_EDGE ( 'NONE', *, *, #67999, .F. ) ;
#10306 = DIRECTION ( 'NONE',  ( -7.751221965937476285E-17, -1.000000000000000000, 0.000000000000000000 ) ) ;
#10307 = VECTOR ( 'NONE', #168, 1000.000000000000000 ) ;
#10308 = EDGE_CURVE ( 'NONE', #13785, #46983, #56200, .T. ) ;
#10309 = ORIENTED_EDGE ( 'NONE', *, *, #69352, .T. ) ;
#10310 = DIRECTION ( 'NONE',  ( 0.000000000000000000, 0.000000000000000000, 1.000000000000000000 ) ) ;
#10311 = AXIS2_PLACEMENT_3D ( 'NONE', #61480, #62536, #8090 ) ;
#10312 = DIRECTION ( 'NONE',  ( 0.000000000000000000, -1.000000000000000000, 0.000000000000000000 ) ) ;
#10313 = AXIS2_PLACEMENT_3D ( 'NONE', #43418, #61053, #33158 ) ;
#10314 = ORIENTED_EDGE ( 'NONE', *, *, #26422, .F. ) ;
#10315 = CARTESIAN_POINT ( 'NONE',  ( -16.75000000000000000, -0.3156864504677194816, 22.25638000318209109 ) ) ;
#10316 = LINE ( 'NONE', #63718, #28342 ) ;
#10317 = ORIENTED_EDGE ( 'NONE', *, *, #68111, .F. ) ;
#10318 = LINE ( 'NONE', #9980, #19930 ) ;
#10319 = CARTESIAN_POINT ( 'NONE',  ( 8.406483450353404052, 6.331612867284015955, 455.0000000000000568 ) ) ;
#10320 = EDGE_CURVE ( 'NONE', #68853, #13557, #51600, .T. ) ;
#10321 = LINE ( 'NONE', #9626, #61397 ) ;
#10322 = VERTEX_POINT ( 'NONE', #41324 ) ;
#10323 = CIRCLE ( 'NONE', #5834, 0.1999999999999987899 ) ;
#10324 = DIRECTION ( 'NONE',  ( 0.000000000000000000, -0.1249999999999996531, -0.9921567416492215186 ) ) ;
#10325 = ORIENTED_EDGE ( 'NONE', *, *, #20360, .T. ) ;
#10326 = EDGE_CURVE ( 'NONE', #57771, #6619, #30634, .T. ) ;
#10327 = ORIENTED_EDGE ( 'NONE', *, *, #49198, .F. ) ;
#10328 = EDGE_CURVE ( 'NONE', #41566, #64346, #171, .T. ) ;
#10329 = LINE ( 'NONE', #31903, #13300 ) ;
#10330 = DIRECTION ( 'NONE',  ( 0.000000000000000000, -1.000000000000000000, 0.000000000000000000 ) ) ;
#10331 = EDGE_CURVE ( 'NONE', #56057, #59106, #39915, .T. ) ;
#10332 = EDGE_CURVE ( 'NONE', #46652, #49722, #3162, .T. ) ;
#10333 = EDGE_CURVE ( 'NONE', #20182, #24541, #8810, .T. ) ;
#10334 = CARTESIAN_POINT ( 'NONE',  ( 8.250000000000005329, 7.250000000000000888, -25.00000000000000000 ) ) ;
#10335 = LINE ( 'NONE', #6074, #62262 ) ;
#10336 = ORIENTED_EDGE ( 'NONE', *, *, #63756, .F. ) ;
#10337 = ORIENTED_EDGE ( 'NONE', *, *, #29112, .T. ) ;
#10338 = AXIS2_PLACEMENT_3D ( 'NONE', #41508, #19585, #14295 ) ;
#10340 = ORIENTED_EDGE ( 'NONE', *, *, #2056, .F. ) ;
#10339 = LINE ( 'NONE', #17029, #21616 ) ;
#10341 = ADVANCED_FACE ( 'NONE', ( #35304 ), #14470, .F. ) ;
#10342 = ORIENTED_EDGE ( 'NONE', *, *, #4814, .T. ) ;
#10343 = CARTESIAN_POINT ( 'NONE',  ( 30.00000000000000000, -9.454754784057099570, -17.53999999999999915 ) ) ;
#10344 = DIRECTION ( 'NONE',  ( -0.000000000000000000, -0.000000000000000000, -1.000000000000000000 ) ) ;
#10345 = EDGE_CURVE ( 'NONE', #42153, #59069, #49814, .T. ) ;
#10346 = DIRECTION ( 'NONE',  ( 0.000000000000000000, 3.673940397442059868E-16, -1.000000000000000000 ) ) ;
#10347 = EDGE_CURVE ( 'NONE', #3392, #67717, #36025, .T. ) ;
#10348 = CARTESIAN_POINT ( 'NONE',  ( -3.663616288757055806, 6.350872789121238426, 54.00000000000000711 ) ) ;
#10350 = DIRECTION ( 'NONE',  ( 0.000000000000000000, 0.000000000000000000, -1.000000000000000000 ) ) ;
#10349 = PLANE ( 'NONE',  #67077 ) ;
#10351 = VERTEX_POINT ( 'NONE', #34962 ) ;
#10352 = ORIENTED_EDGE ( 'NONE', *, *, #37891, .F. ) ;
#10353 = EDGE_LOOP ( 'NONE', ( #42863, #10231, #38646, #6032 ) ) ;
#10354 = EDGE_LOOP ( 'NONE', ( #36290, #45338 ) ) ;
#10355 = VECTOR ( 'NONE', #2484, 1000.000000000000000 ) ;
#10356 = CLOSED_SHELL ( 'NONE', ( #60776, #47861, #55838, #13903, #29892, #53287, #10385, #25898, #26098, #27068 ) ) ;
#10357 = DIRECTION ( 'NONE',  ( 0.000000000000000000, -1.000000000000000000, 0.000000000000000000 ) ) ;
#10358 = EDGE_CURVE ( 'NONE', #24992, #68360, #46280, .T. ) ;
#10359 = DIRECTION ( 'NONE',  ( -1.000000000000000000, 0.000000000000000000, 0.000000000000000000 ) ) ;
#10360 = VECTOR ( 'NONE', #52069, 1000.000000000000000 ) ;
#10361 = EDGE_CURVE ( 'NONE', #10509, #66537, #3541, .T. ) ;
#10362 = CARTESIAN_POINT ( 'NONE',  ( 2.706483450353419862, 10.91351654964658735, 455.0000000000000568 ) ) ;
#10363 = VERTEX_POINT ( 'NONE', #29662 ) ;
#10364 = ORIENTED_EDGE ( 'NONE', *, *, #11148, .T. ) ;
#10365 = ORIENTED_EDGE ( 'NONE', *, *, #10050, .F. ) ;
#10366 = DIRECTION ( 'NONE',  ( 0.000000000000000000, 0.000000000000000000, 1.000000000000000000 ) ) ;
#10367 = ORIENTED_EDGE ( 'NONE', *, *, #29531, .F. ) ;
#10368 = CARTESIAN_POINT ( 'NONE',  ( 2.906483450353372078, 10.91351654964663531, 195.0000000000000284 ) ) ;
#10369 = DIRECTION ( 'NONE',  ( -0.000000000000000000, -0.000000000000000000, 1.000000000000000000 ) ) ;
#10370 = ORIENTED_EDGE ( 'NONE', *, *, #61991, .F. ) ;
#10371 = ORIENTED_EDGE ( 'NONE', *, *, #12455, .F. ) ;
#10372 = CARTESIAN_POINT ( 'NONE',  ( -8.249999999999996447, 8.250000000000001776, -1.000000000000000000 ) ) ;
#10374 = VERTEX_POINT ( 'NONE', #30376 ) ;
#10373 = LINE ( 'NONE', #65504, #654 ) ;
#10375 = ORIENTED_EDGE ( 'NONE', *, *, #54242, .F. ) ;
#10376 = VECTOR ( 'NONE', #64900, 1000.000000000000000 ) ;
#10377 = LINE ( 'NONE', #14625, #64121 ) ;
#10379 = ORIENTED_EDGE ( 'NONE', *, *, #1370, .T. ) ;
#10378 = CARTESIAN_POINT ( 'NONE',  ( -8.250000000000000000, 7.250000000000001776, -17.00000000000000000 ) ) ;
#10380 = VERTEX_POINT ( 'NONE', #35664 ) ;
#10381 = CARTESIAN_POINT ( 'NONE',  ( -25.50000000000000355, -15.50000000000000000, -22.50000000000000000 ) ) ;
#10382 = DIRECTION ( 'NONE',  ( 0.000000000000000000, 1.000000000000000000, 0.000000000000000000 ) ) ;
#10383 = PLANE ( 'NONE',  #11431 ) ;
#10384 = DIRECTION ( 'NONE',  ( 0.000000000000000000, 1.000000000000000000, 0.000000000000000000 ) ) ;
#10385 = ADVANCED_FACE ( 'NONE', ( #24370 ), #2449, .T. ) ;
#10386 = CYLINDRICAL_SURFACE ( 'NONE', #12397, 0.7500000000000006661 ) ;
#10387 = CIRCLE ( 'NONE', #16043, 1.000000000000000000 ) ;
#10388 = ORIENTED_EDGE ( 'NONE', *, *, #67041, .T. ) ;
#10389 = CARTESIAN_POINT ( 'NONE',  ( 1.690483450353415629, 9.828310488885938057, 455.0000000000000568 ) ) ;
#10390 = EDGE_CURVE ( 'NONE', #55788, #60123, #3508, .T. ) ;
#10391 = VERTEX_POINT ( 'NONE', #18708 ) ;
#10392 = CARTESIAN_POINT ( 'NONE',  ( 7.250000000000004441, 7.450000000000001954, -8.500000000000000000 ) ) ;
#10393 = CARTESIAN_POINT ( 'NONE',  ( 16.75000000000000000, -0.3156864504677172611, 22.74361999681791602 ) ) ;
#10395 = EDGE_CURVE ( 'NONE', #10, #54618, #25075, .T. ) ;
#10394 = FACE_OUTER_BOUND ( 'NONE', #68154, .T. ) ;
#10396 = CARTESIAN_POINT ( 'NONE',  ( 30.00000000000000000, -16.64230188589299786, -14.64519951917100116 ) ) ;
#10397 = CARTESIAN_POINT ( 'NONE',  ( 11.50000000000000000, -12.00000000000000000, -11.00000000000000000 ) ) ;
#10398 = EDGE_CURVE ( 'NONE', #58826, #43972, #58307, .T. ) ;
#10399 = AXIS2_PLACEMENT_3D ( 'NONE', #58947, #63562, #27120 ) ;
#10400 = VECTOR ( 'NONE', #67372, 1000.000000000000000 ) ;
#10401 = ORIENTED_EDGE ( 'NONE', *, *, #35369, .T. ) ;
#10402 = CARTESIAN_POINT ( 'NONE',  ( 30.00000000000000000, -12.00000000000000000, -10.52786404500095863 ) ) ;
#10403 = EDGE_CURVE ( 'NONE', #47349, #27438, #52660, .T. ) ;
#10404 = FACE_OUTER_BOUND ( 'NONE', #63044, .T. ) ;
#10405 = ORIENTED_EDGE ( 'NONE', *, *, #52968, .T. ) ;
#10406 = LINE ( 'NONE', #31981, #31619 ) ;
#10407 = DIRECTION ( 'NONE',  ( -0.7671651518152895477, 0.6414496315691698980, -2.309356642088442522E-17 ) ) ;
#10408 = FACE_OUTER_BOUND ( 'NONE', #28695, .T. ) ;
#10409 = EDGE_LOOP ( 'NONE', ( #55998, #51087, #40356, #68383 ) ) ;
#10410 = AXIS2_PLACEMENT_3D ( 'NONE', #30394, #51963, #29326 ) ;
#10411 = DIRECTION ( 'NONE',  ( 0.000000000000000000, 0.000000000000000000, -1.000000000000000000 ) ) ;
#10412 = FACE_OUTER_BOUND ( 'NONE', #21768, .T. ) ;
#10413 = ORIENTED_EDGE ( 'NONE', *, *, #31999, .T. ) ;
#10414 = FACE_OUTER_BOUND ( 'NONE', #15786, .T. ) ;
#10415 = CARTESIAN_POINT ( 'NONE',  ( 6.358413763958960629, 5.779227145995223580, 54.00000000000000711 ) ) ;
#10416 = LINE ( 'NONE', #53557, #46972 ) ;
#10417 = ADVANCED_FACE ( 'NONE', ( #37093 ), #58994, .T. ) ;
#10418 = CARTESIAN_POINT ( 'NONE',  ( -2.752095193409509033, -9.955011587777317317, 455.0000000000000568 ) ) ;
#10419 = DIRECTION ( 'NONE',  ( 0.000000000000000000, 0.000000000000000000, -1.000000000000000000 ) ) ;
#10420 = ORIENTED_EDGE ( 'NONE', *, *, #48125, .F. ) ;
#10422 = VERTEX_POINT ( 'NONE', #69947 ) ;
#10421 = CARTESIAN_POINT ( 'NONE',  ( 0.000000000000000000, -21.00000000000000000, -5.000000000000000000 ) ) ;
#10423 = CARTESIAN_POINT ( 'NONE',  ( -17.00000000000000000, -15.50000000000000000, 14.50000000000000000 ) ) ;
#10424 = CARTESIAN_POINT ( 'NONE',  ( -8.250000000000001776, 0.000000000000000000, -9.000000000000001776 ) ) ;
#10425 = DIRECTION ( 'NONE',  ( 0.000000000000000000, 0.000000000000000000, -1.000000000000000000 ) ) ;
#10426 = EDGE_LOOP ( 'NONE', ( #3999, #7416, #55145, #46573 ) ) ;
#10427 = CARTESIAN_POINT ( 'NONE',  ( 11.75000000000000000, -5.000000000000000000, -26.25000000000000000 ) ) ;
#10428 = DIRECTION ( 'NONE',  ( -0.000000000000000000, 3.673940397442059868E-16, -1.000000000000000000 ) ) ;
#10429 = ORIENTED_EDGE ( 'NONE', *, *, #57163, .T. ) ;
#10430 = EDGE_LOOP ( 'NONE', ( #42821, #38084, #65221, #43435 ) ) ;
#10431 = ORIENTED_EDGE ( 'NONE', *, *, #40306, .T. ) ;
#10432 = VECTOR ( 'NONE', #49766, 1000.000000000000000 ) ;
#10433 = EDGE_CURVE ( 'NONE', #48685, #19113, #4907, .T. ) ;
#10434 = CARTESIAN_POINT ( 'NONE',  ( -8.250000000000001776, -7.249999999999998224, -15.00000000000000000 ) ) ;
#10435 = DIRECTION ( 'NONE',  ( -0.000000000000000000, -0.000000000000000000, -1.000000000000000000 ) ) ;
#10437 = EDGE_CURVE ( 'NONE', #59528, #33844, #47336, .T. ) ;
#10436 = CARTESIAN_POINT ( 'NONE',  ( 7.250000000000005329, -7.249999999999998224, -26.00000000000001066 ) ) ;
#10438 = EDGE_LOOP ( 'NONE', ( #15431, #69587, #10085, #49110, #25816, #61554, #12671, #54765 ) ) ;
#10439 = ORIENTED_EDGE ( 'NONE', *, *, #4812, .T. ) ;
#10440 = CARTESIAN_POINT ( 'NONE',  ( 9.106483450353380249, -11.12648345035339048, 195.0000000000000284 ) ) ;
#10441 = ORIENTED_EDGE ( 'NONE', *, *, #29304, .T. ) ;
#10442 = EDGE_LOOP ( 'NONE', ( #16356, #46252, #61479, #21055 ) ) ;
#10443 = AXIS2_PLACEMENT_3D ( 'NONE', #2585, #67645, #45711 ) ;
#10444 = ORIENTED_EDGE ( 'NONE', *, *, #64810, .F. ) ;
#10445 = ORIENTED_EDGE ( 'NONE', *, *, #66823, .T. ) ;
#10446 = LINE ( 'NONE', #15755, #63211 ) ;
#10448 = VERTEX_POINT ( 'NONE', #21174 ) ;
#10447 = CARTESIAN_POINT ( 'NONE',  ( 0.5000000000000000000, 21.00000000000000000, -18.00000000000000355 ) ) ;
#10449 = CARTESIAN_POINT ( 'NONE',  ( -10.19191654964680360, -9.804883450353337082, 195.0000000000000284 ) ) ;
#10451 = CARTESIAN_POINT ( 'NONE',  ( 9.737023737882815055, -7.969523737882814984, 26.00000000000000000 ) ) ;
#10450 = VECTOR ( 'NONE', #48953, 1000.000000000000000 ) ;
#10452 = DIRECTION ( 'NONE',  ( 1.000000000000000000, 0.000000000000000000, 0.000000000000000000 ) ) ;
#10453 = ORIENTED_EDGE ( 'NONE', *, *, #26374, .T. ) ;
#10454 = CIRCLE ( 'NONE', #52192, 0.4000000000000617506 ) ;
#10455 = VECTOR ( 'NONE', #23600, 1000.000000000000114 ) ;
#10456 = DIRECTION ( 'NONE',  ( -1.000000000000000000, 0.000000000000000000, 0.000000000000000000 ) ) ;
#10457 = CIRCLE ( 'NONE', #56779, 0.5249999999999990230 ) ;
#10458 = LINE ( 'NONE', #10116, #60899 ) ;
#10459 = ORIENTED_EDGE ( 'NONE', *, *, #55328, .T. ) ;
#10460 = EDGE_CURVE ( 'NONE', #13296, #61211, #13976, .T. ) ;
#10461 = VECTOR ( 'NONE', #32194, 1000.000000000000000 ) ;
#10462 = FILL_AREA_STYLE ('',( #21419 ) ) ;
#10463 = CARTESIAN_POINT ( 'NONE',  ( 23.90000000000000213, 0.000000000000000000, 1.723948796001796511E-15 ) ) ;
#10464 = ORIENTED_EDGE ( 'NONE', *, *, #52986, .F. ) ;
#10466 = EDGE_CURVE ( 'NONE', #67402, #43025, #42726, .T. ) ;
#10465 = LINE ( 'NONE', #42645, #42602 ) ;
#10467 = DIRECTION ( 'NONE',  ( 0.000000000000000000, 0.000000000000000000, 1.000000000000000000 ) ) ;
#10468 = CYLINDRICAL_SURFACE ( 'NONE', #13270, 2.204799999999997429 ) ;
#10469 = EDGE_CURVE ( 'NONE', #64055, #62485, #14818, .T. ) ;
#10470 = AXIS2_PLACEMENT_3D ( 'NONE', #62385, #1597, #39427 ) ;
#10471 = EDGE_CURVE ( 'NONE', #43574, #11904, #32483, .T. ) ;
#10472 = DIRECTION ( 'NONE',  ( -1.000000000000000000, 0.000000000000000000, 0.000000000000000000 ) ) ;
#10473 = EDGE_CURVE ( 'NONE', #54618, #50768, #64306, .T. ) ;
#10474 = CARTESIAN_POINT ( 'NONE',  ( 13.90000000000000213, -0.1999999999911430404, -8.864436962241481021E-12 ) ) ;
#10475 = EDGE_CURVE ( 'NONE', #8148, #18538, #48387, .T. ) ;
#10476 = CARTESIAN_POINT ( 'NONE',  ( -8.393516549646712122, 7.603567055985436696, 455.0000000000000568 ) ) ;
#10477 = AXIS2_PLACEMENT_3D ( 'NONE', #8356, #3081, #63872 ) ;
#10478 = CARTESIAN_POINT ( 'NONE',  ( 2.544523737882792069, -8.835729544836313565, 26.00000000000000000 ) ) ;
#10479 = PLANE ( 'NONE',  #15347 ) ;
#10480 = EDGE_CURVE ( 'NONE', #24611, #39384, #5264, .T. ) ;
#10481 = ORIENTED_EDGE ( 'NONE', *, *, #67959, .T. ) ;
#10482 = CYLINDRICAL_SURFACE ( 'NONE', #21361, 24.99999999998784972 ) ;
#10483 = PLANE ( 'NONE',  #54528 ) ;
#10484 = DIRECTION ( 'NONE',  ( 0.000000000000000000, -0.7071067811828075644, 0.7071067811902875810 ) ) ;
#10485 = DIRECTION ( 'NONE',  ( 1.836970198721029934E-16, 1.836970198721010706E-16, -1.000000000000000000 ) ) ;
#10486 = VERTEX_POINT ( 'NONE', #16205 ) ;
#10487 = DIRECTION ( 'NONE',  ( 0.6414496315691494699, 0.7671651518153064231, 2.818519042764025305E-16 ) ) ;
#10488 = DIRECTION ( 'NONE',  ( 1.836970198721029934E-16, 1.836970198721010706E-16, -1.000000000000000000 ) ) ;
#10489 = PLANE ( 'NONE',  #48102 ) ;
#10490 = CARTESIAN_POINT ( 'NONE',  ( 55.00000000000000000, -0.1999999999911795112, 8.826273045769999343E-12 ) ) ;
#10491 = CARTESIAN_POINT ( 'NONE',  ( -6.651770455163781293, -7.357023737882790293, 54.00000000000000711 ) ) ;
#10492 = PLANE ( 'NONE',  #57682 ) ;
#10493 = ORIENTED_EDGE ( 'NONE', *, *, #26422, .T. ) ;
#10494 = VECTOR ( 'NONE', #37223, 1000.000000000000114 ) ;
#10495 = ORIENTED_EDGE ( 'NONE', *, *, #43961, .T. ) ;
#10496 = CYLINDRICAL_SURFACE ( 'NONE', #67708, 24.99999999998789946 ) ;
#10497 = DIRECTION ( 'NONE',  ( 0.000000000000000000, -0.000000000000000000, 1.000000000000000000 ) ) ;
#10498 = VERTEX_POINT ( 'NONE', #26831 ) ;
#10499 = FACE_OUTER_BOUND ( 'NONE', #5224, .T. ) ;
#10500 = VECTOR ( 'NONE', #1956, 1000.000000000000000 ) ;
#10501 = AXIS2_PLACEMENT_3D ( 'NONE', #2045, #17949, #49459 ) ;
#10502 = CARTESIAN_POINT ( 'NONE',  ( 7.000000000000000000, -30.45000000000094786, -14.49999999999906031 ) ) ;
#10503 = VERTEX_POINT ( 'NONE', #10208 ) ;
#10504 = CARTESIAN_POINT ( 'NONE',  ( -9.828310488886053520, 1.677516549646603794, 455.0000000000000568 ) ) ;
#10505 = ORIENTED_EDGE ( 'NONE', *, *, #39519, .F. ) ;
#10506 = CIRCLE ( 'NONE', #34154, 4.000000000000000888 ) ;
#10507 = VERTEX_POINT ( 'NONE', #42032 ) ;
#10508 = PLANE ( 'NONE',  #30629 ) ;
#10509 = VERTEX_POINT ( 'NONE', #32125 ) ;
#10510 = DIRECTION ( 'NONE',  ( 1.000000000000000000, -0.000000000000000000, 0.000000000000000000 ) ) ;
#10511 = CARTESIAN_POINT ( 'NONE',  ( -15.50000000000129852, -15.50000000000000000, 22.50000000000000000 ) ) ;
#10513 = ADVANCED_FACE ( 'NONE', ( #47688 ), #69255, .T. ) ;
#10512 = LINE ( 'NONE', #36694, #30236 ) ;
#10514 = VECTOR ( 'NONE', #6697, 1000.000000000000000 ) ;
#10515 = ORIENTED_EDGE ( 'NONE', *, *, #62383, .F. ) ;
#10517 = ADVANCED_FACE ( 'NONE', ( #64641 ), #4223, .F. ) ;
#10516 = ORIENTED_EDGE ( 'NONE', *, *, #35897, .F. ) ;
#10518 = DIRECTION ( 'NONE',  ( 0.000000000000000000, 0.000000000000000000, 1.000000000000000000 ) ) ;
#10519 = EDGE_CURVE ( 'NONE', #63196, #13233, #62523, .T. ) ;
#10521 = LINE ( 'NONE', #63216, #48007 ) ;
#10520 = LINE ( 'NONE', #59307, #37226 ) ;
#10522 = VERTEX_POINT ( 'NONE', #15172 ) ;
#10523 = VECTOR ( 'NONE', #67975, 1000.000000000000000 ) ;
#10524 = ORIENTED_EDGE ( 'NONE', *, *, #31643, .T. ) ;
#10525 = EDGE_CURVE ( 'NONE', #64753, #20149, #20811, .T. ) ;
#10527 = EDGE_LOOP ( 'NONE', ( #60564, #17112, #37313, #29831 ) ) ;
#10526 = APPLICATION_PROTOCOL_DEFINITION ( 'draft international standard', 'automotive_design', 1998, #52631 ) ;
#10528 = CARTESIAN_POINT ( 'NONE',  ( -4.188533722949335569, 7.259684009079808931, 195.0000000000000284 ) ) ;
#10529 = VECTOR ( 'NONE', #10186, 1000.000000000000000 ) ;
#10531 = ORIENTED_EDGE ( 'NONE', *, *, #9950, .T. ) ;
#10530 = CARTESIAN_POINT ( 'NONE',  ( 25.57999999999999829, 6.429395695523604153E-16, -5.250000000000000000 ) ) ;
#10532 = CARTESIAN_POINT ( 'NONE',  ( 7.250000000000005329, 8.250000000000001776, -26.00000000000001066 ) ) ;
#10533 = CARTESIAN_POINT ( 'NONE',  ( -4.188533722949417282, -4.740315990920197287, 455.0000000000000568 ) ) ;
#10534 = ORIENTED_EDGE ( 'NONE', *, *, #45684, .F. ) ;
#10535 = EDGE_LOOP ( 'NONE', ( #42693, #16764, #21632, #60790 ) ) ;
#10536 = AXIS2_PLACEMENT_3D ( 'NONE', #11629, #21237, #42783 ) ;
#10537 = FACE_OUTER_BOUND ( 'NONE', #40215, .T. ) ;
#10538 = VERTEX_POINT ( 'NONE', #15529 ) ;
#10539 = FACE_OUTER_BOUND ( 'NONE', #18475, .T. ) ;
#10540 = LINE ( 'NONE', #36724, #30134 ) ;
#10541 = DIRECTION ( 'NONE',  ( 1.836970198721029934E-16, 1.836970198721010706E-16, -1.000000000000000000 ) ) ;
#10542 = ORIENTED_EDGE ( 'NONE', *, *, #6881, .T. ) ;
#10543 = EDGE_CURVE ( 'NONE', #13405, #30457, #28659, .T. ) ;
#10544 = VECTOR ( 'NONE', #57644, 1000.000000000000000 ) ;
#10545 = CARTESIAN_POINT ( 'NONE',  ( 0.000000000000000000, -7.449999999999998401, -13.50000000000000178 ) ) ;
#10547 = ORIENTED_EDGE ( 'NONE', *, *, #29465, .T. ) ;
#10546 = LINE ( 'NONE', #37431, #69261 ) ;
#10548 = ORIENTED_EDGE ( 'NONE', *, *, #46218, .T. ) ;
#10550 = CARTESIAN_POINT ( 'NONE',  ( 40.90000000000000568, 21.00000000000000000, -16.96999999999999886 ) ) ;
#10549 = AXIS2_PLACEMENT_3D ( 'NONE', #49194, #69105, #9717 ) ;
#10551 = AXIS2_PLACEMENT_3D ( 'NONE', #60667, #33785, #12555 ) ;
#10553 = VECTOR ( 'NONE', #35459, 1000.000000000000000 ) ;
#10552 = LINE ( 'NONE', #21512, #287 ) ;
#10554 = DIRECTION ( 'NONE',  ( 0.7071067811865474617, -0.7071067811865474617, 0.000000000000000000 ) ) ;
#10555 = CARTESIAN_POINT ( 'NONE',  ( 3.606483450353358045, 7.415254214038261793, 195.0000000000000284 ) ) ;
#10556 = VECTOR ( 'NONE', #2712, 1000.000000000000000 ) ;
#10557 = DIRECTION ( 'NONE',  ( 1.836970198721029934E-16, -1.836970198721036344E-16, 1.000000000000000000 ) ) ;
#10558 = VERTEX_POINT ( 'NONE', #64998 ) ;
#10559 = FACE_OUTER_BOUND ( 'NONE', #43967, .T. ) ;
#10560 = EDGE_CURVE ( 'NONE', #42109, #57811, #17922, .T. ) ;
#10561 = DIRECTION ( 'NONE',  ( 0.000000000000000000, 0.000000000000000000, -1.000000000000000000 ) ) ;
#10562 = DIRECTION ( 'NONE',  ( -0.6414496315691617934, 0.7671651518152962090, 0.000000000000000000 ) ) ;
#10564 = EDGE_LOOP ( 'NONE', ( #29197, #60201, #62002, #39138 ) ) ;
#10563 = CARTESIAN_POINT ( 'NONE',  ( -18.85410196625000268, -15.50000000000000000, -21.50000000000000000 ) ) ;
#10565 = FILL_AREA_STYLE ('',( #59006 ) ) ;
#10566 = EDGE_CURVE ( 'NONE', #55087, #14072, #12608, .T. ) ;
#10567 = FACE_OUTER_BOUND ( 'NONE', #6918, .T. ) ;
#10568 = DIRECTION ( 'NONE',  ( 0.000000000000000000, 0.000000000000000000, 1.000000000000000000 ) ) ;
#10569 = CARTESIAN_POINT ( 'NONE',  ( 11.50000000000000000, -15.97213595500069871, 14.50000000000000000 ) ) ;
#10570 = ORIENTED_EDGE ( 'NONE', *, *, #38115, .T. ) ;
#10571 = DIRECTION ( 'NONE',  ( 0.000000000000000000, 0.000000000000000000, -1.000000000000000000 ) ) ;
#10572 = CARTESIAN_POINT ( 'NONE',  ( 8.250000000000005329, 7.250000000000000888, -26.00000000000001066 ) ) ;
#10573 = EDGE_LOOP ( 'NONE', ( #66684, #35800, #43769, #46663, #25940, #59232, #19418, #44591 ) ) ;
#10574 = CARTESIAN_POINT ( 'NONE',  ( -7.450000000000001954, -7.249999999999998224, -8.500000000000000000 ) ) ;
#10575 = FACE_OUTER_BOUND ( 'NONE', #44652, .T. ) ;
#10576 = CARTESIAN_POINT ( 'NONE',  ( -10.49297626211729018, -6.849523737882743823, 26.00000000000000000 ) ) ;
#10577 = DIRECTION ( 'NONE',  ( 1.000000000000000000, 0.000000000000000000, 0.000000000000000000 ) ) ;
#10579 = ADVANCED_FACE ( 'NONE', ( #22891 ), #16902, .F. ) ;
#10578 = CARTESIAN_POINT ( 'NONE',  ( -6.822336235477446387, 4.135079735113101229, 26.00000000000000711 ) ) ;
#10580 = EDGE_LOOP ( 'NONE', ( #69419, #36798 ) ) ;
#10581 = ORIENTED_EDGE ( 'NONE', *, *, #68969, .T. ) ;
#10582 = CARTESIAN_POINT ( 'NONE',  ( 37.90000000000000568, -0.2000000000089119934, -8.913009219568841313E-12 ) ) ;
#10583 = ORIENTED_EDGE ( 'NONE', *, *, #37235, .T. ) ;
#10584 = ORIENTED_EDGE ( 'NONE', *, *, #45741, .T. ) ;
#10585 = DIRECTION ( 'NONE',  ( 0.000000000000000000, 0.000000000000000000, 1.000000000000000000 ) ) ;
#10586 = DIRECTION ( 'NONE',  ( -1.000000000000000000, 0.000000000000000000, 0.000000000000000000 ) ) ;
#10587 = DIRECTION ( 'NONE',  ( 0.000000000000000000, 0.000000000000000000, 1.000000000000000000 ) ) ;
#10588 = ORIENTED_EDGE ( 'NONE', *, *, #35353, .F. ) ;
#10589 = APPLICATION_CONTEXT ( 'automotive_design' ) ;
#10590 = ORIENTED_EDGE ( 'NONE', *, *, #25741, .F. ) ;
#10591 = DIRECTION ( 'NONE',  ( 0.000000000000000000, 1.000000000000000000, 0.000000000000000000 ) ) ;
#10592 = ORIENTED_EDGE ( 'NONE', *, *, #9471, .F. ) ;
#10593 = VERTEX_POINT ( 'NONE', #38138 ) ;
#10594 = CARTESIAN_POINT ( 'NONE',  ( -10.19191654964686578, -11.08848345035334759, 455.0000000000000568 ) ) ;
#10595 = DIRECTION ( 'NONE',  ( 0.000000000000000000, -0.7071067811865475727, 0.7071067811865475727 ) ) ;
#10596 = AXIS2_PLACEMENT_3D ( 'NONE', #20916, #15272, #41437 ) ;
#10597 = AXIS2_PLACEMENT_3D ( 'NONE', #24947, #51820, #36977 ) ;
#10598 = DIRECTION ( 'NONE',  ( -9.912705577010336396E-15, -1.000000000000000000, 0.000000000000000000 ) ) ;
#10599 = ORIENTED_EDGE ( 'NONE', *, *, #41014, .T. ) ;
#10600 = EDGE_CURVE ( 'NONE', #14190, #15650, #11570, .T. ) ;
#10601 = DIRECTION ( 'NONE',  ( -4.956352788505180820E-15, -1.000000000000000000, 0.000000000000000000 ) ) ;
#10603 = FACE_OUTER_BOUND ( 'NONE', #65006, .T. ) ;
#10602 = CARTESIAN_POINT ( 'NONE',  ( 275.0000000000000000, -42.00000000000000000, 15.10000000000000142 ) ) ;
#10604 = VECTOR ( 'NONE', #53911, 1000.000000000000000 ) ;
#10606 = ORIENTED_EDGE ( 'NONE', *, *, #4289, .T. ) ;
#10605 = VECTOR ( 'NONE', #3685, 1000.000000000000000 ) ;
#10608 = ORIENTED_EDGE ( 'NONE', *, *, #52280, .F. ) ;
#10607 = CARTESIAN_POINT ( 'NONE',  ( 47.00000000000000000, 0.7500000000000000000, -4.943429983321300014 ) ) ;
#10609 = VERTEX_POINT ( 'NONE', #65682 ) ;
#10610 = EDGE_CURVE ( 'NONE', #60691, #39415, #28336, .T. ) ;
#10611 = CIRCLE ( 'NONE', #34299, 24.99999999998784972 ) ;
#10612 = CIRCLE ( 'NONE', #7155, 0.1749999999999980738 ) ;
#10613 = CARTESIAN_POINT ( 'NONE',  ( 9.929523737882817613, -0.9555237378828154160, 26.00000000000000711 ) ) ;
#10614 = CARTESIAN_POINT ( 'NONE',  ( 20.90000000000000213, -14.06939075806900163, -20.80000000000000426 ) ) ;
#10615 = EDGE_LOOP ( 'NONE', ( #11225, #8264, #59351, #60070 ) ) ;
#10616 = CIRCLE ( 'NONE', #55777, 2.204799999999999205 ) ;
#10617 = CARTESIAN_POINT ( 'NONE',  ( -7.250000000000000888, 7.250000000000001776, -17.00000000000000000 ) ) ;
#10618 = CARTESIAN_POINT ( 'NONE',  ( -4.393516549646671265, 11.31351654964658771, 195.0000000000000284 ) ) ;
#10619 = ORIENTED_EDGE ( 'NONE', *, *, #51588, .T. ) ;
#10620 = VERTEX_POINT ( 'NONE', #1331 ) ;
#10621 = DIRECTION ( 'NONE',  ( -1.000000000000000000, 0.000000000000000000, 0.000000000000000000 ) ) ;
#10622 = CARTESIAN_POINT ( 'NONE',  ( 283.0000000000000568, -42.50000000000000000, 7.500000000000000000 ) ) ;
#10623 = EDGE_CURVE ( 'NONE', #61120, #68364, #5601, .T. ) ;
#10624 = FACE_OUTER_BOUND ( 'NONE', #28505, .T. ) ;
#10625 = ORIENTED_EDGE ( 'NONE', *, *, #42876, .F. ) ;
#10626 = CARTESIAN_POINT ( 'NONE',  ( 41.09999999999999432, 20.60000000000000142, -13.86939075806900057 ) ) ;
#10627 = CARTESIAN_POINT ( 'NONE',  ( 14.89999999999999680, 20.60000000000000142, -13.86939075806900057 ) ) ;
#10629 = ORIENTED_EDGE ( 'NONE', *, *, #6172, .T. ) ;
#10628 = DIRECTION ( 'NONE',  ( 0.000000000000000000, 3.673940397442059868E-16, -1.000000000000000000 ) ) ;
#10631 = ORIENTED_EDGE ( 'NONE', *, *, #3204, .T. ) ;
#10630 = DIRECTION ( 'NONE',  ( 1.836970198721029934E-16, 1.836970198721010706E-16, -1.000000000000000000 ) ) ;
#10632 = DIRECTION ( 'NONE',  ( 0.000000000000000000, -0.1249999999999996531, -0.9921567416492215186 ) ) ;
#10633 = CARTESIAN_POINT ( 'NONE',  ( 11.50000000000000000, -11.50000000000000000, 19.00000000000000000 ) ) ;
#10634 = VECTOR ( 'NONE', #52323, 1000.000000000000114 ) ;
#10635 = DIRECTION ( 'NONE',  ( 1.000000000000000000, 0.000000000000000000, 0.000000000000000000 ) ) ;
#10636 = FACE_OUTER_BOUND ( 'NONE', #48429, .T. ) ;
#10637 = CYLINDRICAL_SURFACE ( 'NONE', #21510, 1.000000000000000000 ) ;
#10638 = FACE_OUTER_BOUND ( 'NONE', #6776, .T. ) ;
#10639 = EDGE_LOOP ( 'NONE', ( #15822, #40608, #5220, #13971 ) ) ;
#10640 = CARTESIAN_POINT ( 'NONE',  ( 30.00000000000000000, 0.000000000000000000, 27.00000000000000000 ) ) ;
#10641 = EDGE_CURVE ( 'NONE', #9530, #27811, #38801, .T. ) ;
#10643 = VERTEX_POINT ( 'NONE', #642 ) ;
#10642 = DIRECTION ( 'NONE',  ( 0.6414496315691617934, 0.7671651518152962090, -0.000000000000000000 ) ) ;
#10645 = ORIENTED_EDGE ( 'NONE', *, *, #8644, .F. ) ;
#10644 = DIRECTION ( 'NONE',  ( 0.000000000000000000, 0.000000000000000000, 1.000000000000000000 ) ) ;
#10646 = VECTOR ( 'NONE', #26151, 1000.000000000000000 ) ;
#10647 = AXIS2_PLACEMENT_3D ( 'NONE', #48532, #37585, #59491 ) ;
#10648 = DIRECTION ( 'NONE',  ( 1.000000000000000000, -8.728482790395504563E-15, 0.000000000000000000 ) ) ;
#10649 = EDGE_CURVE ( 'NONE', #24983, #30361, #59689, .T. ) ;
#10650 = ADVANCED_FACE ( 'NONE', ( #38473 ), #6286, .T. ) ;
#10651 = CARTESIAN_POINT ( 'NONE',  ( 8.900000000000005684, 21.00000000000000355, -13.98999642601812354 ) ) ;
#10652 = VECTOR ( 'NONE', #4622, 1000.000000000000000 ) ;
#10653 = AXIS2_PLACEMENT_3D ( 'NONE', #9552, #41362, #36415 ) ;
#10654 = AXIS2_PLACEMENT_3D ( 'NONE', #52849, #31282, #24900 ) ;
#10655 = EDGE_CURVE ( 'NONE', #27235, #29819, #54048, .T. ) ;
#10656 = ORIENTED_EDGE ( 'NONE', *, *, #45022, .F. ) ;
#10657 = LINE ( 'NONE', #36126, #36537 ) ;
#10658 = CARTESIAN_POINT ( 'NONE',  ( -7.250000000000000888, -8.249999999999998224, -9.500000000000001776 ) ) ;
#10659 = ORIENTED_EDGE ( 'NONE', *, *, #11399, .F. ) ;
#10660 = DIRECTION ( 'NONE',  ( 0.000000000000000000, 0.000000000000000000, -1.000000000000000000 ) ) ;
#10661 = DIRECTION ( 'NONE',  ( 1.836970198721029934E-16, 1.836970198721010706E-16, -1.000000000000000000 ) ) ;
#10662 = EDGE_CURVE ( 'NONE', #48157, #35812, #11917, .T. ) ;
#10663 = CONICAL_SURFACE ( 'NONE', #27570, 2.000000000000001776, 0.7853981633974503884 ) ;
#10664 = LINE ( 'NONE', #37543, #56248 ) ;
#10665 = EDGE_CURVE ( 'NONE', #45716, #44206, #60718, .T. ) ;
#10666 = EDGE_CURVE ( 'NONE', #12808, #31731, #999, .T. ) ;
#10667 = VERTEX_POINT ( 'NONE', #33504 ) ;
#10668 = CARTESIAN_POINT ( 'NONE',  ( -11.75000000000000000, -5.200000000000001066, -26.25000000000000000 ) ) ;
#10669 = ORIENTED_EDGE ( 'NONE', *, *, #7260, .F. ) ;
#10670 = ORIENTED_EDGE ( 'NONE', *, *, #4469, .T. ) ;
#10671 = VECTOR ( 'NONE', #10006, 1000.000000000000000 ) ;
#10672 = CARTESIAN_POINT ( 'NONE',  ( 6.836383711243002814, 6.350872789121261519, 54.00000000000000711 ) ) ;
#10673 = DIRECTION ( 'NONE',  ( -1.836970198721029934E-16, -1.836970198721010706E-16, 1.000000000000000000 ) ) ;
#10674 = CARTESIAN_POINT ( 'NONE',  ( -7.798499376344067535, 7.259684009079840017, 455.0000000000000568 ) ) ;
#10675 = CARTESIAN_POINT ( 'NONE',  ( -7.415254214038336400, 3.593516549646602609, 455.0000000000000568 ) ) ;
#10676 = VERTEX_POINT ( 'NONE', #43415 ) ;
#10677 = ORIENTED_EDGE ( 'NONE', *, *, #49535, .T. ) ;
#10679 = EDGE_LOOP ( 'NONE', ( #43393, #12772, #10728, #59459 ) ) ;
#10678 = LINE ( 'NONE', #43545, #57737 ) ;
#10680 = ORIENTED_EDGE ( 'NONE', *, *, #10543, .T. ) ;
#10681 = CARTESIAN_POINT ( 'NONE',  ( 7.250000000000005329, 8.250000000000001776, -25.00000000000000000 ) ) ;
#10682 = CARTESIAN_POINT ( 'NONE',  ( 7.250000000000004441, 7.450000000000001954, -10.00000000000000000 ) ) ;
#10683 = CARTESIAN_POINT ( 'NONE',  ( -10.50000000000000178, 9.690000000000001279, -5.000000000000000000 ) ) ;
#10684 = AXIS2_PLACEMENT_3D ( 'NONE', #55885, #66834, #8128 ) ;
#10685 = DIRECTION ( 'NONE',  ( 0.000000000000000000, 0.000000000000000000, -1.000000000000000000 ) ) ;
#10687 = DIRECTION ( 'NONE',  ( 0.000000000000000000, 1.000000000000000000, 0.000000000000000000 ) ) ;
#10686 = CARTESIAN_POINT ( 'NONE',  ( -6.500000000000002665, 6.500000000000002665, -1.000000000000000000 ) ) ;
#10688 = EDGE_LOOP ( 'NONE', ( #25559, #36257, #56461, #31130, #5368, #17904, #27748, #56006 ) ) ;
#10690 = EDGE_LOOP ( 'NONE', ( #26392, #41397, #3266, #60551 ) ) ;
#10689 = DIRECTION ( 'NONE',  ( 0.7142857142857395036, 0.000000000000000000, 0.6998542122237394469 ) ) ;
#10691 = VECTOR ( 'NONE', #23952, 1000.000000000000000 ) ;
#10692 = ORIENTED_EDGE ( 'NONE', *, *, #15102, .F. ) ;
#10693 = VERTEX_POINT ( 'NONE', #28534 ) ;
#10694 = LINE ( 'NONE', #54194, #7348 ) ;
#10695 = DIRECTION ( 'NONE',  ( -1.000000000000000000, 0.000000000000000000, 0.000000000000000000 ) ) ;
#10696 = CARTESIAN_POINT ( 'NONE',  ( -0.01515536117388802291, 11.99351654964718072, 16.17170636239079329 ) ) ;
#10697 = CIRCLE ( 'NONE', #28708, 1.000000000000000000 ) ;
#10699 = CARTESIAN_POINT ( 'NONE',  ( 30.00000000000000000, -14.33999999999999986, 14.50000000000000000 ) ) ;
#10698 = CIRCLE ( 'NONE', #26550, 0.5000000000009320322 ) ;
#10700 = EDGE_LOOP ( 'NONE', ( #53271, #26628, #43458, #65671 ) ) ;
#10701 = ORIENTED_EDGE ( 'NONE', *, *, #41865, .T. ) ;
#10702 = ORIENTED_EDGE ( 'NONE', *, *, #6165, .F. ) ;
#10703 = CARTESIAN_POINT ( 'NONE',  ( 10.09643294401454661, -9.106483450353492159, 455.0000000000000568 ) ) ;
#10704 = VECTOR ( 'NONE', #43455, 1000.000000000000000 ) ;
#10705 = EDGE_CURVE ( 'NONE', #14268, #8022, #66378, .T. ) ;
#10706 = DIRECTION ( 'NONE',  ( -1.000000000000000000, 0.000000000000000000, 0.000000000000000000 ) ) ;
#10707 = CARTESIAN_POINT ( 'NONE',  ( -11.33351654964671162, 1.077516549646603483, 195.0000000000000284 ) ) ;
#10708 = ORIENTED_EDGE ( 'NONE', *, *, #24528, .F. ) ;
#10709 = VERTEX_POINT ( 'NONE', #5942 ) ;
#10710 = FACE_OUTER_BOUND ( 'NONE', #57371, .T. ) ;
#10711 = AXIS2_PLACEMENT_3D ( 'NONE', #23622, #45183, #34579 ) ;
#10712 = ADVANCED_FACE ( 'NONE', ( #50103 ), #22553, .F. ) ;
#10713 = DIRECTION ( 'NONE',  ( 0.5773502691896257311, 0.5773502691896257311, -0.5773502691896257311 ) ) ;
#10714 = EDGE_LOOP ( 'NONE', ( #52251, #67966, #27681, #64199 ) ) ;
#10715 = VECTOR ( 'NONE', #62451, 1000.000000000000000 ) ;
#10716 = DIRECTION ( 'NONE',  ( -1.000000000000000000, 0.000000000000000000, 0.000000000000000000 ) ) ;
#10717 = ADVANCED_FACE ( 'NONE', ( #17232 ), #61048, .F. ) ;
#10719 = VERTEX_POINT ( 'NONE', #45845 ) ;
#10718 = DIRECTION ( 'NONE',  ( 0.000000000000000000, 3.673940397442059868E-16, -1.000000000000000000 ) ) ;
#10720 = CONICAL_SURFACE ( 'NONE', #56985, 3.233000000000000096, 0.7853981633974362886 ) ;
#10721 = ORIENTED_EDGE ( 'NONE', *, *, #39239, .F. ) ;
#10722 = DIRECTION ( 'NONE',  ( 8.673617379884087537E-15, 1.000000000000000000, 0.000000000000000000 ) ) ;
#10723 = CARTESIAN_POINT ( 'NONE',  ( -8.250000000000001776, -7.249999999999998224, -26.00000000000001066 ) ) ;
#10724 = DIRECTION ( 'NONE',  ( 0.000000000000000000, -1.000000000000000000, 0.000000000000000000 ) ) ;
#10725 = ADVANCED_FACE ( 'NONE', ( #7307 ), #26468, .F. ) ;
#10726 = DIRECTION ( 'NONE',  ( 0.000000000000000000, 3.673940397442059868E-16, -1.000000000000000000 ) ) ;
#10727 = LINE ( 'NONE', #43249, #35016 ) ;
#10728 = ORIENTED_EDGE ( 'NONE', *, *, #49200, .T. ) ;
#10729 = CARTESIAN_POINT ( 'NONE',  ( 25.50000000000000355, 0.000000000000000000, -22.50000000000000000 ) ) ;
#10730 = VERTEX_POINT ( 'NONE', #51861 ) ;
#10731 = CARTESIAN_POINT ( 'NONE',  ( -29.50000000000000355, -15.46862696659690073, 14.50000000000000000 ) ) ;
#10732 = DIRECTION ( 'NONE',  ( 0.000000000000000000, -0.7066873191084664940, 0.7075259945834416753 ) ) ;
#10733 = EDGE_CURVE ( 'NONE', #1298, #48685, #46538, .T. ) ;
#10734 = DIRECTION ( 'NONE',  ( 0.000000000000000000, 0.000000000000000000, 1.000000000000000000 ) ) ;
#10735 = CARTESIAN_POINT ( 'NONE',  ( 8.144523737882810366, 9.547976262117190416, 26.00000000000000711 ) ) ;
#10736 = DIRECTION ( 'NONE',  ( -1.000000000000000000, 0.000000000000000000, 0.000000000000000000 ) ) ;
#10737 = VECTOR ( 'NONE', #11105, 1000.000000000000000 ) ;
#10738 = ORIENTED_EDGE ( 'NONE', *, *, #34961, .F. ) ;
#10739 = EDGE_CURVE ( 'NONE', #14886, #58272, #67063, .T. ) ;
#10740 = DIRECTION ( 'NONE',  ( -1.000000000000000000, 0.000000000000000000, 0.000000000000000000 ) ) ;
#10741 = EDGE_CURVE ( 'NONE', #24680, #50893, #13670, .T. ) ;
#10742 = AXIS2_PLACEMENT_3D ( 'NONE', #51245, #7761, #14481 ) ;
#10743 = VECTOR ( 'NONE', #38864, 1000.000000000000000 ) ;
#10744 = ORIENTED_EDGE ( 'NONE', *, *, #45734, .T. ) ;
#10745 = FACE_OUTER_BOUND ( 'NONE', #47529, .T. ) ;
#10746 = DIRECTION ( 'NONE',  ( -0.000000000000000000, -0.000000000000000000, -1.000000000000000000 ) ) ;
#10747 = ORIENTED_EDGE ( 'NONE', *, *, #10662, .T. ) ;
#10748 = CARTESIAN_POINT ( 'NONE',  ( -7.593516549646711411, 11.77351654964660277, 455.0000000000000568 ) ) ;
#10749 = DIRECTION ( 'NONE',  ( 0.000000000000000000, -0.000000000000000000, 1.000000000000000000 ) ) ;
#10750 = VECTOR ( 'NONE', #4875, 1000.000000000000000 ) ;
#10751 = VERTEX_POINT ( 'NONE', #61761 ) ;
#10752 = DIRECTION ( 'NONE',  ( -1.836970198721029934E-16, 1.836970198721036590E-16, -1.000000000000000000 ) ) ;
#10753 = ADVANCED_FACE ( 'NONE', ( #39829 ), #29929, .F. ) ;
#10754 = CARTESIAN_POINT ( 'NONE',  ( 38.90000000000000568, -0.2000000000089119934, 8.909539772616881237E-12 ) ) ;
#10755 = AXIS2_PLACEMENT_3D ( 'NONE', #31583, #26615, #25930 ) ;
#10756 = DIRECTION ( 'NONE',  ( -0.000000000000000000, 3.673940397442059868E-16, -1.000000000000000000 ) ) ;
#10757 = EDGE_LOOP ( 'NONE', ( #44146, #28883, #64648, #58472 ) ) ;
#10759 = ORIENTED_EDGE ( 'NONE', *, *, #36646, .F. ) ;
#10758 = DIRECTION ( 'NONE',  ( 0.000000000000000000, 0.000000000000000000, 1.000000000000000000 ) ) ;
#10760 = COLOUR_RGB ( '', 0.31764706, 0.68627451, 0.89019608) ;
#10761 = DIRECTION ( 'NONE',  ( -1.836970198721029934E-16, 1.836970198721036344E-16, -1.000000000000000000 ) ) ;
#10762 = FACE_OUTER_BOUND ( 'NONE', #31458, .T. ) ;
#10763 = CARTESIAN_POINT ( 'NONE',  ( 6.836383711242975281, 4.135079735113102117, 54.00000000000000711 ) ) ;
#10764 = ORIENTED_EDGE ( 'NONE', *, *, #30831, .T. ) ;
#10765 =( GEOMETRIC_REPRESENTATION_CONTEXT ( 3 ) GLOBAL_UNCERTAINTY_ASSIGNED_CONTEXT ( ( #47238 ) ) GLOBAL_UNIT_ASSIGNED_CONTEXT ( ( #41232, #62440, #35943 ) ) REPRESENTATION_CONTEXT ( 'NONE', 'WORKASPACE' ) );
#10766 = CARTESIAN_POINT ( 'NONE',  ( 25.50000000000000355, -5.578999999999999737, -24.12099999999999866 ) ) ;
#10767 = LINE ( 'NONE', #59904, #13816 ) ;
#10768 = ORIENTED_EDGE ( 'NONE', *, *, #62259, .T. ) ;
#10769 = VERTEX_POINT ( 'NONE', #19663 ) ;
#10770 = ADVANCED_FACE ( 'NONE', ( #18619 ), #28875, .F. ) ;
#10771 = ORIENTED_EDGE ( 'NONE', *, *, #7064, .T. ) ;
#10772 = DIRECTION ( 'NONE',  ( 0.000000000000000000, 0.000000000000000000, 1.000000000000000000 ) ) ;
#10773 = EDGE_CURVE ( 'NONE', #13118, #9808, #19322, .T. ) ;
#10774 = DIRECTION ( 'NONE',  ( -1.000000000000000000, 0.000000000000000000, 0.000000000000000000 ) ) ;
#10775 = VERTEX_POINT ( 'NONE', #34174 ) ;
#10776 = VERTEX_POINT ( 'NONE', #29220 ) ;
#10777 = ADVANCED_FACE ( 'NONE', ( #67431 ), #7662, .F. ) ;
#10778 = FACE_OUTER_BOUND ( 'NONE', #53669, .T. ) ;
#10779 = VERTEX_POINT ( 'NONE', #2021 ) ;
#10780 = EDGE_CURVE ( 'NONE', #13545, #38341, #24642, .T. ) ;
#10781 = CIRCLE ( 'NONE', #31146, 0.4999999999979843901 ) ;
#10782 = EDGE_LOOP ( 'NONE', ( #38869, #34834, #58546, #50138 ) ) ;
#10783 = VERTEX_POINT ( 'NONE', #45136 ) ;
#10784 = ORIENTED_EDGE ( 'NONE', *, *, #8487, .F. ) ;
#10785 = VECTOR ( 'NONE', #52949, 1000.000000000000000 ) ;
#10786 = CARTESIAN_POINT ( 'NONE',  ( 11.00000000000000000, -9.200000000000120082, 17.30000000000000071 ) ) ;
#10787 = ADVANCED_FACE ( 'NONE', ( #13321 ), #12958, .T. ) ;
#10789 = ORIENTED_EDGE ( 'NONE', *, *, #33995, .F. ) ;
#10788 = DIRECTION ( 'NONE',  ( -0.000000000000000000, -0.000000000000000000, -1.000000000000000000 ) ) ;
#10790 = DIRECTION ( 'NONE',  ( 2.312964634635740689E-15, 1.000000000000000000, 0.000000000000000000 ) ) ;
#10791 = VECTOR ( 'NONE', #55743, 1000.000000000000000 ) ;
#10792 = AXIS2_PLACEMENT_3D ( 'NONE', #55436, #33516, #66387 ) ;
#10793 = VECTOR ( 'NONE', #50083, 1000.000000000000114 ) ;
#10794 = DIRECTION ( 'NONE',  ( -0.000000000000000000, -0.000000000000000000, 1.000000000000000000 ) ) ;
#10795 = CARTESIAN_POINT ( 'NONE',  ( 283.0000000000000568, -25.00000000000000000, -17.50000000000000000 ) ) ;
#10796 = EDGE_CURVE ( 'NONE', #55278, #37989, #8004, .T. ) ;
#10797 = ORIENTED_EDGE ( 'NONE', *, *, #1650, .T. ) ;
#10798 = EDGE_CURVE ( 'NONE', #15964, #52649, #24285, .T. ) ;
#10799 = VECTOR ( 'NONE', #42334, 1000.000000000000000 ) ;
#10800 = VECTOR ( 'NONE', #40682, 1000.000000000000114 ) ;
#10801 = EDGE_CURVE ( 'NONE', #39506, #3304, #56451, .T. ) ;
#10802 = EDGE_CURVE ( 'NONE', #33525, #22414, #40537, .T. ) ;
#10803 = CYLINDRICAL_SURFACE ( 'NONE', #16511, 0.4000000000000010214 ) ;
#10804 = CIRCLE ( 'NONE', #58255, 0.4000000000000609179 ) ;
#10805 = CARTESIAN_POINT ( 'NONE',  ( -25.50000000000000355, -5.578999999999999737, -22.50000000000000000 ) ) ;
#10806 = VERTEX_POINT ( 'NONE', #67762 ) ;
#10807 = CARTESIAN_POINT ( 'NONE',  ( 9.804883450353379715, -10.20488345035352928, 455.0000000000000568 ) ) ;
#10808 = EDGE_CURVE ( 'NONE', #15214, #54732, #40886, .T. ) ;
#10809 = STYLED_ITEM ( 'NONE', ( #42055 ), #44878 ) ;
#10810 = DIRECTION ( 'NONE',  ( -0.000000000000000000, 3.673940397442059868E-16, -1.000000000000000000 ) ) ;
#10811 = CARTESIAN_POINT ( 'NONE',  ( -6.486996718459903555, -2.632023737882784431, 54.00000000000000711 ) ) ;
#10812 = ORIENTED_EDGE ( 'NONE', *, *, #44084, .F. ) ;
#10813 = AXIS2_PLACEMENT_3D ( 'NONE', #67527, #23672, #61144 ) ;
#10814 = DIRECTION ( 'NONE',  ( 0.000000000000000000, -0.000000000000000000, 1.000000000000000000 ) ) ;
#10815 = CARTESIAN_POINT ( 'NONE',  ( 22.90000000000000213, -0.1999999999911795112, 8.826273045769999343E-12 ) ) ;
#10816 = LINE ( 'NONE', #16124, #2064 ) ;
#10817 = DIRECTION ( 'NONE',  ( -0.000000000000000000, -0.000000000000000000, -1.000000000000000000 ) ) ;
#10818 = DIRECTION ( 'NONE',  ( 9.799566706031580591E-15, 1.000000000000000000, 1.836970198721018348E-16 ) ) ;
#10819 = DIRECTION ( 'NONE',  ( 1.000000000000000000, -3.491481338843133355E-15, -1.836970198721036344E-16 ) ) ;
#10820 = EDGE_CURVE ( 'NONE', #36321, #19554, #14381, .T. ) ;
#10821 = LINE ( 'NONE', #20733, #56981 ) ;
#10822 = LINE ( 'NONE', #36652, #39053 ) ;
#10823 = EDGE_CURVE ( 'NONE', #16848, #44232, #25415, .T. ) ;
#10824 = ORIENTED_EDGE ( 'NONE', *, *, #3970, .T. ) ;
#10825 = PLANE ( 'NONE',  #4463 ) ;
#10826 = AXIS2_PLACEMENT_3D ( 'NONE', #37005, #20375, #20720 ) ;
#10827 = CARTESIAN_POINT ( 'NONE',  ( 17.51999999999999957, -15.50000000000000000, 26.00000000000000355 ) ) ;
#10828 = DIRECTION ( 'NONE',  ( -0.000000000000000000, -0.000000000000000000, -1.000000000000000000 ) ) ;
#10829 = LINE ( 'NONE', #43346, #63530 ) ;
#10830 = ORIENTED_EDGE ( 'NONE', *, *, #36927, .T. ) ;
#10831 = CARTESIAN_POINT ( 'NONE',  ( 10.05377373788278739, -8.930623737882855906, 54.00000000000000711 ) ) ;
#10832 = CARTESIAN_POINT ( 'NONE',  ( 31.89999999999999858, -0.000000000000000000, 20.80000000000000426 ) ) ;
#10833 = VECTOR ( 'NONE', #10497, 1000.000000000000000 ) ;
#10834 = DIRECTION ( 'NONE',  ( 1.000000000000000000, 0.000000000000000000, 0.000000000000000000 ) ) ;
#10835 = CARTESIAN_POINT ( 'NONE',  ( 8.250000000000005329, 7.250000000000000888, -10.50000000000000000 ) ) ;
#10836 = VECTOR ( 'NONE', #34462, 1000.000000000000000 ) ;
#10837 = DIRECTION ( 'NONE',  ( 0.000000000000000000, 1.000000000000000000, 0.000000000000000000 ) ) ;
#10838 = CARTESIAN_POINT ( 'NONE',  ( 30.00000000000000000, -15.46862696659690073, -14.50000000000000000 ) ) ;
#10839 = ORIENTED_EDGE ( 'NONE', *, *, #11353, .F. ) ;
#10840 = AXIS2_PLACEMENT_3D ( 'NONE', #28021, #11739, #45298 ) ;
#10841 = VECTOR ( 'NONE', #67441, 1000.000000000000000 ) ;
#10842 = VECTOR ( 'NONE', #66863, 1000.000000000000000 ) ;
#10843 = ORIENTED_EDGE ( 'NONE', *, *, #14921, .F. ) ;
#10844 = DIRECTION ( 'NONE',  ( -1.836970198721029934E-16, 1.836970198721036344E-16, -1.000000000000000000 ) ) ;
#10845 = FACE_OUTER_BOUND ( 'NONE', #6283, .T. ) ;
#10846 = ORIENTED_EDGE ( 'NONE', *, *, #9785, .F. ) ;
#10847 = CYLINDRICAL_SURFACE ( 'NONE', #21299, 0.1999999999999996503 ) ;
#10848 = VECTOR ( 'NONE', #38713, 1000.000000000000000 ) ;
#10849 = VECTOR ( 'NONE', #45275, 1000.000000000000000 ) ;
#10850 = AXIS2_PLACEMENT_3D ( 'NONE', #24689, #28936, #28587 ) ;
#10851 = PLANE ( 'NONE',  #30681 ) ;
#10852 = VERTEX_POINT ( 'NONE', #9421 ) ;
#10853 = AXIS2_PLACEMENT_3D ( 'NONE', #30191, #66617, #40075 ) ;
#10854 = CARTESIAN_POINT ( 'NONE',  ( -15.50000000000000000, -1.037157890325000054, -26.50000000000000000 ) ) ;
#10855 = VERTEX_POINT ( 'NONE', #4479 ) ;
#10856 = ORIENTED_EDGE ( 'NONE', *, *, #61496, .F. ) ;
#10857 = DIRECTION ( 'NONE',  ( 0.000000000000000000, -0.9938079899998859545, 0.1111111111112941946 ) ) ;
#10858 = ORIENTED_EDGE ( 'NONE', *, *, #42880, .F. ) ;
#10859 = DIRECTION ( 'NONE',  ( 0.000000000000000000, 1.000000000000000000, 0.000000000000000000 ) ) ;
#10860 = EDGE_CURVE ( 'NONE', #66251, #32707, #52528, .T. ) ;
#10861 = DIRECTION ( 'NONE',  ( 1.000000000000000000, -3.491481338843133355E-15, -1.836970198721036590E-16 ) ) ;
#10862 = DIRECTION ( 'NONE',  ( 0.000000000000000000, 0.000000000000000000, -1.000000000000000000 ) ) ;
#10863 = CIRCLE ( 'NONE', #28914, 0.3999999999999993006 ) ;
#10864 = ORIENTED_EDGE ( 'NONE', *, *, #41442, .T. ) ;
#10865 = ORIENTED_EDGE ( 'NONE', *, *, #16767, .T. ) ;
#10866 = VECTOR ( 'NONE', #3870, 1000.000000000000000 ) ;
#10867 = EDGE_CURVE ( 'NONE', #40219, #24424, #31071, .T. ) ;
#10868 = LINE ( 'NONE', #32780, #43667 ) ;
#10870 = DIRECTION ( 'NONE',  ( -1.000000000000000000, 0.000000000000000000, 0.000000000000000000 ) ) ;
#10869 = CARTESIAN_POINT ( 'NONE',  ( -7.744988412222897800, -8.465062094116051483, 195.0000000000000284 ) ) ;
#10871 = EDGE_LOOP ( 'NONE', ( #17376, #64731, #15028, #3104, #69163, #19201, #23693, #42706 ) ) ;
#10872 = EDGE_CURVE ( 'NONE', #354, #39516, #49143, .T. ) ;
#10873 = ORIENTED_EDGE ( 'NONE', *, *, #57423, .T. ) ;
#10874 = EDGE_CURVE ( 'NONE', #48603, #3647, #16956, .T. ) ;
#10876 = ORIENTED_EDGE ( 'NONE', *, *, #38863, .F. ) ;
#10875 = APPLICATION_PROTOCOL_DEFINITION ( 'draft international standard', 'automotive_design', 1998, #41764 ) ;
#10877 = EDGE_CURVE ( 'NONE', #12501, #56941, #36291, .T. ) ;
#10878 = EDGE_CURVE ( 'NONE', #62127, #15601, #27160, .T. ) ;
#10879 = CARTESIAN_POINT ( 'NONE',  ( -7.593516549646711411, 11.77351654964660277, 455.0000000000000568 ) ) ;
#10881 = ORIENTED_EDGE ( 'NONE', *, *, #5070, .T. ) ;
#10880 = DIRECTION ( 'NONE',  ( -1.000000000000000000, 0.000000000000000000, 0.000000000000000000 ) ) ;
#10882 = DIRECTION ( 'NONE',  ( 3.540573132209560831E-15, 1.000000000000000000, 0.000000000000000000 ) ) ;
#10883 = DIRECTION ( 'NONE',  ( 0.000000000000000000, 0.000000000000000000, -1.000000000000000000 ) ) ;
#10884 = EDGE_LOOP ( 'NONE', ( #43916, #69405, #52532, #22424 ) ) ;
#10885 = VECTOR ( 'NONE', #21700, 1000.000000000000000 ) ;
#10886 = ORIENTED_EDGE ( 'NONE', *, *, #49405, .T. ) ;
#10887 = CARTESIAN_POINT ( 'NONE',  ( 8.093267424590464998, -8.711985858128690197, 26.00000000000000000 ) ) ;
#10888 = VECTOR ( 'NONE', #21727, 1000.000000000000000 ) ;
#10889 = ORIENTED_EDGE ( 'NONE', *, *, #60917, .T. ) ;
#10890 = CARTESIAN_POINT ( 'NONE',  ( -0.9414762621172249046, 9.915476262117151052, 26.00000000000000711 ) ) ;
#10891 = CARTESIAN_POINT ( 'NONE',  ( -11.11351654964679270, -7.806483450353373321, 455.0000000000000568 ) ) ;
#10892 = VECTOR ( 'NONE', #44884, 1000.000000000000000 ) ;
#10893 = VECTOR ( 'NONE', #51314, 1000.000000000000114 ) ;
#10894 = EDGE_LOOP ( 'NONE', ( #12623, #69695, #36653, #7245 ) ) ;
#10895 = AXIS2_PLACEMENT_3D ( 'NONE', #50573, #55529, #61505 ) ;
#10896 = AXIS2_PLACEMENT_3D ( 'NONE', #65076, #38210, #64041 ) ;
#10897 = DIRECTION ( 'NONE',  ( -0.7071067811865451302, 0.7071067811865500152, 2.597868168706484541E-16 ) ) ;
#10898 = DIRECTION ( 'NONE',  ( 2.309061475090597584E-14, 1.000000000000000000, 1.836970198721053107E-16 ) ) ;
#10900 = EDGE_LOOP ( 'NONE', ( #5598, #65875, #65025, #8087 ) ) ;
#10899 = FILL_AREA_STYLE ('',( #58302 ) ) ;
#10901 = ORIENTED_EDGE ( 'NONE', *, *, #5072, .F. ) ;
#10902 = DIRECTION ( 'NONE',  ( -1.000000000000000000, 0.000000000000000000, 0.000000000000000000 ) ) ;
#10903 = CIRCLE ( 'NONE', #39107, 0.3999999999999993006 ) ;
#10904 = AXIS2_PLACEMENT_3D ( 'NONE', #28165, #53666, #32448 ) ;
#10905 = DIRECTION ( 'NONE',  ( -1.836970198721029934E-16, -1.836970198721010706E-16, 1.000000000000000000 ) ) ;
#10906 = LINE ( 'NONE', #49077, #44918 ) ;
#10907 = CARTESIAN_POINT ( 'NONE',  ( 8.900000000000002132, 0.000000000000000000, 0.000000000000000000 ) ) ;
#10908 = AXIS2_PLACEMENT_3D ( 'NONE', #22628, #33235, #45214 ) ;
#10909 = CARTESIAN_POINT ( 'NONE',  ( 290.0000000000000000, -21.00000000000000000, 0.000000000000000000 ) ) ;
#10910 = ORIENTED_EDGE ( 'NONE', *, *, #4902, .T. ) ;
#10911 = PLANE ( 'NONE',  #27899 ) ;
#10912 = LINE ( 'NONE', #63264, #32743 ) ;
#10913 = CARTESIAN_POINT ( 'NONE',  ( 8.406483450353379183, -5.668387132716048882, 455.0000000000000568 ) ) ;
#10915 = ORIENTED_EDGE ( 'NONE', *, *, #26015, .T. ) ;
#10914 = CARTESIAN_POINT ( 'NONE',  ( 9.247904806590725002, 9.942044687070426434, 455.0000000000000568 ) ) ;
#10916 = ADVANCED_FACE ( 'NONE', ( #10124 ), #41947, .F. ) ;
#10917 = AXIS2_PLACEMENT_3D ( 'NONE', #39999, #29064, #30461 ) ;
#10918 = LINE ( 'NONE', #43426, #22296 ) ;
#10919 = CARTESIAN_POINT ( 'NONE',  ( -10.08346604330797547, -9.306483450353381315, 455.0000000000000568 ) ) ;
#10920 = EDGE_CURVE ( 'NONE', #16796, #3052, #17457, .T. ) ;
#10921 = FACE_BOUND ( 'NONE', #21806, .T. ) ;
#10922 = CARTESIAN_POINT ( 'NONE',  ( 174.0064834503533575, -29.01119750012555443, 5.000000000000000000 ) ) ;
#10923 = ORIENTED_EDGE ( 'NONE', *, *, #35671, .T. ) ;
#10924 = CARTESIAN_POINT ( 'NONE',  ( -24.00000000000000000, -15.50000000000000000, 19.33772233983200195 ) ) ;
#10925 = CARTESIAN_POINT ( 'NONE',  ( -9.690000000000001279, -9.750000000000001776, -7.000000000000000000 ) ) ;
#10926 = VERTEX_POINT ( 'NONE', #52201 ) ;
#10927 = LINE ( 'NONE', #10574, #68402 ) ;
#10928 = CARTESIAN_POINT ( 'NONE',  ( -6.642976262117329611, -10.31452373788278365, 26.00000000000000000 ) ) ;
#10929 = CARTESIAN_POINT ( 'NONE',  ( 9.690000000000001279, 10.50000000000000000, 0.000000000000000000 ) ) ;
#10930 = CARTESIAN_POINT ( 'NONE',  ( 40.90000000000000568, -14.06939075806900163, -20.80000000000000426 ) ) ;
#10931 = CYLINDRICAL_SURFACE ( 'NONE', #48819, 4.500000000000188294 ) ;
#10932 = ORIENTED_EDGE ( 'NONE', *, *, #57568, .F. ) ;
#10933 = ORIENTED_EDGE ( 'NONE', *, *, #41463, .T. ) ;
#10934 = CARTESIAN_POINT ( 'NONE',  ( 0.000000000000000000, -0.7500000000000000000, 0.000000000000000000 ) ) ;
#10935 = ORIENTED_EDGE ( 'NONE', *, *, #19740, .F. ) ;
#10936 = AXIS2_PLACEMENT_3D ( 'NONE', #64076, #20912, #8900 ) ;
#10937 = ORIENTED_EDGE ( 'NONE', *, *, #26223, .T. ) ;
#10938 = DIRECTION ( 'NONE',  ( 1.000000000000000000, -0.000000000000000000, -0.000000000000000000 ) ) ;
#10939 = AXIS2_PLACEMENT_3D ( 'NONE', #46185, #68108, #24279 ) ;
#10940 = CARTESIAN_POINT ( 'NONE',  ( 49.00000000000000000, -0.2000000000089119934, -8.913009219568841313E-12 ) ) ;
#10941 = VECTOR ( 'NONE', #9168, 1000.000000000000000 ) ;
#10942 = VECTOR ( 'NONE', #11564, 1000.000000000000000 ) ;
#10943 = CARTESIAN_POINT ( 'NONE',  ( -9.234937905884020637, 9.942044687070460185, 455.0000000000000568 ) ) ;
#10944 = VERTEX_POINT ( 'NONE', #3763 ) ;
#10945 = ORIENTED_EDGE ( 'NONE', *, *, #53930, .F. ) ;
#10946 = CARTESIAN_POINT ( 'NONE',  ( 46.39999999999999858, 33.00000000000000000, 2.750000000000000444 ) ) ;
#10947 = VERTEX_POINT ( 'NONE', #31364 ) ;
#10948 = ORIENTED_EDGE ( 'NONE', *, *, #51853, .F. ) ;
#10949 = VECTOR ( 'NONE', #18920, 1000.000000000000000 ) ;
#10950 = ADVANCED_FACE ( 'NONE', ( #26044 ), #25335, .T. ) ;
#10951 = VECTOR ( 'NONE', #27243, 1000.000000000000227 ) ;
#10952 = CARTESIAN_POINT ( 'NONE',  ( 41.09999999999999432, -14.06939075806901940, -20.80000000000000426 ) ) ;
#10953 = DIRECTION ( 'NONE',  ( 1.000000000000000000, -0.000000000000000000, -0.000000000000000000 ) ) ;
#10954 = CARTESIAN_POINT ( 'NONE',  ( 3.157023737882797665, 4.031976262117209053, 54.00000000000000711 ) ) ;
#10955 = VERTEX_POINT ( 'NONE', #4822 ) ;
#10956 = CARTESIAN_POINT ( 'NONE',  ( 39.90000000000000568, 6.123233995736766282E-16, -5.000000000000000000 ) ) ;
#10957 = VECTOR ( 'NONE', #17205, 1000.000000000000000 ) ;
#10959 = CARTESIAN_POINT ( 'NONE',  ( 30.00000000000000000, -17.35230188589299871, -15.35019951917099945 ) ) ;
#10958 = DIRECTION ( 'NONE',  ( 1.000000000000000000, 0.000000000000000000, 0.000000000000000000 ) ) ;
#10960 = ORIENTED_EDGE ( 'NONE', *, *, #47939, .T. ) ;
#10961 = ORIENTED_EDGE ( 'NONE', *, *, #67549, .T. ) ;
#10963 = EDGE_LOOP ( 'NONE', ( #68723, #60655, #49210, #24241 ) ) ;
#10962 = DIRECTION ( 'NONE',  ( 0.000000000000000000, 1.000000000000000000, 0.000000000000000000 ) ) ;
#10964 = EDGE_CURVE ( 'NONE', #46013, #57327, #38910, .T. ) ;
#10965 = VERTEX_POINT ( 'NONE', #68473 ) ;
#10966 = ADVANCED_FACE ( 'NONE', ( #26387 ), #42289, .F. ) ;
#10967 = VECTOR ( 'NONE', #63599, 1000.000000000000114 ) ;
#10968 = EDGE_CURVE ( 'NONE', #60323, #9139, #18498, .T. ) ;
#10969 = EDGE_CURVE ( 'NONE', #30449, #6262, #29871, .T. ) ;
#10970 = DIRECTION ( 'NONE',  ( 0.000000000000000000, 0.000000000000000000, -1.000000000000000000 ) ) ;
#10971 = VECTOR ( 'NONE', #54737, 1000.000000000000000 ) ;
#10972 = CARTESIAN_POINT ( 'NONE',  ( 176.4833316329832940, -10.00000000000000178, 282.8454385697650082 ) ) ;
#10973 = EDGE_CURVE ( 'NONE', #48678, #54850, #8409, .T. ) ;
#10974 = ORIENTED_EDGE ( 'NONE', *, *, #42333, .F. ) ;
#10975 = VERTEX_POINT ( 'NONE', #29123 ) ;
#10976 = CARTESIAN_POINT ( 'NONE',  ( -7.839518282750262301, 3.417780618358531530, 455.0000000000000568 ) ) ;
#10977 = LINE ( 'NONE', #32553, #54926 ) ;
#10978 = ORIENTED_EDGE ( 'NONE', *, *, #56602, .F. ) ;
#10979 = ORIENTED_EDGE ( 'NONE', *, *, #44899, .F. ) ;
#10980 = CARTESIAN_POINT ( 'NONE',  ( 7.000000000000000000, -23.65000000000000568, 12.40000000000000213 ) ) ;
#10981 = CARTESIAN_POINT ( 'NONE',  ( -17.00000000000000000, -15.50000000000000000, -14.50000000000000000 ) ) ;
#10982 = DIRECTION ( 'NONE',  ( 1.000000000000000000, 0.000000000000000000, 0.000000000000000000 ) ) ;
#10983 = VERTEX_POINT ( 'NONE', #19553 ) ;
#10984 = DIRECTION ( 'NONE',  ( 0.5773502691896258421, -0.5773502691896257311, -0.5773502691896257311 ) ) ;
#10985 = DIRECTION ( 'NONE',  ( -0.000000000000000000, -1.000000000000000000, -0.000000000000000000 ) ) ;
#10986 = AXIS2_PLACEMENT_3D ( 'NONE', #68218, #30035, #51961 ) ;
#10988 = VERTEX_POINT ( 'NONE', #67653 ) ;
#10987 = LINE ( 'NONE', #32564, #48748 ) ;
#10990 = ORIENTED_EDGE ( 'NONE', *, *, #6094, .F. ) ;
#10989 = LINE ( 'NONE', #380, #52699 ) ;
#10991 = PLANE ( 'NONE',  #11054 ) ;
#10992 = DIRECTION ( 'NONE',  ( 2.135044278125299371E-15, 1.000000000000000000, 0.000000000000000000 ) ) ;
#10993 = CARTESIAN_POINT ( 'NONE',  ( -30.00000000000000000, -9.199999999999999289, -12.34999999999989839 ) ) ;
#10994 = CARTESIAN_POINT ( 'NONE',  ( -5.242976262117259978, 5.242976262117182706, 54.00000000000000711 ) ) ;
#10995 = CARTESIAN_POINT ( 'NONE',  ( -13.00000000000000178, -16.28999999999710369, -14.50000000000000000 ) ) ;
#10996 = AXIS2_PLACEMENT_3D ( 'NONE', #56462, #67071, #61057 ) ;
#10997 = AXIS2_PLACEMENT_3D ( 'NONE', #51857, #51144, #15075 ) ;
#10998 = DIRECTION ( 'NONE',  ( 1.000000000000000000, -0.000000000000000000, 0.000000000000000000 ) ) ;
#10999 = EDGE_LOOP ( 'NONE', ( #12335, #17292, #67496, #61988 ) ) ;
#11000 = CARTESIAN_POINT ( 'NONE',  ( 7.000000000000000000, -42.50000000000000000, -14.50000000000000000 ) ) ;
#11002 = ORIENTED_EDGE ( 'NONE', *, *, #7740, .T. ) ;
#11001 = LINE ( 'NONE', #11673, #37937 ) ;
#11003 = VECTOR ( 'NONE', #51352, 1000.000000000000000 ) ;
#11005 = VERTEX_POINT ( 'NONE', #13906 ) ;
#11004 = CARTESIAN_POINT ( 'NONE',  ( 0.000000000000000000, 0.000000000000000000, -29.90000000000000924 ) ) ;
#11006 = EDGE_CURVE ( 'NONE', #50458, #46020, #57391, .T. ) ;
#11007 = CARTESIAN_POINT ( 'NONE',  ( 3.157023737882819425, -4.046023737882825877, 54.00000000000000711 ) ) ;
#11008 = EDGE_CURVE ( 'NONE', #4595, #30792, #67040, .T. ) ;
#11009 = EDGE_CURVE ( 'NONE', #69932, #8602, #68136, .T. ) ;
#11010 = AXIS2_PLACEMENT_3D ( 'NONE', #54307, #44710, #66297 ) ;
#11011 = VECTOR ( 'NONE', #67561, 1000.000000000000000 ) ;
#11012 = EDGE_LOOP ( 'NONE', ( #65996, #24457, #61322, #62164 ) ) ;
#11013 = DIRECTION ( 'NONE',  ( -0.000000000000000000, 3.673940397442059868E-16, -1.000000000000000000 ) ) ;
#11014 = DIRECTION ( 'NONE',  ( 1.000000000000000000, -0.000000000000000000, -0.000000000000000000 ) ) ;
#11016 = ORIENTED_EDGE ( 'NONE', *, *, #59598, .F. ) ;
#11015 = ADVANCED_FACE ( 'NONE', ( #51036 ), #40781, .F. ) ;
#11017 = DIRECTION ( 'NONE',  ( 0.000000000000000000, 1.000000000000000000, 0.000000000000000000 ) ) ;
#11018 = CARTESIAN_POINT ( 'NONE',  ( -4.135079735113203370, -3.677663764522608236, 26.00000000000000711 ) ) ;
#11019 = CARTESIAN_POINT ( 'NONE',  ( 7.250000000000005329, -8.249999999999998224, -26.00000000000001066 ) ) ;
#11020 = VECTOR ( 'NONE', #15082, 1000.000000000000000 ) ;
#11021 = ORIENTED_EDGE ( 'NONE', *, *, #25663, .T. ) ;
#11022 = FACE_OUTER_BOUND ( 'NONE', #39130, .T. ) ;
#11023 = VERTEX_POINT ( 'NONE', #35822 ) ;
#11024 = ORIENTED_EDGE ( 'NONE', *, *, #6006, .F. ) ;
#11025 = CARTESIAN_POINT ( 'NONE',  ( -10.73351654964664981, -1.690483450353293948, 195.0000000000000284 ) ) ;
#11026 = LINE ( 'NONE', #779, #66984 ) ;
#11027 = DIRECTION ( 'NONE',  ( -0.6414496315691494699, 0.7671651518153064231, 0.000000000000000000 ) ) ;
#11028 = CARTESIAN_POINT ( 'NONE',  ( -25.50000000000000355, -5.200000000000001066, -20.24999999999999645 ) ) ;
#11029 = ORIENTED_EDGE ( 'NONE', *, *, #58341, .T. ) ;
#11030 = EDGE_LOOP ( 'NONE', ( #45869, #2636, #26206, #66511 ) ) ;
#11032 = VERTEX_POINT ( 'NONE', #23819 ) ;
#11031 = CARTESIAN_POINT ( 'NONE',  ( 30.00000000000000000, -17.14999999999999858, 27.00000000000000000 ) ) ;
#11033 = ORIENTED_EDGE ( 'NONE', *, *, #56025, .F. ) ;
#11034 = DIRECTION ( 'NONE',  ( 1.000000000000000000, 0.000000000000000000, 0.000000000000000000 ) ) ;
#11035 = DIRECTION ( 'NONE',  ( 0.000000000000000000, 0.000000000000000000, -1.000000000000000000 ) ) ;
#11036 = FACE_OUTER_BOUND ( 'NONE', #25111, .T. ) ;
#11037 = FACE_BOUND ( 'NONE', #27565, .T. ) ;
#11039 = LINE ( 'NONE', #63748, #63965 ) ;
#11038 = DIRECTION ( 'NONE',  ( -0.000000000000000000, -0.000000000000000000, -1.000000000000000000 ) ) ;
#11040 = VERTEX_POINT ( 'NONE', #19910 ) ;
#11042 = ORIENTED_EDGE ( 'NONE', *, *, #66476, .F. ) ;
#11041 = DIRECTION ( 'NONE',  ( 1.000000000000000000, 0.000000000000000000, 0.000000000000000000 ) ) ;
#11043 = ORIENTED_EDGE ( 'NONE', *, *, #42356, .T. ) ;
#11044 = EDGE_LOOP ( 'NONE', ( #33139, #29185, #43243, #17462 ) ) ;
#11045 = AXIS2_PLACEMENT_3D ( 'NONE', #38465, #64988, #28522 ) ;
#11046 = DIRECTION ( 'NONE',  ( 0.000000000000000000, 0.000000000000000000, 1.000000000000000000 ) ) ;
#11047 = CARTESIAN_POINT ( 'NONE',  ( 25.50000000000000355, 0.000000000000000000, 24.75000000000000000 ) ) ;
#11048 = ADVANCED_FACE ( 'NONE', ( #35110 ), #55718, .T. ) ;
#11049 = AXIS2_PLACEMENT_3D ( 'NONE', #13524, #18467, #56660 ) ;
#11050 = AXIS2_PLACEMENT_3D ( 'NONE', #25603, #47167, #47503 ) ;
#11051 = DIRECTION ( 'NONE',  ( 0.000000000000000000, 0.000000000000000000, -1.000000000000000000 ) ) ;
#11052 = EDGE_CURVE ( 'NONE', #36149, #1729, #7550, .T. ) ;
#11053 = ORIENTED_EDGE ( 'NONE', *, *, #23005, .T. ) ;
#11055 = EDGE_LOOP ( 'NONE', ( #904, #31758, #23118, #67179, #64780, #68908, #49165, #37648 ) ) ;
#11054 = AXIS2_PLACEMENT_3D ( 'NONE', #27262, #69703, #37521 ) ;
#11056 = EDGE_CURVE ( 'NONE', #39844, #35101, #52092, .T. ) ;
#11057 = VERTEX_POINT ( 'NONE', #68004 ) ;
#11058 = CARTESIAN_POINT ( 'NONE',  ( 14.50000000000000000, -0.5000000000000000000, 27.00000000000000000 ) ) ;
#11059 = VECTOR ( 'NONE', #49941, 1000.000000000000000 ) ;
#11060 = VECTOR ( 'NONE', #19708, 1000.000000000000000 ) ;
#11061 = DIRECTION ( 'NONE',  ( -1.000000000000000000, 0.000000000000000000, 0.000000000000000000 ) ) ;
#11062 = EDGE_CURVE ( 'NONE', #42883, #29241, #3783, .T. ) ;
#11063 = DIRECTION ( 'NONE',  ( -1.000000000000000000, -3.016910393003147986E-15, -0.000000000000000000 ) ) ;
#11065 = VERTEX_POINT ( 'NONE', #40059 ) ;
#11064 = PRODUCT_DEFINITION ( 'UNKNOWN', '', #50510, #7007 ) ;
#11066 = ORIENTED_EDGE ( 'NONE', *, *, #29356, .T. ) ;
#11067 = FACE_OUTER_BOUND ( 'NONE', #18579, .T. ) ;
#11068 = ADVANCED_FACE ( 'NONE', ( #62689 ), #46773, .F. ) ;
#11069 = CARTESIAN_POINT ( 'NONE',  ( 6.006483450353379716, -6.006483450353394815, 195.0000000000000284 ) ) ;
#11071 = ORIENTED_EDGE ( 'NONE', *, *, #2170, .F. ) ;
#11070 = ADVANCED_FACE ( 'NONE', ( #68358 ), #34767, .F. ) ;
#11072 = VECTOR ( 'NONE', #4053, 1000.000000000000000 ) ;
#11073 = CARTESIAN_POINT ( 'NONE',  ( 41.09999999999999432, -21.00000000000000000, -13.86939075806900057 ) ) ;
#11075 = EDGE_LOOP ( 'NONE', ( #64592, #53329, #43412, #53389, #40729, #3388 ) ) ;
#11074 = DIRECTION ( 'NONE',  ( -1.000000000000000000, 0.000000000000000000, 0.000000000000000000 ) ) ;
#11076 = VERTEX_POINT ( 'NONE', #63051 ) ;
#11077 = CARTESIAN_POINT ( 'NONE',  ( 289.5000000000000000, -42.50000000000000000, -26.50000000000000000 ) ) ;
#11078 = LINE ( 'NONE', #53525, #22156 ) ;
#11079 = DIRECTION ( 'NONE',  ( 0.000000000000000000, 0.000000000000000000, 1.000000000000000000 ) ) ;
#11080 = CARTESIAN_POINT ( 'NONE',  ( -7.250000000000001776, -7.249999999999998224, -18.50000000000000000 ) ) ;
#11081 = FACE_OUTER_BOUND ( 'NONE', #17674, .T. ) ;
#11082 = ORIENTED_EDGE ( 'NONE', *, *, #64107, .F. ) ;
#11083 = CARTESIAN_POINT ( 'NONE',  ( -7.250000000000000888, 8.250000000000001776, -12.50000000000000000 ) ) ;
#11084 = ORIENTED_EDGE ( 'NONE', *, *, #39431, .F. ) ;
#11085 = DIRECTION ( 'NONE',  ( 0.000000000000000000, 0.7046037717862339012, 0.7096009616570518874 ) ) ;
#11086 = LINE ( 'NONE', #17080, #30054 ) ;
#11087 = VECTOR ( 'NONE', #65790, 1000.000000000000000 ) ;
#11088 = DIRECTION ( 'NONE',  ( 1.000000000000000000, 0.000000000000000000, 0.000000000000000000 ) ) ;
#11089 = FACE_OUTER_BOUND ( 'NONE', #27635, .T. ) ;
#11090 = DIRECTION ( 'NONE',  ( -1.000000000000000000, 0.000000000000000000, 0.000000000000000000 ) ) ;
#11092 = ORIENTED_EDGE ( 'NONE', *, *, #8216, .F. ) ;
#11091 = EDGE_CURVE ( 'NONE', #55546, #40253, #29718, .T. ) ;
#11093 = DIRECTION ( 'NONE',  ( 0.000000000000000000, 0.000000000000000000, 1.000000000000000000 ) ) ;
#11094 = DIRECTION ( 'NONE',  ( 3.491481338843133355E-15, 1.000000000000000000, 1.836970198721029934E-16 ) ) ;
#11095 = AXIS2_PLACEMENT_3D ( 'NONE', #62227, #35339, #8477 ) ;
#11096 = ORIENTED_EDGE ( 'NONE', *, *, #3004, .T. ) ;
#11097 = DIRECTION ( 'NONE',  ( 1.920292680692490463E-14, 1.000000000000000000, 0.000000000000000000 ) ) ;
#11098 = CARTESIAN_POINT ( 'NONE',  ( 2.544523737882818271, 9.722976262117205337, 54.00000000000000711 ) ) ;
#11099 = ORIENTED_EDGE ( 'NONE', *, *, #24357, .F. ) ;
#11100 = CIRCLE ( 'NONE', #59661, 4.500000000000190958 ) ;
#11101 = DIRECTION ( 'NONE',  ( 1.000000000000000000, 0.000000000000000000, 0.000000000000000000 ) ) ;
#11102 = FACE_OUTER_BOUND ( 'NONE', #27352, .T. ) ;
#11104 = ORIENTED_EDGE ( 'NONE', *, *, #56578, .F. ) ;
#11103 = EDGE_CURVE ( 'NONE', #36169, #54230, #24167, .T. ) ;
#11105 = DIRECTION ( 'NONE',  ( 0.000000000000000000, -0.7096009616570518874, -0.7046037717862339012 ) ) ;
#11106 = CARTESIAN_POINT ( 'NONE',  ( 12.00648345035338060, -7.826483450353491023, 455.0000000000000568 ) ) ;
#11107 = CARTESIAN_POINT ( 'NONE',  ( -25.50000000000000355, -15.50000000000000000, 22.50000000000000000 ) ) ;
#11108 = EDGE_CURVE ( 'NONE', #6666, #18538, #48534, .T. ) ;
#11109 = DIRECTION ( 'NONE',  ( 0.000000000000000000, -0.1111111111108840643, -0.9938079899999319178 ) ) ;
#11110 = ORIENTED_EDGE ( 'NONE', *, *, #49906, .F. ) ;
#11112 = ORIENTED_EDGE ( 'NONE', *, *, #26146, .T. ) ;
#11111 = CARTESIAN_POINT ( 'NONE',  ( 0.000000000000000000, 61.65740854044500452, 0.000000000000000000 ) ) ;
#11113 = AXIS2_PLACEMENT_3D ( 'NONE', #15004, #52855, #41867 ) ;
#11114 = CARTESIAN_POINT ( 'NONE',  ( 8.250000000000005329, 7.250000000000000888, -9.500000000000001776 ) ) ;
#11115 = LINE ( 'NONE', #16428, #10888 ) ;
#11116 = DIRECTION ( 'NONE',  ( 0.000000000000000000, 0.000000000000000000, 1.000000000000000000 ) ) ;
#11117 = ORIENTED_EDGE ( 'NONE', *, *, #37017, .F. ) ;
#11118 = CARTESIAN_POINT ( 'NONE',  ( 30.00000000000000000, -5.200000000000001066, 9.400000000000000355 ) ) ;
#11119 = PLANE ( 'NONE',  #46560 ) ;
#11120 = ORIENTED_EDGE ( 'NONE', *, *, #57355, .F. ) ;
#11121 = ORIENTED_EDGE ( 'NONE', *, *, #18884, .T. ) ;
#11122 = ADVANCED_FACE ( 'NONE', ( #16353 ), #20605, .F. ) ;
#11123 = VERTEX_POINT ( 'NONE', #42527 ) ;
#11124 = LINE ( 'NONE', #38012, #26454 ) ;
#11125 = DIRECTION ( 'NONE',  ( 1.000000000000000000, 0.000000000000000000, 0.000000000000000000 ) ) ;
#11126 = EDGE_CURVE ( 'NONE', #11267, #19554, #58463, .T. ) ;
#11127 = ORIENTED_EDGE ( 'NONE', *, *, #28824, .T. ) ;
#11128 = EDGE_LOOP ( 'NONE', ( #16297, #37636, #28196, #33217 ) ) ;
#11129 = ORIENTED_EDGE ( 'NONE', *, *, #39997, .T. ) ;
#11130 = DIRECTION ( 'NONE',  ( -1.000000000000000000, 3.491481338843132961E-15, 0.000000000000000000 ) ) ;
#11131 = ORIENTED_EDGE ( 'NONE', *, *, #43886, .T. ) ;
#11132 = ADVANCED_FACE ( 'NONE', ( #64122 ), #63759, .F. ) ;
#11133 = ORIENTED_EDGE ( 'NONE', *, *, #57437, .F. ) ;
#11134 = ORIENTED_EDGE ( 'NONE', *, *, #51102, .F. ) ;
#11135 = ORIENTED_EDGE ( 'NONE', *, *, #36837, .T. ) ;
#11136 = CARTESIAN_POINT ( 'NONE',  ( -13.00000000000000178, -17.50000000000000000, -15.70500000000000007 ) ) ;
#11137 = UNCERTAINTY_MEASURE_WITH_UNIT (LENGTH_MEASURE( 1.000000000000000082E-05 ), #48189, 'distance_accuracy_value', 'NONE');
#11138 = EDGE_CURVE ( 'NONE', #17846, #23372, #31587, .T. ) ;
#11140 = VERTEX_POINT ( 'NONE', #30873 ) ;
#11139 = CARTESIAN_POINT ( 'NONE',  ( 8.250000000000005329, -7.249999999999998224, -21.00000000000000000 ) ) ;
#11141 = EDGE_CURVE ( 'NONE', #22435, #19590, #4707, .T. ) ;
#11142 = AXIS2_PLACEMENT_3D ( 'NONE', #43020, #62320, #8929 ) ;
#11143 = CARTESIAN_POINT ( 'NONE',  ( -7.250000000000000888, 7.250000000000001776, -24.50000000000000000 ) ) ;
#11144 = CARTESIAN_POINT ( 'NONE',  ( 0.000000000000000000, -7.449999999999998401, -11.00000000000000000 ) ) ;
#11145 = LINE ( 'NONE', #17839, #23409 ) ;
#11146 = VERTEX_POINT ( 'NONE', #37238 ) ;
#11147 = VECTOR ( 'NONE', #13588, 1000.000000000000000 ) ;
#11148 = EDGE_CURVE ( 'NONE', #61739, #59143, #47482, .T. ) ;
#11149 = DIRECTION ( 'NONE',  ( -1.000000000000000000, 0.000000000000000000, 0.000000000000000000 ) ) ;
#11150 = ORIENTED_EDGE ( 'NONE', *, *, #53046, .F. ) ;
#11151 = FACE_BOUND ( 'NONE', #55952, .T. ) ;
#11152 = AXIS2_PLACEMENT_3D ( 'NONE', #6303, #54746, #60729 ) ;
#11153 = FACE_OUTER_BOUND ( 'NONE', #1515, .T. ) ;
#11154 = CYLINDRICAL_SURFACE ( 'NONE', #57317, 0.5249999999999985789 ) ;
#11155 = EDGE_CURVE ( 'NONE', #38091, #37343, #26270, .T. ) ;
#11156 = ORIENTED_EDGE ( 'NONE', *, *, #5292, .F. ) ;
#11157 = CARTESIAN_POINT ( 'NONE',  ( -2.989207322240228226, -6.872275254348431339, 26.00000000000000711 ) ) ;
#11158 = CYLINDRICAL_SURFACE ( 'NONE', #30816, 2.500000000000000000 ) ;
#11159 = FACE_OUTER_BOUND ( 'NONE', #570, .T. ) ;
#11160 = EDGE_CURVE ( 'NONE', #1121, #18785, #64802, .T. ) ;
#11161 = DIRECTION ( 'NONE',  ( 0.000000000000000000, 0.000000000000000000, -1.000000000000000000 ) ) ;
#11162 = LINE ( 'NONE', #64235, #21203 ) ;
#11163 = CARTESIAN_POINT ( 'NONE',  ( -5.242976262117280406, -5.257023737882805747, 54.00000000000000711 ) ) ;
#11164 = ADVANCED_FACE ( 'NONE', ( #25934 ), #14963, .F. ) ;
#11165 = DIRECTION ( 'NONE',  ( 1.000000000000000000, -0.000000000000000000, 0.000000000000000000 ) ) ;
#11166 = ORIENTED_EDGE ( 'NONE', *, *, #57575, .F. ) ;
#11167 = FACE_OUTER_BOUND ( 'NONE', #19957, .T. ) ;
#11168 = DIRECTION ( 'NONE',  ( -0.000000000000000000, -0.000000000000000000, -1.000000000000000000 ) ) ;
#11169 = EDGE_CURVE ( 'NONE', #51101, #86, #21856, .T. ) ;
#11170 = DIRECTION ( 'NONE',  ( 0.000000000000000000, -1.000000000000000000, -0.000000000000000000 ) ) ;
#11171 = DIRECTION ( 'NONE',  ( 0.000000000000000000, 0.000000000000000000, 1.000000000000000000 ) ) ;
#11172 = VERTEX_POINT ( 'NONE', #69400 ) ;
#11173 = CARTESIAN_POINT ( 'NONE',  ( 8.250000000000005329, -7.249999999999998224, -19.00000000000000000 ) ) ;
#11174 = EDGE_CURVE ( 'NONE', #51421, #11793, #36522, .T. ) ;
#11175 = CARTESIAN_POINT ( 'NONE',  ( 10.20488345035338007, -11.08848345035339733, 195.0000000000000284 ) ) ;
#11176 = CARTESIAN_POINT ( 'NONE',  ( 0.9555237378827827754, -9.929523737882790968, 54.00000000000000711 ) ) ;
#11177 = CIRCLE ( 'NONE', #50691, 0.1999999999999987899 ) ;
#11178 = CARTESIAN_POINT ( 'NONE',  ( 41.09999999999999432, 14.08845687959340331, -21.00000000000000000 ) ) ;
#11179 = CARTESIAN_POINT ( 'NONE',  ( 41.09999999999999432, -21.00000000000000000, -13.86939075806900057 ) ) ;
#11180 = EDGE_CURVE ( 'NONE', #18662, #26875, #20959, .T. ) ;
#11181 = LINE ( 'NONE', #5890, #63346 ) ;
#11182 = ORIENTED_EDGE ( 'NONE', *, *, #2106, .F. ) ;
#11183 = CIRCLE ( 'NONE', #64252, 0.1999999999999987899 ) ;
#11184 = ORIENTED_EDGE ( 'NONE', *, *, #55372, .F. ) ;
#11185 = CARTESIAN_POINT ( 'NONE',  ( 30.00000000000000000, -12.00000000000000000, 12.20000000000000107 ) ) ;
#11186 = CARTESIAN_POINT ( 'NONE',  ( -9.781776262117318765, -10.50702373788275246, 26.00000000000000000 ) ) ;
#11188 = ORIENTED_EDGE ( 'NONE', *, *, #28106, .F. ) ;
#11187 = EDGE_CURVE ( 'NONE', #3626, #9916, #28606, .T. ) ;
#11189 = EDGE_CURVE ( 'NONE', #10241, #974, #5051, .T. ) ;
#11190 = AXIS2_PLACEMENT_3D ( 'NONE', #28716, #23064, #54572 ) ;
#11191 = DIRECTION ( 'NONE',  ( -1.000000000000000000, 0.000000000000000000, -0.000000000000000000 ) ) ;
#11192 = EDGE_CURVE ( 'NONE', #38308, #35023, #69764, .T. ) ;
#11193 = ORIENTED_EDGE ( 'NONE', *, *, #11909, .F. ) ;
#11194 = EDGE_CURVE ( 'NONE', #7925, #9482, #21318, .T. ) ;
#11195 = ADVANCED_FACE ( 'NONE', ( #53852 ), #44950, .F. ) ;
#11196 = CARTESIAN_POINT ( 'NONE',  ( -7.450000000000001954, -7.249999999999998224, -9.500000000000001776 ) ) ;
#11197 = ORIENTED_EDGE ( 'NONE', *, *, #44214, .F. ) ;
#11198 = ORIENTED_EDGE ( 'NONE', *, *, #7013, .F. ) ;
#11199 = DIRECTION ( 'NONE',  ( -0.000000000000000000, -0.000000000000000000, 1.000000000000000000 ) ) ;
#11200 = ORIENTED_EDGE ( 'NONE', *, *, #43061, .F. ) ;
#11201 = PLANE ( 'NONE',  #11690 ) ;
#11202 = EDGE_CURVE ( 'NONE', #61739, #53333, #8266, .T. ) ;
#11204 = AXIS2_PLACEMENT_3D ( 'NONE', #7296, #62433, #55750 ) ;
#11203 = CIRCLE ( 'NONE', #50713, 1.000000000000002665 ) ;
#11205 = FACE_OUTER_BOUND ( 'NONE', #34230, .T. ) ;
#11206 = CARTESIAN_POINT ( 'NONE',  ( 7.000000000000000000, -31.30000000000000071, -8.400000000000000355 ) ) ;
#11207 = EDGE_CURVE ( 'NONE', #12942, #32305, #38620, .T. ) ;
#11208 = ORIENTED_EDGE ( 'NONE', *, *, #26741, .T. ) ;
#11209 = EDGE_LOOP ( 'NONE', ( #38311, #66909, #61375, #69278 ) ) ;
#11210 = CARTESIAN_POINT ( 'NONE',  ( 7.250000000000005329, -7.449999999999998401, -24.50000000000000000 ) ) ;
#11211 = EDGE_CURVE ( 'NONE', #5469, #4613, #46686, .T. ) ;
#11213 = CARTESIAN_POINT ( 'NONE',  ( -11.00000000000000000, -16.28999999999710369, -15.00000000000794920 ) ) ;
#11212 = AXIS2_PLACEMENT_3D ( 'NONE', #3599, #9256, #25168 ) ;
#11214 = ORIENTED_EDGE ( 'NONE', *, *, #4368, .T. ) ;
#11215 = VERTEX_POINT ( 'NONE', #5755 ) ;
#11216 = ORIENTED_EDGE ( 'NONE', *, *, #6349, .F. ) ;
#11217 = LINE ( 'NONE', #35468, #17545 ) ;
#11218 = ADVANCED_FACE ( 'NONE', ( #59492 ), #37933, .F. ) ;
#11220 = EDGE_LOOP ( 'NONE', ( #22106, #105, #44082, #60312 ) ) ;
#11219 = CARTESIAN_POINT ( 'NONE',  ( 23.90000000000000213, 20.60000000000000142, -13.86939075806900057 ) ) ;
#11221 = EDGE_CURVE ( 'NONE', #56334, #53583, #65491, .T. ) ;
#11222 = DIRECTION ( 'NONE',  ( 0.000000000000000000, 0.000000000000000000, 1.000000000000000000 ) ) ;
#11223 = LINE ( 'NONE', #66359, #21578 ) ;
#11224 = VERTEX_POINT ( 'NONE', #17048 ) ;
#11225 = ORIENTED_EDGE ( 'NONE', *, *, #36667, .F. ) ;
#11226 = CYLINDRICAL_SURFACE ( 'NONE', #50453, 1.000000000000000000 ) ;
#11227 = EDGE_LOOP ( 'NONE', ( #43818, #52856, #51133, #48174, #47742, #64267, #41310, #20419 ) ) ;
#11228 = LINE ( 'NONE', #49426, #17792 ) ;
#11229 = DIRECTION ( 'NONE',  ( -0.000000000000000000, -0.000000000000000000, -1.000000000000000000 ) ) ;
#11230 = ORIENTED_EDGE ( 'NONE', *, *, #68183, .F. ) ;
#11231 = CIRCLE ( 'NONE', #24768, 0.2000000000000005107 ) ;
#11232 = CARTESIAN_POINT ( 'NONE',  ( 30.00000000000000000, -16.64230188589299786, 14.64519951917100116 ) ) ;
#11233 = ORIENTED_EDGE ( 'NONE', *, *, #39315, .F. ) ;
#11234 = ORIENTED_EDGE ( 'NONE', *, *, #66579, .T. ) ;
#11235 = DIRECTION ( 'NONE',  ( 0.000000000000000000, 0.000000000000000000, -1.000000000000000000 ) ) ;
#11236 = AXIS2_PLACEMENT_3D ( 'NONE', #2802, #51957, #35313 ) ;
#11237 = DIRECTION ( 'NONE',  ( 1.836970198721029934E-16, 1.836970198721010706E-16, -1.000000000000000000 ) ) ;
#11238 = CARTESIAN_POINT ( 'NONE',  ( 290.0000000000000000, -0.5000000000000000000, -26.50000000000000000 ) ) ;
#11239 = CARTESIAN_POINT ( 'NONE',  ( -4.734785091274032354, -5.393625297349961656, 455.0000000000000568 ) ) ;
#11240 = DIRECTION ( 'NONE',  ( 1.000000000000000000, -0.000000000000000000, 0.000000000000000000 ) ) ;
#11241 = ORIENTED_EDGE ( 'NONE', *, *, #30216, .T. ) ;
#11242 = CARTESIAN_POINT ( 'NONE',  ( 8.241237374594247100, 1.620245201994230611, 54.00000000000000711 ) ) ;
#11243 = CARTESIAN_POINT ( 'NONE',  ( -5.993516549646711766, 3.593516549646603497, 455.0000000000000568 ) ) ;
#11244 = LINE ( 'NONE', #69961, #45833 ) ;
#11245 = VECTOR ( 'NONE', #26319, 1000.000000000000000 ) ;
#11246 = EDGE_CURVE ( 'NONE', #29427, #62756, #22959, .T. ) ;
#11248 = ORIENTED_EDGE ( 'NONE', *, *, #26448, .T. ) ;
#11247 = DIRECTION ( 'NONE',  ( 1.000000000000000000, -5.981805089575194965E-17, 0.000000000000000000 ) ) ;
#11249 = CARTESIAN_POINT ( 'NONE',  ( 24.00000000000000000, -17.35230188589299871, -15.35019951917099945 ) ) ;
#11250 = CARTESIAN_POINT ( 'NONE',  ( 9.912023737882815766, -3.682023737882817116, 26.00000000000000711 ) ) ;
#11251 = CARTESIAN_POINT ( 'NONE',  ( -6.835476262117260227, 10.49297626211718359, 54.00000000000000711 ) ) ;
#11252 = EDGE_CURVE ( 'NONE', #27223, #41334, #1817, .T. ) ;
#11253 = AXIS2_PLACEMENT_3D ( 'NONE', #23842, #28787, #45399 ) ;
#11254 = DIRECTION ( 'NONE',  ( 0.000000000000000000, 1.000000000000000000, 0.000000000000000000 ) ) ;
#11255 = ORIENTED_EDGE ( 'NONE', *, *, #53137, .F. ) ;
#11256 = LINE ( 'NONE', #32499, #23048 ) ;
#11257 = ADVANCED_FACE ( 'NONE', ( #449 ), #28337, .T. ) ;
#11258 = DIRECTION ( 'NONE',  ( 0.000000000000000000, 0.7096009616570518874, -0.7046037717862339012 ) ) ;
#11259 = VERTEX_POINT ( 'NONE', #27321 ) ;
#11260 = DIRECTION ( 'NONE',  ( 1.000000000000000000, 0.000000000000000000, 0.000000000000000000 ) ) ;
#11261 = CARTESIAN_POINT ( 'NONE',  ( -9.791916549646712653, 11.07551654964660415, 455.0000000000000568 ) ) ;
#11262 = FACE_OUTER_BOUND ( 'NONE', #19134, .T. ) ;
#11263 = EDGE_CURVE ( 'NONE', #45628, #5787, #22010, .T. ) ;
#11264 = DIRECTION ( 'NONE',  ( -1.794541526872559352E-16, -1.000000000000000000, 0.000000000000000000 ) ) ;
#11265 = DIRECTION ( 'NONE',  ( -0.000000000000000000, -0.000000000000000000, 1.000000000000000000 ) ) ;
#11266 = ORIENTED_EDGE ( 'NONE', *, *, #5160, .T. ) ;
#11267 = VERTEX_POINT ( 'NONE', #54893 ) ;
#11268 = LINE ( 'NONE', #58685, #67928 ) ;
#11269 = AXIS2_PLACEMENT_3D ( 'NONE', #28854, #55742, #1997 ) ;
#11270 = ORIENTED_EDGE ( 'NONE', *, *, #3259, .T. ) ;
#11271 = DIRECTION ( 'NONE',  ( -8.359604446858500663E-15, -1.000000000000000000, 0.000000000000000000 ) ) ;
#11272 = ORIENTED_EDGE ( 'NONE', *, *, #26395, .T. ) ;
#11273 = CARTESIAN_POINT ( 'NONE',  ( -4.173516549646666185, 11.99351654964658920, 195.0000000000000284 ) ) ;
#11274 = EDGE_CURVE ( 'NONE', #30319, #27517, #65154, .T. ) ;
#11275 = DIRECTION ( 'NONE',  ( 8.673617379884051249E-15, 1.000000000000000000, 0.000000000000000000 ) ) ;
#11276 = DIRECTION ( 'NONE',  ( -0.000000000000000000, 3.673940397442059868E-16, -1.000000000000000000 ) ) ;
#11277 = ORIENTED_EDGE ( 'NONE', *, *, #19813, .F. ) ;
#11278 = ORIENTED_EDGE ( 'NONE', *, *, #30439, .T. ) ;
#11279 = PLANE ( 'NONE',  #2354 ) ;
#11280 = VECTOR ( 'NONE', #58163, 1000.000000000000000 ) ;
#11281 = VERTEX_POINT ( 'NONE', #27660 ) ;
#11282 = VECTOR ( 'NONE', #33118, 1000.000000000000000 ) ;
#11283 = ORIENTED_EDGE ( 'NONE', *, *, #58630, .F. ) ;
#11284 = DIRECTION ( 'NONE',  ( 1.000000000000000000, 0.000000000000000000, -0.000000000000000000 ) ) ;
#11285 = LINE ( 'NONE', #54439, #59520 ) ;
#11286 = LINE ( 'NONE', #5994, #1604 ) ;
#11287 = ORIENTED_EDGE ( 'NONE', *, *, #46598, .T. ) ;
#11288 = AXIS2_PLACEMENT_3D ( 'NONE', #16911, #28541, #32820 ) ;
#11289 = CARTESIAN_POINT ( 'NONE',  ( 9.795823737882805915, -10.50702373788282529, 54.00000000000000711 ) ) ;
#11291 = LINE ( 'NONE', #50158, #17502 ) ;
#11290 = CARTESIAN_POINT ( 'NONE',  ( 8.250000000000005329, 0.000000000000000000, -19.00000000000000000 ) ) ;
#11292 = VERTEX_POINT ( 'NONE', #49570 ) ;
#11293 = ORIENTED_EDGE ( 'NONE', *, *, #30706, .F. ) ;
#11295 = VERTEX_POINT ( 'NONE', #6096 ) ;
#11294 = CARTESIAN_POINT ( 'NONE',  ( -7.813516549646839948, -12.00648345035340903, 455.0000000000000568 ) ) ;
#11296 = ORIENTED_EDGE ( 'NONE', *, *, #45756, .F. ) ;
#11297 = VECTOR ( 'NONE', #7686, 1000.000000000000000 ) ;
#11299 = VECTOR ( 'NONE', #57753, 1000.000000000000000 ) ;
#11298 = CARTESIAN_POINT ( 'NONE',  ( -7.250000000000000888, 7.250000000000001776, -13.00000000000000178 ) ) ;
#11300 = EDGE_CURVE ( 'NONE', #2701, #9404, #48978, .T. ) ;
#11301 = VECTOR ( 'NONE', #12123, 1000.000000000000000 ) ;
#11302 = EDGE_CURVE ( 'NONE', #23844, #19581, #65864, .T. ) ;
#11303 = CARTESIAN_POINT ( 'NONE',  ( 25.50000000000000355, -15.12100000000000044, -20.87900000000000134 ) ) ;
#11304 = ORIENTED_EDGE ( 'NONE', *, *, #38372, .T. ) ;
#11306 = ORIENTED_EDGE ( 'NONE', *, *, #20699, .T. ) ;
#11305 = ADVANCED_FACE ( 'NONE', ( #23033 ), #38952, .F. ) ;
#11307 = CIRCLE ( 'NONE', #4567, 0.06000000000000102474 ) ;
#11308 = AXIS2_PLACEMENT_3D ( 'NONE', #26019, #30961, #68796 ) ;
#11309 = FACE_BOUND ( 'NONE', #39487, .T. ) ;
#11310 = CARTESIAN_POINT ( 'NONE',  ( 7.450000000000004619, -1.336933437520057563E-15, -12.50000000000000000 ) ) ;
#11311 = ORIENTED_EDGE ( 'NONE', *, *, #19173, .T. ) ;
#11312 = CARTESIAN_POINT ( 'NONE',  ( 41.09999999999999432, 13.66939075806899950, 20.80000000000000426 ) ) ;
#11313 = DIRECTION ( 'NONE',  ( 8.673617379884087537E-15, 1.000000000000000000, 0.000000000000000000 ) ) ;
#11314 = LINE ( 'NONE', #42458, #20372 ) ;
#11315 = EDGE_LOOP ( 'NONE', ( #45375, #57548, #2609, #32471, #55333, #48344, #5018, #27386 ) ) ;
#11316 = CARTESIAN_POINT ( 'NONE',  ( -11.19000000000000128, -12.00000000000000000, 0.000000000000000000 ) ) ;
#11317 = AXIS2_PLACEMENT_3D ( 'NONE', #68181, #25403, #8067 ) ;
#11318 = CARTESIAN_POINT ( 'NONE',  ( -9.390476262117260831, 0.9414762621171833823, 26.00000000000000711 ) ) ;
#11320 = EDGE_LOOP ( 'NONE', ( #64700, #27661, #34960, #24360 ) ) ;
#11319 = LINE ( 'NONE', #16983, #9227 ) ;
#11322 = ORIENTED_EDGE ( 'NONE', *, *, #66270, .F. ) ;
#11321 = DIRECTION ( 'NONE',  ( 0.000000000000000000, 3.673940397442059868E-16, -1.000000000000000000 ) ) ;
#11323 = DIRECTION ( 'NONE',  ( 0.000000000000000000, 1.000000000000000000, 0.000000000000000000 ) ) ;
#11324 = LINE ( 'NONE', #27593, #240 ) ;
#11325 = DIRECTION ( 'NONE',  ( 0.8660254037844401509, 0.4999999999999974465, 0.000000000000000000 ) ) ;
#11326 = FACE_OUTER_BOUND ( 'NONE', #34838, .T. ) ;
#11327 = CARTESIAN_POINT ( 'NONE',  ( 6.500000000000000888, -6.500000000000002665, -1.000000000000000000 ) ) ;
#11328 = VECTOR ( 'NONE', #56279, 1000.000000000000000 ) ;
#11329 = CARTESIAN_POINT ( 'NONE',  ( 29.50000000000000355, -12.00000000000000000, -11.00000000000000000 ) ) ;
#11330 = ORIENTED_EDGE ( 'NONE', *, *, #31150, .T. ) ;
#11331 = CARTESIAN_POINT ( 'NONE',  ( 7.852485183456924034, 3.417780618358489786, 455.0000000000000568 ) ) ;
#11332 = VECTOR ( 'NONE', #20886, 1000.000000000000000 ) ;
#11334 = ORIENTED_EDGE ( 'NONE', *, *, #30391, .T. ) ;
#11333 = CARTESIAN_POINT ( 'NONE',  ( 17.89999999999999858, 13.66939075806899240, 20.79999999999999361 ) ) ;
#11335 = EDGE_CURVE ( 'NONE', #33105, #57275, #55225, .T. ) ;
#11337 = ORIENTED_EDGE ( 'NONE', *, *, #7285, .T. ) ;
#11336 = DIRECTION ( 'NONE',  ( -1.000000000000000000, 0.000000000000000000, 0.000000000000000000 ) ) ;
#11338 = AXIS2_PLACEMENT_3D ( 'NONE', #50043, #44044, #578 ) ;
#11339 =( NAMED_UNIT ( * ) SI_UNIT ( $, .STERADIAN. ) SOLID_ANGLE_UNIT ( ) );
#11340 = LINE ( 'NONE', #37885, #49914 ) ;
#11342 = EDGE_CURVE ( 'NONE', #66149, #66609, #1507, .T. ) ;
#11341 = VECTOR ( 'NONE', #9795, 1000.000000000000000 ) ;
#11343 = ORIENTED_EDGE ( 'NONE', *, *, #59645, .F. ) ;
#11344 = DIRECTION ( 'NONE',  ( 0.000000000000000000, -1.000000000000000000, 0.000000000000000000 ) ) ;
#11345 = EDGE_CURVE ( 'NONE', #9620, #40700, #33982, .T. ) ;
#11346 = LINE ( 'NONE', #15274, #10246 ) ;
#11347 = EDGE_CURVE ( 'NONE', #19917, #53316, #36548, .T. ) ;
#11348 = VERTEX_POINT ( 'NONE', #19748 ) ;
#11349 = CIRCLE ( 'NONE', #29405, 1.224999999999998757 ) ;
#11350 = CARTESIAN_POINT ( 'NONE',  ( 49.00000000000000000, -21.00000000000000000, 13.86939075806900057 ) ) ;
#11351 = DIRECTION ( 'NONE',  ( -1.000000000000000000, 0.000000000000000000, -0.000000000000000000 ) ) ;
#11352 = FILL_AREA_STYLE ('',( #64756 ) ) ;
#11353 = EDGE_CURVE ( 'NONE', #25227, #17131, #66791, .T. ) ;
#11354 = EDGE_CURVE ( 'NONE', #50609, #66948, #6117, .T. ) ;
#11355 = AXIS2_PLACEMENT_3D ( 'NONE', #25945, #64813, #47496 ) ;
#11356 = CARTESIAN_POINT ( 'NONE',  ( -5.993516549646711766, 5.993516549646603409, 455.0000000000000568 ) ) ;
#11357 = EDGE_CURVE ( 'NONE', #30669, #67341, #61851, .T. ) ;
#11358 = VERTEX_POINT ( 'NONE', #24368 ) ;
#11359 = CYLINDRICAL_SURFACE ( 'NONE', #22618, 1.000000000000000000 ) ;
#11360 = ORIENTED_EDGE ( 'NONE', *, *, #26846, .T. ) ;
#11361 = ORIENTED_EDGE ( 'NONE', *, *, #8887, .T. ) ;
#11362 = DIRECTION ( 'NONE',  ( 0.000000000000000000, 1.000000000000000000, 0.000000000000000000 ) ) ;
#11363 = VECTOR ( 'NONE', #38897, 1000.000000000000000 ) ;
#11364 = DIRECTION ( 'NONE',  ( 1.000000000000000000, -0.000000000000000000, 0.000000000000000000 ) ) ;
#11365 = VECTOR ( 'NONE', #28770, 1000.000000000000000 ) ;
#11366 = DIRECTION ( 'NONE',  ( 0.000000000000000000, -0.000000000000000000, 1.000000000000000000 ) ) ;
#11367 = DIRECTION ( 'NONE',  ( -0.000000000000000000, 3.673940397442059868E-16, -1.000000000000000000 ) ) ;
#11368 = ORIENTED_EDGE ( 'NONE', *, *, #59715, .F. ) ;
#11369 = VERTEX_POINT ( 'NONE', #18344 ) ;
#11371 = ORIENTED_EDGE ( 'NONE', *, *, #29051, .F. ) ;
#11370 = DIRECTION ( 'NONE',  ( -1.000000000000000000, 0.000000000000000000, 0.000000000000000000 ) ) ;
#11372 = ORIENTED_EDGE ( 'NONE', *, *, #38629, .T. ) ;
#11373 = CARTESIAN_POINT ( 'NONE',  ( 6.006483450353401921, 5.993516549646582092, 455.0000000000000568 ) ) ;
#11374 = CARTESIAN_POINT ( 'NONE',  ( -29.50000000000000355, -11.50000000000000000, 15.00000000000000000 ) ) ;
#11375 = VECTOR ( 'NONE', #26813, 1000.000000000000000 ) ;
#11376 = CARTESIAN_POINT ( 'NONE',  ( 0.000000000000000000, -8.249999999999998224, -22.50000000000000000 ) ) ;
#11377 = CARTESIAN_POINT ( 'NONE',  ( 2.765062094116041980, -9.955011587777228499, 195.0000000000000284 ) ) ;
#11379 = CARTESIAN_POINT ( 'NONE',  ( -9.880476262117236175, 7.447976262117216528, 26.00000000000000711 ) ) ;
#11378 = DIRECTION ( 'NONE',  ( 0.000000000000000000, 1.000000000000000000, 0.000000000000000000 ) ) ;
#11380 = VERTEX_POINT ( 'NONE', #35301 ) ;
#11382 = ORIENTED_EDGE ( 'NONE', *, *, #9461, .F. ) ;
#11381 = DIRECTION ( 'NONE',  ( 0.000000000000000000, -1.000000000000000000, -3.673940397442059868E-16 ) ) ;
#11383 = ORIENTED_EDGE ( 'NONE', *, *, #23174, .T. ) ;
#11384 = ORIENTED_EDGE ( 'NONE', *, *, #5237, .T. ) ;
#11385 = CYLINDRICAL_SURFACE ( 'NONE', #46882, 0.2000000000000005107 ) ;
#11386 = LINE ( 'NONE', #59834, #37760 ) ;
#11387 = VECTOR ( 'NONE', #31069, 1000.000000000000000 ) ;
#11388 = EDGE_CURVE ( 'NONE', #55692, #31525, #38804, .T. ) ;
#11389 = DIRECTION ( 'NONE',  ( 0.000000000000000000, 0.000000000000000000, -1.000000000000000000 ) ) ;
#11390 = AXIS2_PLACEMENT_3D ( 'NONE', #31172, #69697, #64727 ) ;
#11391 = ORIENTED_EDGE ( 'NONE', *, *, #50117, .F. ) ;
#11392 = VERTEX_POINT ( 'NONE', #41322 ) ;
#11393 = EDGE_CURVE ( 'NONE', #65422, #56927, #3506, .T. ) ;
#11394 = AXIS2_PLACEMENT_3D ( 'NONE', #12023, #34280, #49531 ) ;
#11395 = EDGE_CURVE ( 'NONE', #19920, #10538, #61394, .T. ) ;
#11396 = DIRECTION ( 'NONE',  ( -1.000000000000000000, 0.000000000000000000, 0.000000000000000000 ) ) ;
#11397 = CARTESIAN_POINT ( 'NONE',  ( 7.250000000000005329, -8.249999999999998224, -15.00000000000000000 ) ) ;
#11398 = CARTESIAN_POINT ( 'NONE',  ( 7.250000000000005329, -7.449999999999998401, -11.50000000000000000 ) ) ;
#11399 = EDGE_CURVE ( 'NONE', #53330, #52904, #30726, .T. ) ;
#11400 = ORIENTED_EDGE ( 'NONE', *, *, #33138, .T. ) ;
#11401 = VECTOR ( 'NONE', #21373, 1000.000000000000000 ) ;
#11402 = VECTOR ( 'NONE', #8764, 1000.000000000000000 ) ;
#11403 = ORIENTED_EDGE ( 'NONE', *, *, #3659, .F. ) ;
#11404 = DIRECTION ( 'NONE',  ( -1.000000000000000000, 0.000000000000000000, 0.000000000000000000 ) ) ;
#11405 = LINE ( 'NONE', #69418, #15346 ) ;
#11406 = VERTEX_POINT ( 'NONE', #56197 ) ;
#11407 = VECTOR ( 'NONE', #17442, 1000.000000000000000 ) ;
#11408 = DIRECTION ( 'NONE',  ( 1.000000000000000000, -0.000000000000000000, -0.000000000000000000 ) ) ;
#11410 = ORIENTED_EDGE ( 'NONE', *, *, #36765, .F. ) ;
#11409 = LINE ( 'NONE', #43929, #149 ) ;
#11411 = EDGE_LOOP ( 'NONE', ( #49987, #7410, #34762, #68698 ) ) ;
#11413 = LINE ( 'NONE', #20628, #13421 ) ;
#11412 = VECTOR ( 'NONE', #31285, 1000.000000000000000 ) ;
#11414 = DIRECTION ( 'NONE',  ( 0.000000000000000000, -1.000000000000000000, 0.000000000000000000 ) ) ;
#11415 = DIRECTION ( 'NONE',  ( 0.000000000000000000, 1.000000000000000000, 0.000000000000000000 ) ) ;
#11416 = LINE ( 'NONE', #23060, #44740 ) ;
#11417 = DIRECTION ( 'NONE',  ( 0.000000000000000000, 1.000000000000000000, 0.000000000000000000 ) ) ;
#11418 = EDGE_LOOP ( 'NONE', ( #19444, #30253, #30061, #32365 ) ) ;
#11419 = PLANE ( 'NONE',  #10099 ) ;
#11420 = VERTEX_POINT ( 'NONE', #13044 ) ;
#11421 = DIRECTION ( 'NONE',  ( 0.000000000000000000, -1.000000000000000000, -7.802196388977322746E-10 ) ) ;
#11422 = CARTESIAN_POINT ( 'NONE',  ( 12.00648345035338060, -7.826483450353491023, 455.0000000000000568 ) ) ;
#11423 = VECTOR ( 'NONE', #36992, 1000.000000000000114 ) ;
#11424 = FACE_OUTER_BOUND ( 'NONE', #61614, .T. ) ;
#11425 = DIRECTION ( 'NONE',  ( -1.000000000000000000, 0.000000000000000000, 0.000000000000000000 ) ) ;
#11426 = CARTESIAN_POINT ( 'NONE',  ( 30.00000000000000000, -12.00000000000000000, 10.52786404500095863 ) ) ;
#11427 = EDGE_LOOP ( 'NONE', ( #49255, #48462, #27236, #58028 ) ) ;
#11428 = ORIENTED_EDGE ( 'NONE', *, *, #13777, .F. ) ;
#11429 = DIRECTION ( 'NONE',  ( 0.000000000000000000, 0.000000000000000000, -1.000000000000000000 ) ) ;
#11430 = EDGE_CURVE ( 'NONE', #2382, #18569, #7743, .T. ) ;
#11431 = AXIS2_PLACEMENT_3D ( 'NONE', #27347, #54222, #27684 ) ;
#11432 = AXIS2_PLACEMENT_3D ( 'NONE', #65084, #38882, #50184 ) ;
#11433 = EDGE_CURVE ( 'NONE', #63779, #19378, #14468, .T. ) ;
#11434 = ORIENTED_EDGE ( 'NONE', *, *, #33427, .F. ) ;
#11435 = PLANE ( 'NONE',  #10150 ) ;
#11436 = LINE ( 'NONE', #21008, #51248 ) ;
#11437 = ORIENTED_EDGE ( 'NONE', *, *, #51689, .F. ) ;
#11438 = CARTESIAN_POINT ( 'NONE',  ( 6.501044194225450212, 3.142976262117187058, 54.00000000000000711 ) ) ;
#11439 = LINE ( 'NONE', #22417, #68103 ) ;
#11440 = ORIENTED_EDGE ( 'NONE', *, *, #25115, .T. ) ;
#11441 = CARTESIAN_POINT ( 'NONE',  ( 7.250000000000005329, -7.249999999999998224, -15.00000000000000000 ) ) ;
#11442 = DIRECTION ( 'NONE',  ( -1.000000000000000000, 0.000000000000000000, 0.000000000000000000 ) ) ;
#11443 = AXIS2_PLACEMENT_3D ( 'NONE', #33630, #6747, #49886 ) ;
#11444 = VECTOR ( 'NONE', #6245, 1000.000000000000000 ) ;
#11445 = DIRECTION ( 'NONE',  ( 1.000000000000000000, -0.000000000000000000, 0.000000000000000000 ) ) ;
#11446 = DIRECTION ( 'NONE',  ( 0.000000000000000000, 0.000000000000000000, 1.000000000000000000 ) ) ;
#11447 = ORIENTED_EDGE ( 'NONE', *, *, #5398, .F. ) ;
#11449 = ORIENTED_EDGE ( 'NONE', *, *, #56407, .F. ) ;
#11448 = DIRECTION ( 'NONE',  ( 0.000000000000000000, -1.000000000000000000, 0.000000000000000000 ) ) ;
#11450 = AXIS2_PLACEMENT_3D ( 'NONE', #51725, #31224, #14244 ) ;
#11451 = EDGE_CURVE ( 'NONE', #37646, #4599, #28656, .T. ) ;
#11452 = CARTESIAN_POINT ( 'NONE',  ( 11.12648345035340647, 7.793516549646564151, 455.0000000000000568 ) ) ;
#11453 = CARTESIAN_POINT ( 'NONE',  ( 30.00000000000000000, -5.599999999999379696, 26.60000000000059828 ) ) ;
#11454 = DIRECTION ( 'NONE',  ( 0.000000000000000000, -0.1111111111108836896, 0.9938079899999319178 ) ) ;
#11455 = VERTEX_POINT ( 'NONE', #34959 ) ;
#11456 = VECTOR ( 'NONE', #53539, 1000.000000000000000 ) ;
#11457 = DIRECTION ( 'NONE',  ( -0.000000000000000000, -0.000000000000000000, -1.000000000000000000 ) ) ;
#11458 = FACE_OUTER_BOUND ( 'NONE', #2350, .T. ) ;
#11459 = ORIENTED_EDGE ( 'NONE', *, *, #47105, .T. ) ;
#11460 = EDGE_LOOP ( 'NONE', ( #65485, #6658, #21823, #47309, #59682, #8828, #46258, #55313, #52450, #13019, #33860, #10286, #3592, #67913, #6821, #35635, #44323 ) ) ;
#11461 = ORIENTED_EDGE ( 'NONE', *, *, #16189, .T. ) ;
#11462 = CARTESIAN_POINT ( 'NONE',  ( 11.78648345035337996, 4.393516549646516722, 455.0000000000000568 ) ) ;
#11463 = CARTESIAN_POINT ( 'NONE',  ( 9.899999999999998579, 13.66939075806899240, -20.79999999999999361 ) ) ;
#11464 = CARTESIAN_POINT ( 'NONE',  ( 8.930623737882839919, 8.566576262117191476, 26.00000000000000711 ) ) ;
#11465 = ORIENTED_EDGE ( 'NONE', *, *, #9969, .T. ) ;
#11466 = EDGE_LOOP ( 'NONE', ( #63419, #8197, #6665, #64532 ) ) ;
#11467 = ORIENTED_EDGE ( 'NONE', *, *, #61910, .F. ) ;
#11468 = EDGE_CURVE ( 'NONE', #27729, #4139, #17354, .T. ) ;
#11469 = FACE_OUTER_BOUND ( 'NONE', #14526, .T. ) ;
#11470 = ORIENTED_EDGE ( 'NONE', *, *, #6871, .F. ) ;
#11471 = VERTEX_POINT ( 'NONE', #67517 ) ;
#11472 = ADVANCED_FACE ( 'NONE', ( #57592 ), #30017, .T. ) ;
#11473 = ORIENTED_EDGE ( 'NONE', *, *, #46118, .F. ) ;
#11474 = ORIENTED_EDGE ( 'NONE', *, *, #17896, .T. ) ;
#11475 = CARTESIAN_POINT ( 'NONE',  ( -7.450000000000001954, 7.250000000000000000, -16.50000000000000000 ) ) ;
#11476 = AXIS2_PLACEMENT_3D ( 'NONE', #36462, #62992, #47418 ) ;
#11478 = EDGE_LOOP ( 'NONE', ( #38495, #25875, #59092, #48845 ) ) ;
#11477 = CARTESIAN_POINT ( 'NONE',  ( -4.173516549646837603, -11.78648345035344214, 455.0000000000000568 ) ) ;
#11479 = CARTESIAN_POINT ( 'NONE',  ( -6.822336235477446387, 4.135079735113102117, 54.00000000000000711 ) ) ;
#11480 = VECTOR ( 'NONE', #22633, 1000.000000000000000 ) ;
#11481 = DIRECTION ( 'NONE',  ( 1.000000000000000000, 0.000000000000000000, 0.000000000000000000 ) ) ;
#11482 = DIRECTION ( 'NONE',  ( 1.000000000000000000, 0.000000000000000000, 0.000000000000000000 ) ) ;
#11483 = ORIENTED_EDGE ( 'NONE', *, *, #49921, .T. ) ;
#11484 = CIRCLE ( 'NONE', #4702, 3.299999999999473577 ) ;
#11485 = AXIS2_PLACEMENT_3D ( 'NONE', #10934, #20842, #63643 ) ;
#11486 = CARTESIAN_POINT ( 'NONE',  ( -4.947141984184481700, 7.342976262117180575, 26.00000000000000711 ) ) ;
#11487 = EDGE_CURVE ( 'NONE', #35639, #61702, #3160, .T. ) ;
#11488 = EDGE_LOOP ( 'NONE', ( #8394, #48614, #13642, #15218 ) ) ;
#11489 = DIRECTION ( 'NONE',  ( -1.000000000000000000, 0.000000000000000000, 0.000000000000000000 ) ) ;
#11490 = DIRECTION ( 'NONE',  ( 0.000000000000000000, 0.000000000000000000, -1.000000000000000000 ) ) ;
#11491 = DIRECTION ( 'NONE',  ( -1.000000000000000000, 0.000000000000000000, -0.000000000000000000 ) ) ;
#11492 = CARTESIAN_POINT ( 'NONE',  ( 11.08848345035341865, 11.07551654964652776, 455.0000000000000568 ) ) ;
#11493 = ORIENTED_EDGE ( 'NONE', *, *, #8042, .F. ) ;
#11494 = LINE ( 'NONE', #44023, #5376 ) ;
#11495 = VECTOR ( 'NONE', #59, 1000.000000000000000 ) ;
#11496 = DIRECTION ( 'NONE',  ( 0.000000000000000000, 1.000000000000000000, 0.000000000000000000 ) ) ;
#11497 = CARTESIAN_POINT ( 'NONE',  ( 17.89999999999999858, 0.000000000000000000, 1.077467997501122647E-15 ) ) ;
#11498 = APPLICATION_CONTEXT ( 'automotive_design' ) ;
#11499 = FACE_BOUND ( 'NONE', #60596, .T. ) ;
#11500 = DIRECTION ( 'NONE',  ( 0.000000000000000000, 0.000000000000000000, 1.000000000000000000 ) ) ;
#11501 = DIRECTION ( 'NONE',  ( 1.000000000000000000, 0.000000000000000000, 0.000000000000000000 ) ) ;
#11502 = CARTESIAN_POINT ( 'NONE',  ( 283.0000000000000568, -40.30000000000000426, 8.900000000000000355 ) ) ;
#11503 = EDGE_CURVE ( 'NONE', #53184, #45669, #60258, .T. ) ;
#11504 = ADVANCED_FACE ( 'NONE', ( #40279 ), #13404, .F. ) ;
#11505 = ORIENTED_EDGE ( 'NONE', *, *, #5442, .T. ) ;
#11506 = FACE_OUTER_BOUND ( 'NONE', #66263, .T. ) ;
#11507 = EDGE_CURVE ( 'NONE', #64155, #32920, #14102, .T. ) ;
#11508 = LINE ( 'NONE', #7602, #37623 ) ;
#11509 = DIRECTION ( 'NONE',  ( 0.000000000000000000, 0.000000000000000000, 1.000000000000000000 ) ) ;
#11510 = EDGE_LOOP ( 'NONE', ( #56599, #38634, #2917, #54684 ) ) ;
#11511 = DIRECTION ( 'NONE',  ( -0.000000000000000000, 3.673940397442059868E-16, -1.000000000000000000 ) ) ;
#11512 = DIRECTION ( 'NONE',  ( 0.000000000000000000, 0.000000000000000000, 1.000000000000000000 ) ) ;
#11513 = EDGE_CURVE ( 'NONE', #37177, #65043, #58652, .T. ) ;
#11514 = AXIS2_PLACEMENT_3D ( 'NONE', #28547, #33856, #55440 ) ;
#11515 = CARTESIAN_POINT ( 'NONE',  ( -6.775514141871423313, -7.408280051175137437, 26.00000000000000000 ) ) ;
#11516 = EDGE_CURVE ( 'NONE', #55748, #65336, #26130, .T. ) ;
#11517 = DIRECTION ( 'NONE',  ( 1.836970198721029934E-16, 1.836970198721010706E-16, -1.000000000000000000 ) ) ;
#11518 = EDGE_CURVE ( 'NONE', #38364, #4410, #31786, .T. ) ;
#11519 = DIRECTION ( 'NONE',  ( 0.000000000000000000, -1.000000000000000000, 0.000000000000000000 ) ) ;
#11520 = VECTOR ( 'NONE', #21855, 1000.000000000000000 ) ;
#11521 = VERTEX_POINT ( 'NONE', #43689 ) ;
#11522 = ADVANCED_FACE ( 'NONE', ( #33070 ), #5859, .T. ) ;
#11523 = ORIENTED_EDGE ( 'NONE', *, *, #23861, .F. ) ;
#11524 = LINE ( 'NONE', #32759, #38354 ) ;
#11525 = FACE_OUTER_BOUND ( 'NONE', #13133, .T. ) ;
#11526 = ORIENTED_EDGE ( 'NONE', *, *, #48604, .T. ) ;
#11527 = AXIS2_PLACEMENT_3D ( 'NONE', #38611, #48881, #10689 ) ;
#11528 = CARTESIAN_POINT ( 'NONE',  ( 7.272650909786602114, 4.188533722949199678, 455.0000000000000568 ) ) ;
#11529 = ORIENTED_EDGE ( 'NONE', *, *, #12599, .F. ) ;
#11530 = AXIS2_PLACEMENT_3D ( 'NONE', #65635, #55381, #65970 ) ;
#11531 = DIRECTION ( 'NONE',  ( 0.000000000000000000, 0.000000000000000000, 1.000000000000000000 ) ) ;
#11532 = ORIENTED_EDGE ( 'NONE', *, *, #17109, .F. ) ;
#11533 = ORIENTED_EDGE ( 'NONE', *, *, #40175, .T. ) ;
#11534 = DIRECTION ( 'NONE',  ( -1.000000000000000000, -1.301042606982605321E-16, 0.000000000000000000 ) ) ;
#11535 = EDGE_LOOP ( 'NONE', ( #35950, #41358, #53049, #25058 ) ) ;
#11536 = CYLINDRICAL_SURFACE ( 'NONE', #25239, 0.3499999999999302558 ) ;
#11537 = DIRECTION ( 'NONE',  ( 1.000000000000000000, 0.000000000000000000, -0.000000000000000000 ) ) ;
#11538 = LINE ( 'NONE', #1624, #68603 ) ;
#11539 = VECTOR ( 'NONE', #39856, 1000.000000000000000 ) ;
#11540 = ADVANCED_FACE ( 'NONE', ( #3854 ), #63253, .T. ) ;
#11541 = VERTEX_POINT ( 'NONE', #20465 ) ;
#11542 = EDGE_LOOP ( 'NONE', ( #41289, #40472, #56529, #58880 ) ) ;
#11543 = DIRECTION ( 'NONE',  ( 0.000000000000000000, 1.000000000000000000, 0.000000000000000000 ) ) ;
#11544 = VECTOR ( 'NONE', #13335, 1000.000000000000000 ) ;
#11545 = CARTESIAN_POINT ( 'NONE',  ( 7.250000000000005329, -8.249999999999998224, -26.00000000000001066 ) ) ;
#11546 = VERTEX_POINT ( 'NONE', #63960 ) ;
#11547 = ORIENTED_EDGE ( 'NONE', *, *, #1244, .T. ) ;
#11548 = EDGE_CURVE ( 'NONE', #31253, #25515, #20744, .T. ) ;
#11550 = ORIENTED_EDGE ( 'NONE', *, *, #34542, .F. ) ;
#11549 = CONTEXT_DEPENDENT_SHAPE_REPRESENTATION ( #51257, #34078 ) ;
#11551 = CARTESIAN_POINT ( 'NONE',  ( 30.00000000000000000, -14.04000000000000092, -14.80000000000000071 ) ) ;
#11553 = ORIENTED_EDGE ( 'NONE', *, *, #62887, .T. ) ;
#11552 = CARTESIAN_POINT ( 'NONE',  ( 25.57999999999999829, 0.000000000000000000, 0.000000000000000000 ) ) ;
#11554 = CARTESIAN_POINT ( 'NONE',  ( -7.250000000000000888, 8.250000000000001776, -26.00000000000001066 ) ) ;
#11555 = DIRECTION ( 'NONE',  ( -0.000000000000000000, 3.673940397442059868E-16, -1.000000000000000000 ) ) ;
#11556 = ORIENTED_EDGE ( 'NONE', *, *, #39673, .T. ) ;
#11557 = EDGE_LOOP ( 'NONE', ( #3135, #58653, #31590, #26165 ) ) ;
#11558 = ORIENTED_EDGE ( 'NONE', *, *, #25907, .F. ) ;
#11559 = CARTESIAN_POINT ( 'NONE',  ( 30.00000000000000000, -9.454754784057099570, -17.53999999999999915 ) ) ;
#11560 = EDGE_CURVE ( 'NONE', #15483, #38190, #20119, .T. ) ;
#11561 = VECTOR ( 'NONE', #44024, 1000.000000000000000 ) ;
#11562 = VERTEX_POINT ( 'NONE', #553 ) ;
#11563 = CYLINDRICAL_SURFACE ( 'NONE', #40131, 0.2999999999998732569 ) ;
#11564 = DIRECTION ( 'NONE',  ( 0.000000000000000000, -1.000000000000000000, 0.000000000000000000 ) ) ;
#11565 = ADVANCED_FACE ( 'NONE', ( #46984 ), #27423, .T. ) ;
#11567 = ORIENTED_EDGE ( 'NONE', *, *, #9777, .F. ) ;
#11566 = CARTESIAN_POINT ( 'NONE',  ( 14.50000000000000000, -42.50000000000000000, 26.50000000000000000 ) ) ;
#11568 = ORIENTED_EDGE ( 'NONE', *, *, #24585, .F. ) ;
#11569 = EDGE_CURVE ( 'NONE', #15576, #42345, #15526, .T. ) ;
#11570 = LINE ( 'NONE', #65347, #43033 ) ;
#11571 = PLANE ( 'NONE',  #5891 ) ;
#11572 = ADVANCED_FACE ( 'NONE', ( #60278 ), #63610, .F. ) ;
#11573 = DIRECTION ( 'NONE',  ( 1.000000000000000000, 3.016910393003147986E-15, 1.108394896831706469E-30 ) ) ;
#11574 = EDGE_CURVE ( 'NONE', #2392, #28744, #58047, .T. ) ;
#11575 = EDGE_CURVE ( 'NONE', #54414, #66278, #51219, .T. ) ;
#11576 = CARTESIAN_POINT ( 'NONE',  ( 11.08848345035341687, 10.19191654964656379, 455.0000000000000568 ) ) ;
#11577 = DIRECTION ( 'NONE',  ( 1.214636490590110272E-14, 1.000000000000000000, 1.836970198721032892E-16 ) ) ;
#11578 = ORIENTED_EDGE ( 'NONE', *, *, #66667, .F. ) ;
#11579 = CARTESIAN_POINT ( 'NONE',  ( 30.00000000000000000, -14.33999999999999986, 14.50000000000000000 ) ) ;
#11580 = DIRECTION ( 'NONE',  ( 8.673617379884030739E-15, 1.000000000000000000, 0.000000000000000000 ) ) ;
#11581 = EDGE_CURVE ( 'NONE', #22725, #30962, #49349, .T. ) ;
#11582 = CARTESIAN_POINT ( 'NONE',  ( 10.74648345035334529, 1.077516549646528876, 455.0000000000000568 ) ) ;
#11583 = FACE_OUTER_BOUND ( 'NONE', #26216, .T. ) ;
#11584 = AXIS2_PLACEMENT_3D ( 'NONE', #7876, #66930, #33716 ) ;
#11585 = ADVANCED_FACE ( 'NONE', ( #58304 ), #47334, .F. ) ;
#11586 = DIRECTION ( 'NONE',  ( 0.000000000000000000, -0.7051282051282052876, -0.7090798363602477394 ) ) ;
#11587 = DIRECTION ( 'NONE',  ( 0.000000000000000000, 1.000000000000000000, 0.000000000000000000 ) ) ;
#11588 = EDGE_CURVE ( 'NONE', #22431, #60745, #52658, .T. ) ;
#11589 = VECTOR ( 'NONE', #33777, 1000.000000000000000 ) ;
#11590 = CARTESIAN_POINT ( 'NONE',  ( 0.000000000000000000, -17.79289321881345032, -20.50000000000000000 ) ) ;
#11591 = AXIS2_PLACEMENT_3D ( 'NONE', #25183, #47446, #25894 ) ;
#11592 = ORIENTED_EDGE ( 'NONE', *, *, #56146, .F. ) ;
#11593 = DIRECTION ( 'NONE',  ( 1.000000000000000000, 0.000000000000000000, -0.000000000000000000 ) ) ;
#11594 = CARTESIAN_POINT ( 'NONE',  ( 39.00000000000000000, 4.286263797015736595E-16, -3.500000000000000000 ) ) ;
#11595 = VERTEX_POINT ( 'NONE', #36732 ) ;
#11596 = CARTESIAN_POINT ( 'NONE',  ( -3.834182069070765309, 7.342976262117171693, 54.00000000000000711 ) ) ;
#11597 = LINE ( 'NONE', #45160, #11874 ) ;
#11598 = CYLINDRICAL_SURFACE ( 'NONE', #2741, 2.250000000000001776 ) ;
#11600 = AXIS2_PLACEMENT_3D ( 'NONE', #69263, #42382, #15536 ) ;
#11599 = DIRECTION ( 'NONE',  ( -0.000000000000000000, 3.673940397442059868E-16, -1.000000000000000000 ) ) ;
#11601 = EDGE_CURVE ( 'NONE', #2273, #3545, #57938, .T. ) ;
#11602 = DIRECTION ( 'NONE',  ( 0.000000000000000000, 0.000000000000000000, -1.000000000000000000 ) ) ;
#11603 = ADVANCED_FACE ( 'NONE', ( #65928 ), #13235, .F. ) ;
#11604 = LINE ( 'NONE', #17612, #42045 ) ;
#11605 = ORIENTED_EDGE ( 'NONE', *, *, #23696, .T. ) ;
#11606 = DIRECTION ( 'NONE',  ( 0.7671651518153105309, -0.6414496315691445849, -0.000000000000000000 ) ) ;
#11607 = CARTESIAN_POINT ( 'NONE',  ( -29.50000000000000355, -11.50000000000000000, 11.00000000000000000 ) ) ;
#11608 = VERTEX_POINT ( 'NONE', #7222 ) ;
#11609 = CARTESIAN_POINT ( 'NONE',  ( 7.450000000000003730, -7.249999999999997335, -9.500000000000001776 ) ) ;
#11610 = AXIS2_PLACEMENT_3D ( 'NONE', #40028, #49955, #34739 ) ;
#11611 = CARTESIAN_POINT ( 'NONE',  ( 7.272650909786597673, 7.798499376343980494, 195.0000000000000284 ) ) ;
#11612 = LINE ( 'NONE', #44832, #26539 ) ;
#11613 = VERTEX_POINT ( 'NONE', #50715 ) ;
#11614 = VERTEX_POINT ( 'NONE', #7581 ) ;
#11615 = CIRCLE ( 'NONE', #4882, 0.1749999999999980738 ) ;
#11616 = DIRECTION ( 'NONE',  ( 0.000000000000000000, 0.000000000000000000, 1.000000000000000000 ) ) ;
#11617 = ORIENTED_EDGE ( 'NONE', *, *, #18270, .T. ) ;
#11618 = EDGE_LOOP ( 'NONE', ( #38273, #59734, #49805, #16270 ) ) ;
#11619 = LINE ( 'NONE', #16616, #3320 ) ;
#11620 = CARTESIAN_POINT ( 'NONE',  ( 4.740315990920131561, -4.201500623656145628, 455.0000000000000568 ) ) ;
#11621 = DIRECTION ( 'NONE',  ( 0.000000000000000000, 0.000000000000000000, 1.000000000000000000 ) ) ;
#11622 = ORIENTED_EDGE ( 'NONE', *, *, #57126, .T. ) ;
#11623 = AXIS2_PLACEMENT_3D ( 'NONE', #66429, #49821, #24341 ) ;
#11624 = CARTESIAN_POINT ( 'NONE',  ( -13.00000000000000178, -17.35230188589299871, -15.35019951917099945 ) ) ;
#11626 = PLANE ( 'NONE',  #38855 ) ;
#11625 = DIRECTION ( 'NONE',  ( -4.336808689942006692E-15, -1.000000000000000000, 0.000000000000000000 ) ) ;
#11627 = ORIENTED_EDGE ( 'NONE', *, *, #68480, .F. ) ;
#11628 = VERTEX_POINT ( 'NONE', #2627 ) ;
#11630 = EDGE_LOOP ( 'NONE', ( #16909, #53940, #31683, #27769 ) ) ;
#11629 = CARTESIAN_POINT ( 'NONE',  ( 283.0000000000000568, -25.93000000000544958, -9.412893218815410634 ) ) ;
#11631 = ORIENTED_EDGE ( 'NONE', *, *, #22615, .F. ) ;
#11632 = EDGE_CURVE ( 'NONE', #17972, #18063, #28792, .T. ) ;
#11633 = LINE ( 'NONE', #44166, #552 ) ;
#11634 = ADVANCED_FACE ( 'NONE', ( #18185 ), #39069, .F. ) ;
#11635 = DIRECTION ( 'NONE',  ( -1.000000000000000000, 0.000000000000000000, 0.000000000000000000 ) ) ;
#11636 = VECTOR ( 'NONE', #13101, 1000.000000000000000 ) ;
#11637 = ORIENTED_EDGE ( 'NONE', *, *, #30744, .F. ) ;
#11638 = ORIENTED_EDGE ( 'NONE', *, *, #45022, .T. ) ;
#11639 = EDGE_CURVE ( 'NONE', #57216, #58124, #56373, .T. ) ;
#11641 = CARTESIAN_POINT ( 'NONE',  ( -8.250000000000001776, 7.250000000000000888, -26.00000000000001066 ) ) ;
#11640 = VECTOR ( 'NONE', #47279, 1000.000000000000000 ) ;
#11642 = VECTOR ( 'NONE', #63405, 1000.000000000000000 ) ;
#11643 = EDGE_CURVE ( 'NONE', #16876, #9687, #29149, .T. ) ;
#11644 = CARTESIAN_POINT ( 'NONE',  ( 4.206483450353343478, -11.12648345035347575, 455.0000000000000568 ) ) ;
#11645 = VERTEX_POINT ( 'NONE', #23846 ) ;
#11646 = DIRECTION ( 'NONE',  ( 9.912705577010336396E-15, 1.000000000000000000, 0.000000000000000000 ) ) ;
#11647 = FACE_OUTER_BOUND ( 'NONE', #58848, .T. ) ;
#11648 = STYLED_ITEM ( 'NONE', ( #49432 ), #43151 ) ;
#11649 = AXIS2_PLACEMENT_3D ( 'NONE', #24646, #46195, #67769 ) ;
#11650 = ADVANCED_FACE ( 'NONE', ( #1937 ), #44704, .T. ) ;
#11651 = FACE_OUTER_BOUND ( 'NONE', #43404, .T. ) ;
#11652 = ORIENTED_EDGE ( 'NONE', *, *, #27978, .F. ) ;
#11653 = DIRECTION ( 'NONE',  ( -1.000000000000000000, 0.000000000000000000, 0.000000000000000000 ) ) ;
#11654 = LINE ( 'NONE', #55504, #50894 ) ;
#11655 = ADVANCED_FACE ( 'NONE', ( #23503 ), #51067, .T. ) ;
#11656 = EDGE_LOOP ( 'NONE', ( #20038, #7724, #39894, #41011 ) ) ;
#11658 = ORIENTED_EDGE ( 'NONE', *, *, #5165, .F. ) ;
#11657 = DIRECTION ( 'NONE',  ( 1.000000000000000000, 0.000000000000000000, 0.000000000000000000 ) ) ;
#11659 = ADVANCED_FACE ( 'NONE', ( #18898 ), #2283, .F. ) ;
#11660 = DIRECTION ( 'NONE',  ( 0.000000000000000000, 0.000000000000000000, 1.000000000000000000 ) ) ;
#11661 = DIRECTION ( 'NONE',  ( -0.000000000000000000, -0.000000000000000000, 1.000000000000000000 ) ) ;
#11662 = VECTOR ( 'NONE', #60143, 1000.000000000000000 ) ;
#11663 = CARTESIAN_POINT ( 'NONE',  ( -16.75000000000000000, -2.500000000000000000, 21.77831216351300014 ) ) ;
#11664 = CARTESIAN_POINT ( 'NONE',  ( -8.250000000000001776, 7.250000000000000888, -26.00000000000001066 ) ) ;
#11665 = EDGE_CURVE ( 'NONE', #20267, #14942, #7922, .T. ) ;
#11666 = EDGE_CURVE ( 'NONE', #31019, #856, #43349, .T. ) ;
#11667 = FACE_OUTER_BOUND ( 'NONE', #50041, .T. ) ;
#11668 = LINE ( 'NONE', #33254, #38330 ) ;
#11669 = CIRCLE ( 'NONE', #65741, 0.1749999999999998224 ) ;
#11670 = ORIENTED_EDGE ( 'NONE', *, *, #66570, .T. ) ;
#11671 = DIRECTION ( 'NONE',  ( -1.000000000000000000, 1.794541526872559352E-16, 0.000000000000000000 ) ) ;
#11672 = EDGE_CURVE ( 'NONE', #9024, #61728, #28448, .T. ) ;
#11674 = ORIENTED_EDGE ( 'NONE', *, *, #39777, .T. ) ;
#11673 = CARTESIAN_POINT ( 'NONE',  ( -15.50000000000000000, -1.037157890325000054, -26.00000000000000000 ) ) ;
#11676 = EDGE_LOOP ( 'NONE', ( #1850, #26566, #30854, #5413 ) ) ;
#11675 = DIRECTION ( 'NONE',  ( -1.000000000000000000, 0.000000000000000000, 0.000000000000000000 ) ) ;
#11677 = CARTESIAN_POINT ( 'NONE',  ( 30.90000000000000213, -14.06939075806900163, -20.80000000000000426 ) ) ;
#11678 = CARTESIAN_POINT ( 'NONE',  ( 20.90000000000000213, -14.06939075806900874, 20.80000000000001137 ) ) ;
#11679 = ORIENTED_EDGE ( 'NONE', *, *, #13200, .F. ) ;
#11680 = DIRECTION ( 'NONE',  ( -1.836970198721029934E-16, -1.836970198721010706E-16, 1.000000000000000000 ) ) ;
#11681 = CARTESIAN_POINT ( 'NONE',  ( 14.25000000000000000, -2.500000000000000000, -23.22168783648699986 ) ) ;
#11682 = ORIENTED_EDGE ( 'NONE', *, *, #9020, .F. ) ;
#11683 = CARTESIAN_POINT ( 'NONE',  ( -7.450000000000001954, -7.249999999999998224, -20.50000000000000000 ) ) ;
#11684 = DIRECTION ( 'NONE',  ( 0.7071067811865474617, 0.000000000000000000, 0.7071067811865474617 ) ) ;
#11685 = EDGE_CURVE ( 'NONE', #41827, #5747, #17850, .T. ) ;
#11686 = CARTESIAN_POINT ( 'NONE',  ( 29.50000000000000355, -11.50000000000100009, -15.00000000000084910 ) ) ;
#11687 = EDGE_CURVE ( 'NONE', #29731, #42484, #55342, .T. ) ;
#11688 = DIRECTION ( 'NONE',  ( 0.000000000000000000, 0.000000000000000000, -1.000000000000000000 ) ) ;
#11689 = AXIS2_PLACEMENT_3D ( 'NONE', #4330, #21281, #37538 ) ;
#11690 = AXIS2_PLACEMENT_3D ( 'NONE', #37738, #27471, #49042 ) ;
#11691 = VERTEX_POINT ( 'NONE', #62019 ) ;
#11692 = DIRECTION ( 'NONE',  ( 0.000000000000000000, -0.1111111111108840643, -0.9938079899999319178 ) ) ;
#11693 = VERTEX_POINT ( 'NONE', #13589 ) ;
#11694 = VERTEX_POINT ( 'NONE', #55006 ) ;
#11695 = VECTOR ( 'NONE', #43100, 1000.000000000000000 ) ;
#11696 = DIRECTION ( 'NONE',  ( 1.000000000000000000, -0.000000000000000000, -0.000000000000000000 ) ) ;
#11697 = DIRECTION ( 'NONE',  ( 1.000000000000000000, -0.000000000000000000, -0.000000000000000000 ) ) ;
#11698 = CIRCLE ( 'NONE', #48977, 0.3499999999999597877 ) ;
#11699 = AXIS2_PLACEMENT_3D ( 'NONE', #33424, #68563, #41675 ) ;
#11700 = DIRECTION ( 'NONE',  ( -0.000000000000000000, -0.000000000000000000, 1.000000000000000000 ) ) ;
#11701 = VECTOR ( 'NONE', #63388, 1000.000000000000000 ) ;
#11702 = AXIS2_PLACEMENT_3D ( 'NONE', #28688, #60864, #56611 ) ;
#11703 = DIRECTION ( 'NONE',  ( -0.4999999999999832356, 0.000000000000000000, -0.8660254037844483666 ) ) ;
#11704 = VERTEX_POINT ( 'NONE', #44355 ) ;
#11705 = VERTEX_POINT ( 'NONE', #50017 ) ;
#11707 = ORIENTED_EDGE ( 'NONE', *, *, #227, .F. ) ;
#11706 = PLANE ( 'NONE',  #39649 ) ;
#11708 = ORIENTED_EDGE ( 'NONE', *, *, #29301, .F. ) ;
#11709 = DIRECTION ( 'NONE',  ( 1.000000000000000000, 0.000000000000000000, 0.000000000000000000 ) ) ;
#11710 = LINE ( 'NONE', #48177, #39903 ) ;
#11711 = CARTESIAN_POINT ( 'NONE',  ( 7.749999999999998224, -7.348062532928000934, 5.000000000000000000 ) ) ;
#11712 = SURFACE_STYLE_USAGE ( .BOTH. , #32951 ) ;
#11714 = LINE ( 'NONE', #12743, #28895 ) ;
#11713 = DIRECTION ( 'NONE',  ( -1.000000000000000000, 1.671920889371702854E-15, 6.142537696789956391E-31 ) ) ;
#11715 = ORIENTED_EDGE ( 'NONE', *, *, #38484, .F. ) ;
#11717 = EDGE_LOOP ( 'NONE', ( #27457, #49338, #6626, #12140 ) ) ;
#11716 = CARTESIAN_POINT ( 'NONE',  ( -11.07551654964667520, 11.07551654964660237, 195.0000000000000284 ) ) ;
#11718 = VERTEX_POINT ( 'NONE', #23145 ) ;
#11719 = EDGE_LOOP ( 'NONE', ( #14228, #61281, #21722, #54494 ) ) ;
#11720 = LINE ( 'NONE', #16710, #27670 ) ;
#11721 = DIRECTION ( 'NONE',  ( -1.000000000000000000, 0.000000000000000000, 0.000000000000000000 ) ) ;
#11722 = EDGE_CURVE ( 'NONE', #31382, #25281, #39408, .T. ) ;
#11723 = DIRECTION ( 'NONE',  ( 0.000000000000000000, 0.000000000000000000, -1.000000000000000000 ) ) ;
#11724 = LINE ( 'NONE', #49571, #54558 ) ;
#11725 = ORIENTED_EDGE ( 'NONE', *, *, #18201, .T. ) ;
#11726 = ORIENTED_EDGE ( 'NONE', *, *, #9792, .F. ) ;
#11727 = AXIS2_PLACEMENT_3D ( 'NONE', #53901, #22060, #16061 ) ;
#11728 = ADVANCED_FACE ( 'NONE', ( #34096 ), #52123, .F. ) ;
#11729 = CYLINDRICAL_SURFACE ( 'NONE', #45564, 0.1999999999999987899 ) ;
#11730 = EDGE_CURVE ( 'NONE', #52010, #66616, #14997, .T. ) ;
#11731 = DIRECTION ( 'NONE',  ( 1.000000000000000000, 0.000000000000000000, 0.000000000000000000 ) ) ;
#11732 = VECTOR ( 'NONE', #60738, 1000.000000000000000 ) ;
#11733 = ADVANCED_FACE ( 'NONE', ( #36556 ), #35857, .F. ) ;
#11734 = ORIENTED_EDGE ( 'NONE', *, *, #64123, .F. ) ;
#11735 = VERTEX_POINT ( 'NONE', #46116 ) ;
#11736 = LINE ( 'NONE', #13832, #47760 ) ;
#11737 = EDGE_CURVE ( 'NONE', #13215, #25374, #15155, .T. ) ;
#11738 = ADVANCED_FACE ( 'NONE', ( #69085 ), #36203, .F. ) ;
#11739 = DIRECTION ( 'NONE',  ( 1.000000000000000000, -0.000000000000000000, 0.000000000000000000 ) ) ;
#11740 = ORIENTED_EDGE ( 'NONE', *, *, #29369, .T. ) ;
#11741 = VECTOR ( 'NONE', #45867, 1000.000000000000000 ) ;
#11742 = AXIS2_PLACEMENT_3D ( 'NONE', #65567, #32696, #48966 ) ;
#11743 = DIRECTION ( 'NONE',  ( 0.000000000000000000, 1.000000000000000000, 0.000000000000000000 ) ) ;
#11745 = ORIENTED_EDGE ( 'NONE', *, *, #5321, .F. ) ;
#11744 = LINE ( 'NONE', #37256, #50951 ) ;
#11746 = ORIENTED_EDGE ( 'NONE', *, *, #43729, .F. ) ;
#11747 = DIRECTION ( 'NONE',  ( -1.836970198721029934E-16, 1.836970198721036590E-16, -1.000000000000000000 ) ) ;
#11748 = CARTESIAN_POINT ( 'NONE',  ( -11.00000000000000000, -11.85423089348099879, 9.852125413066602277 ) ) ;
#11749 = STYLED_ITEM ( 'NONE', ( #44306 ), #66405 ) ;
#11750 = AXIS2_PLACEMENT_3D ( 'NONE', #45571, #36023, #51598 ) ;
#11751 = CARTESIAN_POINT ( 'NONE',  ( 283.0000000000000568, -38.64999999999999858, 12.69999999999999929 ) ) ;
#11752 = DIRECTION ( 'NONE',  ( -1.000000000000000000, 0.000000000000000000, 0.000000000000000000 ) ) ;
#11753 = CARTESIAN_POINT ( 'NONE',  ( -11.31351654964670850, 7.793516549646603231, 455.0000000000000568 ) ) ;
#11754 = AXIS2_PLACEMENT_3D ( 'NONE', #24061, #33637, #2149 ) ;
#11755 = ORIENTED_EDGE ( 'NONE', *, *, #11347, .F. ) ;
#11756 = CARTESIAN_POINT ( 'NONE',  ( 7.000000000000000000, -23.65000000000000568, -12.40000000000000213 ) ) ;
#11758 = ORIENTED_EDGE ( 'NONE', *, *, #14964, .T. ) ;
#11757 =( NAMED_UNIT ( * ) PLANE_ANGLE_UNIT ( ) SI_UNIT ( $, .RADIAN. ) );
#11759 = VECTOR ( 'NONE', #50795, 1000.000000000000000 ) ;
#11760 = CARTESIAN_POINT ( 'NONE',  ( 9.417013320880792904, -1.866219381641561759, 455.0000000000000568 ) ) ;
#11761 = FACE_OUTER_BOUND ( 'NONE', #18307, .T. ) ;
#11762 = PLANE ( 'NONE',  #58470 ) ;
#11763 = CIRCLE ( 'NONE', #1613, 2.204799999999998761 ) ;
#11764 = CARTESIAN_POINT ( 'NONE',  ( 2.765062094116059743, 9.942044687070495712, 195.0000000000000284 ) ) ;
#11765 = DIRECTION ( 'NONE',  ( 0.000000000000000000, -1.000000000000000000, 0.000000000000000000 ) ) ;
#11766 = ORIENTED_EDGE ( 'NONE', *, *, #1277, .F. ) ;
#11767 = VERTEX_POINT ( 'NONE', #14303 ) ;
#11768 = CARTESIAN_POINT ( 'NONE',  ( 23.75054448485400016, -15.50000000000000000, 25.53140320652400064 ) ) ;
#11769 = DIRECTION ( 'NONE',  ( 0.000000000000000000, -1.000000000000000000, 0.000000000000000000 ) ) ;
#11771 = EDGE_CURVE ( 'NONE', #3393, #21681, #24557, .T. ) ;
#11770 =( BOUNDED_CURVE ( )  B_SPLINE_CURVE ( 3, ( #28290, #43865, #39250, #38570 ),
 .UNSPECIFIED., .F., .F. ) 
 B_SPLINE_CURVE_WITH_KNOTS ( ( 4, 4 ),
 ( 2.293530574608309003, 2.418858405776377563 ),
 .UNSPECIFIED. ) 
 CURVE ( )  GEOMETRIC_REPRESENTATION_ITEM ( )  RATIONAL_B_SPLINE_CURVE ( ( 1.000000000000000000, 0.9986915061577686936, 0.9986915061577686936, 1.000000000000000000 ) ) 
 REPRESENTATION_ITEM ( '' )  );
#11772 = VERTEX_POINT ( 'NONE', #4404 ) ;
#11773 = DIRECTION ( 'NONE',  ( -0.7671651518153028704, -0.6414496315691537998, -2.587583378555113506E-16 ) ) ;
#11774 = DIRECTION ( 'NONE',  ( 1.000000000000000000, 0.000000000000000000, 0.000000000000000000 ) ) ;
#11775 = EDGE_CURVE ( 'NONE', #49332, #31165, #41860, .T. ) ;
#11776 = VERTEX_POINT ( 'NONE', #3336 ) ;
#11777 = CARTESIAN_POINT ( 'NONE',  ( 8.750000000000000000, -7.348062532928000934, 0.000000000000000000 ) ) ;
#11778 = DIRECTION ( 'NONE',  ( -0.000000000000000000, -0.000000000000000000, -1.000000000000000000 ) ) ;
#11779 = ORIENTED_EDGE ( 'NONE', *, *, #41450, .T. ) ;
#11780 = DIRECTION ( 'NONE',  ( 0.000000000000000000, -0.7071067811865474617, 0.7071067811865474617 ) ) ;
#11781 = AXIS2_PLACEMENT_3D ( 'NONE', #21880, #16227, #48064 ) ;
#11782 = DIRECTION ( 'NONE',  ( -4.121462285523434458E-16, -1.000000000000000000, 0.000000000000000000 ) ) ;
#11783 = CARTESIAN_POINT ( 'NONE',  ( 2.706483450353370124, 10.08346604330780671, 195.0000000000000284 ) ) ;
#11784 = DIRECTION ( 'NONE',  ( 0.000000000000000000, 1.000000000000000000, 0.000000000000000000 ) ) ;
#11785 = ORIENTED_EDGE ( 'NONE', *, *, #9205, .T. ) ;
#11787 = ORIENTED_EDGE ( 'NONE', *, *, #51834, .F. ) ;
#11786 = LINE ( 'NONE', #32338, #61041 ) ;
#11788 = AXIS2_PLACEMENT_3D ( 'NONE', #46556, #68498, #14034 ) ;
#11789 = AXIS2_PLACEMENT_3D ( 'NONE', #13115, #18069, #55565 ) ;
#11790 = DIRECTION ( 'NONE',  ( -1.000000000000000000, 0.000000000000000000, 0.000000000000000000 ) ) ;
#11791 = LINE ( 'NONE', #64185, #17639 ) ;
#11792 = FACE_OUTER_BOUND ( 'NONE', #42416, .T. ) ;
#11793 = VERTEX_POINT ( 'NONE', #19946 ) ;
#11794 = DIRECTION ( 'NONE',  ( 0.7671651518152962090, 0.6414496315691619044, 2.356647714346269254E-16 ) ) ;
#11795 = VECTOR ( 'NONE', #56920, 1000.000000000000000 ) ;
#11796 = DIRECTION ( 'NONE',  ( 0.000000000000000000, 1.000000000000000000, -0.000000000000000000 ) ) ;
#11797 = VECTOR ( 'NONE', #33344, 999.9999999999998863 ) ;
#11798 = VERTEX_POINT ( 'NONE', #57424 ) ;
#11799 = VERTEX_POINT ( 'NONE', #67684 ) ;
#11801 = VERTEX_POINT ( 'NONE', #8981 ) ;
#11800 = VECTOR ( 'NONE', #9123, 1000.000000000000000 ) ;
#11802 = CARTESIAN_POINT ( 'NONE',  ( 30.00000000000000000, -11.50000000000082068, -10.20500000000000007 ) ) ;
#11803 = FACE_OUTER_BOUND ( 'NONE', #34134, .T. ) ;
#11804 = DIRECTION ( 'NONE',  ( 0.000000000000000000, 1.000000000000000000, 0.000000000000000000 ) ) ;
#11805 = EDGE_CURVE ( 'NONE', #65042, #64711, #30556, .T. ) ;
#11806 = AXIS2_PLACEMENT_3D ( 'NONE', #7130, #49256, #32983 ) ;
#11807 = EDGE_LOOP ( 'NONE', ( #48408, #56240, #6951, #54060 ) ) ;
#11808 = EDGE_LOOP ( 'NONE', ( #843, #20089, #24473, #15328 ) ) ;
#11809 = ORIENTED_EDGE ( 'NONE', *, *, #49962, .T. ) ;
#11810 = AXIS2_PLACEMENT_3D ( 'NONE', #2418, #7015, #12657 ) ;
#11811 = DIRECTION ( 'NONE',  ( -5.981805089575196197E-17, -1.000000000000000000, 0.000000000000000000 ) ) ;
#11812 = EDGE_CURVE ( 'NONE', #25369, #61156, #39996, .T. ) ;
#11813 = VERTEX_POINT ( 'NONE', #68035 ) ;
#11814 = VERTEX_POINT ( 'NONE', #14643 ) ;
#11815 = ORIENTED_EDGE ( 'NONE', *, *, #8381, .T. ) ;
#11816 = ORIENTED_EDGE ( 'NONE', *, *, #64569, .F. ) ;
#11817 = DIRECTION ( 'NONE',  ( 1.000000000000000000, 0.000000000000000000, 0.000000000000000000 ) ) ;
#11818 = ADVANCED_FACE ( 'NONE', ( #46460 ), #25966, .T. ) ;
#11819 = ADVANCED_FACE ( 'NONE', ( #41154 ), #63082, .F. ) ;
#11821 = ORIENTED_EDGE ( 'NONE', *, *, #37564, .T. ) ;
#11820 = DIRECTION ( 'NONE',  ( 1.836970198721029934E-16, 1.836970198721010706E-16, -1.000000000000000000 ) ) ;
#11822 = DIRECTION ( 'NONE',  ( -0.7071067811865446862, 0.7071067811865503483, 0.000000000000000000 ) ) ;
#11823 = DIRECTION ( 'NONE',  ( 0.000000000000000000, 3.673940397442059868E-16, -1.000000000000000000 ) ) ;
#11824 = EDGE_CURVE ( 'NONE', #59587, #29192, #40811, .T. ) ;
#11825 = LINE ( 'NONE', #22462, #14376 ) ;
#11826 = VECTOR ( 'NONE', #54088, 1000.000000000000000 ) ;
#11827 = VERTEX_POINT ( 'NONE', #30909 ) ;
#11828 = AXIS2_PLACEMENT_3D ( 'NONE', #64939, #26765, #48329 ) ;
#11829 = LINE ( 'NONE', #37426, #52023 ) ;
#11830 = LINE ( 'NONE', #60962, #10848 ) ;
#11831 = DIRECTION ( 'NONE',  ( 0.000000000000000000, 1.000000000000000000, 0.000000000000000000 ) ) ;
#11832 = ORIENTED_EDGE ( 'NONE', *, *, #41158, .F. ) ;
#11833 = CARTESIAN_POINT ( 'NONE',  ( 6.836383711242975281, 4.135079735113102117, 54.00000000000000711 ) ) ;
#11834 = VECTOR ( 'NONE', #20130, 1000.000000000000000 ) ;
#11836 = CARTESIAN_POINT ( 'NONE',  ( 7.250000000000005329, 7.250000000000000888, -14.50000000000000000 ) ) ;
#11835 = CIRCLE ( 'NONE', #34385, 2.215251240775983899 ) ;
#11837 = DIRECTION ( 'NONE',  ( 1.000000000000000000, -0.000000000000000000, -0.000000000000000000 ) ) ;
#11838 = ORIENTED_EDGE ( 'NONE', *, *, #50731, .T. ) ;
#11839 = CYLINDRICAL_SURFACE ( 'NONE', #59566, 0.1749999999999998224 ) ;
#11840 = VECTOR ( 'NONE', #27898, 1000.000000000000000 ) ;
#11841 = PLANE ( 'NONE',  #34166 ) ;
#11842 = CARTESIAN_POINT ( 'NONE',  ( 6.006483450353401921, 5.993516549646582092, 455.0000000000000568 ) ) ;
#11843 = CIRCLE ( 'NONE', #53674, 0.5000000000009284795 ) ;
#11844 = DIRECTION ( 'NONE',  ( -0.7071067811865480168, 0.7071067811865470176, 0.000000000000000000 ) ) ;
#11845 = DIRECTION ( 'NONE',  ( 0.000000000000000000, 0.000000000000000000, -1.000000000000000000 ) ) ;
#11846 = CYLINDRICAL_SURFACE ( 'NONE', #5713, 0.3500000000002719824 ) ;
#11847 = DIRECTION ( 'NONE',  ( 0.000000000000000000, -1.000000000000000000, 0.000000000000000000 ) ) ;
#11848 = FACE_OUTER_BOUND ( 'NONE', #57987, .T. ) ;
#11849 = STYLED_ITEM ( 'NONE', ( #52212 ), #44181 ) ;
#11850 = ORIENTED_EDGE ( 'NONE', *, *, #931, .T. ) ;
#11851 = AXIS2_PLACEMENT_3D ( 'NONE', #43932, #66539, #12099 ) ;
#11852 = DIRECTION ( 'NONE',  ( -1.047444401652940007E-14, -1.000000000000000000, -1.836970198721029934E-16 ) ) ;
#11853 = LINE ( 'NONE', #59959, #9344 ) ;
#11854 = ADVANCED_FACE ( 'NONE', ( #19243 ), #4046, .F. ) ;
#11855 = VECTOR ( 'NONE', #24106, 1000.000000000000000 ) ;
#11856 = EDGE_CURVE ( 'NONE', #60174, #56003, #35491, .T. ) ;
#11857 = EDGE_CURVE ( 'NONE', #41912, #58770, #37967, .T. ) ;
#11858 = DIRECTION ( 'NONE',  ( 1.000000000000000000, 0.000000000000000000, 0.000000000000000000 ) ) ;
#11859 = CARTESIAN_POINT ( 'NONE',  ( -11.31351654964670850, 4.193516549646605363, 195.0000000000000284 ) ) ;
#11860 = ORIENTED_EDGE ( 'NONE', *, *, #37158, .T. ) ;
#11861 = CARTESIAN_POINT ( 'NONE',  ( 15.00000000000000000, -25.60000000000000142, 15.10000000000000142 ) ) ;
#11862 = CARTESIAN_POINT ( 'NONE',  ( -7.813516549646711162, 11.99351654964660341, 455.0000000000000568 ) ) ;
#11863 = DIRECTION ( 'NONE',  ( 1.000000000000000000, -0.000000000000000000, 0.000000000000000000 ) ) ;
#11864 = ADVANCED_FACE ( 'NONE', ( #64837 ), #32310, .F. ) ;
#11865 = LINE ( 'NONE', #1605, #19583 ) ;
#11866 = LINE ( 'NONE', #43720, #49753 ) ;
#11867 = ORIENTED_EDGE ( 'NONE', *, *, #65444, .F. ) ;
#11868 = DIRECTION ( 'NONE',  ( -1.794541526872559352E-16, -1.000000000000000000, 0.000000000000000000 ) ) ;
#11869 = CARTESIAN_POINT ( 'NONE',  ( 49.00000000000000000, -0.1999999999911795112, 8.826273045769999343E-12 ) ) ;
#11870 = ORIENTED_EDGE ( 'NONE', *, *, #35587, .F. ) ;
#11871 = DIRECTION ( 'NONE',  ( -0.7071067811865530128, -0.7071067811865421326, 0.000000000000000000 ) ) ;
#11872 = VECTOR ( 'NONE', #40030, 1000.000000000000000 ) ;
#11873 = EDGE_LOOP ( 'NONE', ( #52247, #4941, #63653, #25312 ) ) ;
#11874 = VECTOR ( 'NONE', #33180, 1000.000000000000000 ) ;
#11875 = DIRECTION ( 'NONE',  ( -1.000000000000000000, 0.000000000000000000, 0.000000000000000000 ) ) ;
#11876 = ORIENTED_EDGE ( 'NONE', *, *, #10780, .T. ) ;
#11877 = ORIENTED_EDGE ( 'NONE', *, *, #58771, .F. ) ;
#11878 = FACE_OUTER_BOUND ( 'NONE', #61935, .T. ) ;
#11879 = ORIENTED_EDGE ( 'NONE', *, *, #34876, .F. ) ;
#11880 = DIRECTION ( 'NONE',  ( 8.612436249475772606E-15, 1.000000000000000000, 0.000000000000000000 ) ) ;
#11881 = CARTESIAN_POINT ( 'NONE',  ( -11.99351654964671354, 4.173516549646604901, 455.0000000000000568 ) ) ;
#11882 = LINE ( 'NONE', #27473, #57331 ) ;
#11883 = VECTOR ( 'NONE', #11820, 1000.000000000000000 ) ;
#11884 = VECTOR ( 'NONE', #17592, 1000.000000000000000 ) ;
#11885 = VECTOR ( 'NONE', #31419, 1000.000000000000000 ) ;
#11886 = ORIENTED_EDGE ( 'NONE', *, *, #55303, .F. ) ;
#11887 = ORIENTED_EDGE ( 'NONE', *, *, #25616, .T. ) ;
#11888 = CARTESIAN_POINT ( 'NONE',  ( 289.5000000000000000, -42.50000000000000000, 26.50000000000000000 ) ) ;
#11889 = CARTESIAN_POINT ( 'NONE',  ( 4.406483450353373854, 11.77351654964663119, 195.0000000000000284 ) ) ;
#11890 = CIRCLE ( 'NONE', #54820, 0.2999999999998732569 ) ;
#11891 = ORIENTED_EDGE ( 'NONE', *, *, #22371, .T. ) ;
#11892 = VERTEX_POINT ( 'NONE', #4740 ) ;
#11893 = ORIENTED_EDGE ( 'NONE', *, *, #14237, .T. ) ;
#11894 = VECTOR ( 'NONE', #2688, 1000.000000000000000 ) ;
#11895 = DIRECTION ( 'NONE',  ( 0.000000000000000000, -1.000000000000000000, 0.000000000000000000 ) ) ;
#11897 = VERTEX_POINT ( 'NONE', #53535 ) ;
#11896 = DIRECTION ( 'NONE',  ( 0.000000000000000000, 0.000000000000000000, -1.000000000000000000 ) ) ;
#11898 = EDGE_CURVE ( 'NONE', #19769, #5145, #37618, .T. ) ;
#11899 = LINE ( 'NONE', #43755, #49234 ) ;
#11900 = CARTESIAN_POINT ( 'NONE',  ( 11.12648345035337627, -9.106483450353398013, 195.0000000000000284 ) ) ;
#11901 = EDGE_CURVE ( 'NONE', #47075, #35171, #12893, .T. ) ;
#11902 = EDGE_LOOP ( 'NONE', ( #43252, #26275, #6539, #29501 ) ) ;
#11903 = EDGE_CURVE ( 'NONE', #53683, #49071, #36643, .T. ) ;
#11904 = VERTEX_POINT ( 'NONE', #10731 ) ;
#11905 = AXIS2_PLACEMENT_3D ( 'NONE', #50559, #66805, #19073 ) ;
#11906 = EDGE_CURVE ( 'NONE', #34995, #8213, #69437, .T. ) ;
#11907 = CARTESIAN_POINT ( 'NONE',  ( 9.955011587777271131, 9.234937905883876752, 455.0000000000000568 ) ) ;
#11908 = CARTESIAN_POINT ( 'NONE',  ( -8.697938382363135545, 8.079219948824830411, 26.00000000000000711 ) ) ;
#11909 = EDGE_CURVE ( 'NONE', #53055, #37771, #44498, .T. ) ;
#11910 = EDGE_CURVE ( 'NONE', #28718, #69443, #20994, .T. ) ;
#11911 = DIRECTION ( 'NONE',  ( 0.000000000000000000, -1.000000000000000000, 0.000000000000000000 ) ) ;
#11912 = FACE_OUTER_BOUND ( 'NONE', #48879, .T. ) ;
#11913 = AXIS2_PLACEMENT_3D ( 'NONE', #16473, #65599, #32722 ) ;
#11915 = ORIENTED_EDGE ( 'NONE', *, *, #58013, .T. ) ;
#11914 = DIRECTION ( 'NONE',  ( 0.000000000000000000, 0.000000000000000000, -1.000000000000000000 ) ) ;
#11916 = VERTEX_POINT ( 'NONE', #31961 ) ;
#11917 = LINE ( 'NONE', #43776, #52072 ) ;
#11918 = PLANE ( 'NONE',  #28475 ) ;
#11919 = AXIS2_PLACEMENT_3D ( 'NONE', #20411, #3800, #52602 ) ;
#11920 = CARTESIAN_POINT ( 'NONE',  ( 15.50000000000000000, -15.50000000000000000, -25.99999999999985079 ) ) ;
#11921 = CARTESIAN_POINT ( 'NONE',  ( -6.331612867284154511, 8.393516549646601987, 455.0000000000000568 ) ) ;
#11922 = CIRCLE ( 'NONE', #28830, 4.500000000000190958 ) ;
#11923 = FACE_OUTER_BOUND ( 'NONE', #1533, .T. ) ;
#11924 = VERTEX_POINT ( 'NONE', #6128 ) ;
#11925 = PLANE ( 'NONE',  #65166 ) ;
#11926 = CARTESIAN_POINT ( 'NONE',  ( -9.942044687070668019, -9.247904806590694804, 455.0000000000000568 ) ) ;
#11927 = LINE ( 'NONE', #61773, #46946 ) ;
#11928 = CARTESIAN_POINT ( 'NONE',  ( 12.00000000000000000, 11.18999999999999950, -5.000000000000000000 ) ) ;
#11929 = VECTOR ( 'NONE', #39761, 1000.000000000000000 ) ;
#11930 = AXIS2_PLACEMENT_3D ( 'NONE', #45291, #61552, #13121 ) ;
#11931 = CARTESIAN_POINT ( 'NONE',  ( 6.364920264886851697, 3.663616288756991413, 54.00000000000000711 ) ) ;
#11932 = DIRECTION ( 'NONE',  ( 0.000000000000000000, 0.000000000000000000, 1.000000000000000000 ) ) ;
#11933 = AXIS2_PLACEMENT_3D ( 'NONE', #12997, #23967, #45525 ) ;
#11934 = AXIS2_PLACEMENT_3D ( 'NONE', #67200, #24065, #35723 ) ;
#11935 = CARTESIAN_POINT ( 'NONE',  ( -14.10805890929250062, -5.000000000000000000, -26.25000000000000000 ) ) ;
#11936 = ORIENTED_EDGE ( 'NONE', *, *, #64151, .F. ) ;
#11937 = LINE ( 'NONE', #38157, #35457 ) ;
#11938 = CARTESIAN_POINT ( 'NONE',  ( 283.0000000000000568, -42.50000000000000000, 7.500000000000000000 ) ) ;
#11939 = VERTEX_POINT ( 'NONE', #48572 ) ;
#11940 = CYLINDRICAL_SURFACE ( 'NONE', #35680, 0.3499999999999996447 ) ;
#11941 = CARTESIAN_POINT ( 'NONE',  ( 9.955011587777271131, 9.234937905883876752, 455.0000000000000568 ) ) ;
#11942 = VECTOR ( 'NONE', #26722, 1000.000000000000000 ) ;
#11943 = DIRECTION ( 'NONE',  ( -0.000000000000000000, 0.000000000000000000, -1.000000000000000000 ) ) ;
#11944 = CARTESIAN_POINT ( 'NONE',  ( 4.201500623656003519, -7.272650909786698037, 455.0000000000000568 ) ) ;
#11945 = DIRECTION ( 'NONE',  ( -0.000000000000000000, -0.000000000000000000, 1.000000000000000000 ) ) ;
#11946 = LINE ( 'NONE', #1692, #21852 ) ;
#11947 = CIRCLE ( 'NONE', #18724, 24.99999999998794920 ) ;
#11948 = ORIENTED_EDGE ( 'NONE', *, *, #13761, .F. ) ;
#11949 = CARTESIAN_POINT ( 'NONE',  ( 1.090483450353418426, 10.73351654964659829, 455.0000000000000568 ) ) ;
#11950 = ORIENTED_EDGE ( 'NONE', *, *, #18982, .T. ) ;
#11951 = LINE ( 'NONE', #64678, #6555 ) ;
#11952 = ADVANCED_FACE ( 'NONE', ( #16387 ), #42566, .F. ) ;
#11953 = CARTESIAN_POINT ( 'NONE',  ( 6.358413763958968623, -4.720772854004790631, 54.00000000000000711 ) ) ;
#11954 = EDGE_CURVE ( 'NONE', #39907, #1200, #43605, .T. ) ;
#11955 = CYLINDRICAL_SURFACE ( 'NONE', #2788, 0.1749999999999998224 ) ;
#11956 = VERTEX_POINT ( 'NONE', #54231 ) ;
#11957 = ORIENTED_EDGE ( 'NONE', *, *, #51736, .T. ) ;
#11958 = DIRECTION ( 'NONE',  ( 0.000000000000000000, 0.000000000000000000, 1.000000000000000000 ) ) ;
#11959 = ORIENTED_EDGE ( 'NONE', *, *, #65744, .F. ) ;
#11960 = ORIENTED_EDGE ( 'NONE', *, *, #27842, .T. ) ;
#11961 = PRODUCT_DEFINITION_CONTEXT ( 'detailed design', #12833, 'design' ) ;
#11962 = DIRECTION ( 'NONE',  ( 0.000000000000000000, 0.000000000000000000, -1.000000000000000000 ) ) ;
#11963 = DIRECTION ( 'NONE',  ( -5.163402228214836012E-15, -1.000000000000000000, -1.836970198721026976E-16 ) ) ;
#11964 = FACE_OUTER_BOUND ( 'NONE', #13269, .T. ) ;
#11965 = EDGE_CURVE ( 'NONE', #67463, #40219, #5790, .T. ) ;
#11966 = AXIS2_PLACEMENT_3D ( 'NONE', #22730, #22398, #32999 ) ;
#11967 = ORIENTED_EDGE ( 'NONE', *, *, #13894, .T. ) ;
#11968 = CARTESIAN_POINT ( 'NONE',  ( 30.00000000000000000, -17.14999999999900027, 26.64999999999900027 ) ) ;
#11970 = CARTESIAN_POINT ( 'NONE',  ( 7.250000000000005329, 7.250000000000000888, -11.00000000000000000 ) ) ;
#11969 = CARTESIAN_POINT ( 'NONE',  ( -11.11351654964671098, 7.793516549646603231, 195.0000000000000284 ) ) ;
#11971 = ORIENTED_EDGE ( 'NONE', *, *, #53810, .F. ) ;
#11973 = ORIENTED_EDGE ( 'NONE', *, *, #37002, .F. ) ;
#11972 = LINE ( 'NONE', #61827, #43293 ) ;
#11974 = ORIENTED_EDGE ( 'NONE', *, *, #17667, .T. ) ;
#11975 = EDGE_CURVE ( 'NONE', #48554, #69020, #52455, .T. ) ;
#11976 = DIRECTION ( 'NONE',  ( 0.000000000000000000, 0.000000000000000000, 1.000000000000000000 ) ) ;
#11977 = AXIS2_PLACEMENT_3D ( 'NONE', #53094, #69701, #69335 ) ;
#11978 = CYLINDRICAL_SURFACE ( 'NONE', #50254, 0.3999999999999993006 ) ;
#11979 = AXIS2_PLACEMENT_3D ( 'NONE', #28031, #16378, #43933 ) ;
#11980 = CIRCLE ( 'NONE', #38016, 25.39999999999999858 ) ;
#11981 = AXIS2_PLACEMENT_3D ( 'NONE', #50177, #13391, #33907 ) ;
#11982 = FACE_OUTER_BOUND ( 'NONE', #44677, .T. ) ;
#11983 = EDGE_CURVE ( 'NONE', #18841, #58583, #38857, .T. ) ;
#11984 = ORIENTED_EDGE ( 'NONE', *, *, #7650, .F. ) ;
#11985 = VERTEX_POINT ( 'NONE', #38312 ) ;
#11986 = AXIS2_PLACEMENT_3D ( 'NONE', #12105, #54917, #26997 ) ;
#11987 = VECTOR ( 'NONE', #7964, 1000.000000000000000 ) ;
#11988 = VECTOR ( 'NONE', #52716, 1000.000000000000000 ) ;
#11989 = FACE_OUTER_BOUND ( 'NONE', #2280, .T. ) ;
#11990 = CARTESIAN_POINT ( 'NONE',  ( 283.0000000000000568, -38.15000000000000568, 13.19999999999999929 ) ) ;
#11991 = EDGE_LOOP ( 'NONE', ( #36528, #137, #32596, #14612 ) ) ;
#11992 = CARTESIAN_POINT ( 'NONE',  ( 7.000000000000000000, -25.60000000000000142, -15.10000000000000142 ) ) ;
#11994 = AXIS2_PLACEMENT_3D ( 'NONE', #2094, #6698, #43841 ) ;
#11993 = CARTESIAN_POINT ( 'NONE',  ( 14.89999999999999680, -14.06939075806900874, 20.80000000000001137 ) ) ;
#11995 = EDGE_CURVE ( 'NONE', #35620, #53694, #59868, .T. ) ;
#11996 = LINE ( 'NONE', #33236, #47480 ) ;
#11997 = ORIENTED_EDGE ( 'NONE', *, *, #65563, .F. ) ;
#11998 = EDGE_CURVE ( 'NONE', #23009, #39317, #32998, .T. ) ;
#11999 = CIRCLE ( 'NONE', #44753, 1.929199999999998916 ) ;
#12000 = CARTESIAN_POINT ( 'NONE',  ( 11.00000000000000000, -16.28999999999999915, 14.50000000000000000 ) ) ;
#12001 = CARTESIAN_POINT ( 'NONE',  ( -9.293516549646771097, -10.09643294401451108, 195.0000000000000284 ) ) ;
#12002 = ORIENTED_EDGE ( 'NONE', *, *, #60929, .T. ) ;
#12004 = ORIENTED_EDGE ( 'NONE', *, *, #61631, .T. ) ;
#12003 = CARTESIAN_POINT ( 'NONE',  ( -5.242976262117280406, -5.257023737882805747, 54.00000000000000711 ) ) ;
#12005 = CARTESIAN_POINT ( 'NONE',  ( 7.500000000000000000, -20.49999999999999645, -20.00000000000000000 ) ) ;
#12006 = CARTESIAN_POINT ( 'NONE',  ( 6.006483450353379716, -6.006483450353394815, 195.0000000000000284 ) ) ;
#12007 = EDGE_CURVE ( 'NONE', #37330, #66031, #49272, .T. ) ;
#12008 = DIRECTION ( 'NONE',  ( 8.339399738404099512E-15, 1.000000000000000000, 1.836970198721025990E-16 ) ) ;
#12009 = CARTESIAN_POINT ( 'NONE',  ( 0.000000000000000000, 8.250000000000001776, -10.50000000000000000 ) ) ;
#12010 = PLANE ( 'NONE',  #31718 ) ;
#12011 = DIRECTION ( 'NONE',  ( -1.000000000000000000, 0.000000000000000000, 0.000000000000000000 ) ) ;
#12012 = VERTEX_POINT ( 'NONE', #21351 ) ;
#12013 = DIRECTION ( 'NONE',  ( -1.000000000000000000, 0.000000000000000000, 0.000000000000000000 ) ) ;
#12014 = LINE ( 'NONE', #29672, #25460 ) ;
#12016 = EDGE_LOOP ( 'NONE', ( #49529, #65574, #33024, #41497 ) ) ;
#12015 = DIRECTION ( 'NONE',  ( -0.7071067811865560104, -0.7071067811865391350, -2.597868168706466792E-16 ) ) ;
#12017 = DIRECTION ( 'NONE',  ( 0.000000000000000000, 0.000000000000000000, -1.000000000000000000 ) ) ;
#12018 = COLOUR_RGB ( '', 0.72549020, 0.75294118, 0.79215686) ;
#12019 = DIRECTION ( 'NONE',  ( 0.000000000000000000, 0.000000000000000000, 1.000000000000000000 ) ) ;
#12020 = CIRCLE ( 'NONE', #51567, 4.500000000000190958 ) ;
#12021 = ORIENTED_EDGE ( 'NONE', *, *, #58524, .T. ) ;
#12022 = FACE_OUTER_BOUND ( 'NONE', #45937, .T. ) ;
#12023 = CARTESIAN_POINT ( 'NONE',  ( -5.993516549646776603, -6.006483450353426790, 455.0000000000000568 ) ) ;
#12024 = ORIENTED_EDGE ( 'NONE', *, *, #38961, .T. ) ;
#12025 = EDGE_CURVE ( 'NONE', #26490, #32586, #845, .T. ) ;
#12026 = CARTESIAN_POINT ( 'NONE',  ( 6.364920264886851697, 3.663616288756991413, 54.00000000000000711 ) ) ;
#12027 = LINE ( 'NONE', #38246, #19100 ) ;
#12028 = VECTOR ( 'NONE', #34972, 1000.000000000000000 ) ;
#12029 = VECTOR ( 'NONE', #10984, 999.9999999999998863 ) ;
#12030 = CARTESIAN_POINT ( 'NONE',  ( -28.00000000000000000, -15.50000000000000000, -20.05051025721700242 ) ) ;
#12031 = DIRECTION ( 'NONE',  ( -1.000000000000000000, 0.000000000000000000, 0.000000000000000000 ) ) ;
#12032 = ADVANCED_FACE ( 'NONE', ( #33680 ), #17417, .F. ) ;
#12033 = VECTOR ( 'NONE', #45782, 1000.000000000000000 ) ;
#12035 = CARTESIAN_POINT ( 'NONE',  ( 11.78648345035337819, -7.826483450353395988, 195.0000000000000284 ) ) ;
#12034 = AXIS2_PLACEMENT_3D ( 'NONE', #27577, #38209, #59060 ) ;
#12036 = ORIENTED_EDGE ( 'NONE', *, *, #3622, .F. ) ;
#12037 = AXIS2_PLACEMENT_3D ( 'NONE', #23546, #18234, #35541 ) ;
#12038 = DIRECTION ( 'NONE',  ( -1.000000000000000000, 0.000000000000000000, 0.000000000000000000 ) ) ;
#12039 = ORIENTED_EDGE ( 'NONE', *, *, #33950, .T. ) ;
#12040 = EDGE_CURVE ( 'NONE', #60221, #26009, #12442, .T. ) ;
#12041 = EDGE_LOOP ( 'NONE', ( #60548, #32152 ) ) ;
#12042 = CARTESIAN_POINT ( 'NONE',  ( 280.0000000000000000, -25.60000000000000142, -20.00000000000000000 ) ) ;
#12044 = DIRECTION ( 'NONE',  ( -1.260948829465470062E-14, -1.000000000000000000, -1.836970198721033878E-16 ) ) ;
#12043 = VECTOR ( 'NONE', #58744, 1000.000000000000000 ) ;
#12045 = AXIS2_PLACEMENT_3D ( 'NONE', #21476, #49049, #60329 ) ;
#12046 = EDGE_CURVE ( 'NONE', #51332, #67088, #66212, .T. ) ;
#12047 = VECTOR ( 'NONE', #18608, 1000.000000000000000 ) ;
#12048 = CARTESIAN_POINT ( 'NONE',  ( 30.00000000000000000, -16.64230188589299786, 14.64519951917100116 ) ) ;
#12049 = EDGE_CURVE ( 'NONE', #36255, #37762, #55602, .T. ) ;
#12050 = DIRECTION ( 'NONE',  ( 0.000000000000000000, 0.000000000000000000, -1.000000000000000000 ) ) ;
#12051 = ORIENTED_EDGE ( 'NONE', *, *, #3869, .F. ) ;
#12052 = ORIENTED_EDGE ( 'NONE', *, *, #17117, .F. ) ;
#12054 = ORIENTED_EDGE ( 'NONE', *, *, #58713, .T. ) ;
#12053 = LINE ( 'NONE', #51280, #27273 ) ;
#12055 = ORIENTED_EDGE ( 'NONE', *, *, #69952, .T. ) ;
#12056 = PRODUCT_DEFINITION_SHAPE ( 'NONE', 'NONE',  #69983 ) ;
#12057 = VECTOR ( 'NONE', #57410, 1000.000000000000000 ) ;
#12058 = CARTESIAN_POINT ( 'NONE',  ( -11.11351654964674118, -4.206483450353336373, 455.0000000000000568 ) ) ;
#12059 = FACE_OUTER_BOUND ( 'NONE', #50767, .T. ) ;
#12060 = CARTESIAN_POINT ( 'NONE',  ( 0.000000000000000000, -0.5000000000000000000, 26.50000000000000000 ) ) ;
#12061 = EDGE_CURVE ( 'NONE', #20506, #48716, #14019, .T. ) ;
#12062 = ADVANCED_FACE ( 'NONE', ( #39334 ), #2202, .T. ) ;
#12063 = CARTESIAN_POINT ( 'NONE',  ( 41.09999999999999432, -14.06939075806901940, -20.80000000000000426 ) ) ;
#12065 = LINE ( 'NONE', #66505, #22164 ) ;
#12064 = CARTESIAN_POINT ( 'NONE',  ( -11.77351654964670935, 7.813516549646603693, 455.0000000000000568 ) ) ;
#12066 = ORIENTED_EDGE ( 'NONE', *, *, #48311, .T. ) ;
#12069 = ADVANCED_FACE ( 'NONE', ( #34354 ), #28719, .T. ) ;
#12068 = ORIENTED_EDGE ( 'NONE', *, *, #19552, .F. ) ;
#12067 = CARTESIAN_POINT ( 'NONE',  ( -17.00000000000000000, -15.50000000000000000, -19.33772233983200195 ) ) ;
#12070 = ORIENTED_EDGE ( 'NONE', *, *, #40004, .T. ) ;
#12071 = ORIENTED_EDGE ( 'NONE', *, *, #26359, .T. ) ;
#12072 = ADVANCED_FACE ( 'NONE', ( #12112 ), #60202, .T. ) ;
#12073 = EDGE_CURVE ( 'NONE', #30271, #22374, #28374, .T. ) ;
#12074 = CARTESIAN_POINT ( 'NONE',  ( 275.2500000000000000, -42.25000000000000000, -26.75000000000000000 ) ) ;
#12075 = ADVANCED_FACE ( 'NONE', ( #65857 ), #1857, .T. ) ;
#12076 = DIRECTION ( 'NONE',  ( 0.000000000000000000, -1.000000000000000000, 0.000000000000000000 ) ) ;
#12077 = DIRECTION ( 'NONE',  ( 0.000000000000000000, 0.000000000000000000, 1.000000000000000000 ) ) ;
#12078 = ORIENTED_EDGE ( 'NONE', *, *, #9153, .T. ) ;
#12079 = VECTOR ( 'NONE', #24910, 1000.000000000000000 ) ;
#12080 = VERTEX_POINT ( 'NONE', #23428 ) ;
#12081 = FACE_OUTER_BOUND ( 'NONE', #69531, .T. ) ;
#12082 = CARTESIAN_POINT ( 'NONE',  ( 7.250000000000005329, -7.449999999999998401, -23.00000000000000000 ) ) ;
#12083 = ORIENTED_EDGE ( 'NONE', *, *, #27905, .T. ) ;
#12084 = ORIENTED_EDGE ( 'NONE', *, *, #6452, .F. ) ;
#12085 = CIRCLE ( 'NONE', #15498, 1.399999999999999245 ) ;
#12087 = DIRECTION ( 'NONE',  ( 0.000000000000000000, -0.5625376724249369076, -0.8267716535433071723 ) ) ;
#12086 = AXIS2_PLACEMENT_3D ( 'NONE', #2099, #51230, #24364 ) ;
#12088 = EDGE_CURVE ( 'NONE', #21685, #55203, #62570, .T. ) ;
#12089 = CARTESIAN_POINT ( 'NONE',  ( -10.30047626211725742, 6.835476262117182955, 54.00000000000000711 ) ) ;
#12090 = ORIENTED_EDGE ( 'NONE', *, *, #1527, .T. ) ;
#12091 = EDGE_CURVE ( 'NONE', #29737, #21069, #63766, .T. ) ;
#12092 = CIRCLE ( 'NONE', #13250, 1.620999999999997332 ) ;
#12093 = VECTOR ( 'NONE', #48989, 1000.000000000000000 ) ;
#12094 = AXIS2_PLACEMENT_3D ( 'NONE', #33564, #64800, #49826 ) ;
#12095 = CARTESIAN_POINT ( 'NONE',  ( -7.750000000000001776, 7.750000000000001776, -5.000000000000000000 ) ) ;
#12097 = EDGE_LOOP ( 'NONE', ( #21215, #41794, #25137, #64434 ) ) ;
#12096 = LINE ( 'NONE', #61210, #13699 ) ;
#12098 = VERTEX_POINT ( 'NONE', #66553 ) ;
#12099 = DIRECTION ( 'NONE',  ( -1.000000000000000000, 0.000000000000000000, 0.000000000000000000 ) ) ;
#12100 = AXIS2_PLACEMENT_3D ( 'NONE', #7926, #62726, #19595 ) ;
#12101 = CARTESIAN_POINT ( 'NONE',  ( -9.547976262117217061, -2.369523737882723857, 26.00000000000000711 ) ) ;
#12102 = AXIS2_PLACEMENT_3D ( 'NONE', #59044, #10953, #21561 ) ;
#12103 = CARTESIAN_POINT ( 'NONE',  ( -3.667976262117228714, 9.722976262117169810, 54.00000000000000711 ) ) ;
#12104 = DIRECTION ( 'NONE',  ( -1.000000000000000000, 0.000000000000000000, 0.000000000000000000 ) ) ;
#12105 = CARTESIAN_POINT ( 'NONE',  ( -5.242976262117259978, 5.242976262117182706, 54.00000000000000711 ) ) ;
#12106 = DIRECTION ( 'NONE',  ( 0.000000000000000000, 0.000000000000000000, -1.000000000000000000 ) ) ;
#12107 = ORIENTED_EDGE ( 'NONE', *, *, #14629, .T. ) ;
#12108 = CARTESIAN_POINT ( 'NONE',  ( -7.798499376344067535, 7.259684009079840017, 455.0000000000000568 ) ) ;
#12110 = VERTEX_POINT ( 'NONE', #18104 ) ;
#12109 = DIRECTION ( 'NONE',  ( 0.000000000000000000, 1.000000000000000000, 3.673940397442059868E-16 ) ) ;
#12111 = VECTOR ( 'NONE', #63616, 1000.000000000000000 ) ;
#12112 = FACE_OUTER_BOUND ( 'NONE', #65033, .T. ) ;
#12113 = DIRECTION ( 'NONE',  ( 0.000000000000000000, 0.9760787414516886029, 0.2174173187353931058 ) ) ;
#12114 = LINE ( 'NONE', #27357, #61869 ) ;
#12115 = CARTESIAN_POINT ( 'NONE',  ( 7.000000000000000000, -25.69999999999924967, 14.52500000000000213 ) ) ;
#12116 = DIRECTION ( 'NONE',  ( 1.000000000000000000, 0.000000000000000000, 0.000000000000000000 ) ) ;
#12117 = VERTEX_POINT ( 'NONE', #40011 ) ;
#12118 = ORIENTED_EDGE ( 'NONE', *, *, #49654, .T. ) ;
#12119 = CARTESIAN_POINT ( 'NONE',  ( -11.77351654964679284, -7.826483450353365789, 455.0000000000000568 ) ) ;
#12120 = CYLINDRICAL_SURFACE ( 'NONE', #8579, 0.1749999999999998224 ) ;
#12121 = EDGE_CURVE ( 'NONE', #30178, #47920, #34719, .T. ) ;
#12122 = VERTEX_POINT ( 'NONE', #54927 ) ;
#12123 = DIRECTION ( 'NONE',  ( -0.000000000000000000, -1.000000000000000000, 0.000000000000000000 ) ) ;
#12124 = VERTEX_POINT ( 'NONE', #24108 ) ;
#12125 = EDGE_CURVE ( 'NONE', #16233, #29457, #49939, .T. ) ;
#12126 = EDGE_LOOP ( 'NONE', ( #40582, #68051 ) ) ;
#12127 = CARTESIAN_POINT ( 'NONE',  ( 30.00000000000000000, -5.599999999999379696, -26.60000000000059828 ) ) ;
#12128 = CARTESIAN_POINT ( 'NONE',  ( 283.0000000000000568, -23.65000000000000568, -12.40000000000000213 ) ) ;
#12129 = ORIENTED_EDGE ( 'NONE', *, *, #46488, .F. ) ;
#12130 = DIRECTION ( 'NONE',  ( -1.000000000000000000, 0.000000000000000000, 0.000000000000000000 ) ) ;
#12131 = EDGE_CURVE ( 'NONE', #30539, #16082, #1176, .T. ) ;
#12132 = CARTESIAN_POINT ( 'NONE',  ( 11.19368345035336709, -12.00648345035339659, 195.0000000000000284 ) ) ;
#12133 = CIRCLE ( 'NONE', #33593, 0.2000000000000005107 ) ;
#12134 = CIRCLE ( 'NONE', #49412, 0.2000000000000005107 ) ;
#12135 = CARTESIAN_POINT ( 'NONE',  ( 37.90000000000000568, -21.00000000000000000, 13.86939075806900057 ) ) ;
#12136 = ADVANCED_FACE ( 'NONE', ( #1499 ), #23068, .F. ) ;
#12137 = CARTESIAN_POINT ( 'NONE',  ( -4.135079735113167843, 6.822336235477362010, 54.00000000000000711 ) ) ;
#12138 = EDGE_LOOP ( 'NONE', ( #41684, #19277, #25306, #58295 ) ) ;
#12140 = ORIENTED_EDGE ( 'NONE', *, *, #2371, .F. ) ;
#12139 = DIRECTION ( 'NONE',  ( 0.000000000000000000, 1.000000000000000000, 0.000000000000000000 ) ) ;
#12141 = AXIS2_PLACEMENT_3D ( 'NONE', #1785, #56576, #28652 ) ;
#12142 = CIRCLE ( 'NONE', #881, 4.000000000000000888 ) ;
#12143 = CARTESIAN_POINT ( 'NONE',  ( -30.00000000000000000, -11.50000000000100009, -10.50000000000065903 ) ) ;
#12144 = DIRECTION ( 'NONE',  ( 0.000000000000000000, 0.7096009616570518874, -0.7046037717862339012 ) ) ;
#12145 = DIRECTION ( 'NONE',  ( -0.7071067811865411334, 0.7071067811865539010, 0.000000000000000000 ) ) ;
#12146 = CARTESIAN_POINT ( 'NONE',  ( 7.250000000000005329, 7.250000000000000888, -25.50000000000000355 ) ) ;
#12147 = ORIENTED_EDGE ( 'NONE', *, *, #40003, .F. ) ;
#12148 = VECTOR ( 'NONE', #9343, 999.9999999999998863 ) ;
#12150 = FACE_BOUND ( 'NONE', #31765, .T. ) ;
#12149 = CIRCLE ( 'NONE', #51688, 1.000000000000000000 ) ;
#12151 = CARTESIAN_POINT ( 'NONE',  ( 9.562023737882764607, 2.355476262117153663, 54.00000000000000711 ) ) ;
#12152 = EDGE_LOOP ( 'NONE', ( #23088, #28369, #50666, #678 ) ) ;
#12153 = ORIENTED_EDGE ( 'NONE', *, *, #30029, .F. ) ;
#12154 = ADVANCED_FACE ( 'NONE', ( #41071 ), #3250, .T. ) ;
#12155 = ORIENTED_EDGE ( 'NONE', *, *, #54907, .F. ) ;
#12156 = CARTESIAN_POINT ( 'NONE',  ( -7.250000000000000000, -7.449999999999998401, -8.000000000000000000 ) ) ;
#12157 = DIRECTION ( 'NONE',  ( 1.000000000000000000, -0.000000000000000000, -0.000000000000000000 ) ) ;
#12158 = CARTESIAN_POINT ( 'NONE',  ( 14.10805890929250062, -5.000000000000000000, 26.25000000000000000 ) ) ;
#12159 =( NAMED_UNIT ( * ) SI_UNIT ( $, .STERADIAN. ) SOLID_ANGLE_UNIT ( ) );
#12160 = AXIS2_PLACEMENT_3D ( 'NONE', #12960, #66716, #40540 ) ;
#12161 = CARTESIAN_POINT ( 'NONE',  ( 39.90000000000000568, -14.06939075806902117, -20.80000000000000426 ) ) ;
#12162 = ORIENTED_EDGE ( 'NONE', *, *, #28904, .T. ) ;
#12163 = ORIENTED_EDGE ( 'NONE', *, *, #34557, .T. ) ;
#12164 = ORIENTED_EDGE ( 'NONE', *, *, #49669, .F. ) ;
#12165 = DIRECTION ( 'NONE',  ( 1.000000000000000000, -5.981805089575194965E-17, 0.000000000000000000 ) ) ;
#12166 = EDGE_LOOP ( 'NONE', ( #43579, #14870, #51108, #45714 ) ) ;
#12167 = ORIENTED_EDGE ( 'NONE', *, *, #54589, .T. ) ;
#12168 = ORIENTED_EDGE ( 'NONE', *, *, #42731, .F. ) ;
#12169 = EDGE_LOOP ( 'NONE', ( #13914, #54255, #65125, #54923 ) ) ;
#12170 = CARTESIAN_POINT ( 'NONE',  ( 146.5599459900709860, 9.000000000000001776, 284.4801873289890182 ) ) ;
#12171 = ADVANCED_FACE ( 'NONE', ( #63357 ), #56642, .F. ) ;
#12173 = VERTEX_POINT ( 'NONE', #57691 ) ;
#12172 = CARTESIAN_POINT ( 'NONE',  ( 275.5000000000000000, -42.50000000000000000, -26.50000000000000000 ) ) ;
#12174 = PLANE ( 'NONE',  #14239 ) ;
#12175 = EDGE_CURVE ( 'NONE', #7253, #4233, #35466, .T. ) ;
#12176 = CARTESIAN_POINT ( 'NONE',  ( -10.30047626211724854, -3.664523737882715348, 54.00000000000000711 ) ) ;
#12177 = LINE ( 'NONE', #10795, #31314 ) ;
#12178 =( GEOMETRIC_REPRESENTATION_CONTEXT ( 3 ) GLOBAL_UNCERTAINTY_ASSIGNED_CONTEXT ( ( #14706 ) ) GLOBAL_UNIT_ASSIGNED_CONTEXT ( ( #68, #49191, #38917 ) ) REPRESENTATION_CONTEXT ( 'NONE', 'WORKASPACE' ) );
#12179 = ADVANCED_FACE ( 'NONE', ( #19855 ), #14205, .T. ) ;
#12180 = VERTEX_POINT ( 'NONE', #25530 ) ;
#12181 = CARTESIAN_POINT ( 'NONE',  ( -11.07551654964678711, -11.48848345035328933, 195.0000000000000284 ) ) ;
#12182 = FACE_OUTER_BOUND ( 'NONE', #66102, .T. ) ;
#12183 = CARTESIAN_POINT ( 'NONE',  ( 40.90000000000000568, -14.06939075806902117, -20.80000000000000426 ) ) ;
#12184 = EDGE_LOOP ( 'NONE', ( #34635, #20310, #12221, #34890 ) ) ;
#12185 = DIRECTION ( 'NONE',  ( -0.7671651518153128624, -0.6414496315691420314, 2.309356642089219057E-17 ) ) ;
#12186 = CIRCLE ( 'NONE', #18963, 1.224999999999999423 ) ;
#12187 = CARTESIAN_POINT ( 'NONE',  ( 7.357023737882784076, 3.834182069070697807, 54.00000000000000711 ) ) ;
#12188 = LINE ( 'NONE', #33758, #57109 ) ;
#12189 = ORIENTED_EDGE ( 'NONE', *, *, #1324, .T. ) ;
#12190 = LINE ( 'NONE', #28795, #17760 ) ;
#12191 = CIRCLE ( 'NONE', #37060, 24.99999999998784972 ) ;
#12192 = LINE ( 'NONE', #18192, #11561 ) ;
#12193 = CARTESIAN_POINT ( 'NONE',  ( 48.50000000000000000, -0.7500000000000000000, -3.418698582794335028 ) ) ;
#12194 = ORIENTED_EDGE ( 'NONE', *, *, #63011, .F. ) ;
#12195 = LINE ( 'NONE', #50379, #68145 ) ;
#12196 = DIRECTION ( 'NONE',  ( 0.000000000000000000, 0.000000000000000000, 1.000000000000000000 ) ) ;
#12197 = CYLINDRICAL_SURFACE ( 'NONE', #41229, 0.1999999999999987899 ) ;
#12198 = CARTESIAN_POINT ( 'NONE',  ( 30.00000000000000000, -13.79999999999979998, -17.30000000000000071 ) ) ;
#12199 = VECTOR ( 'NONE', #5457, 1000.000000000000000 ) ;
#12200 = ADVANCED_FACE ( 'NONE', ( #35771 ), #46378, .F. ) ;
#12201 = ORIENTED_EDGE ( 'NONE', *, *, #30115, .T. ) ;
#12202 = DIRECTION ( 'NONE',  ( -1.000000000000000000, 0.000000000000000000, 0.000000000000000000 ) ) ;
#12203 = DIRECTION ( 'NONE',  ( -1.000000000000000000, 3.491481338843133355E-15, 1.836970198721036590E-16 ) ) ;
#12204 = DIRECTION ( 'NONE',  ( 1.836970198721029934E-16, -1.836970198721036344E-16, 1.000000000000000000 ) ) ;
#12205 = PLANE ( 'NONE',  #48208 ) ;
#12206 = LINE ( 'NONE', #33779, #14974 ) ;
#12207 = ORIENTED_EDGE ( 'NONE', *, *, #35160, .F. ) ;
#12208 = CARTESIAN_POINT ( 'NONE',  ( 11.00000000000000000, -8.959999999999999076, 12.95475478405700009 ) ) ;
#12209 = LINE ( 'NONE', #39092, #7936 ) ;
#12210 = ADVANCED_FACE ( 'NONE', ( #31189 ), #36121, .F. ) ;
#12211 = EDGE_CURVE ( 'NONE', #22096, #30661, #12938, .T. ) ;
#12212 = LINE ( 'NONE', #59631, #39045 ) ;
#12213 = CARTESIAN_POINT ( 'NONE',  ( 2.906483450353343656, -10.92648345035336810, 195.0000000000000284 ) ) ;
#12214 = EDGE_CURVE ( 'NONE', #20060, #32671, #16403, .T. ) ;
#12215 = DIRECTION ( 'NONE',  ( -1.836970198721029934E-16, 1.836970198721036344E-16, -1.000000000000000000 ) ) ;
#12216 = EDGE_CURVE ( 'NONE', #9032, #8637, #13856, .T. ) ;
#12217 = EDGE_LOOP ( 'NONE', ( #13783, #61563, #52378, #5386 ) ) ;
#12218 = EDGE_CURVE ( 'NONE', #46458, #64694, #62287, .T. ) ;
#12219 = CARTESIAN_POINT ( 'NONE',  ( 26.90000000000000213, 0.000000000000000000, 0.000000000000000000 ) ) ;
#12220 = CARTESIAN_POINT ( 'NONE',  ( -2.406732575409666008, -8.711985858128704407, 26.00000000000000711 ) ) ;
#12221 = ORIENTED_EDGE ( 'NONE', *, *, #5743, .T. ) ;
#12222 = CARTESIAN_POINT ( 'NONE',  ( -7.250000000000000888, 8.250000000000001776, -26.00000000000001066 ) ) ;
#12223 = EDGE_LOOP ( 'NONE', ( #37494, #31111, #44735, #48529 ) ) ;
#12224 = CARTESIAN_POINT ( 'NONE',  ( 11.25000000000000178, -11.18999999999999950, -5.000000000000000000 ) ) ;
#12225 = EDGE_LOOP ( 'NONE', ( #36366, #37241 ) ) ;
#12226 = ORIENTED_EDGE ( 'NONE', *, *, #55740, .T. ) ;
#12227 = CARTESIAN_POINT ( 'NONE',  ( 15.50000000000000000, -0.2038245569916604938, 23.94337567297399971 ) ) ;
#12228 = CARTESIAN_POINT ( 'NONE',  ( 8.250000000000005329, 0.000000000000000000, -23.00000000000000000 ) ) ;
#12229 = CIRCLE ( 'NONE', #66450, 0.1999999999999987899 ) ;
#12230 = DIRECTION ( 'NONE',  ( 1.836970198721029934E-16, 1.836970198721010706E-16, -1.000000000000000000 ) ) ;
#12231 = DIRECTION ( 'NONE',  ( -1.000000000000000000, 0.000000000000000000, 0.000000000000000000 ) ) ;
#12232 = VERTEX_POINT ( 'NONE', #51702 ) ;
#12233 = ORIENTED_EDGE ( 'NONE', *, *, #25026, .F. ) ;
#12234 = CARTESIAN_POINT ( 'NONE',  ( -23.48000000000000043, -15.50000000000000000, -26.00000000000000355 ) ) ;
#12235 = AXIS2_PLACEMENT_3D ( 'NONE', #14996, #68034, #19591 ) ;
#12236 = CARTESIAN_POINT ( 'NONE',  ( 4.149127210878741145, 3.663616288756999406, 54.00000000000000711 ) ) ;
#12237 = ORIENTED_EDGE ( 'NONE', *, *, #24619, .F. ) ;
#12238 = VERTEX_POINT ( 'NONE', #61940 ) ;
#12239 = ORIENTED_EDGE ( 'NONE', *, *, #16137, .F. ) ;
#12240 = DIRECTION ( 'NONE',  ( 1.000000000000000000, 0.000000000000000000, 0.000000000000000000 ) ) ;
#12241 = CARTESIAN_POINT ( 'NONE',  ( -7.798499376344157241, -7.272650909786626983, 455.0000000000000568 ) ) ;
#12243 = VERTEX_POINT ( 'NONE', #56980 ) ;
#12242 = DIRECTION ( 'NONE',  ( -1.000000000000000000, 0.000000000000000000, 0.000000000000000000 ) ) ;
#12244 = CIRCLE ( 'NONE', #31472, 0.1999999999999996503 ) ;
#12245 = CARTESIAN_POINT ( 'NONE',  ( 7.250000000000005329, 8.250000000000001776, -23.50000000000000000 ) ) ;
#12246 = CARTESIAN_POINT ( 'NONE',  ( 2.632023737882806191, 6.486996718459881350, 54.00000000000000711 ) ) ;
#12247 = ORIENTED_EDGE ( 'NONE', *, *, #30115, .F. ) ;
#12248 = EDGE_CURVE ( 'NONE', #4189, #4894, #25383, .T. ) ;
#12249 = ORIENTED_EDGE ( 'NONE', *, *, #32366, .T. ) ;
#12250 = ADVANCED_FACE ( 'NONE', ( #3958 ), #68665, .T. ) ;
#12251 = ADVANCED_FACE ( 'NONE', ( #13505 ), #58040, .F. ) ;
#12252 = DIRECTION ( 'NONE',  ( 0.000000000000000000, 0.000000000000000000, 1.000000000000000000 ) ) ;
#12253 = DIRECTION ( 'NONE',  ( 0.7071067811865474617, 0.7071067811865474617, 0.000000000000000000 ) ) ;
#12254 = PLANE ( 'NONE',  #42799 ) ;
#12255 = SURFACE_SIDE_STYLE ('',( #637 ) ) ;
#12256 = CARTESIAN_POINT ( 'NONE',  ( 15.00000000000000000, -21.00000000000000000, 0.000000000000000000 ) ) ;
#12258 = ORIENTED_EDGE ( 'NONE', *, *, #55080, .T. ) ;
#12257 = CARTESIAN_POINT ( 'NONE',  ( -7.250000000000000888, 8.250000000000001776, -20.00000000000000000 ) ) ;
#12259 = ORIENTED_EDGE ( 'NONE', *, *, #62299, .T. ) ;
#12260 = DIRECTION ( 'NONE',  ( -1.000000000000000000, 1.047444401652940007E-14, -1.836970198721010706E-16 ) ) ;
#12261 = LINE ( 'NONE', #56116, #23938 ) ;
#12262 = DIRECTION ( 'NONE',  ( -1.000000000000000000, 0.000000000000000000, 0.000000000000000000 ) ) ;
#12263 = CARTESIAN_POINT ( 'NONE',  ( 49.00000000000000000, 13.66939075806899950, 20.80000000000000426 ) ) ;
#12264 = CIRCLE ( 'NONE', #69886, 0.1999999999999987899 ) ;
#12265 = DIRECTION ( 'NONE',  ( 3.304235192336781428E-15, 1.000000000000000000, 0.000000000000000000 ) ) ;
#12266 = ORIENTED_EDGE ( 'NONE', *, *, #23176, .F. ) ;
#12267 = CARTESIAN_POINT ( 'NONE',  ( 6.849523737882817542, -10.50702373788282529, 54.00000000000000711 ) ) ;
#12268 = DIRECTION ( 'NONE',  ( -1.000000000000000000, 0.000000000000000000, 0.000000000000000000 ) ) ;
#12269 = DIRECTION ( 'NONE',  ( -1.836970198721029934E-16, 1.836970198721036344E-16, -1.000000000000000000 ) ) ;
#12270 = VECTOR ( 'NONE', #34750, 1000.000000000000000 ) ;
#12271 = LINE ( 'NONE', #38147, #12985 ) ;
#12272 = CARTESIAN_POINT ( 'NONE',  ( 10.00000000000000000, -21.00000000000000000, 14.57806571531351914 ) ) ;
#12273 = CARTESIAN_POINT ( 'NONE',  ( -6.606374702650169795, 4.734785091273855606, 455.0000000000000568 ) ) ;
#12274 = VECTOR ( 'NONE', #45667, 1000.000000000000000 ) ;
#12275 = DIRECTION ( 'NONE',  ( 0.000000000000000000, 1.000000000000000000, 0.000000000000000000 ) ) ;
#12276 = VERTEX_POINT ( 'NONE', #29759 ) ;
#12277 = LINE ( 'NONE', #39507, #38848 ) ;
#12278 = DIRECTION ( 'NONE',  ( 0.000000000000000000, 0.000000000000000000, 1.000000000000000000 ) ) ;
#12279 = ORIENTED_EDGE ( 'NONE', *, *, #2696, .F. ) ;
#12280 = CYLINDRICAL_SURFACE ( 'NONE', #54892, 1.399999999999998579 ) ;
#12281 = CARTESIAN_POINT ( 'NONE',  ( -7.955476262117259445, 9.722976262117178692, 26.00000000000000711 ) ) ;
#12282 = AXIS2_PLACEMENT_3D ( 'NONE', #7431, #2133, #61885 ) ;
#12283 = CARTESIAN_POINT ( 'NONE',  ( 3.677663764522614454, -4.149127210878770455, 54.00000000000000711 ) ) ;
#12284 = DIRECTION ( 'NONE',  ( 0.000000000000000000, 0.000000000000000000, 1.000000000000000000 ) ) ;
#12285 = LINE ( 'NONE', #60387, #5718 ) ;
#12286 = EDGE_CURVE ( 'NONE', #29958, #11292, #19762, .T. ) ;
#12287 = ORIENTED_EDGE ( 'NONE', *, *, #43450, .F. ) ;
#12289 = VECTOR ( 'NONE', #634, 1000.000000000000000 ) ;
#12288 = AXIS2_PLACEMENT_3D ( 'NONE', #50473, #64241, #37365 ) ;
#12290 = CARTESIAN_POINT ( 'NONE',  ( -30.00000000000000000, -9.487228132326899654, -12.50000000000000000 ) ) ;
#12291 = ORIENTED_EDGE ( 'NONE', *, *, #40768, .F. ) ;
#12292 = ADVANCED_FACE ( 'NONE', ( #54145 ), #5709, .F. ) ;
#12293 = DIRECTION ( 'NONE',  ( -1.000000000000000000, 0.000000000000000000, 0.000000000000000000 ) ) ;
#12294 = EDGE_CURVE ( 'NONE', #25376, #37466, #55, .T. ) ;
#12295 = ORIENTED_EDGE ( 'NONE', *, *, #35160, .T. ) ;
#12296 = CARTESIAN_POINT ( 'NONE',  ( -11.18071654964669648, 11.18071654964658812, 455.0000000000000568 ) ) ;
#12297 = AXIS2_PLACEMENT_3D ( 'NONE', #39663, #8185, #6204 ) ;
#12298 = DIRECTION ( 'NONE',  ( -1.000000000000000000, -8.951101527228104953E-17, 0.000000000000000000 ) ) ;
#12299 = CARTESIAN_POINT ( 'NONE',  ( 30.00000000000000000, -5.599999999999999645, -9.000000000000001776 ) ) ;
#12300 = ORIENTED_EDGE ( 'NONE', *, *, #63043, .F. ) ;
#12301 = VERTEX_POINT ( 'NONE', #27277 ) ;
#12302 = DIRECTION ( 'NONE',  ( -1.000000000000000000, 0.000000000000000000, 0.000000000000000000 ) ) ;
#12304 = ORIENTED_EDGE ( 'NONE', *, *, #32892, .T. ) ;
#12303 = EDGE_CURVE ( 'NONE', #32276, #36995, #21620, .T. ) ;
#12305 = EDGE_LOOP ( 'NONE', ( #7871, #31292, #48530, #8076 ) ) ;
#12306 = DIRECTION ( 'NONE',  ( 1.000000000000000000, -0.000000000000000000, -0.000000000000000000 ) ) ;
#12307 = DIRECTION ( 'NONE',  ( -1.000000000000000000, 0.000000000000000000, 0.000000000000000000 ) ) ;
#12308 = DIRECTION ( 'NONE',  ( -0.000000000000000000, -0.000000000000000000, -1.000000000000000000 ) ) ;
#12309 = ORIENTED_EDGE ( 'NONE', *, *, #6353, .T. ) ;
#12310 = DIRECTION ( 'NONE',  ( -1.261617073437657735E-14, -1.000000000000000000, 0.000000000000000000 ) ) ;
#12312 = DIRECTION ( 'NONE',  ( 0.000000000000000000, 0.000000000000000000, -1.000000000000000000 ) ) ;
#12311 = CARTESIAN_POINT ( 'NONE',  ( 30.00000000000000000, -16.64230188589299786, -14.64519951917100116 ) ) ;
#12313 = ORIENTED_EDGE ( 'NONE', *, *, #3145, .F. ) ;
#12315 = VERTEX_POINT ( 'NONE', #53798 ) ;
#12314 = DIRECTION ( 'NONE',  ( -1.000000000000000000, 8.540177112501197482E-15, 0.000000000000000000 ) ) ;
#12316 = ORIENTED_EDGE ( 'NONE', *, *, #30884, .T. ) ;
#12317 = VECTOR ( 'NONE', #56341, 1000.000000000000000 ) ;
#12318 =( LENGTH_UNIT ( ) NAMED_UNIT ( * ) SI_UNIT ( .MILLI., .METRE. ) );
#12319 = PLANE ( 'NONE',  #50204 ) ;
#12320 = AXIS2_PLACEMENT_3D ( 'NONE', #19692, #25021, #15114 ) ;
#12321 = AXIS2_PLACEMENT_3D ( 'NONE', #59736, #49476, #11284 ) ;
#12322 = ORIENTED_EDGE ( 'NONE', *, *, #61874, .T. ) ;
#12323 = CARTESIAN_POINT ( 'NONE',  ( -7.593516549646711411, 11.31351654964660014, 455.0000000000000568 ) ) ;
#12324 = ORIENTED_EDGE ( 'NONE', *, *, #59021, .F. ) ;
#12325 = ORIENTED_EDGE ( 'NONE', *, *, #14383, .T. ) ;
#12326 = VECTOR ( 'NONE', #9610, 1000.000000000000000 ) ;
#12327 = FACE_OUTER_BOUND ( 'NONE', #29947, .T. ) ;
#12328 = DIRECTION ( 'NONE',  ( 0.000000000000000000, -1.000000000000000000, 0.000000000000000000 ) ) ;
#12329 = ORIENTED_EDGE ( 'NONE', *, *, #52465, .F. ) ;
#12330 = ADVANCED_FACE ( 'NONE', ( #69348 ), #21952, .F. ) ;
#12331 = VECTOR ( 'NONE', #52557, 1000.000000000000000 ) ;
#12332 = LINE ( 'NONE', #7038, #12754 ) ;
#12333 = CARTESIAN_POINT ( 'NONE',  ( 15.50000000000000000, -15.50000000000000000, -25.99999999999985079 ) ) ;
#12334 = DIRECTION ( 'NONE',  ( 0.000000000000000000, -0.000000000000000000, 1.000000000000000000 ) ) ;
#12335 = ORIENTED_EDGE ( 'NONE', *, *, #2494, .T. ) ;
#12336 = AXIS2_PLACEMENT_3D ( 'NONE', #7239, #3006, #35156 ) ;
#12337 = CARTESIAN_POINT ( 'NONE',  ( -11.00000000000000000, -15.97213595500069871, 14.50000000000000000 ) ) ;
#12338 = DIRECTION ( 'NONE',  ( 0.000000000000000000, -3.673940397442059868E-16, 1.000000000000000000 ) ) ;
#12339 = VERTEX_POINT ( 'NONE', #16667 ) ;
#12341 = VERTEX_POINT ( 'NONE', #20562 ) ;
#12340 = DIRECTION ( 'NONE',  ( 0.000000000000000000, 0.000000000000000000, -1.000000000000000000 ) ) ;
#12342 = CARTESIAN_POINT ( 'NONE',  ( 7.250000000000004441, 7.450000000000001954, -14.50000000000000000 ) ) ;
#12343 = AXIS2_PLACEMENT_3D ( 'NONE', #48359, #21825, #32091 ) ;
#12344 = ADVANCED_FACE ( 'NONE', ( #58752 ), #53450, .F. ) ;
#12345 = CARTESIAN_POINT ( 'NONE',  ( 4.155633711806658859, -4.720772854004797736, 26.00000000000000711 ) ) ;
#12346 = CARTESIAN_POINT ( 'NONE',  ( 282.6457513110646005, -20.49999999999999645, -17.00000000000000000 ) ) ;
#12347 = CARTESIAN_POINT ( 'NONE',  ( 15.50000000000000000, -0.4000000000000000222, -22.50000000000000000 ) ) ;
#12348 = EDGE_CURVE ( 'NONE', #6527, #60332, #53661, .T. ) ;
#12349 = LINE ( 'NONE', #13415, #19081 ) ;
#12350 = ORIENTED_EDGE ( 'NONE', *, *, #68823, .F. ) ;
#12351 = FACE_OUTER_BOUND ( 'NONE', #16788, .T. ) ;
#12352 = LINE ( 'NONE', #50198, #28199 ) ;
#12353 = CYLINDRICAL_SURFACE ( 'NONE', #37884, 4.500000000000188294 ) ;
#12355 = ORIENTED_EDGE ( 'NONE', *, *, #29900, .T. ) ;
#12354 = DIRECTION ( 'NONE',  ( 0.000000000000000000, 1.000000000000000000, 0.000000000000000000 ) ) ;
#12356 = CARTESIAN_POINT ( 'NONE',  ( 7.450000000000006395, 7.250000000000000888, -20.50000000000000000 ) ) ;
#12357 = FACE_OUTER_BOUND ( 'NONE', #67318, .T. ) ;
#12358 = ORIENTED_EDGE ( 'NONE', *, *, #49322, .T. ) ;
#12359 = DIRECTION ( 'NONE',  ( 0.4999999999999755196, -0.8660254037844526964, 0.000000000000000000 ) ) ;
#12360 = CARTESIAN_POINT ( 'NONE',  ( 2.906483450353372522, 11.11351654964663638, 195.0000000000000284 ) ) ;
#12361 = ORIENTED_EDGE ( 'NONE', *, *, #65744, .T. ) ;
#12362 = LINE ( 'NONE', #39595, #18756 ) ;
#12363 = FACE_OUTER_BOUND ( 'NONE', #57902, .T. ) ;
#12364 = FACE_BOUND ( 'NONE', #49903, .T. ) ;
#12365 = LINE ( 'NONE', #43877, #22558 ) ;
#12366 = CIRCLE ( 'NONE', #48546, 0.1999999999999987899 ) ;
#12367 = AXIS2_PLACEMENT_3D ( 'NONE', #13286, #67028, #23196 ) ;
#12368 = EDGE_CURVE ( 'NONE', #39654, #57686, #18600, .T. ) ;
#12369 = LINE ( 'NONE', #66137, #1503 ) ;
#12370 = AXIS2_PLACEMENT_3D ( 'NONE', #38822, #44813, #12278 ) ;
#12371 = ORIENTED_EDGE ( 'NONE', *, *, #55150, .F. ) ;
#12372 = ADVANCED_FACE ( 'NONE', ( #42122 ), #43169, .F. ) ;
#12373 = FACE_OUTER_BOUND ( 'NONE', #56033, .T. ) ;
#12374 = ORIENTED_EDGE ( 'NONE', *, *, #29200, .F. ) ;
#12375 = EDGE_CURVE ( 'NONE', #45981, #10245, #59787, .T. ) ;
#12376 = ORIENTED_EDGE ( 'NONE', *, *, #29851, .T. ) ;
#12377 = AXIS2_PLACEMENT_3D ( 'NONE', #43082, #69959, #47696 ) ;
#12378 = DIRECTION ( 'NONE',  ( 0.000000000000000000, 0.000000000000000000, 1.000000000000000000 ) ) ;
#12379 = FACE_OUTER_BOUND ( 'NONE', #1875, .T. ) ;
#12380 = ADVANCED_FACE ( 'NONE', ( #63709 ), #38235, .F. ) ;
#12381 = EDGE_CURVE ( 'NONE', #18763, #8602, #48142, .T. ) ;
#12382 = VECTOR ( 'NONE', #35331, 1000.000000000000000 ) ;
#12383 = SURFACE_STYLE_USAGE ( .BOTH. , #18747 ) ;
#12384 = DIRECTION ( 'NONE',  ( -1.000000000000000000, 0.000000000000000000, 0.000000000000000000 ) ) ;
#12385 = EDGE_LOOP ( 'NONE', ( #40884, #44006, #51539, #24198 ) ) ;
#12386 = EDGE_CURVE ( 'NONE', #41004, #38597, #37533, .T. ) ;
#12387 = EDGE_LOOP ( 'NONE', ( #39589, #5928, #57701, #33088 ) ) ;
#12388 = AXIS2_PLACEMENT_3D ( 'NONE', #66274, #29132, #22788 ) ;
#12389 = CARTESIAN_POINT ( 'NONE',  ( 7.281754163448140638, 8.000000000000001776, -1.000000000000000000 ) ) ;
#12391 = EDGE_LOOP ( 'NONE', ( #29646, #8861, #12068, #40555 ) ) ;
#12390 = EDGE_CURVE ( 'NONE', #61399, #11259, #59091, .T. ) ;
#12392 = CIRCLE ( 'NONE', #51940, 0.2000000000000005107 ) ;
#12393 = LINE ( 'NONE', #65810, #29232 ) ;
#12394 = LINE ( 'NONE', #67562, #27515 ) ;
#12395 = CARTESIAN_POINT ( 'NONE',  ( -10.49297626211726175, 3.650476262117184234, 54.00000000000000711 ) ) ;
#12396 =( NAMED_UNIT ( * ) PLANE_ANGLE_UNIT ( ) SI_UNIT ( $, .RADIAN. ) );
#12397 = AXIS2_PLACEMENT_3D ( 'NONE', #53885, #5083, #16741 ) ;
#12398 = CIRCLE ( 'NONE', #37326, 0.1999999999999987899 ) ;
#12400 = DIRECTION ( 'NONE',  ( 1.000000000000000000, -0.000000000000000000, 0.000000000000000000 ) ) ;
#12399 = PLANE ( 'NONE',  #14031 ) ;
#12401 = VERTEX_POINT ( 'NONE', #15267 ) ;
#12403 = ORIENTED_EDGE ( 'NONE', *, *, #57376, .T. ) ;
#12402 = CARTESIAN_POINT ( 'NONE',  ( 25.50000000000000355, 0.000000000000000000, 22.50000000000000000 ) ) ;
#12404 = VERTEX_POINT ( 'NONE', #53110 ) ;
#12405 = EDGE_LOOP ( 'NONE', ( #19634, #58953, #314, #64627 ) ) ;
#12406 = CARTESIAN_POINT ( 'NONE',  ( 8.406483450353379183, -5.668387132716048882, 455.0000000000000568 ) ) ;
#12407 = DIRECTION ( 'NONE',  ( 0.000000000000000000, 0.000000000000000000, -1.000000000000000000 ) ) ;
#12408 = AXIS2_PLACEMENT_3D ( 'NONE', #18958, #52541, #40517 ) ;
#12409 = CARTESIAN_POINT ( 'NONE',  ( -15.50000000000000000, -2.500000000000000000, -23.94337567297399971 ) ) ;
#12410 = VERTEX_POINT ( 'NONE', #32582 ) ;
#12411 = ORIENTED_EDGE ( 'NONE', *, *, #23174, .F. ) ;
#12412 = DIRECTION ( 'NONE',  ( -0.000000000000000000, 3.673940397442059868E-16, -1.000000000000000000 ) ) ;
#12413 = CARTESIAN_POINT ( 'NONE',  ( 30.00000000000000000, -17.14999999999900027, -26.64999999999900027 ) ) ;
#12414 = ORIENTED_EDGE ( 'NONE', *, *, #18434, .F. ) ;
#12415 = EDGE_CURVE ( 'NONE', #43836, #34688, #7336, .T. ) ;
#12416 = VERTEX_POINT ( 'NONE', #47781 ) ;
#12417 = PLANE ( 'NONE',  #63575 ) ;
#12418 = AXIS2_PLACEMENT_3D ( 'NONE', #25158, #46713, #8178 ) ;
#12419 = CARTESIAN_POINT ( 'NONE',  ( -30.00000000000000000, -8.959999999999999076, 12.95475478405700009 ) ) ;
#12420 = VECTOR ( 'NONE', #50872, 1000.000000000000000 ) ;
#12421 = VERTEX_POINT ( 'NONE', #16301 ) ;
#12422 = EDGE_CURVE ( 'NONE', #66751, #20472, #33311, .T. ) ;
#12423 = AXIS2_PLACEMENT_3D ( 'NONE', #33096, #6228, #23173 ) ;
#12424 = LINE ( 'NONE', #19139, #40251 ) ;
#12426 = ORIENTED_EDGE ( 'NONE', *, *, #7265, .F. ) ;
#12425 = CARTESIAN_POINT ( 'NONE',  ( 10.00000000000000000, -21.00000000000000000, 18.00000000000000355 ) ) ;
#12427 = ORIENTED_EDGE ( 'NONE', *, *, #50874, .T. ) ;
#12428 = VECTOR ( 'NONE', #32403, 1000.000000000000000 ) ;
#12429 = CARTESIAN_POINT ( 'NONE',  ( 29.50000000000000355, -11.50000000000000000, 15.00000000000000000 ) ) ;
#12430 = CYLINDRICAL_SURFACE ( 'NONE', #19929, 0.5000000000004306555 ) ;
#12431 = LINE ( 'NONE', #45659, #36269 ) ;
#12432 = DIRECTION ( 'NONE',  ( 1.000000000000000000, -1.356437060717834379E-15, -1.836970198721032646E-16 ) ) ;
#12433 = CARTESIAN_POINT ( 'NONE',  ( 151.5599459900709860, 9.000000000000001776, 282.8454385697650082 ) ) ;
#12434 = AXIS2_PLACEMENT_3D ( 'NONE', #39181, #44130, #1689 ) ;
#12435 = FACE_BOUND ( 'NONE', #25230, .T. ) ;
#12436 = ADVANCED_FACE ( 'NONE', ( #34271, #22316 ), #38903, .F. ) ;
#12437 = AXIS2_PLACEMENT_3D ( 'NONE', #17059, #7120, #43582 ) ;
#12438 = ORIENTED_EDGE ( 'NONE', *, *, #5492, .T. ) ;
#12439 = PLANE ( 'NONE',  #48453 ) ;
#12441 = EDGE_LOOP ( 'NONE', ( #14083, #46950, #61343, #60943 ) ) ;
#12440 = CARTESIAN_POINT ( 'NONE',  ( -11.31351654964678843, -7.606483450353371367, 455.0000000000000568 ) ) ;
#12442 = LINE ( 'NONE', #6481, #46780 ) ;
#12443 = DIRECTION ( 'NONE',  ( 0.000000000000000000, 0.000000000000000000, -1.000000000000000000 ) ) ;
#12444 = VECTOR ( 'NONE', #15079, 1000.000000000000000 ) ;
#12445 = EDGE_CURVE ( 'NONE', #57359, #20615, #11770, .T. ) ;
#12446 = FACE_OUTER_BOUND ( 'NONE', #13988, .T. ) ;
#12447 = EDGE_CURVE ( 'NONE', #24763, #24032, #17332, .T. ) ;
#12448 = DIRECTION ( 'NONE',  ( 1.000000000000000000, 0.000000000000000000, 0.000000000000000000 ) ) ;
#12449 = VECTOR ( 'NONE', #21946, 1000.000000000000000 ) ;
#12450 = VECTOR ( 'NONE', #56347, 1000.000000000000000 ) ;
#12451 = DIRECTION ( 'NONE',  ( -1.000000000000000000, 0.000000000000000000, 0.000000000000000000 ) ) ;
#12452 = EDGE_CURVE ( 'NONE', #15205, #17604, #60122, .T. ) ;
#12453 = ORIENTED_EDGE ( 'NONE', *, *, #59467, .T. ) ;
#12454 = EDGE_CURVE ( 'NONE', #62655, #60123, #6390, .T. ) ;
#12455 = EDGE_CURVE ( 'NONE', #16007, #63302, #45703, .T. ) ;
#12456 = ORIENTED_EDGE ( 'NONE', *, *, #16860, .F. ) ;
#12457 = DIRECTION ( 'NONE',  ( 1.836970198721029934E-16, 1.836970198721010706E-16, -1.000000000000000000 ) ) ;
#12458 =( NAMED_UNIT ( * ) SI_UNIT ( $, .STERADIAN. ) SOLID_ANGLE_UNIT ( ) );
#12459 = EDGE_CURVE ( 'NONE', #42591, #48280, #66120, .T. ) ;
#12460 = CARTESIAN_POINT ( 'NONE',  ( -7.603567055985545942, 8.393516549646601987, 455.0000000000000568 ) ) ;
#12461 = ORIENTED_EDGE ( 'NONE', *, *, #37659, .T. ) ;
#12462 = AXIS2_PLACEMENT_3D ( 'NONE', #15673, #25938, #68008 ) ;
#12463 = EDGE_CURVE ( 'NONE', #27858, #47920, #23338, .T. ) ;
#12464 = LINE ( 'NONE', #7159, #50806 ) ;
#12465 = VERTEX_POINT ( 'NONE', #60467 ) ;
#12466 = ORIENTED_EDGE ( 'NONE', *, *, #64829, .T. ) ;
#12467 = EDGE_CURVE ( 'NONE', #17187, #18067, #57018, .T. ) ;
#12468 = DIRECTION ( 'NONE',  ( 1.000000000000000000, -0.000000000000000000, -0.000000000000000000 ) ) ;
#12469 = FACE_BOUND ( 'NONE', #49304, .T. ) ;
#12470 = ORIENTED_EDGE ( 'NONE', *, *, #162, .T. ) ;
#12471 = FACE_BOUND ( 'NONE', #35644, .T. ) ;
#12472 = DIRECTION ( 'NONE',  ( -1.000000000000000000, 0.000000000000000000, 0.000000000000000000 ) ) ;
#12473 = VECTOR ( 'NONE', #42469, 1000.000000000000000 ) ;
#12474 = DIRECTION ( 'NONE',  ( -0.000000000000000000, -0.000000000000000000, 1.000000000000000000 ) ) ;
#12475 = EDGE_CURVE ( 'NONE', #14272, #13993, #50562, .T. ) ;
#12476 = ORIENTED_EDGE ( 'NONE', *, *, #2548, .T. ) ;
#12477 = VECTOR ( 'NONE', #68901, 1000.000000000000000 ) ;
#12479 = ORIENTED_EDGE ( 'NONE', *, *, #56136, .F. ) ;
#12478 = LINE ( 'NONE', #24502, #1312 ) ;
#12480 = EDGE_CURVE ( 'NONE', #44460, #43261, #49179, .T. ) ;
#12481 = CIRCLE ( 'NONE', #68982, 0.5249999999999994671 ) ;
#12482 = DIRECTION ( 'NONE',  ( 0.000000000000000000, 0.4606534372016282686, -0.8875800869748744493 ) ) ;
#12483 = CARTESIAN_POINT ( 'NONE',  ( -10.08346604330787777, 9.093516549646603053, 195.0000000000000284 ) ) ;
#12484 = CARTESIAN_POINT ( 'NONE',  ( 283.0000000000000568, -25.93000000000544958, -9.412893218815410634 ) ) ;
#12485 = PLANE ( 'NONE',  #33058 ) ;
#12486 = ORIENTED_EDGE ( 'NONE', *, *, #69077, .T. ) ;
#12487 = VECTOR ( 'NONE', #9978, 1000.000000000000000 ) ;
#12488 = CARTESIAN_POINT ( 'NONE',  ( 277.0217896459287203, -20.81978353999699749, 17.31978353999700104 ) ) ;
#12489 = CARTESIAN_POINT ( 'NONE',  ( 7.272650909786602114, 4.188533722949199678, 455.0000000000000568 ) ) ;
#12490 = VERTEX_POINT ( 'NONE', #750 ) ;
#12491 = ORIENTED_EDGE ( 'NONE', *, *, #8648, .F. ) ;
#12492 = VECTOR ( 'NONE', #11519, 1000.000000000000000 ) ;
#12493 = VECTOR ( 'NONE', #48085, 1000.000000000000114 ) ;
#12494 = EDGE_LOOP ( 'NONE', ( #14876, #14163, #52084, #9949 ) ) ;
#12495 = LINE ( 'NONE', #43986, #53620 ) ;
#12496 = CARTESIAN_POINT ( 'NONE',  ( 46.39999999999999858, 33.00000000000000000, 1.750000000000000222 ) ) ;
#12497 = CIRCLE ( 'NONE', #15909, 24.99999999998784972 ) ;
#12498 = CARTESIAN_POINT ( 'NONE',  ( -11.18071654964682615, -12.00648345035337350, 455.0000000000000568 ) ) ;
#12499 =( NAMED_UNIT ( * ) SI_UNIT ( $, .STERADIAN. ) SOLID_ANGLE_UNIT ( ) );
#12500 = ORIENTED_EDGE ( 'NONE', *, *, #24261, .F. ) ;
#12501 = VERTEX_POINT ( 'NONE', #54833 ) ;
#12502 = ORIENTED_EDGE ( 'NONE', *, *, #5179, .T. ) ;
#12504 = DIRECTION ( 'NONE',  ( -1.000000000000000000, 0.000000000000000000, 0.000000000000000000 ) ) ;
#12503 = AXIS2_PLACEMENT_3D ( 'NONE', #42036, #21514, #69954 ) ;
#12505 = ORIENTED_EDGE ( 'NONE', *, *, #1300, .T. ) ;
#12506 = ORIENTED_EDGE ( 'NONE', *, *, #39906, .F. ) ;
#12507 = EDGE_LOOP ( 'NONE', ( #42723, #47965, #55243, #8146 ) ) ;
#12508 = EDGE_CURVE ( 'NONE', #57228, #58960, #66044, .T. ) ;
#12509 = VERTEX_POINT ( 'NONE', #22985 ) ;
#12510 = FACE_OUTER_BOUND ( 'NONE', #3848, .T. ) ;
#12512 = ORIENTED_EDGE ( 'NONE', *, *, #67100, .T. ) ;
#12511 = CYLINDRICAL_SURFACE ( 'NONE', #36805, 4.000000000000000000 ) ;
#12513 = ADVANCED_FACE ( 'NONE', ( #22649 ), #1090, .F. ) ;
#12514 = CYLINDRICAL_SURFACE ( 'NONE', #34554, 0.5000000000000000000 ) ;
#12515 = CARTESIAN_POINT ( 'NONE',  ( -9.722976262117258628, 6.817976262117182884, 26.00000000000000711 ) ) ;
#12516 = VECTOR ( 'NONE', #44093, 1000.000000000000000 ) ;
#12517 = DIRECTION ( 'NONE',  ( -3.304235192336778667E-15, -1.000000000000000000, 0.000000000000000000 ) ) ;
#12518 = EDGE_CURVE ( 'NONE', #12650, #52657, #33931, .T. ) ;
#12520 = VERTEX_POINT ( 'NONE', #44201 ) ;
#12519 = CARTESIAN_POINT ( 'NONE',  ( -4.706725378239216440, 6.344366288193329595, 54.00000000000000711 ) ) ;
#12521 = ADVANCED_FACE ( 'NONE', ( #7060 ), #33602, .F. ) ;
#12522 = CARTESIAN_POINT ( 'NONE',  ( -5.242976262117259978, 5.242976262117182706, 26.00000000000000711 ) ) ;
#12523 = CARTESIAN_POINT ( 'NONE',  ( 11.08848345035342042, 11.47551654964652812, 455.0000000000000568 ) ) ;
#12524 = CARTESIAN_POINT ( 'NONE',  ( -8.250000000000001776, 7.250000000000000888, -10.50000000000000000 ) ) ;
#12525 = EDGE_CURVE ( 'NONE', #32093, #38982, #44539, .T. ) ;
#12526 = VECTOR ( 'NONE', #69245, 1000.000000000000000 ) ;
#12527 = ORIENTED_EDGE ( 'NONE', *, *, #17412, .F. ) ;
#12528 = CYLINDRICAL_SURFACE ( 'NONE', #46122, 0.5250000000000004663 ) ;
#12529 = DIRECTION ( 'NONE',  ( -1.000000000000000000, 0.000000000000000000, 0.000000000000000000 ) ) ;
#12530 = VECTOR ( 'NONE', #49586, 1000.000000000000000 ) ;
#12531 = DIRECTION ( 'NONE',  ( 1.000000000000000000, 0.000000000000000000, 0.000000000000000000 ) ) ;
#12532 = VERTEX_POINT ( 'NONE', #12704 ) ;
#12534 = LINE ( 'NONE', #5865, #29059 ) ;
#12533 = AXIS2_PLACEMENT_3D ( 'NONE', #62462, #34550, #18285 ) ;
#12535 = CARTESIAN_POINT ( 'NONE',  ( 11.18999999999999950, -11.18999999999999950, -5.000000000000000000 ) ) ;
#12536 = CARTESIAN_POINT ( 'NONE',  ( -30.00000000000000000, -15.46862696659690073, 14.50000000000000000 ) ) ;
#12537 = CIRCLE ( 'NONE', #2353, 0.9999999999999991118 ) ;
#12538 = EDGE_CURVE ( 'NONE', #68548, #9656, #28984, .T. ) ;
#12539 = VECTOR ( 'NONE', #38434, 1000.000000000000000 ) ;
#12540 = ORIENTED_EDGE ( 'NONE', *, *, #41030, .T. ) ;
#12541 = LINE ( 'NONE', #44365, #28662 ) ;
#12542 = DIRECTION ( 'NONE',  ( 0.000000000000000000, 0.7071067811865475727, 0.7071067811865475727 ) ) ;
#12543 = DIRECTION ( 'NONE',  ( 0.000000000000000000, 0.000000000000000000, -1.000000000000000000 ) ) ;
#12544 = ORIENTED_EDGE ( 'NONE', *, *, #38807, .F. ) ;
#12545 = CYLINDRICAL_SURFACE ( 'NONE', #40570, 0.5000000000079367624 ) ;
#12546 = CARTESIAN_POINT ( 'NONE',  ( -4.135079735113208699, -3.677663764522613121, 54.00000000000000711 ) ) ;
#12547 = DIRECTION ( 'NONE',  ( -0.7071067811865475727, 0.000000000000000000, -0.7071067811865475727 ) ) ;
#12548 = CIRCLE ( 'NONE', #6904, 1.000000000000000000 ) ;
#12549 = CARTESIAN_POINT ( 'NONE',  ( 0.000000000000000000, -7.449999999999998401, -24.50000000000000000 ) ) ;
#12550 = CARTESIAN_POINT ( 'NONE',  ( -7.593516549646838421, -11.78648345035340839, 455.0000000000000568 ) ) ;
#12551 = ORIENTED_EDGE ( 'NONE', *, *, #25118, .F. ) ;
#12552 = FACE_OUTER_BOUND ( 'NONE', #65866, .T. ) ;
#12553 = DIRECTION ( 'NONE',  ( -0.000000000000000000, -0.000000000000000000, -1.000000000000000000 ) ) ;
#12554 = LINE ( 'NONE', #6585, #23190 ) ;
#12555 = DIRECTION ( 'NONE',  ( 0.000000000000000000, -0.7051282051282052876, -0.7090798363602477394 ) ) ;
#12556 = CARTESIAN_POINT ( 'NONE',  ( 7.616533956692197016, 8.393516549646621527, 195.0000000000000284 ) ) ;
#12557 = EDGE_CURVE ( 'NONE', #51508, #2931, #3172, .T. ) ;
#12558 = ORIENTED_EDGE ( 'NONE', *, *, #57820, .T. ) ;
#12559 = VERTEX_POINT ( 'NONE', #67529 ) ;
#12560 = EDGE_CURVE ( 'NONE', #35777, #2319, #69446, .T. ) ;
#12561 = DIRECTION ( 'NONE',  ( 1.000000000000000000, -0.000000000000000000, -0.000000000000000000 ) ) ;
#12562 = VECTOR ( 'NONE', #51846, 1000.000000000000000 ) ;
#12563 = DIRECTION ( 'NONE',  ( 0.000000000000000000, 0.000000000000000000, 1.000000000000000000 ) ) ;
#12564 = ORIENTED_EDGE ( 'NONE', *, *, #50774, .F. ) ;
#12565 = DIRECTION ( 'NONE',  ( 0.000000000000000000, 0.000000000000000000, 1.000000000000000000 ) ) ;
#12566 = VERTEX_POINT ( 'NONE', #29322 ) ;
#12567 = CARTESIAN_POINT ( 'NONE',  ( 52.83090410532631864, 5.657408540445001854, 0.000000000000000000 ) ) ;
#12568 = EDGE_LOOP ( 'NONE', ( #12962, #46430, #65470, #34328 ) ) ;
#12569 = ORIENTED_EDGE ( 'NONE', *, *, #31305, .F. ) ;
#12570 = CARTESIAN_POINT ( 'NONE',  ( 2.290483450353367534, 9.828310488885982465, 195.0000000000000284 ) ) ;
#12571 = DIRECTION ( 'NONE',  ( 0.000000000000000000, 0.5625376724249369076, 0.8267716535433071723 ) ) ;
#12572 = PLANE ( 'NONE',  #12367 ) ;
#12573 = CARTESIAN_POINT ( 'NONE',  ( 7.000000000000000000, -31.30000000000000071, 8.400000000000000355 ) ) ;
#12574 = AXIS2_PLACEMENT_3D ( 'NONE', #63335, #49162, #6031 ) ;
#12575 = ORIENTED_EDGE ( 'NONE', *, *, #55889, .T. ) ;
#12576 = ORIENTED_EDGE ( 'NONE', *, *, #49126, .T. ) ;
#12577 = CARTESIAN_POINT ( 'NONE',  ( -7.450000000000001954, 0.000000000000000000, -14.50000000000000000 ) ) ;
#12578 = DIRECTION ( 'NONE',  ( -0.7671651518152895477, 0.6414496315691698980, -2.309356642088442522E-17 ) ) ;
#12579 = ORIENTED_EDGE ( 'NONE', *, *, #48950, .F. ) ;
#12580 = EDGE_LOOP ( 'NONE', ( #30065, #27149, #9383, #8485 ) ) ;
#12581 = AXIS2_PLACEMENT_3D ( 'NONE', #4350, #25910, #69376 ) ;
#12582 = CLOSED_SHELL ( 'NONE', ( #68626, #42533, #3458, #40407, #40882, #21905, #58306, #47250, #23960, #13811 ) ) ;
#12583 = ORIENTED_EDGE ( 'NONE', *, *, #3720, .T. ) ;
#12584 = DIRECTION ( 'NONE',  ( 0.000000000000000000, -0.000000000000000000, -1.000000000000000000 ) ) ;
#12586 = VERTEX_POINT ( 'NONE', #40984 ) ;
#12585 = DIRECTION ( 'NONE',  ( -6.508391731846281342E-15, -1.000000000000000000, -1.836970198721024757E-16 ) ) ;
#12587 = AXIS2_PLACEMENT_3D ( 'NONE', #19793, #8486, #30063 ) ;
#12588 = ADVANCED_FACE ( 'NONE', ( #8451 ), #35677, .F. ) ;
#12589 = DIRECTION ( 'NONE',  ( 1.836970198721029934E-16, 1.836970198721010706E-16, -1.000000000000000000 ) ) ;
#12590 = DIRECTION ( 'NONE',  ( 0.000000000000000000, 0.000000000000000000, 1.000000000000000000 ) ) ;
#12591 = VERTEX_POINT ( 'NONE', #41691 ) ;
#12592 = ADVANCED_FACE ( 'NONE', ( #46998 ), #13768, .F. ) ;
#12593 = ORIENTED_EDGE ( 'NONE', *, *, #47215, .T. ) ;
#12594 = VECTOR ( 'NONE', #14120, 1000.000000000000000 ) ;
#12595 = ADVANCED_FACE ( 'NONE', ( #24735 ), #35315, .T. ) ;
#12596 = EDGE_CURVE ( 'NONE', #50286, #40232, #56214, .T. ) ;
#12597 = LINE ( 'NONE', #44773, #32664 ) ;
#12598 = DIRECTION ( 'NONE',  ( 0.7671651518152895477, -0.6414496315691698980, 0.000000000000000000 ) ) ;
#12599 = EDGE_CURVE ( 'NONE', #36429, #12509, #50892, .T. ) ;
#12600 = EDGE_CURVE ( 'NONE', #28426, #66278, #68387, .T. ) ;
#12601 = CARTESIAN_POINT ( 'NONE',  ( 41.09999999999999432, 13.66939075806899950, 20.80000000000000426 ) ) ;
#12602 = EDGE_CURVE ( 'NONE', #21845, #28990, #68216, .T. ) ;
#12603 = LINE ( 'NONE', #55421, #52582 ) ;
#12604 = CARTESIAN_POINT ( 'NONE',  ( 8.689999999999999503, 8.750000000000000000, -7.000000000000000000 ) ) ;
#12605 = AXIS2_PLACEMENT_3D ( 'NONE', #31605, #53180, #4391 ) ;
#12606 = ORIENTED_EDGE ( 'NONE', *, *, #51742, .F. ) ;
#12607 = EDGE_LOOP ( 'NONE', ( #59989, #50202, #28266, #60270 ) ) ;
#12608 = LINE ( 'NONE', #32809, #7202 ) ;
#12609 = FACE_OUTER_BOUND ( 'NONE', #21156, .T. ) ;
#12610 = DIRECTION ( 'NONE',  ( -0.000000000000000000, -0.000000000000000000, 1.000000000000000000 ) ) ;
#12611 = CYLINDRICAL_SURFACE ( 'NONE', #129, 0.3999999999999993006 ) ;
#12612 = LINE ( 'NONE', #60723, #66972 ) ;
#12613 = ORIENTED_EDGE ( 'NONE', *, *, #62506, .T. ) ;
#12614 = DIRECTION ( 'NONE',  ( 1.000000000000000000, -0.000000000000000000, -0.000000000000000000 ) ) ;
#12615 = LINE ( 'NONE', #55096, #56452 ) ;
#12616 = VECTOR ( 'NONE', #13843, 1000.000000000000000 ) ;
#12617 = CARTESIAN_POINT ( 'NONE',  ( -9.547976262117256141, 2.530476262117183683, 54.00000000000000711 ) ) ;
#12618 = DIRECTION ( 'NONE',  ( 0.000000000000000000, 0.000000000000000000, -1.000000000000000000 ) ) ;
#12619 = PRODUCT_DEFINITION_SHAPE ( 'NONE', 'NONE',  #69997 ) ;
#12620 = DIRECTION ( 'NONE',  ( 1.000000000000000000, 0.000000000000000000, 0.000000000000000000 ) ) ;
#12621 = DIRECTION ( 'NONE',  ( 1.000000000000000000, -0.000000000000000000, 0.000000000000000000 ) ) ;
#12622 = CARTESIAN_POINT ( 'NONE',  ( 47.00000000000000000, 0.000000000000000000, 0.000000000000000000 ) ) ;
#12623 = ORIENTED_EDGE ( 'NONE', *, *, #45719, .T. ) ;
#12624 = DIRECTION ( 'NONE',  ( 0.000000000000000000, 0.000000000000000000, 1.000000000000000000 ) ) ;
#12625 = DIRECTION ( 'NONE',  ( -1.000000000000000000, -5.013651664672856055E-16, 0.000000000000000000 ) ) ;
#12626 = ORIENTED_EDGE ( 'NONE', *, *, #42234, .T. ) ;
#12627 = CARTESIAN_POINT ( 'NONE',  ( 41.09999999999999432, 20.60000000000000142, 13.86939075806900057 ) ) ;
#12628 = VECTOR ( 'NONE', #11871, 1000.000000000000000 ) ;
#12629 = DIRECTION ( 'NONE',  ( 0.000000000000000000, 1.000000000000000000, 0.000000000000000000 ) ) ;
#12630 = LINE ( 'NONE', #33863, #9533 ) ;
#12631 = LINE ( 'NONE', #11944, #10455 ) ;
#12632 = CARTESIAN_POINT ( 'NONE',  ( 39.90000000000000568, -0.2000000000000000111, 0.000000000000000000 ) ) ;
#12633 = VECTOR ( 'NONE', #24328, 1000.000000000000000 ) ;
#12634 = ORIENTED_EDGE ( 'NONE', *, *, #48084, .T. ) ;
#12635 = CARTESIAN_POINT ( 'NONE',  ( 283.0000000000000568, -39.80000000000000426, 12.69999999999999929 ) ) ;
#12636 = EDGE_CURVE ( 'NONE', #16237, #40446, #24023, .T. ) ;
#12637 = ORIENTED_EDGE ( 'NONE', *, *, #20451, .T. ) ;
#12638 = CARTESIAN_POINT ( 'NONE',  ( -7.250000000000000888, 7.450000000000003730, -13.50000000000000178 ) ) ;
#12639 = ORIENTED_EDGE ( 'NONE', *, *, #22905, .T. ) ;
#12640 = EDGE_CURVE ( 'NONE', #39282, #52775, #25437, .T. ) ;
#12641 = LINE ( 'NONE', #56833, #66402 ) ;
#12642 = EDGE_CURVE ( 'NONE', #2475, #14185, #46291, .T. ) ;
#12643 = CIRCLE ( 'NONE', #30745, 4.000000000000001776 ) ;
#12644 = EDGE_CURVE ( 'NONE', #19811, #63685, #3519, .T. ) ;
#12645 = DIRECTION ( 'NONE',  ( 1.047444401652939849E-14, 1.000000000000000000, 1.836970198721029934E-16 ) ) ;
#12646 = CARTESIAN_POINT ( 'NONE',  ( 8.250000000000005329, 7.250000000000000888, -26.00000000000001066 ) ) ;
#12647 = VERTEX_POINT ( 'NONE', #45584 ) ;
#12648 = ORIENTED_EDGE ( 'NONE', *, *, #11263, .F. ) ;
#12649 = PLANE ( 'NONE',  #14946 ) ;
#12650 = VERTEX_POINT ( 'NONE', #57605 ) ;
#12651 = ORIENTED_EDGE ( 'NONE', *, *, #10473, .F. ) ;
#12652 = DIRECTION ( 'NONE',  ( -0.000000000000000000, -0.000000000000000000, -1.000000000000000000 ) ) ;
#12653 = LINE ( 'NONE', #34218, #64080 ) ;
#12654 = CARTESIAN_POINT ( 'NONE',  ( 38.90000000000000568, 0.000000000000000000, 0.000000000000000000 ) ) ;
#12655 = ORIENTED_EDGE ( 'NONE', *, *, #48346, .T. ) ;
#12656 = CARTESIAN_POINT ( 'NONE',  ( 3.552713678800500929E-15, 17.79289321881343255, -20.50000000000000355 ) ) ;
#12658 = CARTESIAN_POINT ( 'NONE',  ( -11.31351654964670850, 4.193516549646605363, 455.0000000000000568 ) ) ;
#12657 = DIRECTION ( 'NONE',  ( 0.000000000000000000, 0.000000000000000000, 1.000000000000000000 ) ) ;
#12659 = ORIENTED_EDGE ( 'NONE', *, *, #48414, .F. ) ;
#12661 = ORIENTED_EDGE ( 'NONE', *, *, #7164, .F. ) ;
#12660 = DIRECTION ( 'NONE',  ( -0.000000000000000000, -1.000000000000000000, -0.000000000000000000 ) ) ;
#12662 = CIRCLE ( 'NONE', #31936, 7.300000000000000711 ) ;
#12663 = ORIENTED_EDGE ( 'NONE', *, *, #2803, .T. ) ;
#12664 = CARTESIAN_POINT ( 'NONE',  ( -1.040834214723497966E-13, 9.833141174520228844, 455.0000000000001137 ) ) ;
#12665 = PLANE ( 'NONE',  #68285 ) ;
#12666 = AXIS2_PLACEMENT_3D ( 'NONE', #15530, #10905, #53697 ) ;
#12667 = ORIENTED_EDGE ( 'NONE', *, *, #28509, .F. ) ;
#12668 = EDGE_CURVE ( 'NONE', #43731, #21439, #3871, .T. ) ;
#12669 = DIRECTION ( 'NONE',  ( -1.000000000000000000, 0.000000000000000000, 0.000000000000000000 ) ) ;
#12670 = DIRECTION ( 'NONE',  ( -1.000000000000000000, 0.000000000000000000, 0.000000000000000000 ) ) ;
#12671 = ORIENTED_EDGE ( 'NONE', *, *, #5930, .T. ) ;
#12672 = ORIENTED_EDGE ( 'NONE', *, *, #1324, .F. ) ;
#12673 = CIRCLE ( 'NONE', #11527, 3.499999999999855227 ) ;
#12674 = DIRECTION ( 'NONE',  ( -0.000000000000000000, 3.673940397442059868E-16, -1.000000000000000000 ) ) ;
#12675 = CARTESIAN_POINT ( 'NONE',  ( 290.0000000000000000, -21.00000000000000000, 5.000000000000000000 ) ) ;
#12676 = AXIS2_PLACEMENT_3D ( 'NONE', #17456, #48609, #38004 ) ;
#12677 = VERTEX_POINT ( 'NONE', #67160 ) ;
#12678 = CARTESIAN_POINT ( 'NONE',  ( 11.50000000000000000, -11.50000000000100009, -15.00000000000084910 ) ) ;
#12679 = DIRECTION ( 'NONE',  ( -1.836970198721029934E-16, 1.836970198721036344E-16, -1.000000000000000000 ) ) ;
#12680 = EDGE_CURVE ( 'NONE', #50148, #61414, #24383, .T. ) ;
#12681 = DIRECTION ( 'NONE',  ( 0.000000000000000000, 0.000000000000000000, 1.000000000000000000 ) ) ;
#12682 = EDGE_CURVE ( 'NONE', #22714, #38860, #40290, .T. ) ;
#12683 = ORIENTED_EDGE ( 'NONE', *, *, #35168, .F. ) ;
#12684 = VECTOR ( 'NONE', #37651, 1000.000000000000000 ) ;
#12685 = EDGE_CURVE ( 'NONE', #49587, #49641, #1742, .T. ) ;
#12686 = FACE_OUTER_BOUND ( 'NONE', #32234, .T. ) ;
#12687 = CARTESIAN_POINT ( 'NONE',  ( 14.25000000000000000, -0.2038245569916330158, -23.22168783648699986 ) ) ;
#12689 = ORIENTED_EDGE ( 'NONE', *, *, #7858, .F. ) ;
#12688 = FILL_AREA_STYLE ('',( #60794 ) ) ;
#12691 = ORIENTED_EDGE ( 'NONE', *, *, #34163, .F. ) ;
#12690 = DIRECTION ( 'NONE',  ( -0.6414496315691494699, -0.7671651518153064231, -0.000000000000000000 ) ) ;
#12693 = CARTESIAN_POINT ( 'NONE',  ( 7.811466277050736373, -7.272650909786728235, 455.0000000000000568 ) ) ;
#12692 = VECTOR ( 'NONE', #1595, 1000.000000000000000 ) ;
#12694 = AXIS2_PLACEMENT_3D ( 'NONE', #36861, #9272, #47108 ) ;
#12695 = DIRECTION ( 'NONE',  ( 0.000000000000000000, -0.000000000000000000, 1.000000000000000000 ) ) ;
#12696 = DIRECTION ( 'NONE',  ( -0.000000000000000000, 3.673940397442059868E-16, -1.000000000000000000 ) ) ;
#12697 = CARTESIAN_POINT ( 'NONE',  ( 6.364920264886885448, -3.677663764522628664, 54.00000000000000711 ) ) ;
#12698 = VECTOR ( 'NONE', #7055, 1000.000000000000000 ) ;
#12699 = DIRECTION ( 'NONE',  ( -1.000000000000000000, 0.000000000000000000, 0.000000000000000000 ) ) ;
#12700 = ORIENTED_EDGE ( 'NONE', *, *, #407, .T. ) ;
#12701 = DIRECTION ( 'NONE',  ( -9.912705577010435793E-15, -1.000000000000000000, 0.000000000000000000 ) ) ;
#12702 = DIRECTION ( 'NONE',  ( 0.000000000000000000, 1.000000000000000000, 0.000000000000000000 ) ) ;
#12703 = DIRECTION ( 'NONE',  ( 1.000000000000000000, 0.000000000000000000, 0.000000000000000000 ) ) ;
#12705 = ORIENTED_EDGE ( 'NONE', *, *, #64533, .T. ) ;
#12704 = CARTESIAN_POINT ( 'NONE',  ( 3.003254798005744242, -6.872275254348413576, 54.00000000000000711 ) ) ;
#12706 = DIRECTION ( 'NONE',  ( 0.000000000000000000, 0.000000000000000000, 1.000000000000000000 ) ) ;
#12707 = VECTOR ( 'NONE', #19136, 1000.000000000000000 ) ;
#12708 = CARTESIAN_POINT ( 'NONE',  ( -7.250000000000000888, 7.450000000000003730, -12.50000000000000000 ) ) ;
#12709 = ORIENTED_EDGE ( 'NONE', *, *, #68032, .T. ) ;
#12710 = DIRECTION ( 'NONE',  ( 0.000000000000000000, 0.6857142857142869419, -0.7278708115918273158 ) ) ;
#12711 = DIRECTION ( 'NONE',  ( -1.836970198721029934E-16, 1.836970198721036590E-16, -1.000000000000000000 ) ) ;
#12712 = VECTOR ( 'NONE', #59884, 1000.000000000000000 ) ;
#12713 = ORIENTED_EDGE ( 'NONE', *, *, #3751, .T. ) ;
#12714 = CARTESIAN_POINT ( 'NONE',  ( -10.19191654964671301, 11.47551654964660450, 195.0000000000000284 ) ) ;
#12715 = DIRECTION ( 'NONE',  ( 1.000000000000000000, 0.000000000000000000, 0.000000000000000000 ) ) ;
#12716 = DIRECTION ( 'NONE',  ( 0.000000000000000000, 1.000000000000000000, 0.000000000000000000 ) ) ;
#12717 = VECTOR ( 'NONE', #62813, 1000.000000000000114 ) ;
#12718 = DIRECTION ( 'NONE',  ( 0.000000000000000000, 1.000000000000000000, -0.000000000000000000 ) ) ;
#12719 = DIRECTION ( 'NONE',  ( 0.000000000000000000, 0.000000000000000000, 1.000000000000000000 ) ) ;
#12720 = ORIENTED_EDGE ( 'NONE', *, *, #11399, .T. ) ;
#12721 = FACE_OUTER_BOUND ( 'NONE', #43651, .T. ) ;
#12722 = EDGE_LOOP ( 'NONE', ( #5837, #42142, #61794, #41940 ) ) ;
#12723 = ORIENTED_EDGE ( 'NONE', *, *, #61311, .T. ) ;
#12724 = CIRCLE ( 'NONE', #21791, 0.1749999999999998224 ) ;
#12725 = EDGE_CURVE ( 'NONE', #51349, #25131, #53366, .T. ) ;
#12726 = EDGE_CURVE ( 'NONE', #5737, #25046, #64962, .T. ) ;
#12727 = DIRECTION ( 'NONE',  ( 0.000000000000000000, -0.7071067811865454633, -0.7071067811865496822 ) ) ;
#12728 = EDGE_CURVE ( 'NONE', #16384, #37841, #42041, .T. ) ;
#12729 = EDGE_CURVE ( 'NONE', #2339, #9556, #69267, .T. ) ;
#12730 =( NAMED_UNIT ( * ) SI_UNIT ( $, .STERADIAN. ) SOLID_ANGLE_UNIT ( ) );
#12731 = FACE_OUTER_BOUND ( 'NONE', #53429, .T. ) ;
#12732 = ORIENTED_EDGE ( 'NONE', *, *, #66486, .T. ) ;
#12733 = ORIENTED_EDGE ( 'NONE', *, *, #40526, .T. ) ;
#12734 = CARTESIAN_POINT ( 'NONE',  ( -7.250000000000000888, 8.250000000000001776, -9.000000000000001776 ) ) ;
#12735 = ORIENTED_EDGE ( 'NONE', *, *, #7594, .T. ) ;
#12736 = CARTESIAN_POINT ( 'NONE',  ( 5.257023737882819070, -5.257023737882825287, 54.00000000000000711 ) ) ;
#12737 = VECTOR ( 'NONE', #18057, 1000.000000000000000 ) ;
#12738 = DIRECTION ( 'NONE',  ( -0.000000000000000000, -0.000000000000000000, 1.000000000000000000 ) ) ;
#12739 = CARTESIAN_POINT ( 'NONE',  ( 10.92648345035337343, -9.306483450353493225, 455.0000000000000568 ) ) ;
#12740 = CIRCLE ( 'NONE', #39841, 3.499999999999054534 ) ;
#12741 = CARTESIAN_POINT ( 'NONE',  ( -10.30047626211725742, 3.842976262117182351, 54.00000000000000711 ) ) ;
#12743 = CARTESIAN_POINT ( 'NONE',  ( 41.09999999999999432, 13.66939075806899950, -20.80000000000000426 ) ) ;
#12742 = CARTESIAN_POINT ( 'NONE',  ( 16.89194109070750116, -5.000000000000000000, -26.25000000000000000 ) ) ;
#12744 =( GEOMETRIC_REPRESENTATION_CONTEXT ( 3 ) GLOBAL_UNCERTAINTY_ASSIGNED_CONTEXT ( ( #63503 ) ) GLOBAL_UNIT_ASSIGNED_CONTEXT ( ( #4504, #37375, #64588 ) ) REPRESENTATION_CONTEXT ( 'NONE', 'WORKASPACE' ) );
#12745 = ORIENTED_EDGE ( 'NONE', *, *, #24137, .T. ) ;
#12747 = EDGE_LOOP ( 'NONE', ( #50686, #5673, #27575, #25943 ) ) ;
#12746 = DIRECTION ( 'NONE',  ( -0.7071067811865474617, 0.000000000000000000, 0.7071067811865474617 ) ) ;
#12748 = ORIENTED_EDGE ( 'NONE', *, *, #3354, .T. ) ;
#12749 = ORIENTED_EDGE ( 'NONE', *, *, #19568, .F. ) ;
#12750 = ADVANCED_FACE ( 'NONE', ( #48046 ), #64652, .T. ) ;
#12751 = VECTOR ( 'NONE', #3768, 1000.000000000000000 ) ;
#12752 = DIRECTION ( 'NONE',  ( -0.000000000000000000, -0.000000000000000000, -1.000000000000000000 ) ) ;
#12753 = FACE_OUTER_BOUND ( 'NONE', #5020, .T. ) ;
#12754 = VECTOR ( 'NONE', #54803, 1000.000000000000000 ) ;
#12755 = DIRECTION ( 'NONE',  ( -7.665540703601096574E-15, -1.000000000000000000, 0.000000000000000000 ) ) ;
#12756 = ORIENTED_EDGE ( 'NONE', *, *, #6405, .T. ) ;
#12757 = ORIENTED_EDGE ( 'NONE', *, *, #51675, .F. ) ;
#12758 = CARTESIAN_POINT ( 'NONE',  ( 5.257023737882819070, -7.186223737882822427, 54.00000000000000711 ) ) ;
#12759 = CARTESIAN_POINT ( 'NONE',  ( 30.00000000000000000, -17.50000000000000000, 15.70500000000000007 ) ) ;
#12760 = AXIS2_PLACEMENT_3D ( 'NONE', #68322, #57711, #52419 ) ;
#12761 = VERTEX_POINT ( 'NONE', #4920 ) ;
#12762 = EDGE_LOOP ( 'NONE', ( #51760, #4351, #66348, #8598 ) ) ;
#12763 = CARTESIAN_POINT ( 'NONE',  ( -7.813516549646839948, -12.00648345035340903, 455.0000000000000568 ) ) ;
#12764 = AXIS2_PLACEMENT_3D ( 'NONE', #65991, #59670, #11896 ) ;
#12765 = FACE_OUTER_BOUND ( 'NONE', #11320, .T. ) ;
#12766 = EDGE_LOOP ( 'NONE', ( #37925, #43116, #23813, #21541, #14200, #63207, #18099, #5353 ) ) ;
#12767 = EDGE_CURVE ( 'NONE', #53797, #17980, #53022, .T. ) ;
#12768 = EDGE_CURVE ( 'NONE', #48721, #25046, #65010, .T. ) ;
#12769 = CARTESIAN_POINT ( 'NONE',  ( -25.50000000000000355, -15.50000000000000000, -20.49999999999999645 ) ) ;
#12770 = EDGE_CURVE ( 'NONE', #54447, #55741, #32251, .T. ) ;
#12771 = VECTOR ( 'NONE', #41651, 1000.000000000000000 ) ;
#12772 = ORIENTED_EDGE ( 'NONE', *, *, #26621, .F. ) ;
#12773 = ORIENTED_EDGE ( 'NONE', *, *, #2427, .F. ) ;
#12774 = DIRECTION ( 'NONE',  ( -1.000000000000000000, 0.000000000000000000, 0.000000000000000000 ) ) ;
#12775 = DIRECTION ( 'NONE',  ( 0.000000000000000000, 0.000000000000000000, -1.000000000000000000 ) ) ;
#12776 = EDGE_CURVE ( 'NONE', #57591, #64137, #32134, .T. ) ;
#12777 = LINE ( 'NONE', #65850, #26141 ) ;
#12778 = CARTESIAN_POINT ( 'NONE',  ( 7.000000000000000000, -27.13000000000000611, -13.50000000000000000 ) ) ;
#12779 = FACE_OUTER_BOUND ( 'NONE', #33128, .T. ) ;
#12780 = DIRECTION ( 'NONE',  ( -1.794541526872559352E-16, -1.000000000000000000, 0.000000000000000000 ) ) ;
#12781 = EDGE_CURVE ( 'NONE', #56261, #40969, #57954, .T. ) ;
#12782 = EDGE_CURVE ( 'NONE', #29317, #52054, #52675, .T. ) ;
#12783 = CARTESIAN_POINT ( 'NONE',  ( -7.450000000000001954, 0.000000000000000000, -22.50000000000000000 ) ) ;
#12784 = ORIENTED_EDGE ( 'NONE', *, *, #16553, .T. ) ;
#12785 = DIRECTION ( 'NONE',  ( -0.000000000000000000, -0.000000000000000000, -1.000000000000000000 ) ) ;
#12786 = ADVANCED_FACE ( 'NONE', ( #4232 ), #15874, .T. ) ;
#12788 = ORIENTED_EDGE ( 'NONE', *, *, #19735, .T. ) ;
#12787 = PLANE ( 'NONE',  #46847 ) ;
#12789 = CARTESIAN_POINT ( 'NONE',  ( 8.580623737882818958, -8.930623737882855906, 54.00000000000000711 ) ) ;
#12790 = VECTOR ( 'NONE', #44547, 1000.000000000000000 ) ;
#12791 = VECTOR ( 'NONE', #39791, 1000.000000000000000 ) ;
#12792 = DIRECTION ( 'NONE',  ( 0.000000000000000000, 0.000000000000000000, 1.000000000000000000 ) ) ;
#12793 = DIRECTION ( 'NONE',  ( 0.000000000000000000, -2.206568261432184716E-12, 1.000000000000000000 ) ) ;
#12795 = DIRECTION ( 'NONE',  ( -1.000000000000000000, 0.000000000000000000, 0.000000000000000000 ) ) ;
#12794 = VECTOR ( 'NONE', #12983, 1000.000000000000000 ) ;
#12796 = VECTOR ( 'NONE', #50045, 1000.000000000000000 ) ;
#12797 = DIRECTION ( 'NONE',  ( 0.000000000000000000, 0.000000000000000000, -1.000000000000000000 ) ) ;
#12798 = AXIS2_PLACEMENT_3D ( 'NONE', #22698, #33313, #11051 ) ;
#12799 = ORIENTED_EDGE ( 'NONE', *, *, #56914, .T. ) ;
#12800 = ORIENTED_EDGE ( 'NONE', *, *, #37009, .F. ) ;
#12801 = VECTOR ( 'NONE', #6961, 1000.000000000000000 ) ;
#12802 = FACE_OUTER_BOUND ( 'NONE', #1637, .T. ) ;
#12803 = AXIS2_PLACEMENT_3D ( 'NONE', #5762, #32970, #26982 ) ;
#12804 = CARTESIAN_POINT ( 'NONE',  ( 8.250000000000005329, 7.250000000000000888, -26.00000000000001066 ) ) ;
#12805 = CARTESIAN_POINT ( 'NONE',  ( 275.5000000000000000, -42.00000000000000000, 27.00000000000000000 ) ) ;
#12806 = ORIENTED_EDGE ( 'NONE', *, *, #40324, .F. ) ;
#12807 = DIRECTION ( 'NONE',  ( 1.000000000000000000, 0.000000000000000000, 0.000000000000000000 ) ) ;
#12808 = VERTEX_POINT ( 'NONE', #10914 ) ;
#12809 = ORIENTED_EDGE ( 'NONE', *, *, #59666, .F. ) ;
#12810 = FACE_OUTER_BOUND ( 'NONE', #60582, .T. ) ;
#12811 = CARTESIAN_POINT ( 'NONE',  ( 152.0064834503532722, 2.160375375128253950, 0.000000000000000000 ) ) ;
#12812 = VERTEX_POINT ( 'NONE', #25797 ) ;
#12813 = CARTESIAN_POINT ( 'NONE',  ( 11.34648345035330053, 1.077516549646569066, 195.0000000000000284 ) ) ;
#12814 = CARTESIAN_POINT ( 'NONE',  ( -15.50000000000000000, -17.50000000000000000, -22.50000000000000000 ) ) ;
#12815 = DIRECTION ( 'NONE',  ( 0.000000000000000000, 0.000000000000000000, 1.000000000000000000 ) ) ;
#12816 = ORIENTED_EDGE ( 'NONE', *, *, #37945, .F. ) ;
#12817 = ORIENTED_EDGE ( 'NONE', *, *, #13777, .T. ) ;
#12819 = VERTEX_POINT ( 'NONE', #15542 ) ;
#12818 = CARTESIAN_POINT ( 'NONE',  ( 290.0000000000000000, -0.5000000000000000000, 26.50000000000000000 ) ) ;
#12820 = EDGE_LOOP ( 'NONE', ( #42364, #25435, #18516, #69830 ) ) ;
#12821 = CARTESIAN_POINT ( 'NONE',  ( 11.00000000000000000, -9.487228132326899654, -12.50000000000000000 ) ) ;
#12822 = LINE ( 'NONE', #34387, #43356 ) ;
#12823 = CYLINDRICAL_SURFACE ( 'NONE', #45903, 2.204799999999996540 ) ;
#12824 = PLANE ( 'NONE',  #14998 ) ;
#12825 = DIRECTION ( 'NONE',  ( -0.000000000000000000, 1.000000000000000000, -0.000000000000000000 ) ) ;
#12826 = EDGE_CURVE ( 'NONE', #23956, #46196, #3989, .T. ) ;
#12827 = FACE_OUTER_BOUND ( 'NONE', #23887, .T. ) ;
#12828 = EDGE_LOOP ( 'NONE', ( #23707, #54320, #50330, #26174 ) ) ;
#12829 = ORIENTED_EDGE ( 'NONE', *, *, #24536, .T. ) ;
#12830 = ORIENTED_EDGE ( 'NONE', *, *, #22755, .F. ) ;
#12831 = EDGE_CURVE ( 'NONE', #55252, #56315, #63625, .T. ) ;
#12832 = DIRECTION ( 'NONE',  ( 0.000000000000000000, 0.000000000000000000, 1.000000000000000000 ) ) ;
#12833 = APPLICATION_CONTEXT ( 'automotive_design' ) ;
#12834 = DIRECTION ( 'NONE',  ( -1.000000000000000000, 0.000000000000000000, 0.000000000000000000 ) ) ;
#12835 = DIRECTION ( 'NONE',  ( 1.000000000000000000, -0.000000000000000000, 0.000000000000000000 ) ) ;
#12836 = CIRCLE ( 'NONE', #33204, 2.215251240775983899 ) ;
#12837 = CIRCLE ( 'NONE', #42239, 1.929199999999998028 ) ;
#12838 = EDGE_LOOP ( 'NONE', ( #39428, #43601, #19082, #53400 ) ) ;
#12840 = EDGE_CURVE ( 'NONE', #13397, #52106, #27183, .T. ) ;
#12839 = VERTEX_POINT ( 'NONE', #47348 ) ;
#12841 = VERTEX_POINT ( 'NONE', #10563 ) ;
#12842 = DIRECTION ( 'NONE',  ( -1.000000000000000000, 0.000000000000000000, 0.000000000000000000 ) ) ;
#12843 = ORIENTED_EDGE ( 'NONE', *, *, #67554, .F. ) ;
#12844 = AXIS2_PLACEMENT_3D ( 'NONE', #63378, #57365, #48167 ) ;
#12845 = VECTOR ( 'NONE', #66976, 1000.000000000000000 ) ;
#12846 = ORIENTED_EDGE ( 'NONE', *, *, #29796, .T. ) ;
#12847 = ADVANCED_FACE ( 'NONE', ( #48399 ), #69963, .F. ) ;
#12848 = ORIENTED_EDGE ( 'NONE', *, *, #40177, .T. ) ;
#12849 = ORIENTED_EDGE ( 'NONE', *, *, #47980, .F. ) ;
#12850 = CARTESIAN_POINT ( 'NONE',  ( -3.710438382363173027, -7.408280051175170300, 26.00000000000000711 ) ) ;
#12851 = CIRCLE ( 'NONE', #17357, 0.1999999999999987899 ) ;
#12853 = ORIENTED_EDGE ( 'NONE', *, *, #32941, .T. ) ;
#12852 = FACE_OUTER_BOUND ( 'NONE', #67939, .T. ) ;
#12854 = DIRECTION ( 'NONE',  ( 1.000000000000000000, 0.000000000000000000, 0.000000000000000000 ) ) ;
#12855 = CARTESIAN_POINT ( 'NONE',  ( 152.0064834503532722, 2.160375375128253950, 5.000000000000000000 ) ) ;
#12856 = ADVANCED_FACE ( 'NONE', ( #20476 ), #36747, .F. ) ;
#12857 = LINE ( 'NONE', #13923, #50506 ) ;
#12859 = ORIENTED_EDGE ( 'NONE', *, *, #51764, .T. ) ;
#12858 = FACE_OUTER_BOUND ( 'NONE', #43216, .T. ) ;
#12860 = CIRCLE ( 'NONE', #37730, 4.500000000000191847 ) ;
#12861 = EDGE_LOOP ( 'NONE', ( #58453, #29175, #9, #56231 ) ) ;
#12862 = FACE_OUTER_BOUND ( 'NONE', #26436, .T. ) ;
#12863 = FACE_OUTER_BOUND ( 'NONE', #49697, .T. ) ;
#12864 = CARTESIAN_POINT ( 'NONE',  ( 25.50000000000000355, -5.578999999999999737, 22.50000000000000000 ) ) ;
#12865 = EDGE_CURVE ( 'NONE', #3828, #29489, #12271, .T. ) ;
#12866 = ORIENTED_EDGE ( 'NONE', *, *, #30744, .T. ) ;
#12867 = CARTESIAN_POINT ( 'NONE',  ( -6.344366288193421077, -4.720772854004749775, 54.00000000000000711 ) ) ;
#12868 = EDGE_CURVE ( 'NONE', #29522, #58319, #22566, .T. ) ;
#12869 = DIRECTION ( 'NONE',  ( -1.221996412923863950E-14, -1.000000000000000000, 0.000000000000000000 ) ) ;
#12870 = CARTESIAN_POINT ( 'NONE',  ( -25.50000000000000355, -15.50000000000000000, -22.50000000000000000 ) ) ;
#12871 = EDGE_LOOP ( 'NONE', ( #43806, #18509, #54281, #64863, #23466, #9545, #13626, #8303 ) ) ;
#12872 = AXIS2_PLACEMENT_3D ( 'NONE', #43270, #37635, #69809 ) ;
#12873 = CARTESIAN_POINT ( 'NONE',  ( 78.77321854994620765, 47.95351654967443977, 29.00000000000000000 ) ) ;
#12874 = DIRECTION ( 'NONE',  ( 0.000000000000000000, 0.000000000000000000, -1.000000000000000000 ) ) ;
#12875 = CARTESIAN_POINT ( 'NONE',  ( -7.250000000000000000, -7.449999999999998401, -14.50000000000000000 ) ) ;
#12876 = EDGE_CURVE ( 'NONE', #60406, #16354, #44454, .T. ) ;
#12877 = AXIS2_PLACEMENT_3D ( 'NONE', #47012, #62928, #19776 ) ;
#12878 = ORIENTED_EDGE ( 'NONE', *, *, #57271, .T. ) ;
#12879 = DIRECTION ( 'NONE',  ( -1.000000000000000000, 0.000000000000000000, 0.000000000000000000 ) ) ;
#12880 = DIRECTION ( 'NONE',  ( -1.000000000000000000, 0.000000000000000000, 0.000000000000000000 ) ) ;
#12881 = DIRECTION ( 'NONE',  ( -2.135044278125301343E-15, 1.000000000000000000, 0.000000000000000000 ) ) ;
#12882 = FACE_OUTER_BOUND ( 'NONE', #53931, .T. ) ;
#12883 = CIRCLE ( 'NONE', #37808, 3.499999999999850342 ) ;
#12884 = AXIS2_PLACEMENT_3D ( 'NONE', #37236, #42869, #64454 ) ;
#12885 = VERTEX_POINT ( 'NONE', #34184 ) ;
#12886 = CARTESIAN_POINT ( 'NONE',  ( -9.093516549646828651, -11.12648345035338870, 455.0000000000000568 ) ) ;
#12887 = CARTESIAN_POINT ( 'NONE',  ( -7.250000000000000888, 8.250000000000001776, -26.00000000000001066 ) ) ;
#12888 = FACE_OUTER_BOUND ( 'NONE', #4498, .T. ) ;
#12889 = CARTESIAN_POINT ( 'NONE',  ( 6.665817930929297752, -7.357023737882814274, 26.00000000000000000 ) ) ;
#12890 = CARTESIAN_POINT ( 'NONE',  ( 9.404523737882817258, -1.480523737882826207, 54.00000000000000711 ) ) ;
#12891 = AXIS2_PLACEMENT_3D ( 'NONE', #2139, #45262, #50233 ) ;
#12892 = ORIENTED_EDGE ( 'NONE', *, *, #51773, .F. ) ;
#12893 = CIRCLE ( 'NONE', #47903, 1.000000000000000000 ) ;
#12894 = PLANE ( 'NONE',  #37759 ) ;
#12895 = CARTESIAN_POINT ( 'NONE',  ( -4.188533722949335569, 4.727349090213398775, 455.0000000000000568 ) ) ;
#12896 = DIRECTION ( 'NONE',  ( -0.000000000000000000, -0.000000000000000000, 1.000000000000000000 ) ) ;
#12897 = EDGE_CURVE ( 'NONE', #13736, #11767, #55774, .T. ) ;
#12898 = VECTOR ( 'NONE', #27911, 1000.000000000000000 ) ;
#12899 = DIRECTION ( 'NONE',  ( -0.000000000000000000, -0.000000000000000000, -1.000000000000000000 ) ) ;
#12900 = DIRECTION ( 'NONE',  ( -1.000000000000000000, 0.000000000000000000, 0.000000000000000000 ) ) ;
#12901 = ORIENTED_EDGE ( 'NONE', *, *, #36507, .F. ) ;
#12903 = EDGE_LOOP ( 'NONE', ( #65189, #9506, #63458, #20887, #11627, #49588, #43664, #52441, #60339, #12371, #57974, #23053, #52464, #55501, #66227, #14587, #16985, #26111, #32083, #43573, #55941, #22691, #67620, #8590, #53348, #51474, #5262, #15077, #47264, #59925, #18598, #47211, #37560, #50345 ) ) ;
#12902 = DIRECTION ( 'NONE',  ( -0.7071067811865472397, 0.5000000000000002220, -0.5000000000000002220 ) ) ;
#12904 = EDGE_CURVE ( 'NONE', #33631, #15862, #16575, .T. ) ;
#12905 = CARTESIAN_POINT ( 'NONE',  ( 8.580623737882849156, 9.689726262117156708, 54.00000000000000711 ) ) ;
#12906 = DIRECTION ( 'NONE',  ( -1.000000000000000000, 1.047444401652940007E-14, 0.000000000000000000 ) ) ;
#12907 = ORIENTED_EDGE ( 'NONE', *, *, #37612, .F. ) ;
#12908 = EDGE_CURVE ( 'NONE', #7367, #66946, #33850, .T. ) ;
#12909 = CIRCLE ( 'NONE', #28723, 0.3499999999999996447 ) ;
#12910 = DIRECTION ( 'NONE',  ( 1.836970198721029934E-16, 1.836970198721010706E-16, -1.000000000000000000 ) ) ;
#12911 = EDGE_CURVE ( 'NONE', #18339, #40441, #48049, .T. ) ;
#12912 = ORIENTED_EDGE ( 'NONE', *, *, #56527, .F. ) ;
#12913 = CARTESIAN_POINT ( 'NONE',  ( -14.24999999999999822, -0.2715193793361436736, -22.01281590054916038 ) ) ;
#12914 = ORIENTED_EDGE ( 'NONE', *, *, #56140, .T. ) ;
#12915 = ADVANCED_FACE ( 'NONE', ( #60372 ), #28543, .F. ) ;
#12916 = ORIENTED_EDGE ( 'NONE', *, *, #69396, .T. ) ;
#12917 = DIRECTION ( 'NONE',  ( 1.047444401652940007E-14, 1.000000000000000000, 0.000000000000000000 ) ) ;
#12918 = DIRECTION ( 'NONE',  ( -4.336808689942006692E-15, -1.000000000000000000, 0.000000000000000000 ) ) ;
#12919 = CARTESIAN_POINT ( 'NONE',  ( 39.00000000000000000, 21.00000000000000000, -16.96999999999999886 ) ) ;
#12920 = LINE ( 'NONE', #29895, #32521 ) ;
#12921 = EDGE_LOOP ( 'NONE', ( #68765, #9668, #24744, #22118, #62463, #46637, #30018, #56943 ) ) ;
#12922 = EDGE_CURVE ( 'NONE', #50270, #5931, #33169, .T. ) ;
#12923 = ORIENTED_EDGE ( 'NONE', *, *, #22467, .F. ) ;
#12924 = PLANE ( 'NONE',  #61712 ) ;
#12925 = EDGE_CURVE ( 'NONE', #68975, #34031, #27703, .T. ) ;
#12926 = CARTESIAN_POINT ( 'NONE',  ( -1.677516549646676625, 10.73351654964656987, 455.0000000000000568 ) ) ;
#12927 = ORIENTED_EDGE ( 'NONE', *, *, #61405, .T. ) ;
#12928 = AXIS2_PLACEMENT_3D ( 'NONE', #13693, #19686, #42315 ) ;
#12929 = ORIENTED_EDGE ( 'NONE', *, *, #33725, .F. ) ;
#12930 = EDGE_CURVE ( 'NONE', #2145, #57928, #39501, .T. ) ;
#12931 = ADVANCED_FACE ( 'NONE', ( #11583 ), #23587, .F. ) ;
#12932 = EDGE_LOOP ( 'NONE', ( #6479, #54895, #38252, #50652 ) ) ;
#12933 = LINE ( 'NONE', #10972, #46294 ) ;
#12935 = ORIENTED_EDGE ( 'NONE', *, *, #7023, .F. ) ;
#12934 = LINE ( 'NONE', #61028, #23633 ) ;
#12936 = EDGE_CURVE ( 'NONE', #52784, #53491, #22225, .T. ) ;
#12937 = LINE ( 'NONE', #40520, #39065 ) ;
#12938 = CIRCLE ( 'NONE', #54760, 5.000000000000000000 ) ;
#12939 = VECTOR ( 'NONE', #20178, 1000.000000000000000 ) ;
#12940 = CARTESIAN_POINT ( 'NONE',  ( 154.0064834503532722, -29.01119750012554732, 0.000000000000000000 ) ) ;
#12941 = ORIENTED_EDGE ( 'NONE', *, *, #24946, .T. ) ;
#12942 = VERTEX_POINT ( 'NONE', #23243 ) ;
#12943 = CIRCLE ( 'NONE', #22016, 0.5249999999999990230 ) ;
#12944 = LINE ( 'NONE', #24272, #60858 ) ;
#12945 = PLANE ( 'NONE',  #21109 ) ;
#12946 = AXIS2_PLACEMENT_3D ( 'NONE', #56339, #55643, #62331 ) ;
#12947 = EDGE_CURVE ( 'NONE', #1574, #61299, #50470, .T. ) ;
#12948 = DIRECTION ( 'NONE',  ( 0.000000000000000000, -2.123301534585676023E-12, 1.000000000000000000 ) ) ;
#12949 = EDGE_CURVE ( 'NONE', #35367, #47586, #33356, .T. ) ;
#12950 = VECTOR ( 'NONE', #48661, 1000.000000000000000 ) ;
#12951 = LINE ( 'NONE', #67426, #23344 ) ;
#12952 = LINE ( 'NONE', #29214, #64065 ) ;
#12953 = VECTOR ( 'NONE', #54566, 1000.000000000000000 ) ;
#12955 = VERTEX_POINT ( 'NONE', #27871 ) ;
#12954 = CARTESIAN_POINT ( 'NONE',  ( 55.00000000000000000, -16.96999999999999886, 21.00000000000000000 ) ) ;
#12956 = ORIENTED_EDGE ( 'NONE', *, *, #22230, .F. ) ;
#12957 = AXIS2_PLACEMENT_3D ( 'NONE', #18440, #46033, #66551 ) ;
#12958 = CYLINDRICAL_SURFACE ( 'NONE', #5016, 1.000000000000000000 ) ;
#12959 = DIRECTION ( 'NONE',  ( 0.6414496315691473605, 0.7671651518153083105, 0.000000000000000000 ) ) ;
#12960 = CARTESIAN_POINT ( 'NONE',  ( -7.250000000000000888, 7.250000000000001776, -16.50000000000000000 ) ) ;
#12961 = DIRECTION ( 'NONE',  ( 0.000000000000000000, 0.7071067811865450192, 0.7071067811865500152 ) ) ;
#12962 = ORIENTED_EDGE ( 'NONE', *, *, #30122, .T. ) ;
#12963 = DIRECTION ( 'NONE',  ( 0.000000000000000000, -1.000000000000000000, 0.000000000000000000 ) ) ;
#12964 = DIRECTION ( 'NONE',  ( -1.000000000000000000, 1.794541526872559352E-16, 0.000000000000000000 ) ) ;
#12965 = DIRECTION ( 'NONE',  ( -1.000000000000000000, 0.000000000000000000, 0.000000000000000000 ) ) ;
#12966 = DIRECTION ( 'NONE',  ( 0.000000000000000000, -1.000000000000000000, 0.000000000000000000 ) ) ;
#12967 = DIRECTION ( 'NONE',  ( 0.000000000000000000, 1.000000000000000000, 0.000000000000000000 ) ) ;
#12968 = LINE ( 'NONE', #29235, #4857 ) ;
#12969 = CARTESIAN_POINT ( 'NONE',  ( -15.50000000000000000, -0.4000000000000000222, -22.50000000000000000 ) ) ;
#12970 = ORIENTED_EDGE ( 'NONE', *, *, #59029, .F. ) ;
#12971 = CARTESIAN_POINT ( 'NONE',  ( 15.00000000000000000, -0.5000000000000000000, 26.50000000000000000 ) ) ;
#12972 = DIRECTION ( 'NONE',  ( 0.7071067811865486830, 0.7071067811865464625, 0.000000000000000000 ) ) ;
#12973 = AXIS2_PLACEMENT_3D ( 'NONE', #41453, #68323, #24497 ) ;
#12974 = ORIENTED_EDGE ( 'NONE', *, *, #64380, .T. ) ;
#12975 = DIRECTION ( 'NONE',  ( -1.836970198721029934E-16, -1.836970198721010706E-16, 1.000000000000000000 ) ) ;
#12976 = DIRECTION ( 'NONE',  ( -0.000000000000000000, -0.000000000000000000, 1.000000000000000000 ) ) ;
#12977 = CARTESIAN_POINT ( 'NONE',  ( 7.250000000000005329, -7.249999999999998224, -20.00000000000000000 ) ) ;
#12978 = AXIS2_PLACEMENT_3D ( 'NONE', #17260, #54755, #44816 ) ;
#12979 = DIRECTION ( 'NONE',  ( 1.000000000000000000, 0.000000000000000000, 0.000000000000000000 ) ) ;
#12980 = CARTESIAN_POINT ( 'NONE',  ( 1.480523737882808444, 8.598420958951642490, 26.00000000000000711 ) ) ;
#12981 = ORIENTED_EDGE ( 'NONE', *, *, #53160, .F. ) ;
#12982 = EDGE_CURVE ( 'NONE', #19489, #51203, #66025, .T. ) ;
#12983 = DIRECTION ( 'NONE',  ( -1.836970198721029934E-16, 1.836970198721036344E-16, -1.000000000000000000 ) ) ;
#12984 = VECTOR ( 'NONE', #52184, 1000.000000000000000 ) ;
#12985 = VECTOR ( 'NONE', #61061, 1000.000000000000000 ) ;
#12986 = AXIS2_PLACEMENT_3D ( 'NONE', #18875, #22535, #28172 ) ;
#12987 = ORIENTED_EDGE ( 'NONE', *, *, #54420, .F. ) ;
#12988 = DIRECTION ( 'NONE',  ( 0.000000000000000000, -1.000000000000000000, 0.000000000000000000 ) ) ;
#12989 = VERTEX_POINT ( 'NONE', #2033 ) ;
#12990 = EDGE_CURVE ( 'NONE', #29373, #1632, #44117, .T. ) ;
#12991 = CARTESIAN_POINT ( 'NONE',  ( 8.711985858128693749, -2.420780051175180692, 54.00000000000000711 ) ) ;
#12992 = AXIS2_PLACEMENT_3D ( 'NONE', #56173, #3130, #50847 ) ;
#12993 = CIRCLE ( 'NONE', #27713, 0.5999999999999998668 ) ;
#12994 = EDGE_CURVE ( 'NONE', #57047, #22012, #22901, .T. ) ;
#12995 = CARTESIAN_POINT ( 'NONE',  ( -1.991476262117235274, 8.598420958951582094, 54.00000000000000711 ) ) ;
#12996 = VECTOR ( 'NONE', #27656, 1000.000000000000000 ) ;
#12997 = CARTESIAN_POINT ( 'NONE',  ( 9.841277389592722358, -2.290483450353490547, 455.0000000000000568 ) ) ;
#12998 = EDGE_LOOP ( 'NONE', ( #48214, #10590, #2660, #35621 ) ) ;
#12999 = EDGE_CURVE ( 'NONE', #46962, #15894, #14028, .T. ) ;
#13000 = ORIENTED_EDGE ( 'NONE', *, *, #43928, .T. ) ;
#13001 = EDGE_CURVE ( 'NONE', #11369, #19166, #23199, .T. ) ;
#13002 = CARTESIAN_POINT ( 'NONE',  ( -4.393516549646835578, -11.78648345035344214, 455.0000000000000568 ) ) ;
#13003 = ORIENTED_EDGE ( 'NONE', *, *, #38830, .F. ) ;
#13004 = ORIENTED_EDGE ( 'NONE', *, *, #21036, .T. ) ;
#13005 = DIRECTION ( 'NONE',  ( 0.000000000000000000, 0.000000000000000000, 1.000000000000000000 ) ) ;
#13006 = CARTESIAN_POINT ( 'NONE',  ( 10.20488345035340494, 9.791916549646614953, 195.0000000000000284 ) ) ;
#13007 = DIRECTION ( 'NONE',  ( -0.000000000000000000, -0.000000000000000000, -1.000000000000000000 ) ) ;
#13008 = ORIENTED_EDGE ( 'NONE', *, *, #16738, .T. ) ;
#13009 = VECTOR ( 'NONE', #8101, 1000.000000000000000 ) ;
#13010 = PLANE ( 'NONE',  #66218 ) ;
#13012 = LINE ( 'NONE', #14070, #7344 ) ;
#13011 = FACE_OUTER_BOUND ( 'NONE', #26816, .T. ) ;
#13013 = EDGE_LOOP ( 'NONE', ( #41662, #36388, #16133, #31133 ) ) ;
#13015 = VERTEX_POINT ( 'NONE', #46202 ) ;
#13014 = CARTESIAN_POINT ( 'NONE',  ( 7.428221114745000797, 3.593516549646565750, 455.0000000000000568 ) ) ;
#13016 = EDGE_LOOP ( 'NONE', ( #25897, #45377, #18902, #60180 ) ) ;
#13017 = DIRECTION ( 'NONE',  ( 1.000000000000000000, 0.000000000000000000, 0.000000000000000000 ) ) ;
#13018 = DIRECTION ( 'NONE',  ( 1.000000000000000000, -5.981805089575196197E-17, 0.000000000000000000 ) ) ;
#13019 = ORIENTED_EDGE ( 'NONE', *, *, #50896, .T. ) ;
#13020 = DIRECTION ( 'NONE',  ( 1.836970198721029934E-16, 1.836970198721010706E-16, -1.000000000000000000 ) ) ;
#13021 = DIRECTION ( 'NONE',  ( 1.088659024508174257E-14, 1.000000000000000000, 1.836970198721030674E-16 ) ) ;
#13022 = ORIENTED_EDGE ( 'NONE', *, *, #24978, .F. ) ;
#13023 = AXIS2_PLACEMENT_3D ( 'NONE', #2359, #18612, #62090 ) ;
#13024 = ORIENTED_EDGE ( 'NONE', *, *, #22491, .T. ) ;
#13025 = CARTESIAN_POINT ( 'NONE',  ( -11.99351654964671354, 4.173516549646604901, 455.0000000000000568 ) ) ;
#13026 = CARTESIAN_POINT ( 'NONE',  ( 23.75054448485400016, -15.50000000000000000, -25.53140320652400064 ) ) ;
#13027 = AXIS2_PLACEMENT_3D ( 'NONE', #38833, #60393, #32515 ) ;
#13028 = ORIENTED_EDGE ( 'NONE', *, *, #38959, .F. ) ;
#13029 = CARTESIAN_POINT ( 'NONE',  ( -7.250000000000001776, -7.249999999999998224, -7.000000000000000000 ) ) ;
#13030 = PLANE ( 'NONE',  #13163 ) ;
#13031 = CIRCLE ( 'NONE', #5198, 24.99999999998794920 ) ;
#13032 = DIRECTION ( 'NONE',  ( 1.000000000000000000, -0.000000000000000000, 0.000000000000000000 ) ) ;
#13033 = EDGE_CURVE ( 'NONE', #37116, #55879, #57069, .T. ) ;
#13034 = EDGE_LOOP ( 'NONE', ( #2352, #31351, #15126, #13603 ) ) ;
#13035 = EDGE_CURVE ( 'NONE', #40232, #42575, #35586, .T. ) ;
#13036 = VECTOR ( 'NONE', #18882, 1000.000000000000000 ) ;
#13037 = AXIS2_PLACEMENT_3D ( 'NONE', #7671, #50807, #2719 ) ;
#13038 = AXIS2_PLACEMENT_3D ( 'NONE', #2173, #18783, #23739 ) ;
#13039 = DIRECTION ( 'NONE',  ( -1.000000000000000000, 8.728482790395504563E-15, 0.000000000000000000 ) ) ;
#13040 = DIRECTION ( 'NONE',  ( -1.000000000000000000, 1.185108578570163402E-14, 1.836970198721051628E-16 ) ) ;
#13043 = ORIENTED_EDGE ( 'NONE', *, *, #68569, .F. ) ;
#13042 = EDGE_CURVE ( 'NONE', #46007, #7648, #45498, .T. ) ;
#13041 = DIRECTION ( 'NONE',  ( -1.836970198721029934E-16, 1.836970198721036590E-16, -1.000000000000000000 ) ) ;
#13045 = VERTEX_POINT ( 'NONE', #61404 ) ;
#13044 = CARTESIAN_POINT ( 'NONE',  ( 9.900000000000000355, -14.48845687959340012, -21.00000000000000000 ) ) ;
#13046 = DIRECTION ( 'NONE',  ( 0.000000000000000000, -0.7096009616570518874, -0.7046037717862339012 ) ) ;
#13047 = AXIS2_PLACEMENT_3D ( 'NONE', #48636, #54296, #65923 ) ;
#13048 = AXIS2_PLACEMENT_3D ( 'NONE', #13709, #29972, #56836 ) ;
#13049 = VECTOR ( 'NONE', #65815, 1000.000000000000000 ) ;
#13050 = FACE_OUTER_BOUND ( 'NONE', #19450, .T. ) ;
#13051 = CARTESIAN_POINT ( 'NONE',  ( -2.530476262117327568, -9.737023737882829266, 54.00000000000000711 ) ) ;
#13052 = DIRECTION ( 'NONE',  ( 1.000000000000000000, -0.000000000000000000, -0.000000000000000000 ) ) ;
#13053 = CIRCLE ( 'NONE', #35615, 2.204799999999997873 ) ;
#13054 = DIRECTION ( 'NONE',  ( 1.000000000000000000, 0.000000000000000000, 0.000000000000000000 ) ) ;
#13055 = VERTEX_POINT ( 'NONE', #8014 ) ;
#13056 = CYLINDRICAL_SURFACE ( 'NONE', #21083, 0.1999999999999996503 ) ;
#13057 = PLANE ( 'NONE',  #59806 ) ;
#13058 = FACE_OUTER_BOUND ( 'NONE', #11220, .T. ) ;
#13060 = VERTEX_POINT ( 'NONE', #29588 ) ;
#13059 = DIRECTION ( 'NONE',  ( -0.7671651518153006499, -0.6414496315691565753, -2.356647714346250026E-16 ) ) ;
#13061 = VECTOR ( 'NONE', #6985, 1000.000000000000000 ) ;
#13062 = DIRECTION ( 'NONE',  ( 1.000000000000000000, 0.000000000000000000, 0.000000000000000000 ) ) ;
#13063 = EDGE_CURVE ( 'NONE', #14787, #55576, #18989, .T. ) ;
#13064 = CIRCLE ( 'NONE', #57144, 0.1749999999999998224 ) ;
#13065 = CARTESIAN_POINT ( 'NONE',  ( -11.07551654964667520, 9.791916549646639822, 455.0000000000000568 ) ) ;
#13066 = ORIENTED_EDGE ( 'NONE', *, *, #60434, .T. ) ;
#13067 = DIRECTION ( 'NONE',  ( 0.000000000000000000, 0.000000000000000000, -1.000000000000000000 ) ) ;
#13068 = LINE ( 'NONE', #44548, #21546 ) ;
#13069 = ORIENTED_EDGE ( 'NONE', *, *, #10226, .F. ) ;
#13070 = DIRECTION ( 'NONE',  ( -1.000000000000000000, 0.000000000000000000, 0.000000000000000000 ) ) ;
#13071 = CARTESIAN_POINT ( 'NONE',  ( 8.093267424590454340, 8.697938382363069820, 26.00000000000000711 ) ) ;
#13072 = CARTESIAN_POINT ( 'NONE',  ( 11.50000000000000000, -15.46862696659690073, 14.50000000000000000 ) ) ;
#13073 = DIRECTION ( 'NONE',  ( 1.000000000000000000, 0.000000000000000000, 0.000000000000000000 ) ) ;
#13074 = EDGE_CURVE ( 'NONE', #65968, #1391, #51519, .T. ) ;
#13075 = DIRECTION ( 'NONE',  ( -1.000000000000000000, 0.000000000000000000, 0.000000000000000000 ) ) ;
#13076 = EDGE_LOOP ( 'NONE', ( #45935, #20950, #28467, #42499 ) ) ;
#13077 = DIRECTION ( 'NONE',  ( 0.000000000000000000, 0.000000000000000000, 1.000000000000000000 ) ) ;
#13078 = ORIENTED_EDGE ( 'NONE', *, *, #10666, .F. ) ;
#13079 = AXIS2_PLACEMENT_3D ( 'NONE', #32392, #1250, #44021 ) ;
#13080 = ORIENTED_EDGE ( 'NONE', *, *, #56051, .T. ) ;
#13081 = CARTESIAN_POINT ( 'NONE',  ( 14.99999999999999822, -42.00000000000000000, 26.50000000000000000 ) ) ;
#13082 = EDGE_CURVE ( 'NONE', #2465, #54584, #61591, .T. ) ;
#13083 = CIRCLE ( 'NONE', #58288, 0.5249999999999990230 ) ;
#13084 = ADVANCED_FACE ( 'NONE', ( #13682 ), #51158, .F. ) ;
#13085 = EDGE_CURVE ( 'NONE', #40022, #43129, #29942, .T. ) ;
#13086 = CARTESIAN_POINT ( 'NONE',  ( -7.250000000000000888, 8.250000000000001776, -9.500000000000001776 ) ) ;
#13088 = CARTESIAN_POINT ( 'NONE',  ( 9.562023737882812569, -2.369523737882825998, 54.00000000000000711 ) ) ;
#13087 = CARTESIAN_POINT ( 'NONE',  ( 176.0064834503533575, 2.160375375128253950, 0.000000000000000000 ) ) ;
#13089 = VERTEX_POINT ( 'NONE', #25350 ) ;
#13090 = ADVANCED_FACE ( 'NONE', ( #62110 ), #30305, .F. ) ;
#13091 = EDGE_LOOP ( 'NONE', ( #13149, #60862, #50717, #60950 ) ) ;
#13092 = ADVANCED_FACE ( 'NONE', ( #24651 ), #2377, .F. ) ;
#13093 = DIRECTION ( 'NONE',  ( 0.000000000000000000, 0.000000000000000000, 1.000000000000000000 ) ) ;
#13094 = EDGE_LOOP ( 'NONE', ( #32447, #27475, #54753, #7575 ) ) ;
#13095 = AXIS2_PLACEMENT_3D ( 'NONE', #63073, #42200, #63783 ) ;
#13096 = VECTOR ( 'NONE', #16678, 1000.000000000000000 ) ;
#13097 = VECTOR ( 'NONE', #65417, 1000.000000000000000 ) ;
#13098 = DIRECTION ( 'NONE',  ( -1.000000000000000000, 0.000000000000000000, 0.000000000000000000 ) ) ;
#13099 = CARTESIAN_POINT ( 'NONE',  ( 15.89999999999999680, -21.00000000000000000, 13.86939075806900057 ) ) ;
#13100 = EDGE_CURVE ( 'NONE', #69664, #60907, #34884, .T. ) ;
#13101 = DIRECTION ( 'NONE',  ( 1.000000000000000000, -1.047444401652940007E-14, 1.836970198721010706E-16 ) ) ;
#13102 = VERTEX_POINT ( 'NONE', #40899 ) ;
#13103 = CARTESIAN_POINT ( 'NONE',  ( -8.452095193409485674, -7.757955312929543545, 455.0000000000000568 ) ) ;
#13104 = AXIS2_PLACEMENT_3D ( 'NONE', #14637, #57768, #58494 ) ;
#13105 = VECTOR ( 'NONE', #53842, 1000.000000000000000 ) ;
#13106 = VECTOR ( 'NONE', #702, 1000.000000000000000 ) ;
#13108 = DIRECTION ( 'NONE',  ( 1.836970198721029934E-16, -1.836970198721036344E-16, 1.000000000000000000 ) ) ;
#13107 = CARTESIAN_POINT ( 'NONE',  ( 7.250000000000005329, 7.250000000000000888, -24.50000000000000000 ) ) ;
#13109 = VERTEX_POINT ( 'NONE', #68127 ) ;
#13111 = ORIENTED_EDGE ( 'NONE', *, *, #9785, .T. ) ;
#13110 = CARTESIAN_POINT ( 'NONE',  ( -5.242976262117280406, -5.257023737882805747, 54.00000000000000711 ) ) ;
#13112 = EDGE_LOOP ( 'NONE', ( #8683, #46906, #59138, #41464 ) ) ;
#13113 = VERTEX_POINT ( 'NONE', #61775 ) ;
#13114 = AXIS2_PLACEMENT_3D ( 'NONE', #7569, #56358, #29135 ) ;
#13115 = CARTESIAN_POINT ( 'NONE',  ( 30.00000000000000000, -16.28999999999999915, 14.50000000000000000 ) ) ;
#13116 = AXIS2_PLACEMENT_3D ( 'NONE', #29952, #30314, #57876 ) ;
#13117 = DIRECTION ( 'NONE',  ( 0.000000000000000000, 0.000000000000000000, 1.000000000000000000 ) ) ;
#13118 = VERTEX_POINT ( 'NONE', #3431 ) ;
#13119 = ORIENTED_EDGE ( 'NONE', *, *, #69564, .T. ) ;
#13120 = DIRECTION ( 'NONE',  ( 0.000000000000000000, 0.000000000000000000, 1.000000000000000000 ) ) ;
#13121 = DIRECTION ( 'NONE',  ( -1.000000000000000000, 0.000000000000000000, 0.000000000000000000 ) ) ;
#13122 = ORIENTED_EDGE ( 'NONE', *, *, #62887, .F. ) ;
#13123 = ORIENTED_EDGE ( 'NONE', *, *, #50782, .T. ) ;
#13124 = DIRECTION ( 'NONE',  ( 0.000000000000000000, 0.000000000000000000, 1.000000000000000000 ) ) ;
#13125 = DIRECTION ( 'NONE',  ( 1.000000000000000000, 0.000000000000000000, 0.000000000000000000 ) ) ;
#13126 = ORIENTED_EDGE ( 'NONE', *, *, #68120, .F. ) ;
#13127 = CARTESIAN_POINT ( 'NONE',  ( 4.186483450353337687, -11.78648345035347589, 455.0000000000000568 ) ) ;
#13128 = FACE_OUTER_BOUND ( 'NONE', #53755, .T. ) ;
#13129 = AXIS2_PLACEMENT_3D ( 'NONE', #60890, #24478, #12443 ) ;
#13132 = EDGE_LOOP ( 'NONE', ( #54151, #29116, #69210, #55000 ) ) ;
#13131 = ADVANCED_FACE ( 'NONE', ( #62452, #13331 ), #19673, .T. ) ;
#13130 = LINE ( 'NONE', #17756, #22741 ) ;
#13133 = EDGE_LOOP ( 'NONE', ( #62699, #4352, #26310, #24239 ) ) ;
#13134 = ADVANCED_FACE ( 'NONE', ( #35954 ), #57516, .F. ) ;
#13135 = CARTESIAN_POINT ( 'NONE',  ( 9.899999999999998579, -21.00000000000000355, 14.57806571531352269 ) ) ;
#13136 = CARTESIAN_POINT ( 'NONE',  ( -11.00000000000000000, -11.70000000000000284, -12.50000000000000000 ) ) ;
#13137 = AXIS2_PLACEMENT_3D ( 'NONE', #18481, #44314, #12145 ) ;
#13138 = DIRECTION ( 'NONE',  ( -0.000000000000000000, 3.673940397442059868E-16, -1.000000000000000000 ) ) ;
#13139 = CARTESIAN_POINT ( 'NONE',  ( 11.12648345035336384, 2.893516549646526048, 455.0000000000000568 ) ) ;
#13140 = CARTESIAN_POINT ( 'NONE',  ( 17.24945551514599984, -17.50000000000000000, -25.53140320652400064 ) ) ;
#13141 = EDGE_CURVE ( 'NONE', #1276, #14260, #34491, .T. ) ;
#13142 = FACE_OUTER_BOUND ( 'NONE', #18161, .T. ) ;
#13143 = AXIS2_PLACEMENT_3D ( 'NONE', #5354, #52749, #26912 ) ;
#13144 = AXIS2_PLACEMENT_3D ( 'NONE', #33239, #22631, #44877 ) ;
#13145 = FACE_OUTER_BOUND ( 'NONE', #48087, .T. ) ;
#13146 = ORIENTED_EDGE ( 'NONE', *, *, #27199, .T. ) ;
#13147 = CARTESIAN_POINT ( 'NONE',  ( 41.09999999999999432, -14.06939075806902117, -20.80000000000000426 ) ) ;
#13149 = ORIENTED_EDGE ( 'NONE', *, *, #14654, .F. ) ;
#13148 = DIRECTION ( 'NONE',  ( 0.000000000000000000, 0.000000000000000000, 1.000000000000000000 ) ) ;
#13150 = VECTOR ( 'NONE', #36660, 1000.000000000000000 ) ;
#13151 = AXIS2_PLACEMENT_3D ( 'NONE', #43097, #15195, #68932 ) ;
#13153 = DIRECTION ( 'NONE',  ( 1.000000000000000000, 0.000000000000000000, 0.000000000000000000 ) ) ;
#13152 = VECTOR ( 'NONE', #43403, 1000.000000000000000 ) ;
#13154 = CARTESIAN_POINT ( 'NONE',  ( 69.92576880110368620, 0.000000000000000000, 281.4830310981151911 ) ) ;
#13155 = DIRECTION ( 'NONE',  ( -1.000000000000000000, 0.000000000000000000, 0.000000000000000000 ) ) ;
#13156 = DIRECTION ( 'NONE',  ( 0.000000000000000000, 1.000000000000000000, 0.000000000000000000 ) ) ;
#13157 = VECTOR ( 'NONE', #48562, 999.9999999999998863 ) ;
#13158 = VECTOR ( 'NONE', #15824, 999.9999999999998863 ) ;
#13159 = DIRECTION ( 'NONE',  ( 0.000000000000000000, 0.000000000000000000, 1.000000000000000000 ) ) ;
#13160 = VERTEX_POINT ( 'NONE', #9431 ) ;
#13161 = DIRECTION ( 'NONE',  ( 0.000000000000000000, -1.000000000000000000, 0.000000000000000000 ) ) ;
#13162 = ORIENTED_EDGE ( 'NONE', *, *, #35388, .T. ) ;
#13163 = AXIS2_PLACEMENT_3D ( 'NONE', #17998, #61122, #34251 ) ;
#13164 = DIRECTION ( 'NONE',  ( -0.000000000000000000, 3.673940397442059868E-16, -1.000000000000000000 ) ) ;
#13165 = LINE ( 'NONE', #69279, #23214 ) ;
#13166 = AXIS2_PLACEMENT_3D ( 'NONE', #62993, #14545, #36109 ) ;
#13167 = CARTESIAN_POINT ( 'NONE',  ( 8.249999999999996447, -7.848062532927998269, -1.000000000000000000 ) ) ;
#13168 = ORIENTED_EDGE ( 'NONE', *, *, #55805, .T. ) ;
#13169 = DIRECTION ( 'NONE',  ( -0.000000000000000000, -0.000000000000000000, 1.000000000000000000 ) ) ;
#13170 = ORIENTED_EDGE ( 'NONE', *, *, #29374, .T. ) ;
#13171 = EDGE_LOOP ( 'NONE', ( #47311, #56926, #2434, #11766 ) ) ;
#13172 = DIRECTION ( 'NONE',  ( 0.000000000000000000, 1.000000000000000000, 0.000000000000000000 ) ) ;
#13173 = LINE ( 'NONE', #45692, #38725 ) ;
#13174 = VERTEX_POINT ( 'NONE', #47963 ) ;
#13175 = CARTESIAN_POINT ( 'NONE',  ( 10.20488345035345645, 11.47551654964653167, 455.0000000000000568 ) ) ;
#13176 = LINE ( 'NONE', #24142, #45608 ) ;
#13177 = CARTESIAN_POINT ( 'NONE',  ( 7.969523737882818537, -8.835729544836334881, 26.00000000000000000 ) ) ;
#13178 = VERTEX_POINT ( 'NONE', #26748 ) ;
#13179 = ORIENTED_EDGE ( 'NONE', *, *, #65837, .T. ) ;
#13180 = EDGE_CURVE ( 'NONE', #2734, #30841, #15785, .T. ) ;
#13182 = EDGE_LOOP ( 'NONE', ( #30974, #56816, #26406, #62352 ) ) ;
#13181 = FACE_OUTER_BOUND ( 'NONE', #43863, .T. ) ;
#13183 = EDGE_CURVE ( 'NONE', #59074, #30760, #10822, .T. ) ;
#13184 = ORIENTED_EDGE ( 'NONE', *, *, #5549, .T. ) ;
#13185 = CARTESIAN_POINT ( 'NONE',  ( 46.39999999999999858, 21.00000000000000000, 0.7500000000000000000 ) ) ;
#13186 = DIRECTION ( 'NONE',  ( 0.000000000000000000, -0.7071067811865474617, -0.7071067811865474617 ) ) ;
#13187 = EDGE_CURVE ( 'NONE', #705, #39630, #41608, .T. ) ;
#13188 = DIRECTION ( 'NONE',  ( 1.000000000000000000, 0.000000000000000000, 0.000000000000000000 ) ) ;
#13189 = DIRECTION ( 'NONE',  ( 1.000000000000000000, 0.000000000000000000, 0.000000000000000000 ) ) ;
#13190 = EDGE_CURVE ( 'NONE', #52180, #41930, #22109, .T. ) ;
#13191 =( NAMED_UNIT ( * ) PLANE_ANGLE_UNIT ( ) SI_UNIT ( $, .RADIAN. ) );
#13192 = DIRECTION ( 'NONE',  ( 0.000000000000000000, 1.000000000000000000, 0.000000000000000000 ) ) ;
#13193 = VERTEX_POINT ( 'NONE', #59266 ) ;
#13194 = VERTEX_POINT ( 'NONE', #42998 ) ;
#13195 = VERTEX_POINT ( 'NONE', #69181 ) ;
#13196 = AXIS2_PLACEMENT_3D ( 'NONE', #42735, #49082, #27518 ) ;
#13197 = VECTOR ( 'NONE', #52287, 1000.000000000000000 ) ;
#13198 = ORIENTED_EDGE ( 'NONE', *, *, #21253, .T. ) ;
#13199 = FACE_OUTER_BOUND ( 'NONE', #45729, .T. ) ;
#13200 = EDGE_CURVE ( 'NONE', #15780, #34574, #69530, .T. ) ;
#13201 = DIRECTION ( 'NONE',  ( 1.000000000000000000, -1.678252938371784572E-14, 1.836970198720999119E-16 ) ) ;
#13202 = EDGE_CURVE ( 'NONE', #60150, #59731, #42654, .T. ) ;
#13203 = CARTESIAN_POINT ( 'NONE',  ( -10.30047626211729295, -6.657023737882751924, 54.00000000000000711 ) ) ;
#13204 = CIRCLE ( 'NONE', #32462, 0.1749999999999998224 ) ;
#13205 = CIRCLE ( 'NONE', #18861, 4.000000000000000888 ) ;
#13206 = CARTESIAN_POINT ( 'NONE',  ( 7.428221114744952835, 3.593516549646614155, 195.0000000000000284 ) ) ;
#13207 = EDGE_LOOP ( 'NONE', ( #55238, #59916, #52359, #56992, #52413, #29460, #50423 ) ) ;
#13208 = EDGE_LOOP ( 'NONE', ( #5378, #14852, #20083, #51125, #46877, #3228, #14531, #25939 ) ) ;
#13209 = ORIENTED_EDGE ( 'NONE', *, *, #63946, .T. ) ;
#13210 = DIRECTION ( 'NONE',  ( 0.000000000000000000, 0.000000000000000000, 1.000000000000000000 ) ) ;
#13211 = VECTOR ( 'NONE', #27597, 1000.000000000000000 ) ;
#13212 = VECTOR ( 'NONE', #1045, 1000.000000000000000 ) ;
#13213 = VERTEX_POINT ( 'NONE', #47612 ) ;
#13214 = ORIENTED_EDGE ( 'NONE', *, *, #53936, .F. ) ;
#13215 = VERTEX_POINT ( 'NONE', #31713 ) ;
#13216 = ORIENTED_EDGE ( 'NONE', *, *, #44313, .F. ) ;
#13217 = VECTOR ( 'NONE', #30630, 1000.000000000000000 ) ;
#13218 = CARTESIAN_POINT ( 'NONE',  ( 11.48848345035334617, -11.08848345035339733, 195.0000000000000284 ) ) ;
#13220 = ORIENTED_EDGE ( 'NONE', *, *, #63826, .F. ) ;
#13219 = FACE_OUTER_BOUND ( 'NONE', #47735, .T. ) ;
#13221 = VERTEX_POINT ( 'NONE', #21091 ) ;
#13222 = CYLINDRICAL_SURFACE ( 'NONE', #13114, 24.99999999998789946 ) ;
#13223 = VECTOR ( 'NONE', #61855, 1000.000000000000000 ) ;
#13224 = DIRECTION ( 'NONE',  ( 0.000000000000000000, 0.000000000000000000, -1.000000000000000000 ) ) ;
#13225 = DIRECTION ( 'NONE',  ( 0.000000000000000000, 1.000000000000000000, 0.000000000000000000 ) ) ;
#13227 = EDGE_LOOP ( 'NONE', ( #49246, #19097, #26472, #6127 ) ) ;
#13226 = CARTESIAN_POINT ( 'NONE',  ( 5.257023737882795977, 5.242976262117205799, 26.00000000000000711 ) ) ;
#13228 = VERTEX_POINT ( 'NONE', #69871 ) ;
#13229 = CARTESIAN_POINT ( 'NONE',  ( 8.000000000000001776, -8.000000000000000000, -1.000000000000000000 ) ) ;
#13230 = CARTESIAN_POINT ( 'NONE',  ( 9.804883450353379715, -11.08848345035349325, 455.0000000000000568 ) ) ;
#13231 = EDGE_CURVE ( 'NONE', #69664, #35311, #64239, .T. ) ;
#13232 = FACE_OUTER_BOUND ( 'NONE', #20507, .T. ) ;
#13233 = VERTEX_POINT ( 'NONE', #31375 ) ;
#13234 = DIRECTION ( 'NONE',  ( 1.000000000000000000, 0.000000000000000000, 0.000000000000000000 ) ) ;
#13235 = PLANE ( 'NONE',  #63715 ) ;
#13236 = DIRECTION ( 'NONE',  ( -0.000000000000000000, -0.000000000000000000, -1.000000000000000000 ) ) ;
#13237 = VECTOR ( 'NONE', #657, 1000.000000000000000 ) ;
#13238 = ORIENTED_EDGE ( 'NONE', *, *, #29787, .T. ) ;
#13239 = CARTESIAN_POINT ( 'NONE',  ( 7.250000000000005329, -7.249999999999998224, -16.50000000000000000 ) ) ;
#13240 = EDGE_CURVE ( 'NONE', #25255, #60406, #41317, .T. ) ;
#13241 = FACE_OUTER_BOUND ( 'NONE', #57104, .T. ) ;
#13242 = CARTESIAN_POINT ( 'NONE',  ( 12.00648345035338238, 4.173516549646515195, 455.0000000000000568 ) ) ;
#13243 = ORIENTED_EDGE ( 'NONE', *, *, #33765, .F. ) ;
#13244 = AXIS2_PLACEMENT_3D ( 'NONE', #67137, #19738, #62176 ) ;
#13245 = AXIS2_PLACEMENT_3D ( 'NONE', #59951, #564, #32402 ) ;
#13246 = AXIS2_PLACEMENT_3D ( 'NONE', #56108, #50455, #18259 ) ;
#13247 = ADVANCED_FACE ( 'NONE', ( #58221 ), #10479, .T. ) ;
#13248 = CARTESIAN_POINT ( 'NONE',  ( -8.750000000000003553, -7.348062532927999158, 5.000000000000000000 ) ) ;
#13249 = DIRECTION ( 'NONE',  ( -0.000000000000000000, -0.000000000000000000, 1.000000000000000000 ) ) ;
#13250 = AXIS2_PLACEMENT_3D ( 'NONE', #38670, #39352, #64854 ) ;
#13251 = CIRCLE ( 'NONE', #22315, 0.1999999999999987899 ) ;
#13252 = ORIENTED_EDGE ( 'NONE', *, *, #14494, .T. ) ;
#13253 = CARTESIAN_POINT ( 'NONE',  ( -7.342976262117273833, -4.961189459950004377, 54.00000000000000711 ) ) ;
#13254 = DIRECTION ( 'NONE',  ( -1.836970198721029934E-16, 1.836970198721036344E-16, -1.000000000000000000 ) ) ;
#13255 = DIRECTION ( 'NONE',  ( 1.000000000000000000, -0.000000000000000000, 0.000000000000000000 ) ) ;
#13256 = VECTOR ( 'NONE', #57504, 1000.000000000000000 ) ;
#13257 = DIRECTION ( 'NONE',  ( 0.000000000000000000, 0.000000000000000000, 1.000000000000000000 ) ) ;
#13258 = AXIS2_PLACEMENT_3D ( 'NONE', #62148, #3813, #8051 ) ;
#13259 = PLANE ( 'NONE',  #65785 ) ;
#13260 = ORIENTED_EDGE ( 'NONE', *, *, #49261, .F. ) ;
#13261 = CARTESIAN_POINT ( 'NONE',  ( -30.00000000000000000, -5.000000000000000000, 27.00000000000000000 ) ) ;
#13262 = DIRECTION ( 'NONE',  ( 0.000000000000000000, -1.000000000000000000, 0.000000000000000000 ) ) ;
#13263 = EDGE_CURVE ( 'NONE', #51293, #65543, #52940, .T. ) ;
#13264 = LINE ( 'NONE', #34821, #57161 ) ;
#13265 = DIRECTION ( 'NONE',  ( -0.5773502691896243988, 0.5773502691896263972, -0.5773502691896263972 ) ) ;
#13266 = DIRECTION ( 'NONE',  ( -0.000000000000000000, -0.000000000000000000, -1.000000000000000000 ) ) ;
#13267 = ORIENTED_EDGE ( 'NONE', *, *, #4007, .T. ) ;
#13269 = EDGE_LOOP ( 'NONE', ( #27324, #29736, #51483, #51189 ) ) ;
#13268 = CARTESIAN_POINT ( 'NONE',  ( 0.5000000000000000000, 18.00000000000000355, -21.00000000000000000 ) ) ;
#13270 = AXIS2_PLACEMENT_3D ( 'NONE', #11842, #59259, #49357 ) ;
#13271 = CARTESIAN_POINT ( 'NONE',  ( 6.657023737882821202, 10.30047626211719347, 54.00000000000000711 ) ) ;
#13272 = EDGE_CURVE ( 'NONE', #56475, #14148, #62776, .T. ) ;
#13273 = DIRECTION ( 'NONE',  ( 1.000000000000000000, -0.000000000000000000, 0.000000000000000000 ) ) ;
#13274 = ORIENTED_EDGE ( 'NONE', *, *, #43445, .T. ) ;
#13275 = EDGE_CURVE ( 'NONE', #22435, #5714, #5529, .T. ) ;
#13276 = DIRECTION ( 'NONE',  ( 1.000000000000000000, 0.000000000000000000, 0.000000000000000000 ) ) ;
#13277 = EDGE_CURVE ( 'NONE', #13881, #5466, #16504, .T. ) ;
#13278 = ORIENTED_EDGE ( 'NONE', *, *, #5140, .T. ) ;
#13279 = CARTESIAN_POINT ( 'NONE',  ( -8.693516549646711056, 11.11351654964659730, 195.0000000000000284 ) ) ;
#13280 = ORIENTED_EDGE ( 'NONE', *, *, #11983, .T. ) ;
#13281 = ORIENTED_EDGE ( 'NONE', *, *, #69088, .F. ) ;
#13283 = ADVANCED_FACE ( 'NONE', ( #63537 ), #63880, .F. ) ;
#13282 = PLANE ( 'NONE',  #27358 ) ;
#13284 = DIRECTION ( 'NONE',  ( 1.000000000000000000, -1.047444401652940007E-14, 1.836970198721010706E-16 ) ) ;
#13285 = ADVANCED_FACE ( 'NONE', ( #4834 ), #53626, .F. ) ;
#13286 = CARTESIAN_POINT ( 'NONE',  ( 7.811466277050743479, 4.727349090213326832, 455.0000000000000568 ) ) ;
#13287 = DIRECTION ( 'NONE',  ( -0.000000000000000000, -0.000000000000000000, -1.000000000000000000 ) ) ;
#13288 = COLOUR_RGB ( '', 0.66274510, 0.83137255, 0.94901961) ;
#13289 = EDGE_LOOP ( 'NONE', ( #12788, #52463, #18699, #60669 ) ) ;
#13290 = ORIENTED_EDGE ( 'NONE', *, *, #39086, .F. ) ;
#13291 = FACE_OUTER_BOUND ( 'NONE', #12932, .T. ) ;
#13292 = LINE ( 'NONE', #51830, #23719 ) ;
#13293 = ORIENTED_EDGE ( 'NONE', *, *, #59326, .T. ) ;
#13294 = EDGE_CURVE ( 'NONE', #10448, #25545, #54317, .T. ) ;
#13295 = VERTEX_POINT ( 'NONE', #65939 ) ;
#13296 = VERTEX_POINT ( 'NONE', #43338 ) ;
#13297 = LINE ( 'NONE', #44764, #7875 ) ;
#13299 = VERTEX_POINT ( 'NONE', #6218 ) ;
#13298 = CARTESIAN_POINT ( 'NONE',  ( 8.250000000000005329, 0.000000000000000000, -13.00000000000000178 ) ) ;
#13300 = VECTOR ( 'NONE', #48161, 1000.000000000000000 ) ;
#13301 = DIRECTION ( 'NONE',  ( 0.8660254037844363761, -0.5000000000000038858, 0.000000000000000000 ) ) ;
#13302 = LINE ( 'NONE', #3402, #20462 ) ;
#13303 = EDGE_CURVE ( 'NONE', #43882, #30792, #38065, .T. ) ;
#13304 = AXIS2_PLACEMENT_3D ( 'NONE', #23326, #65765, #44887 ) ;
#13305 = ORIENTED_EDGE ( 'NONE', *, *, #7728, .T. ) ;
#13306 = EDGE_LOOP ( 'NONE', ( #6850, #28491, #11973, #66869 ) ) ;
#13307 = AXIS2_PLACEMENT_3D ( 'NONE', #14646, #37275, #47867 ) ;
#13308 = CIRCLE ( 'NONE', #12037, 2.204799999999998761 ) ;
#13309 = ADVANCED_FACE ( 'NONE', ( #44718 ), #55691, .T. ) ;
#13310 = DIRECTION ( 'NONE',  ( -1.047444401652940007E-14, -1.000000000000000000, -1.836970198721029934E-16 ) ) ;
#13311 = PLANE ( 'NONE',  #31326 ) ;
#13312 = FACE_OUTER_BOUND ( 'NONE', #2827, .T. ) ;
#13313 = EDGE_CURVE ( 'NONE', #67681, #56335, #66306, .T. ) ;
#13314 = VECTOR ( 'NONE', #68044, 1000.000000000000000 ) ;
#13315 = DIRECTION ( 'NONE',  ( 0.000000000000000000, -0.7071067811865454633, -0.7071067811865496822 ) ) ;
#13316 = DIRECTION ( 'NONE',  ( 1.000000000000000000, -0.000000000000000000, -0.000000000000000000 ) ) ;
#13318 = ORIENTED_EDGE ( 'NONE', *, *, #54806, .F. ) ;
#13317 = FACE_OUTER_BOUND ( 'NONE', #16548, .T. ) ;
#13319 = VERTEX_POINT ( 'NONE', #64927 ) ;
#13320 = ADVANCED_FACE ( 'NONE', ( #60292 ), #27087, .F. ) ;
#13321 = FACE_OUTER_BOUND ( 'NONE', #46303, .T. ) ;
#13322 = CARTESIAN_POINT ( 'NONE',  ( 0.000000000000000000, -8.249999999999998224, -12.50000000000000000 ) ) ;
#13323 = DIRECTION ( 'NONE',  ( 1.000000000000000000, -0.000000000000000000, 0.000000000000000000 ) ) ;
#13324 = PLANE ( 'NONE',  #21228 ) ;
#13325 = ADVANCED_FACE ( 'NONE', ( #11848 ), #223, .F. ) ;
#13326 = LINE ( 'NONE', #39162, #19529 ) ;
#13327 = VERTEX_POINT ( 'NONE', #49010 ) ;
#13328 = DIRECTION ( 'NONE',  ( -1.000000000000000000, 3.491481338843133355E-15, 1.836970198721036590E-16 ) ) ;
#13329 = CARTESIAN_POINT ( 'NONE',  ( 7.000000000000000000, -42.50000000000000000, -15.10000000000000142 ) ) ;
#13330 = DIRECTION ( 'NONE',  ( -0.000000000000000000, -0.000000000000000000, -1.000000000000000000 ) ) ;
#13331 = FACE_BOUND ( 'NONE', #42166, .T. ) ;
#13332 = VECTOR ( 'NONE', #5721, 1000.000000000000000 ) ;
#13333 = FACE_OUTER_BOUND ( 'NONE', #47793, .T. ) ;
#13334 = ADVANCED_FACE ( 'NONE', ( #39080 ), #59621, .F. ) ;
#13335 = DIRECTION ( 'NONE',  ( -1.000000000000000000, 0.000000000000000000, 0.000000000000000000 ) ) ;
#13336 = EDGE_CURVE ( 'NONE', #31143, #69756, #32737, .T. ) ;
#13337 = CYLINDRICAL_SURFACE ( 'NONE', #42168, 24.99999999998784972 ) ;
#13338 = ORIENTED_EDGE ( 'NONE', *, *, #38391, .T. ) ;
#13339 = CARTESIAN_POINT ( 'NONE',  ( 7.250000000000005329, -7.449999999999998401, -22.50000000000000000 ) ) ;
#13340 = LINE ( 'NONE', #67081, #57725 ) ;
#13341 = EDGE_CURVE ( 'NONE', #47150, #12339, #936, .T. ) ;
#13342 = ORIENTED_EDGE ( 'NONE', *, *, #43236, .T. ) ;
#13343 = CARTESIAN_POINT ( 'NONE',  ( -7.793516549646783531, -11.32648345035335780, 195.0000000000000284 ) ) ;
#13344 = ADVANCED_FACE ( 'NONE', ( #33087 ), #567, .T. ) ;
#13345 = ADVANCED_FACE ( 'NONE', ( #23159 ), #33773, .F. ) ;
#13346 = LINE ( 'NONE', #51534, #30008 ) ;
#13347 = PLANE ( 'NONE',  #43434 ) ;
#13348 = CARTESIAN_POINT ( 'NONE',  ( 2.005523737882793256, -8.612468434717222010, 54.00000000000000711 ) ) ;
#13349 = CARTESIAN_POINT ( 'NONE',  ( 283.0000000000000568, -32.95000000000000284, 14.50000000000000000 ) ) ;
#13350 = ORIENTED_EDGE ( 'NONE', *, *, #55499, .T. ) ;
#13351 = EDGE_CURVE ( 'NONE', #37678, #50851, #38731, .T. ) ;
#13352 = VECTOR ( 'NONE', #42419, 1000.000000000000114 ) ;
#13353 = DIRECTION ( 'NONE',  ( 1.000000000000000000, 0.000000000000000000, 0.000000000000000000 ) ) ;
#13354 = ORIENTED_EDGE ( 'NONE', *, *, #59914, .F. ) ;
#13355 = ADVANCED_FACE ( 'NONE', ( #6898 ), #60652, .T. ) ;
#13356 = LINE ( 'NONE', #29252, #43538 ) ;
#13357 = ORIENTED_EDGE ( 'NONE', *, *, #61910, .T. ) ;
#13358 = PLANE ( 'NONE',  #63081 ) ;
#13359 = EDGE_CURVE ( 'NONE', #48929, #65032, #50033, .T. ) ;
#13360 = AXIS2_PLACEMENT_3D ( 'NONE', #51209, #3491, #2773 ) ;
#13361 = ORIENTED_EDGE ( 'NONE', *, *, #12445, .F. ) ;
#13362 = CARTESIAN_POINT ( 'NONE',  ( 8.250000000000005329, 0.000000000000000000, -18.50000000000000000 ) ) ;
#13363 = EDGE_LOOP ( 'NONE', ( #41323, #19399, #13385, #2818 ) ) ;
#13364 = EDGE_LOOP ( 'NONE', ( #68735, #34228, #67473, #5585 ) ) ;
#13366 = EDGE_CURVE ( 'NONE', #26371, #36344, #18549, .T. ) ;
#13365 = DIRECTION ( 'NONE',  ( -1.836970198721029934E-16, 1.836970198721036344E-16, -1.000000000000000000 ) ) ;
#13367 = ORIENTED_EDGE ( 'NONE', *, *, #30540, .F. ) ;
#13368 = EDGE_LOOP ( 'NONE', ( #7158, #58684, #20527, #19337, #50812, #59875, #3648, #40452 ) ) ;
#13369 = EDGE_CURVE ( 'NONE', #61801, #63673, #36483, .T. ) ;
#13370 = VECTOR ( 'NONE', #69271, 999.9999999999998863 ) ;
#13371 = CARTESIAN_POINT ( 'NONE',  ( 6.344579767990853547, 8.393516549646580671, 455.0000000000000568 ) ) ;
#13372 = PLANE ( 'NONE',  #18871 ) ;
#13373 = LINE ( 'NONE', #44843, #53576 ) ;
#13374 = VERTEX_POINT ( 'NONE', #7235 ) ;
#13375 = CYLINDRICAL_SURFACE ( 'NONE', #14294, 0.8100000000000017186 ) ;
#13377 = CARTESIAN_POINT ( 'NONE',  ( 10.50702373788281996, -3.664523737882816157, 26.00000000000000711 ) ) ;
#13376 = PLANE ( 'NONE',  #30446 ) ;
#13378 = ORIENTED_EDGE ( 'NONE', *, *, #23166, .F. ) ;
#13380 = ORIENTED_EDGE ( 'NONE', *, *, #36241, .F. ) ;
#13379 = LINE ( 'NONE', #17637, #53454 ) ;
#13381 = EDGE_CURVE ( 'NONE', #7564, #13118, #61683, .T. ) ;
#13382 = ORIENTED_EDGE ( 'NONE', *, *, #49864, .T. ) ;
#13383 = DIRECTION ( 'NONE',  ( 0.000000000000000000, 0.000000000000000000, 1.000000000000000000 ) ) ;
#13384 = CARTESIAN_POINT ( 'NONE',  ( -5.242976262117259978, 5.242976262117182706, 54.00000000000000711 ) ) ;
#13385 = ORIENTED_EDGE ( 'NONE', *, *, #22597, .T. ) ;
#13386 = DIRECTION ( 'NONE',  ( 0.000000000000000000, 0.000000000000000000, 1.000000000000000000 ) ) ;
#13387 = CARTESIAN_POINT ( 'NONE',  ( 5.257023737882801306, 5.242976262117200470, 54.00000000000000711 ) ) ;
#13388 = EDGE_LOOP ( 'NONE', ( #67804, #3963, #63810, #23555 ) ) ;
#13389 = ORIENTED_EDGE ( 'NONE', *, *, #102, .F. ) ;
#13390 = FACE_OUTER_BOUND ( 'NONE', #13486, .T. ) ;
#13391 = DIRECTION ( 'NONE',  ( -1.000000000000000000, 0.000000000000000000, 0.000000000000000000 ) ) ;
#13392 = ORIENTED_EDGE ( 'NONE', *, *, #29316, .T. ) ;
#13393 = VECTOR ( 'NONE', #47227, 1000.000000000000000 ) ;
#13394 = CARTESIAN_POINT ( 'NONE',  ( -13.00000000000000178, -16.28999999999999915, 14.50000000000000000 ) ) ;
#13395 = LINE ( 'NONE', #3152, #48166 ) ;
#13396 = FACE_OUTER_BOUND ( 'NONE', #49950, .T. ) ;
#13397 = VERTEX_POINT ( 'NONE', #29514 ) ;
#13398 = VECTOR ( 'NONE', #45356, 1000.000000000000000 ) ;
#13399 = EDGE_CURVE ( 'NONE', #63180, #26023, #51471, .T. ) ;
#13400 = CARTESIAN_POINT ( 'NONE',  ( 8.250000000000005329, -8.249999999999998224, -26.00000000000001066 ) ) ;
#13401 = CARTESIAN_POINT ( 'NONE',  ( 282.7711612342632179, -20.61060115624107425, 17.11060115624107425 ) ) ;
#13403 = ORIENTED_EDGE ( 'NONE', *, *, #50396, .T. ) ;
#13402 = DIRECTION ( 'NONE',  ( 1.836970198721029934E-16, 1.836970198721010706E-16, -1.000000000000000000 ) ) ;
#13405 = VERTEX_POINT ( 'NONE', #56041 ) ;
#13404 = PLANE ( 'NONE',  #35415 ) ;
#13406 = ADVANCED_FACE ( 'NONE', ( #14566 ), #34806, .F. ) ;
#13407 = CARTESIAN_POINT ( 'NONE',  ( -24.00000000000000000, -16.64230188589299786, -14.64519951917100116 ) ) ;
#13408 = CIRCLE ( 'NONE', #42747, 0.1749999999999989342 ) ;
#13409 = FACE_OUTER_BOUND ( 'NONE', #10442, .T. ) ;
#13410 = EDGE_CURVE ( 'NONE', #8213, #16525, #26655, .T. ) ;
#13411 = DIRECTION ( 'NONE',  ( -1.836970198721029934E-16, 1.836970198721036344E-16, -1.000000000000000000 ) ) ;
#13412 = DIRECTION ( 'NONE',  ( 0.000000000000000000, 1.000000000000000000, 0.000000000000000000 ) ) ;
#13413 = VECTOR ( 'NONE', #68596, 1000.000000000000114 ) ;
#13414 = EDGE_CURVE ( 'NONE', #51859, #11281, #23860, .T. ) ;
#13415 = CARTESIAN_POINT ( 'NONE',  ( 41.09999999999999432, 20.60000000000000142, 13.86939075806900057 ) ) ;
#13416 = ORIENTED_EDGE ( 'NONE', *, *, #17185, .T. ) ;
#13417 = CARTESIAN_POINT ( 'NONE',  ( 283.0000000000000568, -25.60000000000000142, 17.60000000000000142 ) ) ;
#13418 = CARTESIAN_POINT ( 'NONE',  ( -11.77351654964670935, 7.593516549646604830, 455.0000000000000568 ) ) ;
#13419 = CARTESIAN_POINT ( 'NONE',  ( 3.677663764522614454, -6.364920264886879231, 54.00000000000000711 ) ) ;
#13421 = VECTOR ( 'NONE', #43592, 1000.000000000000000 ) ;
#13420 = CIRCLE ( 'NONE', #33754, 0.3999999999999993006 ) ;
#13423 = ORIENTED_EDGE ( 'NONE', *, *, #49985, .T. ) ;
#13422 = DIRECTION ( 'NONE',  ( -0.6414496315691494699, 0.7671651518153064231, 2.818519042764025305E-16 ) ) ;
#13424 = CARTESIAN_POINT ( 'NONE',  ( 31.89999999999999858, 3.010794155703768650E-16, -2.458500000000000796 ) ) ;
#13425 = FACE_OUTER_BOUND ( 'NONE', #22349, .T. ) ;
#13426 = AXIS2_PLACEMENT_3D ( 'NONE', #52390, #42117, #3953 ) ;
#13427 = EDGE_LOOP ( 'NONE', ( #6112, #7768 ) ) ;
#13428 = ORIENTED_EDGE ( 'NONE', *, *, #33567, .F. ) ;
#13429 = DIRECTION ( 'NONE',  ( -1.000000000000000000, 0.000000000000000000, 0.000000000000000000 ) ) ;
#13430 = DIRECTION ( 'NONE',  ( -1.000000000000000000, 0.000000000000000000, 0.000000000000000000 ) ) ;
#13431 = VERTEX_POINT ( 'NONE', #63720 ) ;
#13432 = EDGE_CURVE ( 'NONE', #10776, #21056, #45420, .T. ) ;
#13433 = LINE ( 'NONE', #31113, #2968 ) ;
#13434 = FILL_AREA_STYLE_COLOUR ( '', #25323 ) ;
#13435 = LINE ( 'NONE', #67174, #63186 ) ;
#13436 = CARTESIAN_POINT ( 'NONE',  ( 21.90000000000000213, -0.2000000000089119934, 8.909539772616881237E-12 ) ) ;
#13437 = ORIENTED_EDGE ( 'NONE', *, *, #64224, .F. ) ;
#13438 = PLANE ( 'NONE',  #27011 ) ;
#13439 = ORIENTED_EDGE ( 'NONE', *, *, #65268, .F. ) ;
#13440 = ORIENTED_EDGE ( 'NONE', *, *, #4855, .T. ) ;
#13441 = CARTESIAN_POINT ( 'NONE',  ( -30.00000000000000000, -5.599999999999999645, 9.400000000000000355 ) ) ;
#13442 = VECTOR ( 'NONE', #18246, 1000.000000000000000 ) ;
#13443 = CARTESIAN_POINT ( 'NONE',  ( 30.00000000000000000, -14.04000000000000092, -14.80000000000000071 ) ) ;
#13444 = DIRECTION ( 'NONE',  ( -0.000000000000000000, 3.673940397442059868E-16, -1.000000000000000000 ) ) ;
#13445 = ORIENTED_EDGE ( 'NONE', *, *, #17855, .F. ) ;
#13446 = ORIENTED_EDGE ( 'NONE', *, *, #61233, .T. ) ;
#13448 = EDGE_CURVE ( 'NONE', #32678, #34396, #25182, .T. ) ;
#13447 = FACE_OUTER_BOUND ( 'NONE', #31897, .T. ) ;
#13449 = ORIENTED_EDGE ( 'NONE', *, *, #48125, .T. ) ;
#13450 = AXIS2_PLACEMENT_3D ( 'NONE', #33966, #7092, #46674 ) ;
#13451 = ADVANCED_FACE ( 'NONE', ( #56384 ), #3616, .F. ) ;
#13452 = DIRECTION ( 'NONE',  ( -1.000000000000000000, 0.000000000000000000, 0.000000000000000000 ) ) ;
#13453 = LINE ( 'NONE', #25472, #55029 ) ;
#13454 = LINE ( 'NONE', #6755, #37720 ) ;
#13455 = DIRECTION ( 'NONE',  ( 0.000000000000000000, 0.000000000000000000, -1.000000000000000000 ) ) ;
#13456 = EDGE_LOOP ( 'NONE', ( #27828, #2561, #13840, #61249 ) ) ;
#13457 = VECTOR ( 'NONE', #20206, 1000.000000000000000 ) ;
#13458 = DIRECTION ( 'NONE',  ( 0.000000000000000000, -0.1500000000000000777, 0.9886859966642594921 ) ) ;
#13460 = DIRECTION ( 'NONE',  ( -0.5000000000000004441, 0.8660254037844383745, 0.000000000000000000 ) ) ;
#13459 = DIRECTION ( 'NONE',  ( -1.794541526872559352E-16, -1.000000000000000000, 0.000000000000000000 ) ) ;
#13461 = ORIENTED_EDGE ( 'NONE', *, *, #12922, .F. ) ;
#13463 = ORIENTED_EDGE ( 'NONE', *, *, #42538, .F. ) ;
#13462 = CARTESIAN_POINT ( 'NONE',  ( 6.657023737882813208, 9.897976262117198942, 26.00000000000000711 ) ) ;
#13464 = ORIENTED_EDGE ( 'NONE', *, *, #17572, .T. ) ;
#13465 = ORIENTED_EDGE ( 'NONE', *, *, #2811, .T. ) ;
#13466 = CIRCLE ( 'NONE', #57529, 3.999999999999993339 ) ;
#13467 = CARTESIAN_POINT ( 'NONE',  ( 11.12648345035337982, -4.206483450353492692, 455.0000000000000568 ) ) ;
#13468 = VECTOR ( 'NONE', #52139, 1000.000000000000114 ) ;
#13469 = DIRECTION ( 'NONE',  ( 1.000000000000000000, 0.000000000000000000, 0.000000000000000000 ) ) ;
#13470 = EDGE_LOOP ( 'NONE', ( #11474, #36297, #8923, #36206 ) ) ;
#13471 = ORIENTED_EDGE ( 'NONE', *, *, #34055, .T. ) ;
#13472 = AXIS2_PLACEMENT_3D ( 'NONE', #68167, #52979, #4529 ) ;
#13473 = LINE ( 'NONE', #36813, #8319 ) ;
#13474 = CARTESIAN_POINT ( 'NONE',  ( 7.250000000000005329, 7.250000000000000888, -12.50000000000000000 ) ) ;
#13475 = ORIENTED_EDGE ( 'NONE', *, *, #4065, .F. ) ;
#13476 = ORIENTED_EDGE ( 'NONE', *, *, #38350, .T. ) ;
#13477 = CARTESIAN_POINT ( 'NONE',  ( 6.619341603356875936, 7.252248008019321901, 455.0000000000000568 ) ) ;
#13478 = DIRECTION ( 'NONE',  ( 0.000000000000000000, 0.000000000000000000, -1.000000000000000000 ) ) ;
#13479 = VERTEX_POINT ( 'NONE', #61327 ) ;
#13480 = EDGE_CURVE ( 'NONE', #58172, #25429, #22157, .T. ) ;
#13481 = CARTESIAN_POINT ( 'NONE',  ( 0.4999999999999920064, -7.105427357601001859E-15, 26.49999999999998579 ) ) ;
#13482 = AXIS2_PLACEMENT_3D ( 'NONE', #26895, #15234, #41740 ) ;
#13483 = LINE ( 'NONE', #3589, #18139 ) ;
#13485 = EDGE_LOOP ( 'NONE', ( #35075, #38129, #9523, #46703 ) ) ;
#13484 = CARTESIAN_POINT ( 'NONE',  ( 8.580623737882842050, 8.916576262117192897, 26.00000000000000711 ) ) ;
#13486 = EDGE_LOOP ( 'NONE', ( #20968, #47499, #60611, #67740 ) ) ;
#13487 = EDGE_CURVE ( 'NONE', #65843, #53480, #58054, .T. ) ;
#13488 = DIRECTION ( 'NONE',  ( -8.802523127157697409E-15, -1.000000000000000000, -1.836970198721026976E-16 ) ) ;
#13489 = LINE ( 'NONE', #51320, #65121 ) ;
#13490 = CARTESIAN_POINT ( 'NONE',  ( 3.677663764522614454, -4.149127210878761574, 26.00000000000000711 ) ) ;
#13491 = EDGE_CURVE ( 'NONE', #68617, #28757, #57702, .T. ) ;
#13492 = DIRECTION ( 'NONE',  ( -1.000000000000000000, 0.000000000000000000, 0.000000000000000000 ) ) ;
#13493 = ADVANCED_FACE ( 'NONE', ( #12882 ), #9270, .F. ) ;
#13494 = CYLINDRICAL_SURFACE ( 'NONE', #19937, 9.300000000000002487 ) ;
#13495 = LINE ( 'NONE', #46718, #30548 ) ;
#13496 = ADVANCED_FACE ( 'NONE', ( #29160 ), #50726, .T. ) ;
#13497 = EDGE_CURVE ( 'NONE', #47507, #36887, #9624, .T. ) ;
#13498 = DIRECTION ( 'NONE',  ( -0.000000000000000000, -0.000000000000000000, -1.000000000000000000 ) ) ;
#13499 = ORIENTED_EDGE ( 'NONE', *, *, #35834, .F. ) ;
#13500 = CARTESIAN_POINT ( 'NONE',  ( 7.250000000000005329, -7.249999999999998224, -16.00000000000000000 ) ) ;
#13501 = VECTOR ( 'NONE', #22160, 1000.000000000000000 ) ;
#13502 = AXIS2_PLACEMENT_3D ( 'NONE', #15219, #37138, #53401 ) ;
#13504 = EDGE_LOOP ( 'NONE', ( #21889, #26928, #13123, #3229 ) ) ;
#13503 = CARTESIAN_POINT ( 'NONE',  ( 6.872275254348426010, -3.003254798005762449, 54.00000000000000711 ) ) ;
#13505 = FACE_OUTER_BOUND ( 'NONE', #4394, .T. ) ;
#13506 = LINE ( 'NONE', #35062, #49310 ) ;
#13507 = EDGE_CURVE ( 'NONE', #52907, #16354, #4334, .T. ) ;
#13508 = DIRECTION ( 'NONE',  ( 0.000000000000000000, 0.000000000000000000, 1.000000000000000000 ) ) ;
#13509 = LINE ( 'NONE', #20213, #60007 ) ;
#13510 = VECTOR ( 'NONE', #68213, 1000.000000000000000 ) ;
#13511 = CARTESIAN_POINT ( 'NONE',  ( 8.930623737882818602, -10.05377373788282469, 54.00000000000000711 ) ) ;
#13512 = ORIENTED_EDGE ( 'NONE', *, *, #30285, .F. ) ;
#13513 = DIRECTION ( 'NONE',  ( 1.062171939662867618E-14, 1.000000000000000000, 0.000000000000000000 ) ) ;
#13514 = ORIENTED_EDGE ( 'NONE', *, *, #8700, .F. ) ;
#13515 = VECTOR ( 'NONE', #50577, 1000.000000000000114 ) ;
#13516 = DIRECTION ( 'NONE',  ( 0.000000000000000000, 0.000000000000000000, -1.000000000000000000 ) ) ;
#13517 = PLANE ( 'NONE',  #42460 ) ;
#13518 = VECTOR ( 'NONE', #15978, 1000.000000000000000 ) ;
#13519 = CARTESIAN_POINT ( 'NONE',  ( 275.0000000000000000, -26.42999999999999972, -9.412893218813501051 ) ) ;
#13520 = EDGE_LOOP ( 'NONE', ( #50074, #53896, #20397, #60905 ) ) ;
#13521 = DIRECTION ( 'NONE',  ( -0.000000000000000000, -0.000000000000000000, 1.000000000000000000 ) ) ;
#13522 = ORIENTED_EDGE ( 'NONE', *, *, #13294, .F. ) ;
#13523 = ORIENTED_EDGE ( 'NONE', *, *, #51413, .F. ) ;
#13524 = CARTESIAN_POINT ( 'NONE',  ( 7.250000000000005329, -7.249999999999998224, -9.500000000000001776 ) ) ;
#13525 = FACE_BOUND ( 'NONE', #38549, .T. ) ;
#13526 = EDGE_LOOP ( 'NONE', ( #64602, #24884, #69296, #38841 ) ) ;
#13527 = CARTESIAN_POINT ( 'NONE',  ( 7.250000000000005329, -7.449999999999998401, -18.50000000000000000 ) ) ;
#13528 = DIRECTION ( 'NONE',  ( 0.000000000000000000, -0.000000000000000000, 1.000000000000000000 ) ) ;
#13529 = DIRECTION ( 'NONE',  ( 1.000000000000000000, -0.000000000000000000, -0.000000000000000000 ) ) ;
#13530 = VERTEX_POINT ( 'NONE', #15633 ) ;
#13531 = ORIENTED_EDGE ( 'NONE', *, *, #37352, .F. ) ;
#13533 = VERTEX_POINT ( 'NONE', #49189 ) ;
#13532 = LINE ( 'NONE', #28397, #47555 ) ;
#13534 = ORIENTED_EDGE ( 'NONE', *, *, #12073, .T. ) ;
#13535 = ADVANCED_FACE ( 'NONE', ( #48497 ), #54504, .F. ) ;
#13536 = DIRECTION ( 'NONE',  ( -1.836970198721029934E-16, 1.836970198721036344E-16, -1.000000000000000000 ) ) ;
#13537 = FACE_OUTER_BOUND ( 'NONE', #31300, .T. ) ;
#13538 = LINE ( 'NONE', #18845, #57217 ) ;
#13539 = AXIS2_PLACEMENT_3D ( 'NONE', #30615, #67408, #41575 ) ;
#13540 = CARTESIAN_POINT ( 'NONE',  ( -25.50000000000000355, -5.578999999999999737, 22.50000000000000000 ) ) ;
#13541 = EDGE_CURVE ( 'NONE', #49662, #50027, #21630, .T. ) ;
#13542 = EDGE_CURVE ( 'NONE', #50249, #30827, #4145, .T. ) ;
#13543 = FILL_AREA_STYLE_COLOUR ( '', #69507 ) ;
#13544 = DIRECTION ( 'NONE',  ( 1.836970198721029934E-16, 1.836970198721010706E-16, -1.000000000000000000 ) ) ;
#13545 = VERTEX_POINT ( 'NONE', #27286 ) ;
#13546 = ORIENTED_EDGE ( 'NONE', *, *, #7813, .F. ) ;
#13547 = ADVANCED_FACE ( 'NONE', ( #48151 ), #16315, .T. ) ;
#13548 = ORIENTED_EDGE ( 'NONE', *, *, #18471, .F. ) ;
#13549 = ORIENTED_EDGE ( 'NONE', *, *, #32518, .T. ) ;
#13550 = AXIS2_PLACEMENT_3D ( 'NONE', #51685, #9249, #2527 ) ;
#13551 = DIRECTION ( 'NONE',  ( 0.000000000000000000, -1.901256929667050114E-12, 1.000000000000000000 ) ) ;
#13552 = DIRECTION ( 'NONE',  ( 0.000000000000000000, 1.000000000000000000, 0.000000000000000000 ) ) ;
#13553 = AXIS2_PLACEMENT_3D ( 'NONE', #18221, #2317, #67013 ) ;
#13554 = VECTOR ( 'NONE', #31405, 1000.000000000000000 ) ;
#13555 = CARTESIAN_POINT ( 'NONE',  ( -16.54686605390243059, -0.2715358723599923807, 23.33896727494797929 ) ) ;
#13556 = AXIS2_PLACEMENT_3D ( 'NONE', #32500, #37114, #21196 ) ;
#13557 = VERTEX_POINT ( 'NONE', #26582 ) ;
#13558 = ORIENTED_EDGE ( 'NONE', *, *, #66618, .F. ) ;
#13559 = ORIENTED_EDGE ( 'NONE', *, *, #20675, .T. ) ;
#13560 = AXIS2_PLACEMENT_3D ( 'NONE', #15539, #37101, #10561 ) ;
#13561 = DIRECTION ( 'NONE',  ( 0.000000000000000000, 1.000000000000000000, 0.000000000000000000 ) ) ;
#13562 = ORIENTED_EDGE ( 'NONE', *, *, #41204, .T. ) ;
#13563 = VERTEX_POINT ( 'NONE', #20919 ) ;
#13564 = LINE ( 'NONE', #35119, #34434 ) ;
#13565 = ORIENTED_EDGE ( 'NONE', *, *, #14865, .F. ) ;
#13566 = VECTOR ( 'NONE', #58239, 1000.000000000000000 ) ;
#13567 = ORIENTED_EDGE ( 'NONE', *, *, #57462, .F. ) ;
#13568 = DIRECTION ( 'NONE',  ( -1.000000000000000000, 8.359604446858499085E-15, 3.071268848394973203E-30 ) ) ;
#13569 = CIRCLE ( 'NONE', #58764, 0.1999999999999996503 ) ;
#13571 = ORIENTED_EDGE ( 'NONE', *, *, #42443, .T. ) ;
#13570 = CARTESIAN_POINT ( 'NONE',  ( 25.49999999999869971, -15.50000000000000000, 22.50000000000000000 ) ) ;
#13572 = EDGE_LOOP ( 'NONE', ( #62703, #7615, #23075, #52233 ) ) ;
#13573 = AXIS2_PLACEMENT_3D ( 'NONE', #55192, #44218, #45604 ) ;
#13574 = DIRECTION ( 'NONE',  ( 1.000000000000000000, 0.000000000000000000, 0.000000000000000000 ) ) ;
#13575 = EDGE_CURVE ( 'NONE', #40712, #47459, #43874, .T. ) ;
#13576 = LINE ( 'NONE', #2270, #49879 ) ;
#13577 = CARTESIAN_POINT ( 'NONE',  ( 7.450000000000003730, -7.249999999999997335, -23.50000000000000000 ) ) ;
#13579 = ORIENTED_EDGE ( 'NONE', *, *, #33756, .T. ) ;
#13578 = CARTESIAN_POINT ( 'NONE',  ( 7.408280051175133885, 3.710438382363056675, 26.00000000000000711 ) ) ;
#13580 = ORIENTED_EDGE ( 'NONE', *, *, #25892, .T. ) ;
#13581 = VECTOR ( 'NONE', #32302, 1000.000000000000000 ) ;
#13582 = VECTOR ( 'NONE', #21398, 1000.000000000000000 ) ;
#13583 = LINE ( 'NONE', #35136, #54349 ) ;
#13584 = CARTESIAN_POINT ( 'NONE',  ( 283.0000000000000568, -21.00000000000000000, -17.50000000000000000 ) ) ;
#13585 = CARTESIAN_POINT ( 'NONE',  ( -8.598420958951642490, -2.005523737882745738, 54.00000000000000711 ) ) ;
#13586 = EDGE_CURVE ( 'NONE', #427, #11005, #10318, .T. ) ;
#13587 = ORIENTED_EDGE ( 'NONE', *, *, #6349, .T. ) ;
#13588 = DIRECTION ( 'NONE',  ( 1.000000000000000000, -7.304098846218132892E-15, -2.683482381803073952E-30 ) ) ;
#13589 = CARTESIAN_POINT ( 'NONE',  ( 12.00000000000000178, -11.18999999999999950, -4.250000000000000000 ) ) ;
#13590 = LINE ( 'NONE', #29500, #34522 ) ;
#13591 = ADVANCED_FACE ( 'NONE', ( #58425, #17010 ), #21284, .T. ) ;
#13592 = CIRCLE ( 'NONE', #5687, 1.224999999999998757 ) ;
#13593 = EDGE_LOOP ( 'NONE', ( #69636, #49214, #48372, #29285 ) ) ;
#13594 = DIRECTION ( 'NONE',  ( -1.000000000000000000, 0.000000000000000000, 0.000000000000000000 ) ) ;
#13595 = DIRECTION ( 'NONE',  ( 0.000000000000000000, 0.000000000000000000, 1.000000000000000000 ) ) ;
#13596 = DIRECTION ( 'NONE',  ( 1.000000000000000000, 0.000000000000000000, 0.000000000000000000 ) ) ;
#13597 = ORIENTED_EDGE ( 'NONE', *, *, #33608, .T. ) ;
#13598 = FACE_OUTER_BOUND ( 'NONE', #41574, .T. ) ;
#13599 = AXIS2_PLACEMENT_3D ( 'NONE', #47756, #59421, #59762 ) ;
#13600 = DIRECTION ( 'NONE',  ( 0.000000000000000000, 0.000000000000000000, -1.000000000000000000 ) ) ;
#13601 = ADVANCED_FACE ( 'NONE', ( #37892 ), #53121, .F. ) ;
#13602 = VECTOR ( 'NONE', #56743, 1000.000000000000000 ) ;
#13603 = ORIENTED_EDGE ( 'NONE', *, *, #36265, .T. ) ;
#13604 = LINE ( 'NONE', #44720, #27062 ) ;
#13605 = CARTESIAN_POINT ( 'NONE',  ( 30.00000000000000000, -17.50000000000000000, -15.70500000000000007 ) ) ;
#13606 = CARTESIAN_POINT ( 'NONE',  ( 46.39999999999999858, 21.00000000000000000, 2.250000000000000444 ) ) ;
#13607 = VECTOR ( 'NONE', #69724, 1000.000000000000000 ) ;
#13608 = DIRECTION ( 'NONE',  ( 1.000000000000000000, -0.000000000000000000, 0.000000000000000000 ) ) ;
#13609 = DIRECTION ( 'NONE',  ( 0.000000000000000000, -1.000000000000000000, 0.000000000000000000 ) ) ;
#13610 = ORIENTED_EDGE ( 'NONE', *, *, #38044, .T. ) ;
#13611 = LINE ( 'NONE', #2307, #17445 ) ;
#13612 = DIRECTION ( 'NONE',  ( 0.000000000000000000, 1.000000000000000000, 0.000000000000000000 ) ) ;
#13613 = LINE ( 'NONE', #56052, #18697 ) ;
#13614 = AXIS2_PLACEMENT_3D ( 'NONE', #13961, #35170, #66326 ) ;
#13615 = PLANE ( 'NONE',  #63671 ) ;
#13616 = DIRECTION ( 'NONE',  ( -0.000000000000000000, -0.000000000000000000, -1.000000000000000000 ) ) ;
#13617 = EDGE_LOOP ( 'NONE', ( #56693, #20647, #12247, #40669, #56065, #42389, #62778, #47296 ) ) ;
#13619 = ORIENTED_EDGE ( 'NONE', *, *, #15687, .F. ) ;
#13618 = DIRECTION ( 'NONE',  ( -0.000000000000000000, 3.673940397442059868E-16, -1.000000000000000000 ) ) ;
#13620 = LINE ( 'NONE', #46494, #30467 ) ;
#13621 = LINE ( 'NONE', #3029, #53758 ) ;
#13622 = ORIENTED_EDGE ( 'NONE', *, *, #16510, .F. ) ;
#13623 = EDGE_CURVE ( 'NONE', #29287, #8225, #59452, .T. ) ;
#13624 = CIRCLE ( 'NONE', #54278, 24.99999999998789946 ) ;
#13625 = FACE_OUTER_BOUND ( 'NONE', #59042, .T. ) ;
#13626 = ORIENTED_EDGE ( 'NONE', *, *, #58009, .F. ) ;
#13627 = ADVANCED_FACE ( 'NONE', ( #43179 ), #59795, .F. ) ;
#13628 = CARTESIAN_POINT ( 'NONE',  ( 152.0064834503532722, -35.83962462487175316, 0.000000000000000000 ) ) ;
#13629 = ORIENTED_EDGE ( 'NONE', *, *, #25802, .T. ) ;
#13630 = ORIENTED_EDGE ( 'NONE', *, *, #58427, .F. ) ;
#13631 = PLANE ( 'NONE',  #20488 ) ;
#13632 = CARTESIAN_POINT ( 'NONE',  ( -10.30047626211725742, 6.835476262117182955, 54.00000000000000711 ) ) ;
#13633 = DIRECTION ( 'NONE',  ( -1.000000000000000000, 0.000000000000000000, 0.000000000000000000 ) ) ;
#13634 = FACE_OUTER_BOUND ( 'NONE', #9880, .T. ) ;
#13635 = AXIS2_PLACEMENT_3D ( 'NONE', #274, #31768, #63939 ) ;
#13636 = VERTEX_POINT ( 'NONE', #15972 ) ;
#13637 = ORIENTED_EDGE ( 'NONE', *, *, #62518, .F. ) ;
#13638 = FACE_BOUND ( 'NONE', #29626, .T. ) ;
#13639 = DIRECTION ( 'NONE',  ( 0.000000000000000000, 0.000000000000000000, -1.000000000000000000 ) ) ;
#13640 = ORIENTED_EDGE ( 'NONE', *, *, #51422, .F. ) ;
#13641 = ORIENTED_EDGE ( 'NONE', *, *, #42492, .F. ) ;
#13642 = ORIENTED_EDGE ( 'NONE', *, *, #17923, .T. ) ;
#13643 = EDGE_CURVE ( 'NONE', #34775, #54337, #5382, .T. ) ;
#13644 = LINE ( 'NONE', #30273, #65493 ) ;
#13645 = VECTOR ( 'NONE', #40269, 1000.000000000000000 ) ;
#13647 = ORIENTED_EDGE ( 'NONE', *, *, #39134, .F. ) ;
#13646 = DIRECTION ( 'NONE',  ( 0.000000000000000000, 0.000000000000000000, -1.000000000000000000 ) ) ;
#13648 = DIRECTION ( 'NONE',  ( 1.836970198721029934E-16, 1.836970198721010706E-16, -1.000000000000000000 ) ) ;
#13649 = PRODUCT_DEFINITION_SHAPE ( 'NONE', 'NONE',  #1166 ) ;
#13650 = VECTOR ( 'NONE', #12260, 1000.000000000000000 ) ;
#13651 = AXIS2_PLACEMENT_3D ( 'NONE', #30455, #40362, #2523 ) ;
#13652 = FACE_OUTER_BOUND ( 'NONE', #21314, .T. ) ;
#13653 = ORIENTED_EDGE ( 'NONE', *, *, #16992, .T. ) ;
#13654 = AXIS2_PLACEMENT_3D ( 'NONE', #67878, #68584, #46651 ) ;
#13655 = ORIENTED_EDGE ( 'NONE', *, *, #2247, .T. ) ;
#13656 = CIRCLE ( 'NONE', #53221, 5.000000000000000000 ) ;
#13657 = AXIS2_PLACEMENT_3D ( 'NONE', #64266, #37389, #21468 ) ;
#13658 = DIRECTION ( 'NONE',  ( 0.000000000000000000, -1.000000000000000000, -3.673940397442059868E-16 ) ) ;
#13659 = DIRECTION ( 'NONE',  ( 0.000000000000000000, -1.000000000000000000, 0.000000000000000000 ) ) ;
#13660 = DIRECTION ( 'NONE',  ( -1.000000000000000000, 0.000000000000000000, 0.000000000000000000 ) ) ;
#13661 = AXIS2_PLACEMENT_3D ( 'NONE', #33025, #21375, #16077 ) ;
#13662 = EDGE_CURVE ( 'NONE', #65035, #40390, #51521, .T. ) ;
#13663 = PLANE ( 'NONE',  #41413 ) ;
#13664 = DIRECTION ( 'NONE',  ( -1.000000000000000000, 0.000000000000000000, 0.000000000000000000 ) ) ;
#13665 = EDGE_CURVE ( 'NONE', #59933, #60538, #5719, .T. ) ;
#13666 = EDGE_CURVE ( 'NONE', #8802, #47752, #31893, .T. ) ;
#13668 = VERTEX_POINT ( 'NONE', #53462 ) ;
#13667 = DIRECTION ( 'NONE',  ( 0.000000000000000000, 0.000000000000000000, 1.000000000000000000 ) ) ;
#13669 = VERTEX_POINT ( 'NONE', #5013 ) ;
#13670 = LINE ( 'NONE', #40184, #17419 ) ;
#13671 = PLANE ( 'NONE',  #19988 ) ;
#13672 = VECTOR ( 'NONE', #64645, 1000.000000000000000 ) ;
#13673 = DIRECTION ( 'NONE',  ( -1.000000000000000000, 0.000000000000000000, 0.000000000000000000 ) ) ;
#13674 = EDGE_CURVE ( 'NONE', #54447, #12080, #64754, .T. ) ;
#13675 = DIRECTION ( 'NONE',  ( 0.000000000000000000, 0.000000000000000000, 1.000000000000000000 ) ) ;
#13676 = CARTESIAN_POINT ( 'NONE',  ( -8.130476262117259267, 9.547976262117177981, 54.00000000000000711 ) ) ;
#13677 = EDGE_CURVE ( 'NONE', #19158, #45832, #23683, .T. ) ;
#13678 = ORIENTED_EDGE ( 'NONE', *, *, #59901, .T. ) ;
#13679 = DIRECTION ( 'NONE',  ( -1.000000000000000000, 7.304098846218132892E-15, -0.000000000000000000 ) ) ;
#13680 = DIRECTION ( 'NONE',  ( -1.000000000000000000, -0.000000000000000000, -0.000000000000000000 ) ) ;
#13681 = EDGE_CURVE ( 'NONE', #51881, #48238, #28995, .T. ) ;
#13682 = FACE_OUTER_BOUND ( 'NONE', #9330, .T. ) ;
#13683 = AXIS2_PLACEMENT_3D ( 'NONE', #12940, #57489, #61742 ) ;
#13684 = DIRECTION ( 'NONE',  ( -0.000000000000000000, -0.000000000000000000, -1.000000000000000000 ) ) ;
#13685 = CARTESIAN_POINT ( 'NONE',  ( -11.75000000000000000, -5.000000000000000000, -11.75000000000000000 ) ) ;
#13686 = LINE ( 'NONE', #55778, #1386 ) ;
#13687 = EDGE_LOOP ( 'NONE', ( #49837, #36996, #37579, #22909, #38124, #23102, #42951, #46408 ) ) ;
#13688 = CARTESIAN_POINT ( 'NONE',  ( 10.50702373788280752, 6.835476262117182067, 54.00000000000000711 ) ) ;
#13689 = CARTESIAN_POINT ( 'NONE',  ( -30.00000000000000000, -8.959999999999999076, 17.04524521594300523 ) ) ;
#13690 = VERTEX_POINT ( 'NONE', #12714 ) ;
#13691 = LINE ( 'NONE', #19341, #32322 ) ;
#13692 = CARTESIAN_POINT ( 'NONE',  ( 0.2499999999999982236, -42.25000000000000000, 26.75000000000000000 ) ) ;
#13693 = CARTESIAN_POINT ( 'NONE',  ( 7.250000000000005329, 7.250000000000000888, -11.50000000000000000 ) ) ;
#13694 = CARTESIAN_POINT ( 'NONE',  ( -7.250000000000000888, -8.249999999999998224, -25.50000000000000355 ) ) ;
#13695 = DIRECTION ( 'NONE',  ( -1.000000000000000000, 0.000000000000000000, 0.000000000000000000 ) ) ;
#13696 = VECTOR ( 'NONE', #3679, 1000.000000000000000 ) ;
#13697 = VERTEX_POINT ( 'NONE', #50216 ) ;
#13698 = CARTESIAN_POINT ( 'NONE',  ( 275.0000000000000000, -38.65000000000095781, 14.49999999999903899 ) ) ;
#13699 = VECTOR ( 'NONE', #6784, 1000.000000000000000 ) ;
#13700 = ORIENTED_EDGE ( 'NONE', *, *, #19816, .T. ) ;
#13701 = FACE_OUTER_BOUND ( 'NONE', #55451, .T. ) ;
#13702 = DIRECTION ( 'NONE',  ( 0.000000000000000000, -1.000000000000000000, 0.000000000000000000 ) ) ;
#13703 = EDGE_CURVE ( 'NONE', #21641, #50270, #39261, .T. ) ;
#13704 = ORIENTED_EDGE ( 'NONE', *, *, #62041, .T. ) ;
#13705 = CARTESIAN_POINT ( 'NONE',  ( 0.9555237378827827754, -9.929523737882790968, 54.00000000000000711 ) ) ;
#13706 = ORIENTED_EDGE ( 'NONE', *, *, #65120, .F. ) ;
#13707 = AXIS2_PLACEMENT_3D ( 'NONE', #53830, #48168, #26950 ) ;
#13708 = CLOSED_SHELL ( 'NONE', ( #39678, #17573, #61161, #40415, #52899, #67510, #53452, #43063 ) ) ;
#13709 = CARTESIAN_POINT ( 'NONE',  ( 8.406483450353379183, -7.616533956692325802, 455.0000000000000568 ) ) ;
#13710 = ORIENTED_EDGE ( 'NONE', *, *, #3857, .F. ) ;
#13711 = ORIENTED_EDGE ( 'NONE', *, *, #57610, .F. ) ;
#13712 = CARTESIAN_POINT ( 'NONE',  ( 41.09999999999999432, 20.60000000000000142, 13.86939075806900057 ) ) ;
#13713 = ORIENTED_EDGE ( 'NONE', *, *, #32369, .T. ) ;
#13714 = ORIENTED_EDGE ( 'NONE', *, *, #15116, .F. ) ;
#13715 = DIRECTION ( 'NONE',  ( -1.062075597536821678E-14, -1.000000000000000000, 0.000000000000000000 ) ) ;
#13716 = LINE ( 'NONE', #2752, #68652 ) ;
#13717 = B_SPLINE_CURVE_WITH_KNOTS ( 'NONE', 3,
 ( #19338, #19680, #36663, #47274, #68137, #57873 ),
 .UNSPECIFIED., .F., .F.,
 ( 4, 2, 4 ),
 ( 0.0002380763768115301549, 0.7291065797294569162, 1.457975083082102330 ),
 .UNSPECIFIED. ) ;
#13718 = CARTESIAN_POINT ( 'NONE',  ( 5.257023737882819070, -5.257023737882825287, 54.00000000000000711 ) ) ;
#13719 = ORIENTED_EDGE ( 'NONE', *, *, #5921, .T. ) ;
#13720 = DIRECTION ( 'NONE',  ( -0.000000000000000000, 3.673940397442059868E-16, -1.000000000000000000 ) ) ;
#13721 = VECTOR ( 'NONE', #36937, 1000.000000000000000 ) ;
#13723 = CARTESIAN_POINT ( 'NONE',  ( 11.12648345035340647, 9.093516549646563973, 455.0000000000000568 ) ) ;
#13722 = FACE_OUTER_BOUND ( 'NONE', #44601, .T. ) ;
#13724 = ORIENTED_EDGE ( 'NONE', *, *, #15123, .F. ) ;
#13726 = ORIENTED_EDGE ( 'NONE', *, *, #19740, .T. ) ;
#13725 = CARTESIAN_POINT ( 'NONE',  ( 146.5599459900709860, 9.000000000000001776, 276.7801873289890295 ) ) ;
#13727 = ORIENTED_EDGE ( 'NONE', *, *, #65606, .F. ) ;
#13728 = EDGE_CURVE ( 'NONE', #20190, #24845, #66815, .T. ) ;
#13729 = DIRECTION ( 'NONE',  ( 0.000000000000000000, 0.000000000000000000, 1.000000000000000000 ) ) ;
#13730 = ORIENTED_EDGE ( 'NONE', *, *, #11345, .F. ) ;
#13731 = CYLINDRICAL_SURFACE ( 'NONE', #49467, 3.499999999999850342 ) ;
#13732 = DIRECTION ( 'NONE',  ( -0.000000000000000000, -0.000000000000000000, -1.000000000000000000 ) ) ;
#13733 = AXIS2_PLACEMENT_3D ( 'NONE', #69066, #41842, #9325 ) ;
#13734 = ORIENTED_EDGE ( 'NONE', *, *, #37274, .F. ) ;
#13735 = ADVANCED_FACE ( 'NONE', ( #50906 ), #18372, .F. ) ;
#13736 = VERTEX_POINT ( 'NONE', #17697 ) ;
#13737 = FACE_OUTER_BOUND ( 'NONE', #12223, .T. ) ;
#13738 = CARTESIAN_POINT ( 'NONE',  ( 9.703773737882785966, -9.703773737882823269, 54.00000000000000711 ) ) ;
#13739 = EDGE_CURVE ( 'NONE', #12315, #69253, #6357, .T. ) ;
#13740 = ADVANCED_FACE ( 'NONE', ( #1775 ), #34641, .F. ) ;
#13741 = ORIENTED_EDGE ( 'NONE', *, *, #55021, .T. ) ;
#13742 = CARTESIAN_POINT ( 'NONE',  ( -10.19191654964685156, -9.804883450353383267, 455.0000000000000568 ) ) ;
#13743 = CARTESIAN_POINT ( 'NONE',  ( 10.00000000000000000, 18.00000000000000355, -21.00000000000000000 ) ) ;
#13744 = CARTESIAN_POINT ( 'NONE',  ( 7.250000000000004441, 7.450000000000001954, -12.50000000000000000 ) ) ;
#13745 = AXIS2_PLACEMENT_3D ( 'NONE', #16290, #65432, #38558 ) ;
#13746 = EDGE_LOOP ( 'NONE', ( #21987, #36631, #56829, #4876 ) ) ;
#13747 = VECTOR ( 'NONE', #69333, 1000.000000000000114 ) ;
#13748 = DIRECTION ( 'NONE',  ( -1.000000000000000000, -1.570596175624152290E-15, 0.000000000000000000 ) ) ;
#13749 = EDGE_CURVE ( 'NONE', #48624, #36267, #28950, .T. ) ;
#13750 = CARTESIAN_POINT ( 'NONE',  ( 24.90000000000000213, -0.1999999999911795112, 8.826273045769999343E-12 ) ) ;
#13751 = VERTEX_POINT ( 'NONE', #56225 ) ;
#13753 = ORIENTED_EDGE ( 'NONE', *, *, #55882, .F. ) ;
#13752 = DIRECTION ( 'NONE',  ( 1.000000000000000000, 0.000000000000000000, 0.000000000000000000 ) ) ;
#13754 = DIRECTION ( 'NONE',  ( -1.836970198721029934E-16, 1.836970198721036590E-16, -1.000000000000000000 ) ) ;
#13755 = DIRECTION ( 'NONE',  ( 0.000000000000000000, 0.000000000000000000, 1.000000000000000000 ) ) ;
#13756 = DIRECTION ( 'NONE',  ( 0.000000000000000000, 0.000000000000000000, -1.000000000000000000 ) ) ;
#13757 = VECTOR ( 'NONE', #18225, 1000.000000000000000 ) ;
#13758 = AXIS2_PLACEMENT_3D ( 'NONE', #10582, #53733, #69286 ) ;
#13759 = DIRECTION ( 'NONE',  ( -1.254221251785257574E-14, -1.000000000000000000, -1.836970198721013171E-16 ) ) ;
#13760 = CARTESIAN_POINT ( 'NONE',  ( 283.0000000000000568, -26.28355339059299922, 9.766446609406699508 ) ) ;
#13761 = EDGE_CURVE ( 'NONE', #67569, #41004, #55869, .T. ) ;
#13762 = ORIENTED_EDGE ( 'NONE', *, *, #16872, .T. ) ;
#13763 = CARTESIAN_POINT ( 'NONE',  ( -9.689999999999999503, -10.50000000000000178, 0.000000000000000000 ) ) ;
#13764 = DIRECTION ( 'NONE',  ( 0.000000000000000000, 1.000000000000000000, 0.000000000000000000 ) ) ;
#13765 = VECTOR ( 'NONE', #55204, 1000.000000000000000 ) ;
#13767 = EDGE_CURVE ( 'NONE', #24647, #31689, #11980, .T. ) ;
#13766 = CARTESIAN_POINT ( 'NONE',  ( 4.046023737882819660, -3.157023737882826087, 54.00000000000000711 ) ) ;
#13769 = ORIENTED_EDGE ( 'NONE', *, *, #41480, .F. ) ;
#13768 = CYLINDRICAL_SURFACE ( 'NONE', #10742, 1.999999999999314770 ) ;
#13770 = CARTESIAN_POINT ( 'NONE',  ( -9.404046420174113408, -1.866219381641437636, 455.0000000000000568 ) ) ;
#13771 = FACE_BOUND ( 'NONE', #50801, .T. ) ;
#13772 = AXIS2_PLACEMENT_3D ( 'NONE', #62209, #67873, #25091 ) ;
#13773 = ORIENTED_EDGE ( 'NONE', *, *, #20766, .F. ) ;
#13774 = ORIENTED_EDGE ( 'NONE', *, *, #15210, .T. ) ;
#13775 = CARTESIAN_POINT ( 'NONE',  ( 30.00000000000000000, -9.199999999999999289, -12.69999999999986073 ) ) ;
#13776 = CARTESIAN_POINT ( 'NONE',  ( 49.00000000000000000, -0.1999999999911430404, -8.864436962241481021E-12 ) ) ;
#13777 = EDGE_CURVE ( 'NONE', #43815, #51738, #12362, .T. ) ;
#13778 = ORIENTED_EDGE ( 'NONE', *, *, #9846, .T. ) ;
#13779 = CARTESIAN_POINT ( 'NONE',  ( 11.00000000000000000, -11.50000000000082068, 10.20500000000000007 ) ) ;
#13780 = DIRECTION ( 'NONE',  ( 0.000000000000000000, -1.000000000000000000, 0.000000000000000000 ) ) ;
#13781 = DIRECTION ( 'NONE',  ( -1.000000000000000000, 0.000000000000000000, 0.000000000000000000 ) ) ;
#13782 = DIRECTION ( 'NONE',  ( -1.836970198721029934E-16, -1.836970198721010706E-16, 1.000000000000000000 ) ) ;
#13783 = ORIENTED_EDGE ( 'NONE', *, *, #38873, .T. ) ;
#13784 = CARTESIAN_POINT ( 'NONE',  ( 10.05377373788281581, 8.916576262117182239, 54.00000000000000711 ) ) ;
#13785 = VERTEX_POINT ( 'NONE', #2127 ) ;
#13786 = DIRECTION ( 'NONE',  ( 0.000000000000000000, 0.000000000000000000, 1.000000000000000000 ) ) ;
#13787 = ORIENTED_EDGE ( 'NONE', *, *, #7987, .F. ) ;
#13788 = LINE ( 'NONE', #40314, #67477 ) ;
#13789 = CIRCLE ( 'NONE', #11514, 0.5000000000001392220 ) ;
#13790 = EDGE_CURVE ( 'NONE', #46624, #54560, #7497, .T. ) ;
#13791 = FACE_OUTER_BOUND ( 'NONE', #51037, .T. ) ;
#13792 = DIRECTION ( 'NONE',  ( 0.000000000000000000, 0.000000000000000000, -1.000000000000000000 ) ) ;
#13793 = VERTEX_POINT ( 'NONE', #60132 ) ;
#13794 = ORIENTED_EDGE ( 'NONE', *, *, #34729, .T. ) ;
#13795 = AXIS2_PLACEMENT_3D ( 'NONE', #58311, #10211, #20812 ) ;
#13796 = CYLINDRICAL_SURFACE ( 'NONE', #1357, 0.2000000000000005107 ) ;
#13797 = ORIENTED_EDGE ( 'NONE', *, *, #52975, .F. ) ;
#13798 = EDGE_CURVE ( 'NONE', #9544, #48304, #44914, .T. ) ;
#13799 = ORIENTED_EDGE ( 'NONE', *, *, #1493, .F. ) ;
#13800 = CARTESIAN_POINT ( 'NONE',  ( 8.250000000000005329, 0.000000000000000000, -23.50000000000000000 ) ) ;
#13801 = CARTESIAN_POINT ( 'NONE',  ( 50.83090410532631864, 63.65740854044500452, 10.00000000000000000 ) ) ;
#13802 = CARTESIAN_POINT ( 'NONE',  ( 280.0000000000000000, -53.81370849898476649, -20.00000000000000000 ) ) ;
#13803 = CARTESIAN_POINT ( 'NONE',  ( 7.450000000000004619, -1.336933437520057563E-15, -10.50000000000000000 ) ) ;
#13804 = ORIENTED_EDGE ( 'NONE', *, *, #9742, .T. ) ;
#13805 = EDGE_CURVE ( 'NONE', #58919, #8225, #27805, .T. ) ;
#13806 = AXIS2_PLACEMENT_3D ( 'NONE', #11716, #33303, #54881 ) ;
#13807 = LINE ( 'NONE', #12741, #4052 ) ;
#13809 = DIRECTION ( 'NONE',  ( 0.000000000000000000, 0.000000000000000000, -1.000000000000000000 ) ) ;
#13808 = CARTESIAN_POINT ( 'NONE',  ( -7.394232575409614761, 6.775514141871308738, 54.00000000000000711 ) ) ;
#13810 = ORIENTED_EDGE ( 'NONE', *, *, #12726, .F. ) ;
#13811 = ADVANCED_FACE ( 'NONE', ( #6400 ), #27967, .T. ) ;
#13813 = ORIENTED_EDGE ( 'NONE', *, *, #11995, .T. ) ;
#13812 = DIRECTION ( 'NONE',  ( 0.000000000000000000, 0.000000000000000000, -1.000000000000000000 ) ) ;
#13814 = ORIENTED_EDGE ( 'NONE', *, *, #52579, .F. ) ;
#13815 = VERTEX_POINT ( 'NONE', #65788 ) ;
#13816 = VECTOR ( 'NONE', #43981, 1000.000000000000000 ) ;
#13817 = EDGE_CURVE ( 'NONE', #63555, #21380, #67326, .T. ) ;
#13818 = CARTESIAN_POINT ( 'NONE',  ( 8.093267424590464998, -8.711985858128699078, 54.00000000000000711 ) ) ;
#13819 = FACE_OUTER_BOUND ( 'NONE', #45472, .T. ) ;
#13820 = AXIS2_PLACEMENT_3D ( 'NONE', #68777, #41897, #36589 ) ;
#13821 = ORIENTED_EDGE ( 'NONE', *, *, #17570, .T. ) ;
#13822 = ORIENTED_EDGE ( 'NONE', *, *, #34479, .T. ) ;
#13823 = ADVANCED_FACE ( 'NONE', ( #33613 ), #6729, .T. ) ;
#13824 = EDGE_CURVE ( 'NONE', #10241, #30976, #63277, .T. ) ;
#13825 = AXIS2_PLACEMENT_3D ( 'NONE', #44120, #65698, #27525 ) ;
#13826 = DIRECTION ( 'NONE',  ( 0.000000000000000000, -0.000000000000000000, -1.000000000000000000 ) ) ;
#13827 = CARTESIAN_POINT ( 'NONE',  ( 30.00000000000000000, -11.10796162543699950, -9.102987789146602893 ) ) ;
#13828 = ORIENTED_EDGE ( 'NONE', *, *, #34039, .F. ) ;
#13829 = ADVANCED_FACE ( 'NONE', ( #40995 ), #68587, .F. ) ;
#13830 = EDGE_CURVE ( 'NONE', #18780, #46315, #45961, .T. ) ;
#13831 = ORIENTED_EDGE ( 'NONE', *, *, #66754, .T. ) ;
#13832 = CARTESIAN_POINT ( 'NONE',  ( 10.20488345035338185, -9.804883450353528929, 455.0000000000000568 ) ) ;
#13833 = CARTESIAN_POINT ( 'NONE',  ( -25.50000000000000355, -15.12100000000000044, -22.50000000000000000 ) ) ;
#13834 = ORIENTED_EDGE ( 'NONE', *, *, #46080, .F. ) ;
#13835 = EDGE_CURVE ( 'NONE', #43261, #56939, #13433, .T. ) ;
#13836 = LINE ( 'NONE', #56624, #20078 ) ;
#13837 = CARTESIAN_POINT ( 'NONE',  ( 283.0000000000000568, -32.94999999999885176, 7.700000000000000178 ) ) ;
#13839 = ORIENTED_EDGE ( 'NONE', *, *, #25037, .T. ) ;
#13838 = DIRECTION ( 'NONE',  ( -0.7071067811865474617, -0.7071067811865474617, -0.000000000000000000 ) ) ;
#13840 = ORIENTED_EDGE ( 'NONE', *, *, #7858, .T. ) ;
#13841 = DIRECTION ( 'NONE',  ( -1.000000000000000000, 0.000000000000000000, -0.000000000000000000 ) ) ;
#13842 = LINE ( 'NONE', #15858, #31138 ) ;
#13843 = DIRECTION ( 'NONE',  ( 1.000000000000000000, -5.981805089575194965E-17, 0.000000000000000000 ) ) ;
#13844 = VECTOR ( 'NONE', #18558, 1000.000000000000000 ) ;
#13845 = DIRECTION ( 'NONE',  ( -0.000000000000000000, -0.000000000000000000, -1.000000000000000000 ) ) ;
#13846 = CARTESIAN_POINT ( 'NONE',  ( 7.250000000000005329, 7.250000000000000888, -22.00000000000000000 ) ) ;
#13847 = DIRECTION ( 'NONE',  ( 1.000000000000000000, -0.000000000000000000, 0.000000000000000000 ) ) ;
#13848 = CARTESIAN_POINT ( 'NONE',  ( 176.4833316329832940, 9.000000000000001776, 322.4587476295993156 ) ) ;
#13849 = AXIS2_PLACEMENT_3D ( 'NONE', #42291, #37016, #25706 ) ;
#13850 = EDGE_CURVE ( 'NONE', #21103, #38962, #29685, .T. ) ;
#13851 = VERTEX_POINT ( 'NONE', #41703 ) ;
#13852 = DIRECTION ( 'NONE',  ( 0.000000000000000000, 0.000000000000000000, -1.000000000000000000 ) ) ;
#13855 = ORIENTED_EDGE ( 'NONE', *, *, #32802, .F. ) ;
#13854 = ADVANCED_FACE ( 'NONE', ( #41348 ), #8114, .F. ) ;
#13853 = DIRECTION ( 'NONE',  ( -0.000000000000000000, 3.673940397442059868E-16, -1.000000000000000000 ) ) ;
#13856 = LINE ( 'NONE', #8899, #59301 ) ;
#13857 = LINE ( 'NONE', #40731, #45894 ) ;
#13858 = DIRECTION ( 'NONE',  ( 1.000000000000000000, -0.000000000000000000, -0.000000000000000000 ) ) ;
#13859 = DIRECTION ( 'NONE',  ( 0.000000000000000000, 0.000000000000000000, -1.000000000000000000 ) ) ;
#13860 = DIRECTION ( 'NONE',  ( 0.000000000000000000, -1.000000000000000000, 0.000000000000000000 ) ) ;
#13861 = ORIENTED_EDGE ( 'NONE', *, *, #37158, .F. ) ;
#13862 = DIRECTION ( 'NONE',  ( -1.000000000000000000, 0.000000000000000000, 0.000000000000000000 ) ) ;
#13863 = DIRECTION ( 'NONE',  ( -2.135044278125299371E-15, -1.000000000000000000, 0.000000000000000000 ) ) ;
#13864 = VERTEX_POINT ( 'NONE', #14846 ) ;
#13865 = FACE_OUTER_BOUND ( 'NONE', #29745, .T. ) ;
#13866 = LINE ( 'NONE', #39686, #68043 ) ;
#13867 = AXIS2_PLACEMENT_3D ( 'NONE', #26959, #15301, #59129 ) ;
#13868 = ORIENTED_EDGE ( 'NONE', *, *, #58761, .T. ) ;
#13869 = CARTESIAN_POINT ( 'NONE',  ( -7.250000000000000888, 7.250000000000001776, -7.000000000000000000 ) ) ;
#13870 = ORIENTED_EDGE ( 'NONE', *, *, #23861, .T. ) ;
#13871 = ORIENTED_EDGE ( 'NONE', *, *, #40562, .T. ) ;
#13872 = VECTOR ( 'NONE', #10139, 1000.000000000000000 ) ;
#13873 = DIRECTION ( 'NONE',  ( -1.836970198721029934E-16, 1.836970198721036590E-16, -1.000000000000000000 ) ) ;
#13874 = CARTESIAN_POINT ( 'NONE',  ( 283.0000000000000568, -23.50007830495750127, 12.28007262201345995 ) ) ;
#13875 = CARTESIAN_POINT ( 'NONE',  ( -14.25000000000000000, -2.500000000000000000, 21.77831216351300014 ) ) ;
#13876 = VECTOR ( 'NONE', #14040, 1000.000000000000000 ) ;
#13877 = CARTESIAN_POINT ( 'NONE',  ( 7.250000000000005329, -7.249999999999998224, -23.00000000000000000 ) ) ;
#13878 = AXIS2_PLACEMENT_3D ( 'NONE', #24728, #19755, #52303 ) ;
#13879 = DIRECTION ( 'NONE',  ( -1.000000000000000000, 0.000000000000000000, 0.000000000000000000 ) ) ;
#13880 = ORIENTED_EDGE ( 'NONE', *, *, #24403, .F. ) ;
#13881 = VERTEX_POINT ( 'NONE', #52686 ) ;
#13883 = ORIENTED_EDGE ( 'NONE', *, *, #27720, .T. ) ;
#13882 = DIRECTION ( 'NONE',  ( 0.000000000000000000, 0.000000000000000000, -1.000000000000000000 ) ) ;
#13884 = ORIENTED_EDGE ( 'NONE', *, *, #30128, .T. ) ;
#13885 = EDGE_CURVE ( 'NONE', #11924, #46765, #48154, .T. ) ;
#13886 = FACE_OUTER_BOUND ( 'NONE', #64856, .T. ) ;
#13887 = VECTOR ( 'NONE', #39901, 1000.000000000000000 ) ;
#13888 = PLANE ( 'NONE',  #47859 ) ;
#13889 = DIRECTION ( 'NONE',  ( 0.000000000000000000, 0.000000000000000000, -1.000000000000000000 ) ) ;
#13890 = LINE ( 'NONE', #36508, #44385 ) ;
#13891 = EDGE_CURVE ( 'NONE', #4079, #28664, #24306, .T. ) ;
#13892 = DIRECTION ( 'NONE',  ( -1.000000000000000000, 0.000000000000000000, 0.000000000000000000 ) ) ;
#13893 = FACE_OUTER_BOUND ( 'NONE', #31432, .T. ) ;
#13894 = EDGE_CURVE ( 'NONE', #22546, #65963, #20140, .T. ) ;
#13895 = AXIS2_PLACEMENT_3D ( 'NONE', #55698, #40116, #50392 ) ;
#13896 = ORIENTED_EDGE ( 'NONE', *, *, #60442, .F. ) ;
#13897 = VERTEX_POINT ( 'NONE', #14491 ) ;
#13898 = EDGE_CURVE ( 'NONE', #24794, #25369, #51619, .T. ) ;
#13899 = ORIENTED_EDGE ( 'NONE', *, *, #61727, .F. ) ;
#13900 = EDGE_LOOP ( 'NONE', ( #49965, #67156, #52060, #41916 ) ) ;
#13901 = CARTESIAN_POINT ( 'NONE',  ( 30.00000000000000000, -17.14999999999999858, -27.00000000000000000 ) ) ;
#13902 = ADVANCED_FACE ( 'NONE', ( #9537 ), #24394, .F. ) ;
#13903 = ADVANCED_FACE ( 'NONE', ( #14128 ), #56903, .F. ) ;
#13904 = TOROIDAL_SURFACE ( 'NONE', #60182, 3.299999999999474909, 0.2000000000005234813 ) ;
#13905 = CARTESIAN_POINT ( 'NONE',  ( -10.91351654964666906, -2.906483450353290809, 195.0000000000000284 ) ) ;
#13906 = CARTESIAN_POINT ( 'NONE',  ( 39.00000000000000000, -16.96999999999999886, 21.00000000000000000 ) ) ;
#13907 = EDGE_LOOP ( 'NONE', ( #61341, #38932, #54987, #54004 ) ) ;
#13908 = ORIENTED_EDGE ( 'NONE', *, *, #29756, .F. ) ;
#13909 = ORIENTED_EDGE ( 'NONE', *, *, #38950, .T. ) ;
#13910 = DIRECTION ( 'NONE',  ( 0.000000000000000000, -1.000000000000000000, 0.000000000000000000 ) ) ;
#13911 = ORIENTED_EDGE ( 'NONE', *, *, #44360, .F. ) ;
#13912 = ORIENTED_EDGE ( 'NONE', *, *, #6735, .T. ) ;
#13913 = FACE_OUTER_BOUND ( 'NONE', #52449, .T. ) ;
#13914 = ORIENTED_EDGE ( 'NONE', *, *, #44980, .F. ) ;
#13915 = VERTEX_POINT ( 'NONE', #24745 ) ;
#13916 = DIRECTION ( 'NONE',  ( 0.000000000000000000, 0.000000000000000000, -1.000000000000000000 ) ) ;
#13918 = ORIENTED_EDGE ( 'NONE', *, *, #64757, .F. ) ;
#13917 = FACE_OUTER_BOUND ( 'NONE', #60692, .T. ) ;
#13919 = ORIENTED_EDGE ( 'NONE', *, *, #26624, .T. ) ;
#13920 = DIRECTION ( 'NONE',  ( 0.000000000000000000, 1.000000000000000000, 0.000000000000000000 ) ) ;
#13922 = CARTESIAN_POINT ( 'NONE',  ( -11.00000000000000000, -5.200000000000001066, -9.400000000000005684 ) ) ;
#13921 = AXIS2_PLACEMENT_3D ( 'NONE', #12146, #45708, #18846 ) ;
#13923 = CARTESIAN_POINT ( 'NONE',  ( 7.000000000000000000, -42.50000000000000000, 15.10000000000000142 ) ) ;
#13925 = ORIENTED_EDGE ( 'NONE', *, *, #61452, .F. ) ;
#13924 = DIRECTION ( 'NONE',  ( -0.6414496315691592399, 0.7671651518152985405, 2.587583378555133228E-16 ) ) ;
#13927 = ORIENTED_EDGE ( 'NONE', *, *, #282, .F. ) ;
#13926 = VECTOR ( 'NONE', #1104, 1000.000000000000000 ) ;
#13928 = AXIS2_PLACEMENT_3D ( 'NONE', #23876, #67004, #40122 ) ;
#13929 = AXIS2_PLACEMENT_3D ( 'NONE', #64457, #47826, #42172 ) ;
#13930 = CYLINDRICAL_SURFACE ( 'NONE', #41923, 2.204799999999998761 ) ;
#13931 = FACE_OUTER_BOUND ( 'NONE', #43130, .T. ) ;
#13932 = DIRECTION ( 'NONE',  ( 9.050731179009442381E-15, 1.000000000000000000, 3.673940397442060361E-16 ) ) ;
#13933 = VECTOR ( 'NONE', #66011, 1000.000000000000000 ) ;
#13934 = AXIS2_PLACEMENT_3D ( 'NONE', #45849, #2372, #23934 ) ;
#13935 = VERTEX_POINT ( 'NONE', #40651 ) ;
#13936 = LINE ( 'NONE', #57066, #58605 ) ;
#13937 = ADVANCED_FACE ( 'NONE', ( #67883 ), #35687, .F. ) ;
#13938 = DIRECTION ( 'NONE',  ( -0.5000000000000038858, -0.8660254037844363761, 0.000000000000000000 ) ) ;
#13939 = CARTESIAN_POINT ( 'NONE',  ( -11.99351654964671354, 11.18071654964658990, 455.0000000000000568 ) ) ;
#13940 = ORIENTED_EDGE ( 'NONE', *, *, #30275, .T. ) ;
#13941 = EDGE_CURVE ( 'NONE', #4410, #67915, #53701, .T. ) ;
#13942 = DIRECTION ( 'NONE',  ( 0.000000000000000000, 0.000000000000000000, -1.000000000000000000 ) ) ;
#13943 = CARTESIAN_POINT ( 'NONE',  ( -6.344366288193410419, 5.779227145995219139, 54.00000000000000711 ) ) ;
#13944 = CARTESIAN_POINT ( 'NONE',  ( 3.682023737882818448, 9.722976262117203561, 54.00000000000000711 ) ) ;
#13945 = CIRCLE ( 'NONE', #384, 4.000000000000000000 ) ;
#13946 = ORIENTED_EDGE ( 'NONE', *, *, #58145, .F. ) ;
#13947 = DIRECTION ( 'NONE',  ( 0.000000000000000000, 1.000000000000000000, -0.000000000000000000 ) ) ;
#13948 = DIRECTION ( 'NONE',  ( -1.000000000000000000, 0.000000000000000000, 0.000000000000000000 ) ) ;
#13949 = ORIENTED_EDGE ( 'NONE', *, *, #15667, .F. ) ;
#13950 = DIRECTION ( 'NONE',  ( 1.000000000000000000, 0.000000000000000000, 0.000000000000000000 ) ) ;
#13951 = DIRECTION ( 'NONE',  ( -1.000000000000000000, 0.000000000000000000, 0.000000000000000000 ) ) ;
#13952 = CARTESIAN_POINT ( 'NONE',  ( -6.606374702650169795, 7.252248008019353875, 195.0000000000000284 ) ) ;
#13953 = VECTOR ( 'NONE', #41171, 1000.000000000000000 ) ;
#13954 = CARTESIAN_POINT ( 'NONE',  ( -5.993516549646711766, 3.593516549646603497, 195.0000000000000284 ) ) ;
#13955 = DIRECTION ( 'NONE',  ( 0.000000000000000000, 0.000000000000000000, 1.000000000000000000 ) ) ;
#13956 = ORIENTED_EDGE ( 'NONE', *, *, #49363, .T. ) ;
#13957 = DIRECTION ( 'NONE',  ( 1.836970198721029934E-16, 1.836970198721010706E-16, -1.000000000000000000 ) ) ;
#13958 = CARTESIAN_POINT ( 'NONE',  ( -25.50000000000000355, -15.50000000000000000, 22.50000000000000000 ) ) ;
#13959 = DIRECTION ( 'NONE',  ( 1.000000000000000000, -0.000000000000000000, 0.000000000000000000 ) ) ;
#13960 = SURFACE_SIDE_STYLE ('',( #25277 ) ) ;
#13961 = CARTESIAN_POINT ( 'NONE',  ( -9.690000000000001279, -9.690000000000001279, -4.250000000000000000 ) ) ;
#13962 = ORIENTED_EDGE ( 'NONE', *, *, #21002, .T. ) ;
#13964 = ORIENTED_EDGE ( 'NONE', *, *, #20622, .F. ) ;
#13963 = CYLINDRICAL_SURFACE ( 'NONE', #25080, 0.2000000000000005107 ) ;
#13965 = EDGE_CURVE ( 'NONE', #46962, #22289, #31088, .T. ) ;
#13966 = VECTOR ( 'NONE', #39590, 1000.000000000000000 ) ;
#13967 = AXIS2_PLACEMENT_3D ( 'NONE', #57118, #30954, #69131 ) ;
#13968 = DIRECTION ( 'NONE',  ( -0.000000000000000000, -0.000000000000000000, -1.000000000000000000 ) ) ;
#13969 = CARTESIAN_POINT ( 'NONE',  ( 283.0000000000000568, -32.94999999999885176, 7.700000000000000178 ) ) ;
#13970 = LINE ( 'NONE', #68423, #51116 ) ;
#13971 = ORIENTED_EDGE ( 'NONE', *, *, #51215, .T. ) ;
#13972 = MECHANICAL_DESIGN_GEOMETRIC_PRESENTATION_REPRESENTATION (  '', ( #11749 ), #28655 ) ;
#13973 = DIRECTION ( 'NONE',  ( 0.000000000000000000, 0.000000000000000000, 1.000000000000000000 ) ) ;
#13974 = AXIS2_PLACEMENT_3D ( 'NONE', #66292, #34435, #39748 ) ;
#13975 = VERTEX_POINT ( 'NONE', #47359 ) ;
#13976 = CIRCLE ( 'NONE', #9498, 1.929199999999998028 ) ;
#13978 = ORIENTED_EDGE ( 'NONE', *, *, #28042, .T. ) ;
#13977 = VECTOR ( 'NONE', #47467, 1000.000000000000000 ) ;
#13979 = AXIS2_PLACEMENT_3D ( 'NONE', #30447, #9940, #52367 ) ;
#13980 = ORIENTED_EDGE ( 'NONE', *, *, #43454, .F. ) ;
#13981 = DIRECTION ( 'NONE',  ( -1.000000000000000000, 0.000000000000000000, 0.000000000000000000 ) ) ;
#13982 = EDGE_CURVE ( 'NONE', #54230, #65046, #63846, .T. ) ;
#13983 = ADVANCED_FACE ( 'NONE', ( #58337 ), #36767, .F. ) ;
#13984 = DIRECTION ( 'NONE',  ( -0.000000000000000000, 1.000000000000000000, -0.000000000000000000 ) ) ;
#13985 = DIRECTION ( 'NONE',  ( -1.000000000000000000, 0.000000000000000000, -0.000000000000000000 ) ) ;
#13986 = EDGE_CURVE ( 'NONE', #12586, #30907, #10233, .T. ) ;
#13987 = VERTEX_POINT ( 'NONE', #15886 ) ;
#13988 = EDGE_LOOP ( 'NONE', ( #41139, #47706, #32058, #15481 ) ) ;
#13989 = PLANE ( 'NONE',  #54984 ) ;
#13990 = DIRECTION ( 'NONE',  ( -0.000000000000000000, -0.000000000000000000, -1.000000000000000000 ) ) ;
#13991 = ORIENTED_EDGE ( 'NONE', *, *, #34009, .T. ) ;
#13992 = ORIENTED_EDGE ( 'NONE', *, *, #38863, .T. ) ;
#13993 = VERTEX_POINT ( 'NONE', #26157 ) ;
#13994 = ORIENTED_EDGE ( 'NONE', *, *, #51274, .F. ) ;
#13995 = CARTESIAN_POINT ( 'NONE',  ( 9.841277389592722358, -1.690483450353395201, 195.0000000000000284 ) ) ;
#13997 = EDGE_LOOP ( 'NONE', ( #7172, #26441, #429, #45791 ) ) ;
#13996 = DIRECTION ( 'NONE',  ( -1.000000000000000000, 0.000000000000000000, 0.000000000000000000 ) ) ;
#13998 = CARTESIAN_POINT ( 'NONE',  ( 16.75000000000000000, -2.500000000000000000, -21.77831216351300014 ) ) ;
#13999 = CARTESIAN_POINT ( 'NONE',  ( 10.50702373788281818, -9.795823737882813020, 54.00000000000000711 ) ) ;
#14000 = EDGE_LOOP ( 'NONE', ( #57859, #52707, #58890, #59657, #15265, #28385, #13994, #12118, #65367, #8391, #11135, #37322, #55653, #61972, #963, #31776, #3302, #7312, #32676, #47219 ) ) ;
#14001 = ORIENTED_EDGE ( 'NONE', *, *, #17234, .F. ) ;
#14002 = CIRCLE ( 'NONE', #55798, 0.5000000000079362072 ) ;
#14003 = CARTESIAN_POINT ( 'NONE',  ( -4.727349090213511573, -7.811466277050747919, 195.0000000000000284 ) ) ;
#14004 = DIRECTION ( 'NONE',  ( -1.000000000000000000, 0.000000000000000000, 0.000000000000000000 ) ) ;
#14005 = LINE ( 'NONE', #19314, #43954 ) ;
#14006 = CIRCLE ( 'NONE', #24166, 2.204799999999997873 ) ;
#14007 = CARTESIAN_POINT ( 'NONE',  ( -25.49999999999869971, -17.50000000000000000, -22.50000000000000000 ) ) ;
#14008 = PLANE ( 'NONE',  #55066 ) ;
#14010 = ORIENTED_EDGE ( 'NONE', *, *, #37707, .F. ) ;
#14009 = DIRECTION ( 'NONE',  ( -1.000000000000000000, 0.000000000000000000, 0.000000000000000000 ) ) ;
#14011 = ORIENTED_EDGE ( 'NONE', *, *, #26442, .T. ) ;
#14012 = EDGE_CURVE ( 'NONE', #58992, #48298, #37118, .T. ) ;
#14013 = CARTESIAN_POINT ( 'NONE',  ( 15.50000000000000000, -2.500000000000000000, 21.05662432702600029 ) ) ;
#14014 = CARTESIAN_POINT ( 'NONE',  ( 25.57999999999999829, 3.010794155703768650E-16, -2.458500000000000796 ) ) ;
#14015 = EDGE_CURVE ( 'NONE', #22396, #52737, #67376, .T. ) ;
#14016 = EDGE_CURVE ( 'NONE', #68360, #43734, #59017, .T. ) ;
#14017 = CIRCLE ( 'NONE', #8408, 24.99999999998784972 ) ;
#14019 = CIRCLE ( 'NONE', #2763, 0.1749999999999989342 ) ;
#14018 = DIRECTION ( 'NONE',  ( -0.000000000000000000, -0.000000000000000000, -1.000000000000000000 ) ) ;
#14020 = CARTESIAN_POINT ( 'NONE',  ( 7.000000000000000000, -26.42999999999999972, 5.874955318979029784 ) ) ;
#14021 = EDGE_CURVE ( 'NONE', #18603, #11471, #20489, .T. ) ;
#14022 = VECTOR ( 'NONE', #34669, 1000.000000000000000 ) ;
#14023 = CARTESIAN_POINT ( 'NONE',  ( 1.866219381641437192, 9.404046420174054788, 195.0000000000000284 ) ) ;
#14024 = ORIENTED_EDGE ( 'NONE', *, *, #631, .T. ) ;
#14025 = DIRECTION ( 'NONE',  ( 0.000000000000000000, 1.000000000000000000, 0.000000000000000000 ) ) ;
#14026 = DIRECTION ( 'NONE',  ( 1.000000000000000000, -6.308085367188446447E-15, 0.000000000000000000 ) ) ;
#14027 = CARTESIAN_POINT ( 'NONE',  ( 15.89999999999999680, -14.06939075806902117, -20.80000000000000426 ) ) ;
#14028 = LINE ( 'NONE', #29233, #60444 ) ;
#14029 = CARTESIAN_POINT ( 'NONE',  ( 14.89999999999999680, -0.1999999999911795112, 8.826273045769999343E-12 ) ) ;
#14030 = LINE ( 'NONE', #13685, #31918 ) ;
#14031 = AXIS2_PLACEMENT_3D ( 'NONE', #34672, #55555, #45990 ) ;
#14032 = LINE ( 'NONE', #30309, #36359 ) ;
#14033 = ORIENTED_EDGE ( 'NONE', *, *, #24177, .T. ) ;
#14034 = DIRECTION ( 'NONE',  ( 0.000000000000000000, -1.000000000000000000, -6.036837696397607468E-13 ) ) ;
#14035 = PLANE ( 'NONE',  #12533 ) ;
#14036 = ORIENTED_EDGE ( 'NONE', *, *, #28352, .F. ) ;
#14037 = DIRECTION ( 'NONE',  ( -0.5773502691896273964, -0.5773502691896268413, 0.5773502691896232886 ) ) ;
#14038 = CYLINDRICAL_SURFACE ( 'NONE', #29955, 3.500000000000003109 ) ;
#14039 = DIRECTION ( 'NONE',  ( 0.000000000000000000, 0.000000000000000000, 1.000000000000000000 ) ) ;
#14040 = DIRECTION ( 'NONE',  ( -1.000000000000000000, 0.000000000000000000, 0.000000000000000000 ) ) ;
#14041 = CARTESIAN_POINT ( 'NONE',  ( 5.552858015815571591, 7.342976262117199227, 54.00000000000000711 ) ) ;
#14042 = ORIENTED_EDGE ( 'NONE', *, *, #53456, .F. ) ;
#14043 = DIRECTION ( 'NONE',  ( 0.000000000000000000, -0.9938079899998859545, 0.1111111111112941946 ) ) ;
#14044 =( BOUNDED_CURVE ( )  B_SPLINE_CURVE ( 3, ( #48958, #43649, #60592, #1536 ),
 .UNSPECIFIED., .F., .F. ) 
 B_SPLINE_CURVE_WITH_KNOTS ( ( 4, 4 ),
 ( 0.000000000000000000, 1.570796326794896558 ),
 .UNSPECIFIED. ) 
 CURVE ( )  GEOMETRIC_REPRESENTATION_ITEM ( )  RATIONAL_B_SPLINE_CURVE ( ( 1.000000000000000000, 0.8047378541243649375, 0.8047378541243649375, 1.000000000000000000 ) ) 
 REPRESENTATION_ITEM ( '' )  );
#14045 = VERTEX_POINT ( 'NONE', #42406 ) ;
#14046 = CARTESIAN_POINT ( 'NONE',  ( 289.5000000000000000, -0.5000000000000000000, 27.00000000000000000 ) ) ;
#14047 = DIRECTION ( 'NONE',  ( -1.000000000000000000, 0.000000000000000000, 0.000000000000000000 ) ) ;
#14048 = VERTEX_POINT ( 'NONE', #47711 ) ;
#14049 = CIRCLE ( 'NONE', #68271, 0.2000000000000005107 ) ;
#14050 = CARTESIAN_POINT ( 'NONE',  ( 7.852485183456924034, 3.417780618358489786, 455.0000000000000568 ) ) ;
#14051 = VECTOR ( 'NONE', #53297, 1000.000000000000000 ) ;
#14052 = ORIENTED_EDGE ( 'NONE', *, *, #69769, .T. ) ;
#14053 = DIRECTION ( 'NONE',  ( 0.000000000000000000, 0.7278708115913771204, 0.6857142857147648929 ) ) ;
#14054 = VERTEX_POINT ( 'NONE', #21879 ) ;
#14055 = ORIENTED_EDGE ( 'NONE', *, *, #3776, .T. ) ;
#14056 = DIRECTION ( 'NONE',  ( -0.6414496315691521344, -0.7671651518153044247, -2.309356642088966375E-17 ) ) ;
#14057 = ORIENTED_EDGE ( 'NONE', *, *, #12636, .F. ) ;
#14058 = VERTEX_POINT ( 'NONE', #37804 ) ;
#14059 = EDGE_CURVE ( 'NONE', #13697, #47387, #42381, .T. ) ;
#14060 = DIRECTION ( 'NONE',  ( 1.000000000000000000, 0.000000000000000000, 0.000000000000000000 ) ) ;
#14061 = CARTESIAN_POINT ( 'NONE',  ( -3.650476262117333892, -10.31452373788281740, 54.00000000000000711 ) ) ;
#14062 = AXIS2_PLACEMENT_3D ( 'NONE', #51879, #41966, #63888 ) ;
#14063 = VECTOR ( 'NONE', #14264, 1000.000000000000000 ) ;
#14064 = CARTESIAN_POINT ( 'NONE',  ( 283.0000000000000568, -21.00000000000000000, -12.50000000000000000 ) ) ;
#14065 = EDGE_CURVE ( 'NONE', #62186, #51473, #63635, .T. ) ;
#14066 = EDGE_CURVE ( 'NONE', #55064, #8160, #31813, .T. ) ;
#14067 = ORIENTED_EDGE ( 'NONE', *, *, #51436, .F. ) ;
#14068 = CARTESIAN_POINT ( 'NONE',  ( 7.000000000000000000, -41.99999999999906208, 14.49999999999903899 ) ) ;
#14070 = CARTESIAN_POINT ( 'NONE',  ( 26.90000000000000213, 13.66939075806899950, 20.80000000000000426 ) ) ;
#14069 = LINE ( 'NONE', #52623, #7861 ) ;
#14071 = AXIS2_PLACEMENT_3D ( 'NONE', #12995, #34569, #8041 ) ;
#14072 = VERTEX_POINT ( 'NONE', #10928 ) ;
#14075 = EDGE_LOOP ( 'NONE', ( #37192, #58893, #56346, #33075 ) ) ;
#14074 = EDGE_CURVE ( 'NONE', #52876, #18487, #37461, .T. ) ;
#14073 = LINE ( 'NONE', #3132, #45484 ) ;
#14076 = ORIENTED_EDGE ( 'NONE', *, *, #68255, .F. ) ;
#14077 = APPLICATION_PROTOCOL_DEFINITION ( 'draft international standard', 'automotive_design', 1998, #53971 ) ;
#14078 = VECTOR ( 'NONE', #19711, 1000.000000000000000 ) ;
#14079 = ADVANCED_FACE ( 'NONE', ( #64331 ), #27197, .F. ) ;
#14080 = CARTESIAN_POINT ( 'NONE',  ( 275.0000000000000000, -32.95000000000000284, -13.19999999999999929 ) ) ;
#14081 = ADVANCED_FACE ( 'NONE', ( #10575 ), #4932, .F. ) ;
#14083 = ORIENTED_EDGE ( 'NONE', *, *, #50402, .F. ) ;
#14082 = DIRECTION ( 'NONE',  ( 0.000000000000000000, 1.000000000000000000, 0.000000000000000000 ) ) ;
#14084 = CARTESIAN_POINT ( 'NONE',  ( -7.250000000000001776, -7.249999999999998224, -20.00000000000000000 ) ) ;
#14085 = AXIS2_PLACEMENT_3D ( 'NONE', #17242, #7315, #29230 ) ;
#14086 = CARTESIAN_POINT ( 'NONE',  ( 7.250000000000005329, 8.250000000000001776, -26.00000000000001066 ) ) ;
#14088 = ORIENTED_EDGE ( 'NONE', *, *, #48472, .F. ) ;
#14087 = VECTOR ( 'NONE', #64480, 1000.000000000000000 ) ;
#14089 = ORIENTED_EDGE ( 'NONE', *, *, #6011, .T. ) ;
#14090 = AXIS2_PLACEMENT_3D ( 'NONE', #36796, #349, #10958 ) ;
#14091 = FACE_OUTER_BOUND ( 'NONE', #49957, .T. ) ;
#14092 = ORIENTED_EDGE ( 'NONE', *, *, #58692, .F. ) ;
#14093 = CARTESIAN_POINT ( 'NONE',  ( 40.90000000000000568, 16.96999999999999886, 21.00000000000000000 ) ) ;
#14094 = FACE_OUTER_BOUND ( 'NONE', #45722, .T. ) ;
#14095 = DIRECTION ( 'NONE',  ( -0.000000000000000000, -0.000000000000000000, -1.000000000000000000 ) ) ;
#14096 = VERTEX_POINT ( 'NONE', #26496 ) ;
#14097 = CARTESIAN_POINT ( 'NONE',  ( 30.00000000000000000, -14.04000000000000092, -17.04524521594300523 ) ) ;
#14098 = LINE ( 'NONE', #35298, #16761 ) ;
#14099 = AXIS2_PLACEMENT_3D ( 'NONE', #36062, #9554, #31129 ) ;
#14101 = VERTEX_POINT ( 'NONE', #15556 ) ;
#14100 = DIRECTION ( 'NONE',  ( 0.000000000000000000, 1.000000000000000000, 0.000000000000000000 ) ) ;
#14103 = ORIENTED_EDGE ( 'NONE', *, *, #24449, .F. ) ;
#14102 = LINE ( 'NONE', #9160, #67066 ) ;
#14104 = DIRECTION ( 'NONE',  ( -0.000000000000000000, -0.000000000000000000, -1.000000000000000000 ) ) ;
#14105 = CARTESIAN_POINT ( 'NONE',  ( 4.201500623656003519, -4.740315990920286104, 455.0000000000000568 ) ) ;
#14106 = CIRCLE ( 'NONE', #29904, 3.499999999999849454 ) ;
#14107 = CARTESIAN_POINT ( 'NONE',  ( 22.14589803375000088, -15.50000000000000000, 21.50000000000000000 ) ) ;
#14108 = LINE ( 'NONE', #41330, #32810 ) ;
#14109 = EDGE_CURVE ( 'NONE', #4070, #44826, #35599, .T. ) ;
#14110 = CARTESIAN_POINT ( 'NONE',  ( 176.0064834503533575, -16.00648345035295250, 5.000000000000000000 ) ) ;
#14111 = ORIENTED_EDGE ( 'NONE', *, *, #61802, .T. ) ;
#14112 = DIRECTION ( 'NONE',  ( -3.491481338843133355E-15, -1.000000000000000000, -1.836970198721029934E-16 ) ) ;
#14113 = CARTESIAN_POINT ( 'NONE',  ( 275.0000000000000000, -42.00000000000000000, -15.10000000000000142 ) ) ;
#14114 = DIRECTION ( 'NONE',  ( -0.7071067811865474617, -0.7071067811865474617, -2.597868168706479611E-16 ) ) ;
#14116 = ORIENTED_EDGE ( 'NONE', *, *, #30675, .F. ) ;
#14115 = CARTESIAN_POINT ( 'NONE',  ( 4.456444791733522252E-16, 7.450000000000002842, -12.00000000000000000 ) ) ;
#14117 = VECTOR ( 'NONE', #59404, 1000.000000000000000 ) ;
#14118 = LINE ( 'NONE', #42044, #39186 ) ;
#14119 = AXIS2_PLACEMENT_3D ( 'NONE', #64360, #53753, #15919 ) ;
#14120 = DIRECTION ( 'NONE',  ( 0.000000000000000000, 1.000000000000000000, 3.673940397442059868E-16 ) ) ;
#14121 = AXIS2_PLACEMENT_3D ( 'NONE', #23627, #45899, #8777 ) ;
#14122 = VECTOR ( 'NONE', #22251, 1000.000000000000000 ) ;
#14123 = EDGE_CURVE ( 'NONE', #27624, #47490, #5289, .T. ) ;
#14124 = ORIENTED_EDGE ( 'NONE', *, *, #6444, .T. ) ;
#14125 = DIRECTION ( 'NONE',  ( 1.000000000000000000, -0.000000000000000000, 0.000000000000000000 ) ) ;
#14126 = CARTESIAN_POINT ( 'NONE',  ( -7.450000000000001954, -7.249999999999998224, -9.500000000000001776 ) ) ;
#14127 = ORIENTED_EDGE ( 'NONE', *, *, #25097, .F. ) ;
#14128 = FACE_OUTER_BOUND ( 'NONE', #67929, .T. ) ;
#14129 = VECTOR ( 'NONE', #35105, 1000.000000000000000 ) ;
#14130 = DIRECTION ( 'NONE',  ( 0.000000000000000000, 0.000000000000000000, -1.000000000000000000 ) ) ;
#14131 = ADVANCED_FACE ( 'NONE', ( #16588 ), #319, .F. ) ;
#14132 = LINE ( 'NONE', #24396, #1114 ) ;
#14133 = DIRECTION ( 'NONE',  ( 0.9583148474998867128, 0.000000000000000000, -0.2857142857143631365 ) ) ;
#14134 = STYLED_ITEM ( 'NONE', ( #44990 ), #44754 ) ;
#14135 = EDGE_LOOP ( 'NONE', ( #69268, #1617, #37887, #3638 ) ) ;
#14136 = DIRECTION ( 'NONE',  ( -1.794541526872559352E-16, -1.000000000000000000, 0.000000000000000000 ) ) ;
#14137 = ORIENTED_EDGE ( 'NONE', *, *, #57426, .T. ) ;
#14138 = ORIENTED_EDGE ( 'NONE', *, *, #63997, .T. ) ;
#14139 = VERTEX_POINT ( 'NONE', #12281 ) ;
#14140 = CARTESIAN_POINT ( 'NONE',  ( -23.75054448485400016, -15.50000000000000000, -25.53140320652400064 ) ) ;
#14141 = EDGE_CURVE ( 'NONE', #55545, #9367, #2043, .T. ) ;
#14142 = LINE ( 'NONE', #68948, #1598 ) ;
#14143 = PLANE ( 'NONE',  #5036 ) ;
#14144 = ORIENTED_EDGE ( 'NONE', *, *, #52256, .T. ) ;
#14145 = ORIENTED_EDGE ( 'NONE', *, *, #13790, .F. ) ;
#14146 = DIRECTION ( 'NONE',  ( 0.000000000000000000, 0.000000000000000000, 1.000000000000000000 ) ) ;
#14147 = EDGE_LOOP ( 'NONE', ( #55490, #21362, #1723, #57677 ) ) ;
#14148 = VERTEX_POINT ( 'NONE', #43797 ) ;
#14149 = DIRECTION ( 'NONE',  ( 0.000000000000000000, 1.000000000000000000, 0.000000000000000000 ) ) ;
#14150 = FACE_OUTER_BOUND ( 'NONE', #36246, .T. ) ;
#14151 = DIRECTION ( 'NONE',  ( 0.000000000000000000, -0.1111111111108840643, -0.9938079899999319178 ) ) ;
#14152 = EDGE_CURVE ( 'NONE', #36987, #3267, #22239, .T. ) ;
#14153 = CARTESIAN_POINT ( 'NONE',  ( 0.000000000000000000, -7.449999999999998401, -14.50000000000000000 ) ) ;
#14154 = ORIENTED_EDGE ( 'NONE', *, *, #22871, .F. ) ;
#14155 = CYLINDRICAL_SURFACE ( 'NONE', #11934, 0.1749999999999998224 ) ;
#14157 = CARTESIAN_POINT ( 'NONE',  ( 6.344579767990853547, 8.393516549646580671, 455.0000000000000568 ) ) ;
#14156 = DIRECTION ( 'NONE',  ( 0.000000000000000000, 1.000000000000000000, 0.000000000000000000 ) ) ;
#14158 = ORIENTED_EDGE ( 'NONE', *, *, #40103, .F. ) ;
#14160 = ORIENTED_EDGE ( 'NONE', *, *, #62136, .F. ) ;
#14159 = DIRECTION ( 'NONE',  ( -1.836970198721029934E-16, -1.836970198721010706E-16, 1.000000000000000000 ) ) ;
#14161 = VECTOR ( 'NONE', #1697, 1000.000000000000000 ) ;
#14162 = ORIENTED_EDGE ( 'NONE', *, *, #5131, .T. ) ;
#14163 = ORIENTED_EDGE ( 'NONE', *, *, #58630, .T. ) ;
#14164 = AXIS2_PLACEMENT_3D ( 'NONE', #6314, #27882, #49457 ) ;
#14165 = ADVANCED_FACE ( 'NONE', ( #38825 ), #34197, .F. ) ;
#14166 = CARTESIAN_POINT ( 'NONE',  ( 7.186223737882818874, -5.257023737882825287, 54.00000000000000711 ) ) ;
#14167 = EDGE_CURVE ( 'NONE', #48590, #55190, #65709, .T. ) ;
#14168 = VECTOR ( 'NONE', #27752, 1000.000000000000000 ) ;
#14169 = AXIS2_PLACEMENT_3D ( 'NONE', #50118, #44805, #12618 ) ;
#14171 = DIRECTION ( 'NONE',  ( 0.000000000000000000, -1.000000000000000000, 0.000000000000000000 ) ) ;
#14170 = VECTOR ( 'NONE', #57398, 1000.000000000000000 ) ;
#14172 = ORIENTED_EDGE ( 'NONE', *, *, #33836, .T. ) ;
#14173 = ORIENTED_EDGE ( 'NONE', *, *, #47526, .F. ) ;
#14174 = AXIS2_PLACEMENT_3D ( 'NONE', #33111, #27464, #22514 ) ;
#14175 = CIRCLE ( 'NONE', #34441, 1.224999999999999423 ) ;
#14176 = CARTESIAN_POINT ( 'NONE',  ( 283.0000000000000568, -25.60000000000000142, 17.60000000000000142 ) ) ;
#14177 = DIRECTION ( 'NONE',  ( 0.000000000000000000, 0.000000000000000000, -1.000000000000000000 ) ) ;
#14178 = EDGE_CURVE ( 'NONE', #55616, #44242, #58187, .T. ) ;
#14179 = ORIENTED_EDGE ( 'NONE', *, *, #58140, .F. ) ;
#14180 = ORIENTED_EDGE ( 'NONE', *, *, #44525, .T. ) ;
#14181 = FACE_BOUND ( 'NONE', #8872, .T. ) ;
#14182 = VECTOR ( 'NONE', #38785, 1000.000000000000114 ) ;
#14183 = SHAPE_REPRESENTATION ( 'Part2', ( #45918 ), #65174 ) ;
#14184 = CARTESIAN_POINT ( 'NONE',  ( 4.961189459950040792, 7.342976262117206332, 26.00000000000000711 ) ) ;
#14185 = VERTEX_POINT ( 'NONE', #16925 ) ;
#14186 = CIRCLE ( 'NONE', #55978, 0.3499999999998879008 ) ;
#14187 = DIRECTION ( 'NONE',  ( 0.000000000000000000, 0.000000000000000000, 1.000000000000000000 ) ) ;
#14188 = CARTESIAN_POINT ( 'NONE',  ( 15.50000000000000000, -5.000000000000000000, -19.00000000000000000 ) ) ;
#14190 = VERTEX_POINT ( 'NONE', #6651 ) ;
#14189 = FACE_OUTER_BOUND ( 'NONE', #53483, .T. ) ;
#14191 = VECTOR ( 'NONE', #49177, 1000.000000000000000 ) ;
#14192 = ORIENTED_EDGE ( 'NONE', *, *, #38108, .F. ) ;
#14193 = CARTESIAN_POINT ( 'NONE',  ( 30.00000000000000000, -14.04000000000000092, 14.80000000000000071 ) ) ;
#14194 = FACE_OUTER_BOUND ( 'NONE', #67922, .T. ) ;
#14195 = DIRECTION ( 'NONE',  ( 0.5000000000000004441, -0.8660254037844383745, 0.000000000000000000 ) ) ;
#14196 = DIRECTION ( 'NONE',  ( 1.000000000000000000, 0.000000000000000000, 0.000000000000000000 ) ) ;
#14197 = EDGE_CURVE ( 'NONE', #50347, #40313, #669, .T. ) ;
#14198 = DIRECTION ( 'NONE',  ( 1.000000000000000000, -5.981805089575194965E-17, 0.000000000000000000 ) ) ;
#14199 = DIRECTION ( 'NONE',  ( 0.000000000000000000, 0.6857142857146703019, -0.7278708115914659382 ) ) ;
#14200 = ORIENTED_EDGE ( 'NONE', *, *, #54153, .F. ) ;
#14201 = CARTESIAN_POINT ( 'NONE',  ( 4.622483450353394474, 3.593516549646586622, 455.0000000000000568 ) ) ;
#14202 = ADVANCED_FACE ( 'NONE', ( #1353 ), #38497, .F. ) ;
#14204 = ORIENTED_EDGE ( 'NONE', *, *, #46094, .F. ) ;
#14203 = DIRECTION ( 'NONE',  ( -1.000000000000000000, 1.610765207321970913E-14, 1.836970198721059516E-16 ) ) ;
#14205 = CYLINDRICAL_SURFACE ( 'NONE', #55859, 0.5000000000001357803 ) ;
#14206 = FACE_OUTER_BOUND ( 'NONE', #59409, .T. ) ;
#14207 = PRESENTATION_LAYER_ASSIGNMENT (  '', '', ( #53749 ) ) ;
#14208 = EDGE_CURVE ( 'NONE', #37440, #21386, #11597, .T. ) ;
#14209 = CARTESIAN_POINT ( 'NONE',  ( 27.90000000000000213, 0.000000000000000000, 0.000000000000000000 ) ) ;
#14210 = LINE ( 'NONE', #46382, #5516 ) ;
#14211 = ADVANCED_FACE ( 'NONE', ( #39849 ), #44468, .F. ) ;
#14212 = AXIS2_PLACEMENT_3D ( 'NONE', #14676, #68422, #58532 ) ;
#14213 = ORIENTED_EDGE ( 'NONE', *, *, #39662, .T. ) ;
#14214 = CARTESIAN_POINT ( 'NONE',  ( 7.000000000000000000, -23.70411739045900390, 12.50000000000000000 ) ) ;
#14215 = CARTESIAN_POINT ( 'NONE',  ( 1.690483450353351458, -9.841277389592704594, 195.0000000000000284 ) ) ;
#14216 = ORIENTED_EDGE ( 'NONE', *, *, #43400, .T. ) ;
#14217 = VECTOR ( 'NONE', #37373, 1000.000000000000000 ) ;
#14218 = FACE_OUTER_BOUND ( 'NONE', #9985, .T. ) ;
#14219 = EDGE_CURVE ( 'NONE', #1371, #330, #597, .T. ) ;
#14220 = AXIS2_PLACEMENT_3D ( 'NONE', #43923, #38633, #48545 ) ;
#14221 = AXIS2_PLACEMENT_3D ( 'NONE', #3773, #26396, #64577 ) ;
#14222 = CIRCLE ( 'NONE', #49217, 24.99999999998789946 ) ;
#14223 = FACE_OUTER_BOUND ( 'NONE', #40104, .T. ) ;
#14224 = ORIENTED_EDGE ( 'NONE', *, *, #13074, .T. ) ;
#14225 = DIRECTION ( 'NONE',  ( 1.836970198721029934E-16, 1.836970198721010706E-16, -1.000000000000000000 ) ) ;
#14226 = ORIENTED_EDGE ( 'NONE', *, *, #27557, .T. ) ;
#14227 = EDGE_CURVE ( 'NONE', #63302, #9904, #1021, .T. ) ;
#14228 = ORIENTED_EDGE ( 'NONE', *, *, #66657, .F. ) ;
#14229 = ADVANCED_FACE ( 'NONE', ( #22915, #61416 ), #22578, .T. ) ;
#14230 = PLANE ( 'NONE',  #8716 ) ;
#14232 = DIRECTION ( 'NONE',  ( 0.000000000000000000, 0.000000000000000000, -1.000000000000000000 ) ) ;
#14231 = AXIS2_PLACEMENT_3D ( 'NONE', #43685, #65265, #33749 ) ;
#14233 = VECTOR ( 'NONE', #1457, 1000.000000000000000 ) ;
#14234 = AXIS2_PLACEMENT_3D ( 'NONE', #66503, #8856, #61529 ) ;
#14235 = CARTESIAN_POINT ( 'NONE',  ( 7.000000000000000000, -20.40000000000000213, 12.40000000000000213 ) ) ;
#14236 = EDGE_CURVE ( 'NONE', #68170, #2518, #17606, .T. ) ;
#14237 = EDGE_CURVE ( 'NONE', #53541, #57893, #60439, .T. ) ;
#14238 = ADVANCED_FACE ( 'NONE', ( #34553 ), #33862, .T. ) ;
#14239 = AXIS2_PLACEMENT_3D ( 'NONE', #6864, #28432, #1565 ) ;
#14240 = CARTESIAN_POINT ( 'NONE',  ( 7.000000000000000000, -25.93000000000544958, -9.412893218815410634 ) ) ;
#14241 = LINE ( 'NONE', #68692, #21662 ) ;
#14242 = ORIENTED_EDGE ( 'NONE', *, *, #30535, .T. ) ;
#14243 = VERTEX_POINT ( 'NONE', #50481 ) ;
#14245 = ORIENTED_EDGE ( 'NONE', *, *, #61716, .F. ) ;
#14244 = DIRECTION ( 'NONE',  ( 0.000000000000000000, 1.000000000000000000, 0.000000000000000000 ) ) ;
#14246 = EDGE_CURVE ( 'NONE', #34313, #58981, #28555, .T. ) ;
#14247 = ORIENTED_EDGE ( 'NONE', *, *, #545, .T. ) ;
#14248 = AXIS2_PLACEMENT_3D ( 'NONE', #3675, #58488, #15333 ) ;
#14249 = DIRECTION ( 'NONE',  ( 4.336808689942043768E-15, 1.000000000000000000, 0.000000000000000000 ) ) ;
#14250 = DIRECTION ( 'NONE',  ( -0.8660254037844485886, 0.000000000000000000, -0.4999999999999827360 ) ) ;
#14251 = DIRECTION ( 'NONE',  ( -0.7671651518153105309, 0.6414496315691445849, 2.356647714346206145E-16 ) ) ;
#14252 = EDGE_CURVE ( 'NONE', #14966, #36267, #67452, .T. ) ;
#14253 = FACE_BOUND ( 'NONE', #59773, .T. ) ;
#14254 = VECTOR ( 'NONE', #12269, 1000.000000000000000 ) ;
#14255 = EDGE_CURVE ( 'NONE', #11801, #41002, #45914, .T. ) ;
#14256 = CARTESIAN_POINT ( 'NONE',  ( 11.00000000000000000, -17.50000000000000000, 60.00000000000000000 ) ) ;
#14257 = CARTESIAN_POINT ( 'NONE',  ( 10.09643294401457858, 9.293516549646566816, 455.0000000000000568 ) ) ;
#14258 = ORIENTED_EDGE ( 'NONE', *, *, #50558, .T. ) ;
#14259 = VERTEX_POINT ( 'NONE', #18640 ) ;
#14260 = VERTEX_POINT ( 'NONE', #8377 ) ;
#14261 = EDGE_LOOP ( 'NONE', ( #51194, #39236, #4739, #14036 ) ) ;
#14262 = CARTESIAN_POINT ( 'NONE',  ( 7.000000000000000000, -20.40000000000000213, -17.60000000000000142 ) ) ;
#14263 = ADVANCED_FACE ( 'NONE', ( #30663 ), #14038, .F. ) ;
#14264 = DIRECTION ( 'NONE',  ( -1.000000000000000000, 0.000000000000000000, 0.000000000000000000 ) ) ;
#14266 = ADVANCED_FACE ( 'NONE', ( #68502 ), #3444, .F. ) ;
#14265 = DIRECTION ( 'NONE',  ( 0.000000000000000000, 0.000000000000000000, 1.000000000000000000 ) ) ;
#14267 = CARTESIAN_POINT ( 'NONE',  ( -11.50000000000000000, -12.00000000000000000, -10.69999999999999929 ) ) ;
#14268 = VERTEX_POINT ( 'NONE', #24660 ) ;
#14269 = ORIENTED_EDGE ( 'NONE', *, *, #63737, .F. ) ;
#14270 = ORIENTED_EDGE ( 'NONE', *, *, #43401, .F. ) ;
#14271 = CARTESIAN_POINT ( 'NONE',  ( -7.415254214038299097, -3.006483450353353515, 195.0000000000000284 ) ) ;
#14272 = VERTEX_POINT ( 'NONE', #20054 ) ;
#14273 = ORIENTED_EDGE ( 'NONE', *, *, #2157, .F. ) ;
#14274 = CARTESIAN_POINT ( 'NONE',  ( 7.265214908726123078, -6.619341603356961201, 455.0000000000000568 ) ) ;
#14275 = ORIENTED_EDGE ( 'NONE', *, *, #56282, .T. ) ;
#14276 = VERTEX_POINT ( 'NONE', #41619 ) ;
#14277 = AXIS2_PLACEMENT_3D ( 'NONE', #26679, #21371, #42932 ) ;
#14278 = CARTESIAN_POINT ( 'NONE',  ( -7.250000000000001776, -7.249999999999998224, -13.50000000000000178 ) ) ;
#14280 = ORIENTED_EDGE ( 'NONE', *, *, #46153, .T. ) ;
#14279 = DIRECTION ( 'NONE',  ( 0.000000000000000000, 0.000000000000000000, 1.000000000000000000 ) ) ;
#14281 = ORIENTED_EDGE ( 'NONE', *, *, #26979, .T. ) ;
#14282 = CARTESIAN_POINT ( 'NONE',  ( 7.000000000000000000, -20.40000000000000213, 12.40000000000000213 ) ) ;
#14283 = AXIS2_PLACEMENT_3D ( 'NONE', #34341, #28362, #2528 ) ;
#14284 = VECTOR ( 'NONE', #7073, 1000.000000000000000 ) ;
#14285 = VECTOR ( 'NONE', #6366, 1000.000000000000000 ) ;
#14286 = ADVANCED_FACE ( 'NONE', ( #40563 ), #25011, .F. ) ;
#14287 = LINE ( 'NONE', #47502, #31840 ) ;
#14288 = DIRECTION ( 'NONE',  ( -1.000000000000000000, 0.000000000000000000, 0.000000000000000000 ) ) ;
#14290 = ORIENTED_EDGE ( 'NONE', *, *, #1156, .F. ) ;
#14289 = DIRECTION ( 'NONE',  ( 1.836970198721029934E-16, 1.836970198721010706E-16, -1.000000000000000000 ) ) ;
#14291 = ORIENTED_EDGE ( 'NONE', *, *, #19516, .T. ) ;
#14292 = VECTOR ( 'NONE', #69078, 1000.000000000000000 ) ;
#14293 = DIRECTION ( 'NONE',  ( -3.304235192336781428E-15, -1.000000000000000000, 0.000000000000000000 ) ) ;
#14294 = AXIS2_PLACEMENT_3D ( 'NONE', #24337, #55815, #61821 ) ;
#14295 = DIRECTION ( 'NONE',  ( 0.000000000000000000, 0.000000000000000000, -1.000000000000000000 ) ) ;
#14296 = DIRECTION ( 'NONE',  ( -1.047444401652940007E-14, -1.000000000000000000, -1.836970198721029934E-16 ) ) ;
#14297 = CARTESIAN_POINT ( 'NONE',  ( 9.703773737882814387, 8.566576262117184370, 54.00000000000000711 ) ) ;
#14298 = VECTOR ( 'NONE', #32557, 1000.000000000000000 ) ;
#14299 = ORIENTED_EDGE ( 'NONE', *, *, #2533, .F. ) ;
#14300 = LINE ( 'NONE', #31280, #19064 ) ;
#14301 = ADVANCED_FACE ( 'NONE', ( #23951 ), #19001, .T. ) ;
#14302 = VECTOR ( 'NONE', #19578, 1000.000000000000000 ) ;
#14303 = CARTESIAN_POINT ( 'NONE',  ( 275.0000000000000000, -20.40000000000000213, -17.60000000000000142 ) ) ;
#14304 = DIRECTION ( 'NONE',  ( 1.000000000000000000, 0.000000000000000000, 0.000000000000000000 ) ) ;
#14305 = ORIENTED_EDGE ( 'NONE', *, *, #59327, .F. ) ;
#14307 = EDGE_CURVE ( 'NONE', #44568, #44075, #57877, .T. ) ;
#14306 = CARTESIAN_POINT ( 'NONE',  ( 283.0000000000000568, -20.40000000000000213, -12.40000000000000213 ) ) ;
#14308 = FACE_OUTER_BOUND ( 'NONE', #19177, .T. ) ;
#14309 = DIRECTION ( 'NONE',  ( -1.000000000000000000, 0.000000000000000000, 0.000000000000000000 ) ) ;
#14310 = ADVANCED_FACE ( 'NONE', ( #3788 ), #25361, .F. ) ;
#14311 = ORIENTED_EDGE ( 'NONE', *, *, #17808, .F. ) ;
#14312 = CARTESIAN_POINT ( 'NONE',  ( -2.752095193409461071, -9.955011587777271131, 195.0000000000000284 ) ) ;
#14313 = EDGE_CURVE ( 'NONE', #32701, #16734, #57528, .T. ) ;
#14314 = FACE_OUTER_BOUND ( 'NONE', #52292, .T. ) ;
#14315 = DIRECTION ( 'NONE',  ( -0.000000000000000000, -0.000000000000000000, 1.000000000000000000 ) ) ;
#14316 = VERTEX_POINT ( 'NONE', #61787 ) ;
#14317 = FACE_OUTER_BOUND ( 'NONE', #46578, .T. ) ;
#14318 = DIRECTION ( 'NONE',  ( 1.836970198721029934E-16, 1.836970198721010706E-16, -1.000000000000000000 ) ) ;
#14319 = PRESENTATION_LAYER_ASSIGNMENT (  '', '', ( #51559 ) ) ;
#14320 = LINE ( 'NONE', #56738, #20643 ) ;
#14321 = DIRECTION ( 'NONE',  ( 0.000000000000000000, -1.000000000000000000, 0.000000000000000000 ) ) ;
#14322 = DIRECTION ( 'NONE',  ( 0.8660254037844363761, -0.5000000000000038858, -1.836970198721044232E-16 ) ) ;
#14323 = ORIENTED_EDGE ( 'NONE', *, *, #13850, .T. ) ;
#14324 = CARTESIAN_POINT ( 'NONE',  ( 70.47321854994621049, 47.95351654967443977, 40.00000000000000000 ) ) ;
#14325 = FACE_OUTER_BOUND ( 'NONE', #45221, .T. ) ;
#14326 = LINE ( 'NONE', #7610, #10836 ) ;
#14327 = EDGE_CURVE ( 'NONE', #59333, #1005, #13346, .T. ) ;
#14328 = VECTOR ( 'NONE', #55507, 1000.000000000000000 ) ;
#14329 = VECTOR ( 'NONE', #68904, 1000.000000000000000 ) ;
#14330 = DIRECTION ( 'NONE',  ( 1.000000000000000000, -0.000000000000000000, -0.000000000000000000 ) ) ;
#14331 = DIRECTION ( 'NONE',  ( 0.000000000000000000, 0.7071067811865474617, 0.7071067811865474617 ) ) ;
#14332 = ORIENTED_EDGE ( 'NONE', *, *, #64381, .T. ) ;
#14334 = ORIENTED_EDGE ( 'NONE', *, *, #59723, .F. ) ;
#14333 = CARTESIAN_POINT ( 'NONE',  ( -8.452095193409485674, -7.757955312929543545, 455.0000000000000568 ) ) ;
#14335 = CIRCLE ( 'NONE', #3024, 0.2000000000005226763 ) ;
#14336 = AXIS2_PLACEMENT_3D ( 'NONE', #7727, #18333, #66082 ) ;
#14337 = DIRECTION ( 'NONE',  ( 0.000000000000000000, -1.000000000000000000, 0.000000000000000000 ) ) ;
#14338 = LINE ( 'NONE', #30249, #67364 ) ;
#14339 = DIRECTION ( 'NONE',  ( 1.000000000000000000, 0.000000000000000000, 0.000000000000000000 ) ) ;
#14340 = ORIENTED_EDGE ( 'NONE', *, *, #15323, .F. ) ;
#14341 = CIRCLE ( 'NONE', #66266, 3.500000000000000000 ) ;
#14342 = DIRECTION ( 'NONE',  ( 0.000000000000000000, 0.000000000000000000, -1.000000000000000000 ) ) ;
#14343 = ORIENTED_EDGE ( 'NONE', *, *, #32827, .T. ) ;
#14344 = AXIS2_PLACEMENT_3D ( 'NONE', #21844, #47327, #5251 ) ;
#14345 = ORIENTED_EDGE ( 'NONE', *, *, #64781, .T. ) ;
#14346 = EDGE_LOOP ( 'NONE', ( #42724, #36184, #26823, #31652 ) ) ;
#14347 = LINE ( 'NONE', #23893, #25124 ) ;
#14348 = EDGE_CURVE ( 'NONE', #10806, #34214, #41259, .T. ) ;
#14349 = CARTESIAN_POINT ( 'NONE',  ( 9.562023737882764607, 2.355476262117153663, 54.00000000000000711 ) ) ;
#14350 = LINE ( 'NONE', #40853, #22452 ) ;
#14352 = EDGE_CURVE ( 'NONE', #9482, #15805, #35652, .T. ) ;
#14351 = FACE_OUTER_BOUND ( 'NONE', #38769, .T. ) ;
#14353 = VECTOR ( 'NONE', #68375, 1000.000000000000114 ) ;
#14354 = EDGE_LOOP ( 'NONE', ( #64393, #26836 ) ) ;
#14356 = EDGE_CURVE ( 'NONE', #69700, #51833, #63895, .T. ) ;
#14355 = ORIENTED_EDGE ( 'NONE', *, *, #33705, .F. ) ;
#14357 = CARTESIAN_POINT ( 'NONE',  ( -11.00000000000000000, -12.00000000000000000, -12.20000000000000107 ) ) ;
#14358 = DIRECTION ( 'NONE',  ( 0.000000000000000000, 1.000000000000000000, 0.000000000000000000 ) ) ;
#14359 = ORIENTED_EDGE ( 'NONE', *, *, #24633, .T. ) ;
#14360 = ORIENTED_EDGE ( 'NONE', *, *, #17660, .T. ) ;
#14361 = ORIENTED_EDGE ( 'NONE', *, *, #48744, .F. ) ;
#14362 = ORIENTED_EDGE ( 'NONE', *, *, #67780, .T. ) ;
#14363 = DIRECTION ( 'NONE',  ( 0.000000000000000000, 0.000000000000000000, -1.000000000000000000 ) ) ;
#14365 = ORIENTED_EDGE ( 'NONE', *, *, #50731, .F. ) ;
#14364 = DIRECTION ( 'NONE',  ( -1.000000000000000000, 0.000000000000000000, 0.000000000000000000 ) ) ;
#14366 = CARTESIAN_POINT ( 'NONE',  ( 11.25000000000000178, 11.18999999999999950, -5.000000000000000000 ) ) ;
#14367 = DIRECTION ( 'NONE',  ( -0.7071067811865527908, -0.7071067811865422437, 0.000000000000000000 ) ) ;
#14368 = ORIENTED_EDGE ( 'NONE', *, *, #64536, .F. ) ;
#14369 = ORIENTED_EDGE ( 'NONE', *, *, #53600, .F. ) ;
#14370 = CARTESIAN_POINT ( 'NONE',  ( -8.250000000000001776, -8.249999999999998224, -26.00000000000001066 ) ) ;
#14371 = AXIS2_PLACEMENT_3D ( 'NONE', #24648, #14736, #40896 ) ;
#14372 = AXIS2_PLACEMENT_3D ( 'NONE', #49843, #34256, #23657 ) ;
#14373 = CARTESIAN_POINT ( 'NONE',  ( 7.250000000000005329, -7.249999999999998224, -20.00000000000000000 ) ) ;
#14374 = AXIS2_PLACEMENT_3D ( 'NONE', #3009, #35882, #8997 ) ;
#14375 = ADVANCED_FACE ( 'NONE', ( #56477 ), #62838, .F. ) ;
#14376 = VECTOR ( 'NONE', #59932, 1000.000000000000000 ) ;
#14377 = DIRECTION ( 'NONE',  ( -0.000000000000000000, 0.000000000000000000, 1.000000000000000000 ) ) ;
#14378 = AXIS2_PLACEMENT_3D ( 'NONE', #45106, #18233, #6928 ) ;
#14379 = DIRECTION ( 'NONE',  ( -1.000000000000000000, 0.000000000000000000, 0.000000000000000000 ) ) ;
#14380 = ORIENTED_EDGE ( 'NONE', *, *, #19426, .T. ) ;
#14381 = LINE ( 'NONE', #63526, #55891 ) ;
#14383 = EDGE_CURVE ( 'NONE', #59069, #42153, #41261, .T. ) ;
#14382 = DIRECTION ( 'NONE',  ( 0.000000000000000000, -0.7046037717859445770, 0.7096009616573392131 ) ) ;
#14384 = VECTOR ( 'NONE', #20167, 1000.000000000000000 ) ;
#14385 = PLANE ( 'NONE',  #45434 ) ;
#14386 = CARTESIAN_POINT ( 'NONE',  ( -11.99351654964671354, 7.813516549646603693, 455.0000000000000568 ) ) ;
#14387 = EDGE_CURVE ( 'NONE', #14943, #15805, #31385, .T. ) ;
#14388 = EDGE_CURVE ( 'NONE', #21817, #44081, #48328, .T. ) ;
#14389 = CARTESIAN_POINT ( 'NONE',  ( 41.09999999999999432, -14.06939075806901940, -20.80000000000000426 ) ) ;
#14391 = ORIENTED_EDGE ( 'NONE', *, *, #32593, .T. ) ;
#14390 = ADVANCED_FACE ( 'NONE', ( #53296 ), #25724, .T. ) ;
#14392 = DIRECTION ( 'NONE',  ( 0.000000000000000000, 0.000000000000000000, -1.000000000000000000 ) ) ;
#14393 = EDGE_CURVE ( 'NONE', #47898, #65081, #59277, .T. ) ;
#14394 = CARTESIAN_POINT ( 'NONE',  ( 27.00000000000000000, 3.010794155703768650E-16, 2.458500000000000796 ) ) ;
#14395 = CARTESIAN_POINT ( 'NONE',  ( -25.50000000000000355, -5.578999999999999737, 24.12099999999999511 ) ) ;
#14396 = CARTESIAN_POINT ( 'NONE',  ( -25.50000000000000355, -5.200000000000001066, 22.50000000000000000 ) ) ;
#14397 = CIRCLE ( 'NONE', #29022, 0.5000000000000000000 ) ;
#14398 = ADVANCED_FACE ( 'NONE', ( #20401 ), #41969, .T. ) ;
#14399 = CARTESIAN_POINT ( 'NONE',  ( -29.50000000000000355, -12.00000000000000000, -11.03137303340310282 ) ) ;
#14400 = CARTESIAN_POINT ( 'NONE',  ( 15.00000000000000000, -42.00000000000000000, 26.50000000000000000 ) ) ;
#14401 = FACE_OUTER_BOUND ( 'NONE', #59122, .T. ) ;
#14402 = DIRECTION ( 'NONE',  ( 1.000000000000000000, 0.000000000000000000, 0.000000000000000000 ) ) ;
#14403 = ORIENTED_EDGE ( 'NONE', *, *, #44870, .F. ) ;
#14404 = PLANE ( 'NONE',  #14062 ) ;
#14405 = CARTESIAN_POINT ( 'NONE',  ( 283.0000000000000568, -23.29603921945599865, 12.50000000000000000 ) ) ;
#14406 = VERTEX_POINT ( 'NONE', #4501 ) ;
#14407 = PLANE ( 'NONE',  #45877 ) ;
#14408 = CARTESIAN_POINT ( 'NONE',  ( 5.257023737882801306, 5.242976262117200470, 54.00000000000000711 ) ) ;
#14409 = DIRECTION ( 'NONE',  ( -0.8660254037844363761, 0.5000000000000038858, -0.000000000000000000 ) ) ;
#14410 = DIRECTION ( 'NONE',  ( 0.000000000000000000, 0.000000000000000000, -1.000000000000000000 ) ) ;
#14411 = VERTEX_POINT ( 'NONE', #5195 ) ;
#14412 = CARTESIAN_POINT ( 'NONE',  ( 5.257023737882801306, 5.242976262117200470, 54.00000000000000711 ) ) ;
#14413 = ORIENTED_EDGE ( 'NONE', *, *, #5875, .T. ) ;
#14414 = LINE ( 'NONE', #24316, #42838 ) ;
#14415 = CARTESIAN_POINT ( 'NONE',  ( 1.866219381641426533, -9.417013320880776917, 195.0000000000000284 ) ) ;
#14416 = VECTOR ( 'NONE', #6811, 1000.000000000000000 ) ;
#14417 = ORIENTED_EDGE ( 'NONE', *, *, #46608, .F. ) ;
#14418 = DIRECTION ( 'NONE',  ( 0.000000000000000000, -0.7071067811865496822, -0.7071067811865454633 ) ) ;
#14419 = CARTESIAN_POINT ( 'NONE',  ( 24.00000000000000000, -15.50000000000000000, 14.50000000000000000 ) ) ;
#14420 = ORIENTED_EDGE ( 'NONE', *, *, #53513, .T. ) ;
#14421 = CIRCLE ( 'NONE', #23449, 2.458500000000000796 ) ;
#14422 = CIRCLE ( 'NONE', #36999, 1.000000000000000000 ) ;
#14423 = LINE ( 'NONE', #63913, #51478 ) ;
#14424 = ORIENTED_EDGE ( 'NONE', *, *, #3754, .F. ) ;
#14425 = ORIENTED_EDGE ( 'NONE', *, *, #45326, .T. ) ;
#14426 = CARTESIAN_POINT ( 'NONE',  ( 4.747751991980625696, -5.393625297350043368, 455.0000000000000568 ) ) ;
#14427 = ORIENTED_EDGE ( 'NONE', *, *, #7285, .F. ) ;
#14428 = VERTEX_POINT ( 'NONE', #52591 ) ;
#14429 = CIRCLE ( 'NONE', #9901, 0.3499999999999996447 ) ;
#14430 = VECTOR ( 'NONE', #66535, 1000.000000000000000 ) ;
#14431 = CARTESIAN_POINT ( 'NONE',  ( -11.00000000000000000, -13.79999999999979998, 17.64999999999988844 ) ) ;
#14433 = ADVANCED_FACE ( 'NONE', ( #26071 ), #42667, .T. ) ;
#14432 = DIRECTION ( 'NONE',  ( -1.000000000000000000, 0.000000000000000000, 0.000000000000000000 ) ) ;
#14434 = CARTESIAN_POINT ( 'NONE',  ( 275.0000000000000000, -21.00000000000000000, -12.50000000000000000 ) ) ;
#14435 = VECTOR ( 'NONE', #11323, 1000.000000000000000 ) ;
#14436 = ORIENTED_EDGE ( 'NONE', *, *, #10969, .F. ) ;
#14437 = ADVANCED_FACE ( 'NONE', ( #42314 ), #26763, .T. ) ;
#14438 = CARTESIAN_POINT ( 'NONE',  ( -2.893516549646828473, -10.92648345035345514, 455.0000000000000568 ) ) ;
#14439 = EDGE_CURVE ( 'NONE', #66152, #52010, #37906, .T. ) ;
#14440 = AXIS2_PLACEMENT_3D ( 'NONE', #44984, #13858, #2544 ) ;
#14441 = VECTOR ( 'NONE', #64959, 1000.000000000000000 ) ;
#14443 = PLANE ( 'NONE',  #69455 ) ;
#14442 = FACE_OUTER_BOUND ( 'NONE', #66496, .T. ) ;
#14444 = ORIENTED_EDGE ( 'NONE', *, *, #5254, .T. ) ;
#14446 = ORIENTED_EDGE ( 'NONE', *, *, #43607, .T. ) ;
#14445 = DIRECTION ( 'NONE',  ( 1.000000000000000000, -7.304098846218132892E-15, -2.683482381803073952E-30 ) ) ;
#14447 = ORIENTED_EDGE ( 'NONE', *, *, #27982, .F. ) ;
#14448 = EDGE_CURVE ( 'NONE', #29117, #44931, #69543, .T. ) ;
#14449 = DIRECTION ( 'NONE',  ( 1.000000000000000000, -0.000000000000000000, -0.000000000000000000 ) ) ;
#14451 = ORIENTED_EDGE ( 'NONE', *, *, #31637, .F. ) ;
#14450 = DIRECTION ( 'NONE',  ( -1.000000000000000000, 0.000000000000000000, 0.000000000000000000 ) ) ;
#14452 = AXIS2_PLACEMENT_3D ( 'NONE', #27430, #37695, #17160 ) ;
#14453 = CARTESIAN_POINT ( 'NONE',  ( -7.450000000000001954, 7.250000000000000000, -20.50000000000000000 ) ) ;
#14454 = PLANE ( 'NONE',  #40694 ) ;
#14455 = EDGE_LOOP ( 'NONE', ( #43373, #8423, #4713, #62315 ) ) ;
#14456 = ORIENTED_EDGE ( 'NONE', *, *, #3089, .T. ) ;
#14457 = DIRECTION ( 'NONE',  ( -0.000000000000000000, -0.000000000000000000, -1.000000000000000000 ) ) ;
#14458 = ORIENTED_EDGE ( 'NONE', *, *, #56249, .F. ) ;
#14459 = DIRECTION ( 'NONE',  ( 1.000000000000000000, 0.000000000000000000, 0.000000000000000000 ) ) ;
#14460 = CARTESIAN_POINT ( 'NONE',  ( 7.250000000000004441, 7.450000000000001954, -8.500000000000000000 ) ) ;
#14461 = CARTESIAN_POINT ( 'NONE',  ( -7.450000000000001954, -7.249999999999998224, -13.00000000000000178 ) ) ;
#14462 = ORIENTED_EDGE ( 'NONE', *, *, #49090, .T. ) ;
#14463 = CARTESIAN_POINT ( 'NONE',  ( 8.711985858128693749, -2.420780051175170478, 26.00000000000000711 ) ) ;
#14464 = CARTESIAN_POINT ( 'NONE',  ( 0.000000000000000000, 0.000000000000000000, -16.00000000000000000 ) ) ;
#14465 = VECTOR ( 'NONE', #17701, 1000.000000000000000 ) ;
#14467 = ORIENTED_EDGE ( 'NONE', *, *, #13063, .F. ) ;
#14466 = PRESENTATION_STYLE_ASSIGNMENT (( #14814 ) ) ;
#14469 = EDGE_LOOP ( 'NONE', ( #29180, #22375, #4614, #54037, #19234, #2335, #55858, #29162, #25032, #1318, #3750, #47366, #2590, #8961, #61178, #21812, #57229, #13022, #53493, #61918, #58444, #63381, #42948, #19083, #6360, #13622, #52640, #27366, #1281, #61411, #62296, #18077, #11428, #57955, #3907, #43646, #52370, #36360, #68429, #4182, #53457, #4785, #45288, #23081, #35906, #30957, #28238, #22961, #22591, #63515, #45594, #66309, #51555, #16430, #37388, #57051, #55269, #59538, #39035, #63940, #53119, #44967, #51615, #31360, #6021, #66567, #57705, #8457, #59571, #37257, #42075, #59387, #32876, #50169, #22609, #28832, #18740, #55304, #21762, #62487, #27999, #37081, #17197, #42546, #38125, #32532, #61626, #24915, #19046, #12551, #32823, #29463, #8676, #66677, #43931, #11708, #66342, #5412, #5284, #64124, #45299, #53434, #19652, #55833, #40230, #35134, #62459, #36981, #52009, #28359, #35790, #499, #45770, #9034, #63131, #10625, #21347, #13810, #26301, #56706, #69919, #63751, #4930, #69945, #25728, #5690, #58185, #8575, #65462, #52786, #55999, #31421, #4572, #47015, #16334, #54397, #46403, #65243, #57304, #38109, #13880, #66629, #20339, #65680, #59709, #12279, #64552, #1853, #35127, #50742, #28500, #4195, #57308, #31984, #49572, #11150, #53237, #68508, #50467, #24434, #27747, #3542, #18438, #32039, #26471, #46396, #54479, #40924, #14269, #23269, #7716, #6818, #54958, #60452, #57238, #2799, #242, #54705, #45216, #37092, #37298, #16875, #40126, #3276, #59176, #28100, #35429, #67456, #29495, #11971, #67208, #54490, #18465, #28702, #46168, #8925, #15588, #56538, #15178, #48798, #39807, #18165, #55010, #56584, #49653, #68217, #47370, #33269, #22650, #24202, #22676, #69843, #19480, #49990 ) ) ;
#14468 = LINE ( 'NONE', #24008, #39948 ) ;
#14470 = PLANE ( 'NONE',  #10311 ) ;
#14471 = CARTESIAN_POINT ( 'NONE',  ( 7.450000000000006395, 7.250000000000000888, -20.00000000000000000 ) ) ;
#14472 = CARTESIAN_POINT ( 'NONE',  ( 28.90000000000000213, -21.00000000000001421, -13.86939075806900945 ) ) ;
#14473 = CARTESIAN_POINT ( 'NONE',  ( -3.142976262117251451, 6.486996718459839606, 54.00000000000000711 ) ) ;
#14474 = CARTESIAN_POINT ( 'NONE',  ( 33.89999999999999858, 13.66939075806899240, 20.79999999999999361 ) ) ;
#14475 = ORIENTED_EDGE ( 'NONE', *, *, #30616, .T. ) ;
#14476 = FACE_OUTER_BOUND ( 'NONE', #23008, .T. ) ;
#14477 = EDGE_CURVE ( 'NONE', #596, #63351, #15462, .T. ) ;
#14478 = CARTESIAN_POINT ( 'NONE',  ( 289.2330000000000041, 0.000000000000000000, 0.000000000000000000 ) ) ;
#14479 =( NAMED_UNIT ( * ) SI_UNIT ( $, .STERADIAN. ) SOLID_ANGLE_UNIT ( ) );
#14480 = AXIS2_PLACEMENT_3D ( 'NONE', #47371, #26507, #69653 ) ;
#14482 = EDGE_LOOP ( 'NONE', ( #65484, #12233, #62603, #38975 ) ) ;
#14481 = DIRECTION ( 'NONE',  ( 0.000000000000000000, 0.000000000000000000, 1.000000000000000000 ) ) ;
#14483 = LINE ( 'NONE', #46644, #60636 ) ;
#14484 = EDGE_CURVE ( 'NONE', #58198, #1953, #59344, .T. ) ;
#14485 = PLANE ( 'NONE',  #20594 ) ;
#14486 = VECTOR ( 'NONE', #34938, 1000.000000000000000 ) ;
#14487 = ORIENTED_EDGE ( 'NONE', *, *, #14742, .T. ) ;
#14488 = CARTESIAN_POINT ( 'NONE',  ( -7.250000000000000888, 7.250000000000001776, -26.00000000000001066 ) ) ;
#14489 = DIRECTION ( 'NONE',  ( -0.4999999999999755196, 0.8660254037844526964, 2.509347957447861534E-16 ) ) ;
#14490 = VERTEX_POINT ( 'NONE', #43354 ) ;
#14491 = CARTESIAN_POINT ( 'NONE',  ( 8.900000000000002132, -18.00000000000000355, 21.00000000000000000 ) ) ;
#14492 = CARTESIAN_POINT ( 'NONE',  ( 15.00000000000000000, -25.60000000000000142, 17.60000000000000142 ) ) ;
#14493 = LINE ( 'NONE', #24747, #34947 ) ;
#14494 = EDGE_CURVE ( 'NONE', #9143, #49824, #236, .T. ) ;
#14495 = CIRCLE ( 'NONE', #68664, 0.6000000000000006439 ) ;
#14496 = CARTESIAN_POINT ( 'NONE',  ( -11.00000000000000000, -9.487228132326899654, 12.50000000000000000 ) ) ;
#14497 = ORIENTED_EDGE ( 'NONE', *, *, #66042, .T. ) ;
#14498 = LINE ( 'NONE', #51976, #19229 ) ;
#14499 = EDGE_LOOP ( 'NONE', ( #47694, #49786, #49107, #4644 ) ) ;
#14500 = CARTESIAN_POINT ( 'NONE',  ( -7.250000000000000888, 7.250000000000001776, -10.50000000000000000 ) ) ;
#14501 = ORIENTED_EDGE ( 'NONE', *, *, #26754, .F. ) ;
#14502 = DIRECTION ( 'NONE',  ( -1.000000000000000000, 0.000000000000000000, 0.000000000000000000 ) ) ;
#14503 = CARTESIAN_POINT ( 'NONE',  ( 13.00000000000000178, -16.28999999999999915, -14.50000000000000000 ) ) ;
#14504 = LINE ( 'NONE', #46668, #27643 ) ;
#14505 = ORIENTED_EDGE ( 'NONE', *, *, #16011, .T. ) ;
#14506 = ORIENTED_EDGE ( 'NONE', *, *, #18107, .T. ) ;
#14507 = FACE_OUTER_BOUND ( 'NONE', #17735, .T. ) ;
#14508 = ORIENTED_EDGE ( 'NONE', *, *, #29057, .F. ) ;
#14509 = VERTEX_POINT ( 'NONE', #63548 ) ;
#14510 = LINE ( 'NONE', #41374, #50746 ) ;
#14511 = DIRECTION ( 'NONE',  ( 1.000000000000000000, 2.135044278125301343E-15, -0.000000000000000000 ) ) ;
#14512 = DIRECTION ( 'NONE',  ( 1.836970198721029934E-16, 1.836970198721010706E-16, -1.000000000000000000 ) ) ;
#14513 = VERTEX_POINT ( 'NONE', #15105 ) ;
#14514 = CARTESIAN_POINT ( 'NONE',  ( 283.0000000000000568, -20.50000000000000000, 17.00000000000000000 ) ) ;
#14516 = DIRECTION ( 'NONE',  ( 0.8660254037844383745, 0.5000000000000004441, -0.000000000000000000 ) ) ;
#14515 = DIRECTION ( 'NONE',  ( 1.000000000000000000, 0.000000000000000000, 0.000000000000000000 ) ) ;
#14517 = ORIENTED_EDGE ( 'NONE', *, *, #20290, .T. ) ;
#14519 = EDGE_LOOP ( 'NONE', ( #60985, #43817, #58441, #60067 ) ) ;
#14518 = DIRECTION ( 'NONE',  ( -0.000000000000000000, -0.000000000000000000, -1.000000000000000000 ) ) ;
#14520 = EDGE_LOOP ( 'NONE', ( #4338, #34062, #47298, #15387, #55149, #9853, #28215, #59700 ) ) ;
#14521 = EDGE_CURVE ( 'NONE', #47155, #26513, #11922, .T. ) ;
#14522 = DIRECTION ( 'NONE',  ( 0.000000000000000000, 0.7071067811865474617, -0.7071067811865474617 ) ) ;
#14523 = CIRCLE ( 'NONE', #31503, 0.2000000000000005107 ) ;
#14524 = PLANE ( 'NONE',  #64338 ) ;
#14525 = EDGE_LOOP ( 'NONE', ( #66547, #37289, #45653, #7520 ) ) ;
#14526 = EDGE_LOOP ( 'NONE', ( #40088, #40278, #65874, #32208 ) ) ;
#14527 = CIRCLE ( 'NONE', #23551, 0.6000000000000006439 ) ;
#14528 = ADVANCED_FACE ( 'NONE', ( #32418 ), #58592, .T. ) ;
#14529 = CARTESIAN_POINT ( 'NONE',  ( 7.250000000000005329, -7.249999999999998224, -13.50000000000000178 ) ) ;
#14530 = PLANE ( 'NONE',  #35657 ) ;
#14531 = ORIENTED_EDGE ( 'NONE', *, *, #61585, .T. ) ;
#14532 = VERTEX_POINT ( 'NONE', #15796 ) ;
#14533 = CARTESIAN_POINT ( 'NONE',  ( 32.89999999999999858, 3.010794155703768650E-16, -2.458500000000000796 ) ) ;
#14534 = ADVANCED_FACE ( 'NONE', ( #58934 ), #10489, .F. ) ;
#14535 = CARTESIAN_POINT ( 'NONE',  ( 7.000000000000000000, -26.50000000000000000, -9.080000000000000071 ) ) ;
#14536 = ORIENTED_EDGE ( 'NONE', *, *, #37882, .F. ) ;
#14537 = VECTOR ( 'NONE', #44627, 1000.000000000000000 ) ;
#14538 = LINE ( 'NONE', #15248, #67368 ) ;
#14539 = CARTESIAN_POINT ( 'NONE',  ( 11.90000000000000036, -21.00000000000001421, -13.86939075806900945 ) ) ;
#14541 = ORIENTED_EDGE ( 'NONE', *, *, #12725, .T. ) ;
#14540 = CARTESIAN_POINT ( 'NONE',  ( 7.250000000000005329, 7.250000000000000888, -10.50000000000000000 ) ) ;
#14542 = ORIENTED_EDGE ( 'NONE', *, *, #52068, .T. ) ;
#14543 = PLANE ( 'NONE',  #7257 ) ;
#14544 = CARTESIAN_POINT ( 'NONE',  ( 28.00000000000000000, -16.28999999999710369, -14.50000000000000000 ) ) ;
#14545 = DIRECTION ( 'NONE',  ( 1.000000000000000000, -0.000000000000000000, 0.000000000000000000 ) ) ;
#14546 = DIRECTION ( 'NONE',  ( 0.000000000000000000, 1.000000000000000000, 0.000000000000000000 ) ) ;
#14547 = CARTESIAN_POINT ( 'NONE',  ( 41.09999999999999432, 20.60000000000000142, 13.86939075806900057 ) ) ;
#14548 = CARTESIAN_POINT ( 'NONE',  ( 7.969523737882818537, -9.737023737882820384, 54.00000000000000711 ) ) ;
#14549 = ORIENTED_EDGE ( 'NONE', *, *, #26124, .T. ) ;
#14550 = CARTESIAN_POINT ( 'NONE',  ( -2.530476262117233865, 8.821682069070682530, 54.00000000000000711 ) ) ;
#14551 = EDGE_CURVE ( 'NONE', #20459, #60747, #22500, .T. ) ;
#14553 = ORIENTED_EDGE ( 'NONE', *, *, #62355, .F. ) ;
#14552 = CARTESIAN_POINT ( 'NONE',  ( 8.250000000000005329, -7.249999999999998224, -9.000000000000001776 ) ) ;
#14554 = CARTESIAN_POINT ( 'NONE',  ( 11.18999999999999950, -11.18999999999999950, -5.000000000000000000 ) ) ;
#14555 = CARTESIAN_POINT ( 'NONE',  ( 41.09999999999999432, 14.08845687959340331, -21.00000000000000000 ) ) ;
#14556 = EDGE_CURVE ( 'NONE', #829, #15613, #55367, .T. ) ;
#14557 = EDGE_CURVE ( 'NONE', #67314, #69920, #5887, .T. ) ;
#14558 = DIRECTION ( 'NONE',  ( 1.011922027653139155E-14, 1.000000000000000000, 0.000000000000000000 ) ) ;
#14559 = EDGE_CURVE ( 'NONE', #49881, #69042, #49382, .T. ) ;
#14560 = ORIENTED_EDGE ( 'NONE', *, *, #57067, .F. ) ;
#14561 = DIRECTION ( 'NONE',  ( 0.000000000000000000, 0.000000000000000000, -1.000000000000000000 ) ) ;
#14562 = DIRECTION ( 'NONE',  ( 0.000000000000000000, -0.000000000000000000, 1.000000000000000000 ) ) ;
#14563 = VERTEX_POINT ( 'NONE', #28471 ) ;
#14564 = EDGE_CURVE ( 'NONE', #40478, #50332, #12212, .T. ) ;
#14565 = VECTOR ( 'NONE', #13633, 1000.000000000000000 ) ;
#14566 = FACE_OUTER_BOUND ( 'NONE', #59847, .T. ) ;
#14567 = CARTESIAN_POINT ( 'NONE',  ( 29.89999999999999858, 13.66939075806899240, 20.79999999999999361 ) ) ;
#14568 = EDGE_CURVE ( 'NONE', #18679, #22860, #60306, .T. ) ;
#14569 = ADVANCED_FACE ( 'NONE', ( #45081 ), #946, .T. ) ;
#14570 = AXIS2_PLACEMENT_3D ( 'NONE', #37916, #28670, #23375 ) ;
#14571 = DIRECTION ( 'NONE',  ( 1.000000000000000000, 0.000000000000000000, 0.000000000000000000 ) ) ;
#14572 = ORIENTED_EDGE ( 'NONE', *, *, #27902, .T. ) ;
#14573 = CARTESIAN_POINT ( 'NONE',  ( -5.993516549646728642, -6.006483450353378828, 195.0000000000000284 ) ) ;
#14574 = ORIENTED_EDGE ( 'NONE', *, *, #9346, .T. ) ;
#14575 = ORIENTED_EDGE ( 'NONE', *, *, #3486, .T. ) ;
#14576 = AXIS2_PLACEMENT_3D ( 'NONE', #42563, #32652, #15344 ) ;
#14577 = LINE ( 'NONE', #37553, #15562 ) ;
#14578 = DIRECTION ( 'NONE',  ( 1.000000000000000000, 0.000000000000000000, 0.000000000000000000 ) ) ;
#14579 = LINE ( 'NONE', #30493, #58182 ) ;
#14580 = CIRCLE ( 'NONE', #67679, 25.39999999999999858 ) ;
#14581 = DIRECTION ( 'NONE',  ( 0.000000000000000000, 0.000000000000000000, -1.000000000000000000 ) ) ;
#14582 = CARTESIAN_POINT ( 'NONE',  ( -7.393516549646710345, 5.993516549646603409, 455.0000000000000568 ) ) ;
#14583 = VERTEX_POINT ( 'NONE', #65956 ) ;
#14584 = EDGE_LOOP ( 'NONE', ( #28093, #67191, #28794, #47838, #28017, #56989, #57716, #28423 ) ) ;
#14586 = VERTEX_POINT ( 'NONE', #50044 ) ;
#14585 = DIRECTION ( 'NONE',  ( 0.000000000000000000, -3.673940397442059868E-16, 1.000000000000000000 ) ) ;
#14587 = ORIENTED_EDGE ( 'NONE', *, *, #48476, .T. ) ;
#14589 = AXIS2_PLACEMENT_3D ( 'NONE', #34862, #30286, #29209 ) ;
#14588 = CIRCLE ( 'NONE', #63143, 4.000000000000000000 ) ;
#14590 = FACE_OUTER_BOUND ( 'NONE', #46846, .T. ) ;
#14591 = CARTESIAN_POINT ( 'NONE',  ( -30.00000000000000000, -5.599999999999999645, 27.00000000000000000 ) ) ;
#14592 = DIRECTION ( 'NONE',  ( -1.000000000000000000, 0.000000000000000000, 0.000000000000000000 ) ) ;
#14593 = ADVANCED_FACE ( 'NONE', ( #17875 ), #581, .F. ) ;
#14594 = DIRECTION ( 'NONE',  ( 0.000000000000000000, 0.000000000000000000, 1.000000000000000000 ) ) ;
#14595 = DIRECTION ( 'NONE',  ( 0.5000000000000129896, 0.8660254037844311581, 0.000000000000000000 ) ) ;
#14596 = VECTOR ( 'NONE', #42474, 1000.000000000000000 ) ;
#14597 = CARTESIAN_POINT ( 'NONE',  ( 73.77321854994620765, 47.95351654967443977, 15.00000000000000000 ) ) ;
#14598 = ORIENTED_EDGE ( 'NONE', *, *, #57260, .F. ) ;
#14599 = ORIENTED_EDGE ( 'NONE', *, *, #4982, .F. ) ;
#14600 = ORIENTED_EDGE ( 'NONE', *, *, #20759, .T. ) ;
#14601 = EDGE_CURVE ( 'NONE', #33973, #49824, #32750, .T. ) ;
#14602 = VERTEX_POINT ( 'NONE', #11515 ) ;
#14603 = CARTESIAN_POINT ( 'NONE',  ( -6.651770455163739548, 7.342976262117183239, 54.00000000000000711 ) ) ;
#14604 = LINE ( 'NONE', #35818, #27607 ) ;
#14605 =( NAMED_UNIT ( * ) SI_UNIT ( $, .STERADIAN. ) SOLID_ANGLE_UNIT ( ) );
#14606 = CARTESIAN_POINT ( 'NONE',  ( 7.000000000000000000, -32.44999999999905071, -14.49999999999906031 ) ) ;
#14607 = EDGE_LOOP ( 'NONE', ( #12479, #9765, #41396, #60716 ) ) ;
#14608 = EDGE_LOOP ( 'NONE', ( #6347, #59142, #12155 ) ) ;
#14609 = ORIENTED_EDGE ( 'NONE', *, *, #8713, .T. ) ;
#14610 = CARTESIAN_POINT ( 'NONE',  ( -7.250000000000000000, -7.449999999999998401, -11.50000000000000000 ) ) ;
#14611 = ORIENTED_EDGE ( 'NONE', *, *, #55739, .T. ) ;
#14612 = ORIENTED_EDGE ( 'NONE', *, *, #24319, .F. ) ;
#14613 = LINE ( 'NONE', #20266, #62722 ) ;
#14614 = ORIENTED_EDGE ( 'NONE', *, *, #1238, .T. ) ;
#14615 = VECTOR ( 'NONE', #23471, 1000.000000000000000 ) ;
#14616 = ORIENTED_EDGE ( 'NONE', *, *, #24120, .F. ) ;
#14617 = DIRECTION ( 'NONE',  ( 0.000000000000000000, 0.000000000000000000, 1.000000000000000000 ) ) ;
#14618 = EDGE_CURVE ( 'NONE', #6963, #17758, #13031, .T. ) ;
#14620 = ORIENTED_EDGE ( 'NONE', *, *, #33890, .T. ) ;
#14619 = CARTESIAN_POINT ( 'NONE',  ( -7.750000000000001776, -7.348062532927999158, 0.000000000000000000 ) ) ;
#14621 = VECTOR ( 'NONE', #69554, 1000.000000000000000 ) ;
#14622 = ORIENTED_EDGE ( 'NONE', *, *, #60722, .F. ) ;
#14623 = VECTOR ( 'NONE', #32170, 1000.000000000000000 ) ;
#14624 = DIRECTION ( 'NONE',  ( -0.000000000000000000, -0.000000000000000000, -1.000000000000000000 ) ) ;
#14625 = CARTESIAN_POINT ( 'NONE',  ( 12.00648345035336284, 7.813516549646607245, 195.0000000000000284 ) ) ;
#14626 = EDGE_CURVE ( 'NONE', #54865, #57591, #44730, .T. ) ;
#14628 = ORIENTED_EDGE ( 'NONE', *, *, #47434, .F. ) ;
#14627 = LINE ( 'NONE', #25954, #68507 ) ;
#14629 = EDGE_CURVE ( 'NONE', #20614, #51641, #31148, .T. ) ;
#14630 = EDGE_LOOP ( 'NONE', ( #69922, #31996, #37487, #3835 ) ) ;
#14631 = VECTOR ( 'NONE', #31186, 1000.000000000000000 ) ;
#14632 = CYLINDRICAL_SURFACE ( 'NONE', #60552, 0.5000000000000000000 ) ;
#14633 = EDGE_CURVE ( 'NONE', #69920, #40971, #38410, .T. ) ;
#14634 = DIRECTION ( 'NONE',  ( 0.000000000000000000, 1.000000000000000000, 0.000000000000000000 ) ) ;
#14635 = ADVANCED_FACE ( 'NONE', ( #55036 ), #60666, .F. ) ;
#14636 = EDGE_CURVE ( 'NONE', #29083, #67623, #9693, .T. ) ;
#14637 = CARTESIAN_POINT ( 'NONE',  ( 3.006483450353369502, -7.428221114744997244, 195.0000000000000284 ) ) ;
#14638 = AXIS2_PLACEMENT_3D ( 'NONE', #36048, #29689, #19777 ) ;
#14639 = DIRECTION ( 'NONE',  ( 1.000000000000000000, -0.000000000000000000, 0.000000000000000000 ) ) ;
#14640 = EDGE_LOOP ( 'NONE', ( #60533, #29649, #68232, #26240 ) ) ;
#14641 = CARTESIAN_POINT ( 'NONE',  ( 8.250000000000005329, 0.000000000000000000, -8.500000000000000000 ) ) ;
#14642 = EDGE_CURVE ( 'NONE', #28515, #55190, #17178, .T. ) ;
#14643 = CARTESIAN_POINT ( 'NONE',  ( -11.11351654964666835, -2.906483450353287257, 195.0000000000000284 ) ) ;
#14644 = EDGE_CURVE ( 'NONE', #36079, #63788, #23237, .T. ) ;
#14645 = ORIENTED_EDGE ( 'NONE', *, *, #11180, .T. ) ;
#14646 = CARTESIAN_POINT ( 'NONE',  ( 29.50000000000000355, -11.50000000000100009, -15.00000000000084910 ) ) ;
#14647 = EDGE_CURVE ( 'NONE', #44331, #65063, #12554, .T. ) ;
#14648 = DIRECTION ( 'NONE',  ( 1.000000000000000000, -0.000000000000000000, 0.000000000000000000 ) ) ;
#14649 = VECTOR ( 'NONE', #7578, 1000.000000000000000 ) ;
#14650 = CARTESIAN_POINT ( 'NONE',  ( 0.000000000000000000, -8.249999999999998224, -16.50000000000000000 ) ) ;
#14651 = ORIENTED_EDGE ( 'NONE', *, *, #65102, .F. ) ;
#14652 = EDGE_CURVE ( 'NONE', #38222, #66537, #13613, .T. ) ;
#14653 = CARTESIAN_POINT ( 'NONE',  ( 9.804883450353454322, 10.19191654964656912, 455.0000000000000568 ) ) ;
#14654 = EDGE_CURVE ( 'NONE', #63930, #28581, #6292, .T. ) ;
#14655 = CARTESIAN_POINT ( 'NONE',  ( -30.00000000000000000, -12.00000000000000000, -11.03137303340310282 ) ) ;
#14656 = ORIENTED_EDGE ( 'NONE', *, *, #47569, .F. ) ;
#14657 = VECTOR ( 'NONE', #67741, 1000.000000000000000 ) ;
#14658 = DIRECTION ( 'NONE',  ( 0.000000000000000000, 0.000000000000000000, 1.000000000000000000 ) ) ;
#14659 = LINE ( 'NONE', #30571, #46761 ) ;
#14660 = CARTESIAN_POINT ( 'NONE',  ( 6.006483450353401921, 5.993516549646582092, 455.0000000000000568 ) ) ;
#14661 = CARTESIAN_POINT ( 'NONE',  ( 0.000000000000000000, 0.000000000000000000, -11.00000000000000000 ) ) ;
#14662 = CARTESIAN_POINT ( 'NONE',  ( -7.450000000000001954, 7.250000000000000000, -20.50000000000000000 ) ) ;
#14663 = VERTEX_POINT ( 'NONE', #39773 ) ;
#14664 = DIRECTION ( 'NONE',  ( 0.000000000000000000, -0.000000000000000000, -1.000000000000000000 ) ) ;
#14665 = DIRECTION ( 'NONE',  ( 8.339399738404099512E-15, 1.000000000000000000, 1.836970198721025990E-16 ) ) ;
#14666 = ADVANCED_FACE ( 'NONE', ( #19611 ), #18564, .F. ) ;
#14667 = CARTESIAN_POINT ( 'NONE',  ( -15.50000000000000000, -0.4000000000005236034, 19.20000000000052509 ) ) ;
#14668 = FACE_OUTER_BOUND ( 'NONE', #33696, .T. ) ;
#14669 = ORIENTED_EDGE ( 'NONE', *, *, #23119, .F. ) ;
#14670 = VECTOR ( 'NONE', #13968, 1000.000000000000000 ) ;
#14672 = ORIENTED_EDGE ( 'NONE', *, *, #11345, .T. ) ;
#14671 = CARTESIAN_POINT ( 'NONE',  ( 283.0000000000000568, -37.15000000000001279, 7.700000000000000178 ) ) ;
#14673 = AXIS2_PLACEMENT_3D ( 'NONE', #39874, #13005, #56843 ) ;
#14674 = AXIS2_PLACEMENT_3D ( 'NONE', #44462, #38494, #60734 ) ;
#14675 = FACE_OUTER_BOUND ( 'NONE', #20236, .T. ) ;
#14676 = CARTESIAN_POINT ( 'NONE',  ( 283.0000000000000568, -38.65000000000095781, 14.49999999999903899 ) ) ;
#14677 = DIRECTION ( 'NONE',  ( 0.000000000000000000, 0.000000000000000000, -1.000000000000000000 ) ) ;
#14678 = VERTEX_POINT ( 'NONE', #3712 ) ;
#14679 = AXIS2_PLACEMENT_3D ( 'NONE', #69624, #10218, #59348 ) ;
#14680 =( NAMED_UNIT ( * ) PLANE_ANGLE_UNIT ( ) SI_UNIT ( $, .RADIAN. ) );
#14681 = CARTESIAN_POINT ( 'NONE',  ( 280.0000000000000000, -20.40000000000000213, -16.00000000000000711 ) ) ;
#14682 = ORIENTED_EDGE ( 'NONE', *, *, #12865, .F. ) ;
#14683 = VERTEX_POINT ( 'NONE', #56745 ) ;
#14684 = AXIS2_PLACEMENT_3D ( 'NONE', #48065, #53382, #10577 ) ;
#14685 = EDGE_CURVE ( 'NONE', #40434, #56856, #29525, .T. ) ;
#14686 = ORIENTED_EDGE ( 'NONE', *, *, #28893, .T. ) ;
#14687 = FACE_OUTER_BOUND ( 'NONE', #43795, .T. ) ;
#14688 = VECTOR ( 'NONE', #29827, 1000.000000000000000 ) ;
#14689 = CARTESIAN_POINT ( 'NONE',  ( 30.00000000000000000, -5.000000000000000000, 27.00000000000000000 ) ) ;
#14690 = CIRCLE ( 'NONE', #54229, 1.399999999999998579 ) ;
#14691 = ADVANCED_FACE ( 'NONE', ( #30241 ), #50738, .F. ) ;
#14692 = CARTESIAN_POINT ( 'NONE',  ( 8.750000000000003553, 7.750000000000000000, 0.000000000000000000 ) ) ;
#14693 = ORIENTED_EDGE ( 'NONE', *, *, #8481, .T. ) ;
#14694 = VERTEX_POINT ( 'NONE', #24584 ) ;
#14695 = EDGE_CURVE ( 'NONE', #40478, #4544, #2906, .T. ) ;
#14696 = CARTESIAN_POINT ( 'NONE',  ( 16.75000000000000000, -0.2038245569916320166, 21.77831216351300014 ) ) ;
#14698 = DIRECTION ( 'NONE',  ( 0.8660254037844485886, 0.000000000000000000, -0.4999999999999827360 ) ) ;
#14697 = AXIS2_PLACEMENT_3D ( 'NONE', #34011, #23421, #12106 ) ;
#14699 = VECTOR ( 'NONE', #36260, 1000.000000000000000 ) ;
#14700 = ORIENTED_EDGE ( 'NONE', *, *, #52760, .T. ) ;
#14701 = EDGE_CURVE ( 'NONE', #15085, #19699, #9002, .T. ) ;
#14702 = ORIENTED_EDGE ( 'NONE', *, *, #67947, .F. ) ;
#14703 = VERTEX_POINT ( 'NONE', #68061 ) ;
#14704 = ORIENTED_EDGE ( 'NONE', *, *, #27795, .F. ) ;
#14705 = DIRECTION ( 'NONE',  ( 0.000000000000000000, 0.000000000000000000, 1.000000000000000000 ) ) ;
#14706 = UNCERTAINTY_MEASURE_WITH_UNIT (LENGTH_MEASURE( 1.000000000000000082E-05 ), #68, 'distance_accuracy_value', 'NONE');
#14707 = ADVANCED_FACE ( 'NONE', ( #23875 ), #24925, .T. ) ;
#14709 = ORIENTED_EDGE ( 'NONE', *, *, #41596, .T. ) ;
#14708 = CARTESIAN_POINT ( 'NONE',  ( 4.206483450353341702, -11.32648345035347504, 455.0000000000000568 ) ) ;
#14710 = DIRECTION ( 'NONE',  ( 0.7071067811865514585, 0.7071067811865435759, -0.000000000000000000 ) ) ;
#14711 = CARTESIAN_POINT ( 'NONE',  ( 6.789561617636943325, -7.408280051175168524, 26.00000000000000000 ) ) ;
#14712 = VECTOR ( 'NONE', #13732, 1000.000000000000000 ) ;
#14713 = ORIENTED_EDGE ( 'NONE', *, *, #60023, .T. ) ;
#14714 = VERTEX_POINT ( 'NONE', #8298 ) ;
#14715 = EDGE_CURVE ( 'NONE', #38637, #13897, #24228, .T. ) ;
#14716 = EDGE_CURVE ( 'NONE', #17555, #15458, #50349, .T. ) ;
#14717 = EDGE_CURVE ( 'NONE', #62442, #44065, #14326, .T. ) ;
#14718 = CARTESIAN_POINT ( 'NONE',  ( 7.250000000000005329, 7.250000000000000888, -24.00000000000000000 ) ) ;
#14719 = DIRECTION ( 'NONE',  ( -1.000000000000000000, 0.000000000000000000, 0.000000000000000000 ) ) ;
#14720 = AXIS2_PLACEMENT_3D ( 'NONE', #62613, #8875, #24797 ) ;
#14721 = EDGE_LOOP ( 'NONE', ( #50189, #34148, #66462, #5893 ) ) ;
#14722 = ADVANCED_FACE ( 'NONE', ( #29171 ), #35889, .T. ) ;
#14723 = VECTOR ( 'NONE', #12553, 1000.000000000000000 ) ;
#14724 = PLANE ( 'NONE',  #59392 ) ;
#14725 = DIRECTION ( 'NONE',  ( -0.000000000000000000, 3.673940397442059868E-16, -1.000000000000000000 ) ) ;
#14726 = FILL_AREA_STYLE_COLOUR ( '', #41235 ) ;
#14727 = ORIENTED_EDGE ( 'NONE', *, *, #2413, .T. ) ;
#14728 = CARTESIAN_POINT ( 'NONE',  ( 5.552858015815566262, 7.342976262117203667, 26.00000000000000711 ) ) ;
#14730 = DIRECTION ( 'NONE',  ( 1.000000000000000000, -0.000000000000000000, 0.000000000000000000 ) ) ;
#14729 = VECTOR ( 'NONE', #1260, 1000.000000000000000 ) ;
#14731 = DIRECTION ( 'NONE',  ( 0.6785983445458467767, 0.6785983445458462215, -0.2810846377148228381 ) ) ;
#14732 = LINE ( 'NONE', #24989, #3143 ) ;
#14733 = CIRCLE ( 'NONE', #7899, 0.1749999999999980738 ) ;
#14734 = CARTESIAN_POINT ( 'NONE',  ( 8.900000000000002132, 21.00000000000000000, -18.00000000000000355 ) ) ;
#14735 = ORIENTED_EDGE ( 'NONE', *, *, #21587, .F. ) ;
#14736 = DIRECTION ( 'NONE',  ( 1.836970198721029934E-16, 1.836970198721010706E-16, -1.000000000000000000 ) ) ;
#14738 = AXIS2_PLACEMENT_3D ( 'NONE', #6777, #44261, #49580 ) ;
#14737 = DIRECTION ( 'NONE',  ( -1.000000000000000000, 0.000000000000000000, 0.000000000000000000 ) ) ;
#14739 = EDGE_CURVE ( 'NONE', #7353, #35907, #8661, .T. ) ;
#14740 = DIRECTION ( 'NONE',  ( 0.000000000000000000, 0.000000000000000000, -1.000000000000000000 ) ) ;
#14741 = CARTESIAN_POINT ( 'NONE',  ( -11.00000000000000000, -14.04000000000000092, -17.04524521594300523 ) ) ;
#14742 = EDGE_CURVE ( 'NONE', #36372, #38001, #43599, .T. ) ;
#14743 = CARTESIAN_POINT ( 'NONE',  ( 49.00000000000000000, -0.2000000000089119934, 8.909539772616881237E-12 ) ) ;
#14744 = DIRECTION ( 'NONE',  ( 0.000000000000000000, 1.000000000000000000, 0.000000000000000000 ) ) ;
#14745 = VECTOR ( 'NONE', #15957, 1000.000000000000000 ) ;
#14746 = FACE_OUTER_BOUND ( 'NONE', #17681, .T. ) ;
#14747 = VECTOR ( 'NONE', #12165, 1000.000000000000000 ) ;
#14748 = LINE ( 'NONE', #52219, #8181 ) ;
#14749 = ORIENTED_EDGE ( 'NONE', *, *, #45261, .F. ) ;
#14750 = CARTESIAN_POINT ( 'NONE',  ( 275.5000000000001137, -42.00000000000004263, -26.99999999999991829 ) ) ;
#14751 = CARTESIAN_POINT ( 'NONE',  ( 7.450000000000004619, -1.336933437520057563E-15, -9.500000000000001776 ) ) ;
#14752 = VERTEX_POINT ( 'NONE', #67365 ) ;
#14753 = DIRECTION ( 'NONE',  ( 0.000000000000000000, -0.000000000000000000, 1.000000000000000000 ) ) ;
#14754 = DIRECTION ( 'NONE',  ( 0.000000000000000000, 0.000000000000000000, 1.000000000000000000 ) ) ;
#14755 = CARTESIAN_POINT ( 'NONE',  ( -11.00000000000000000, -14.04000000000000092, 14.80000000000000071 ) ) ;
#14756 =( NAMED_UNIT ( * ) PLANE_ANGLE_UNIT ( ) SI_UNIT ( $, .RADIAN. ) );
#14757 = CARTESIAN_POINT ( 'NONE',  ( -6.822336235477484578, -6.364920264886849921, 26.00000000000000711 ) ) ;
#14758 = ORIENTED_EDGE ( 'NONE', *, *, #58761, .F. ) ;
#14759 = ORIENTED_EDGE ( 'NONE', *, *, #60399, .F. ) ;
#14760 = CARTESIAN_POINT ( 'NONE',  ( -7.450000000000001954, 0.000000000000000000, -16.50000000000000000 ) ) ;
#14761 = CIRCLE ( 'NONE', #55437, 0.5250000000000003553 ) ;
#14762 = DIRECTION ( 'NONE',  ( 0.000000000000000000, 0.000000000000000000, -1.000000000000000000 ) ) ;
#14763 = ORIENTED_EDGE ( 'NONE', *, *, #28192, .T. ) ;
#14764 = DIRECTION ( 'NONE',  ( -0.7071067811865472397, -0.5000000000000002220, 0.5000000000000002220 ) ) ;
#14765 = DIRECTION ( 'NONE',  ( -1.836970198721029934E-16, 1.836970198721036590E-16, -1.000000000000000000 ) ) ;
#14766 = ORIENTED_EDGE ( 'NONE', *, *, #58383, .T. ) ;
#14767 = DIRECTION ( 'NONE',  ( -1.836970198721029934E-16, 1.836970198721036590E-16, -1.000000000000000000 ) ) ;
#14768 = ORIENTED_EDGE ( 'NONE', *, *, #47551, .T. ) ;
#14769 = EDGE_LOOP ( 'NONE', ( #63130, #57081, #63630, #30762 ) ) ;
#14770 = DIRECTION ( 'NONE',  ( -0.000000000000000000, -0.000000000000000000, -1.000000000000000000 ) ) ;
#14771 = AXIS2_PLACEMENT_3D ( 'NONE', #45929, #67140, #62179 ) ;
#14772 = ORIENTED_EDGE ( 'NONE', *, *, #48481, .T. ) ;
#14773 = ORIENTED_EDGE ( 'NONE', *, *, #36236, .F. ) ;
#14774 = EDGE_CURVE ( 'NONE', #58038, #48042, #13264, .T. ) ;
#14775 = LINE ( 'NONE', #15820, #45128 ) ;
#14776 = CARTESIAN_POINT ( 'NONE',  ( -8.250000000000001776, 7.250000000000000888, -25.50000000000000355 ) ) ;
#14778 = CARTESIAN_POINT ( 'NONE',  ( -10.73351654964668533, -1.090483450353341155, 455.0000000000000568 ) ) ;
#14777 = VECTOR ( 'NONE', #38218, 1000.000000000000000 ) ;
#14779 = ORIENTED_EDGE ( 'NONE', *, *, #27692, .F. ) ;
#14781 = EDGE_CURVE ( 'NONE', #62375, #54885, #51514, .T. ) ;
#14780 = AXIS2_PLACEMENT_3D ( 'NONE', #758, #54839, #22659 ) ;
#14782 = DIRECTION ( 'NONE',  ( -0.000000000000000000, -0.000000000000000000, -1.000000000000000000 ) ) ;
#14784 = CYLINDRICAL_SURFACE ( 'NONE', #55915, 3.499999999999853895 ) ;
#14783 = DIRECTION ( 'NONE',  ( -0.000000000000000000, 1.000000000000000000, -0.000000000000000000 ) ) ;
#14785 = EDGE_LOOP ( 'NONE', ( #69795, #50182, #55279, #29530 ) ) ;
#14787 = VERTEX_POINT ( 'NONE', #57098 ) ;
#14786 = LINE ( 'NONE', #36345, #36526 ) ;
#14788 = EDGE_CURVE ( 'NONE', #64, #52369, #7437, .T. ) ;
#14789 = VERTEX_POINT ( 'NONE', #69818 ) ;
#14790 = EDGE_CURVE ( 'NONE', #21838, #30889, #59403, .T. ) ;
#14791 = VECTOR ( 'NONE', #68771, 1000.000000000000114 ) ;
#14792 = VECTOR ( 'NONE', #45887, 1000.000000000000000 ) ;
#14793 = EDGE_CURVE ( 'NONE', #20570, #20601, #27798, .T. ) ;
#14794 = EDGE_CURVE ( 'NONE', #67236, #28, #9743, .T. ) ;
#14795 = CARTESIAN_POINT ( 'NONE',  ( 8.211283450353379365, -6.006483450353490738, 455.0000000000000568 ) ) ;
#14797 = VERTEX_POINT ( 'NONE', #36228 ) ;
#14796 = LINE ( 'NONE', #15501, #50030 ) ;
#14798 = AXIS2_PLACEMENT_3D ( 'NONE', #34746, #28743, #12139 ) ;
#14799 = DIRECTION ( 'NONE',  ( -0.000000000000000000, -0.000000000000000000, -1.000000000000000000 ) ) ;
#14800 = EDGE_CURVE ( 'NONE', #52916, #55613, #20662, .T. ) ;
#14801 = PLANE ( 'NONE',  #9155 ) ;
#14802 = ORIENTED_EDGE ( 'NONE', *, *, #18733, .F. ) ;
#14803 = ORIENTED_EDGE ( 'NONE', *, *, #64572, .T. ) ;
#14804 = AXIS2_PLACEMENT_3D ( 'NONE', #38141, #49768, #1334 ) ;
#14805 = DIRECTION ( 'NONE',  ( -1.000000000000000000, 0.000000000000000000, 0.000000000000000000 ) ) ;
#14806 = VERTEX_POINT ( 'NONE', #30932 ) ;
#14807 = DIRECTION ( 'NONE',  ( -1.000000000000000000, 0.000000000000000000, 0.000000000000000000 ) ) ;
#14808 = DIRECTION ( 'NONE',  ( 0.000000000000000000, -0.7071067811865474617, -0.7071067811865474617 ) ) ;
#14809 = DIRECTION ( 'NONE',  ( 0.000000000000000000, 0.000000000000000000, 1.000000000000000000 ) ) ;
#14810 = VERTEX_POINT ( 'NONE', #15376 ) ;
#14811 = DIRECTION ( 'NONE',  ( -1.000000000000000000, 0.000000000000000000, 0.000000000000000000 ) ) ;
#14812 = AXIS2_PLACEMENT_3D ( 'NONE', #36354, #10189, #64288 ) ;
#14813 = LINE ( 'NONE', #9504, #35978 ) ;
#14815 = VERTEX_POINT ( 'NONE', #52873 ) ;
#14814 = SURFACE_STYLE_USAGE ( .BOTH. , #30372 ) ;
#14817 = ORIENTED_EDGE ( 'NONE', *, *, #24545, .F. ) ;
#14816 = CARTESIAN_POINT ( 'NONE',  ( -8.598420958951683346, 1.991476262117183316, 54.00000000000000711 ) ) ;
#14818 = LINE ( 'NONE', #10550, #59170 ) ;
#14819 = CARTESIAN_POINT ( 'NONE',  ( -10.49297626211726175, 6.835476262117182955, 54.00000000000000711 ) ) ;
#14820 = DIRECTION ( 'NONE',  ( -8.612436249475772606E-15, -1.000000000000000000, -1.836970198721020566E-16 ) ) ;
#14821 = DIRECTION ( 'NONE',  ( 0.000000000000000000, 1.000000000000000000, 0.000000000000000000 ) ) ;
#14822 = CARTESIAN_POINT ( 'NONE',  ( -8.250000000000001776, -7.249999999999998224, -12.50000000000000000 ) ) ;
#14823 = VERTEX_POINT ( 'NONE', #69461 ) ;
#14824 = DIRECTION ( 'NONE',  ( 0.000000000000000000, 0.000000000000000000, -1.000000000000000000 ) ) ;
#14825 = DIRECTION ( 'NONE',  ( 1.047444401652940007E-14, 1.000000000000000000, 1.836970198721029934E-16 ) ) ;
#14826 = VECTOR ( 'NONE', #18797, 1000.000000000000114 ) ;
#14827 =( NAMED_UNIT ( * ) PLANE_ANGLE_UNIT ( ) SI_UNIT ( $, .RADIAN. ) );
#14829 = ORIENTED_EDGE ( 'NONE', *, *, #59154, .T. ) ;
#14828 = CARTESIAN_POINT ( 'NONE',  ( 9.690000000000001279, -9.690000000000001279, -5.000000000000000000 ) ) ;
#14830 = ADVANCED_FACE ( 'NONE', ( #25988 ), #37641, .F. ) ;
#14831 = CIRCLE ( 'NONE', #11432, 0.5000000000001362244 ) ;
#14832 = PLANE ( 'NONE',  #68578 ) ;
#14833 = ADVANCED_FACE ( 'NONE', ( #63108 ), #42586, .T. ) ;
#14834 = DIRECTION ( 'NONE',  ( -0.6414496315691484707, 0.7671651518153074223, 2.309356642088893343E-17 ) ) ;
#14835 = VECTOR ( 'NONE', #60044, 1000.000000000000000 ) ;
#14836 = CARTESIAN_POINT ( 'NONE',  ( 34.89999999999999858, 13.66939075806899240, -20.79999999999999361 ) ) ;
#14837 = VERTEX_POINT ( 'NONE', #63461 ) ;
#14838 = DIRECTION ( 'NONE',  ( -0.000000000000000000, -0.000000000000000000, -1.000000000000000000 ) ) ;
#14839 = DIRECTION ( 'NONE',  ( 1.000000000000000000, 0.000000000000000000, 0.000000000000000000 ) ) ;
#14841 = VERTEX_POINT ( 'NONE', #9364 ) ;
#14840 = EDGE_CURVE ( 'NONE', #23983, #427, #47546, .T. ) ;
#14842 = FACE_OUTER_BOUND ( 'NONE', #33458, .T. ) ;
#14844 = EDGE_CURVE ( 'NONE', #43562, #64155, #32333, .T. ) ;
#14843 = AXIS2_PLACEMENT_3D ( 'NONE', #13177, #60918, #2574 ) ;
#14845 = VECTOR ( 'NONE', #3729, 1000.000000000000000 ) ;
#14846 = CARTESIAN_POINT ( 'NONE',  ( -7.250000000000000888, 7.450000000000003730, -21.00000000000000000 ) ) ;
#14847 = LINE ( 'NONE', #4248, #16291 ) ;
#14848 = LINE ( 'NONE', #25812, #2209 ) ;
#14849 = CARTESIAN_POINT ( 'NONE',  ( -11.31351654964669429, -4.206483450353285747, 195.0000000000000284 ) ) ;
#14850 = ORIENTED_EDGE ( 'NONE', *, *, #46148, .F. ) ;
#14851 = CARTESIAN_POINT ( 'NONE',  ( 277.3542486889354564, -25.50000000000000355, 17.00000000000000000 ) ) ;
#14852 = ORIENTED_EDGE ( 'NONE', *, *, #55487, .T. ) ;
#14853 = LINE ( 'NONE', #6323, #67978 ) ;
#14854 = EDGE_LOOP ( 'NONE', ( #66415, #64987, #61117, #24936 ) ) ;
#14855 = VERTEX_POINT ( 'NONE', #31991 ) ;
#14856 = PLANE ( 'NONE',  #40412 ) ;
#14857 = AXIS2_PLACEMENT_3D ( 'NONE', #35412, #3962, #19163 ) ;
#14858 = DIRECTION ( 'NONE',  ( 1.000000000000000000, 0.000000000000000000, 0.000000000000000000 ) ) ;
#14859 = CARTESIAN_POINT ( 'NONE',  ( -7.250000000000000888, 7.250000000000001776, -11.50000000000000000 ) ) ;
#14860 = ORIENTED_EDGE ( 'NONE', *, *, #37957, .F. ) ;
#14861 = VERTEX_POINT ( 'NONE', #42232 ) ;
#14862 = LINE ( 'NONE', #35345, #52136 ) ;
#14863 = ORIENTED_EDGE ( 'NONE', *, *, #55375, .T. ) ;
#14864 = VERTEX_POINT ( 'NONE', #4768 ) ;
#14865 = EDGE_CURVE ( 'NONE', #62405, #22621, #41542, .T. ) ;
#14866 = CARTESIAN_POINT ( 'NONE',  ( -9.781776262117247711, 9.781776262117171328, 54.00000000000000711 ) ) ;
#14867 = PLANE ( 'NONE',  #41492 ) ;
#14868 = CARTESIAN_POINT ( 'NONE',  ( 11.78648345035337996, 4.173516549646518747, 455.0000000000000568 ) ) ;
#14869 = VECTOR ( 'NONE', #20362, 1000.000000000000000 ) ;
#14870 = ORIENTED_EDGE ( 'NONE', *, *, #50771, .F. ) ;
#14871 = CARTESIAN_POINT ( 'NONE',  ( -25.50000000000000355, -5.578999999999999737, -22.50000000000000000 ) ) ;
#14873 = FACE_OUTER_BOUND ( 'NONE', #14968, .T. ) ;
#14872 = CARTESIAN_POINT ( 'NONE',  ( -3.842976262117329345, -9.912023737882817542, 54.00000000000000711 ) ) ;
#14874 = ORIENTED_EDGE ( 'NONE', *, *, #39823, .F. ) ;
#14876 = ORIENTED_EDGE ( 'NONE', *, *, #43802, .F. ) ;
#14875 = CARTESIAN_POINT ( 'NONE',  ( 157.4206970127263787, -35.25383818724483831, 0.000000000000000000 ) ) ;
#14877 = VERTEX_POINT ( 'NONE', #63813 ) ;
#14878 = ADVANCED_FACE ( 'NONE', ( #36577 ), #31645, .F. ) ;
#14879 = EDGE_CURVE ( 'NONE', #16920, #7564, #52504, .T. ) ;
#14880 = CARTESIAN_POINT ( 'NONE',  ( 4.456444791733522252E-16, 7.450000000000002842, -16.50000000000000000 ) ) ;
#14881 = CIRCLE ( 'NONE', #26191, 0.1749999999999980738 ) ;
#14882 = LINE ( 'NONE', #42447, #32683 ) ;
#14883 =( GEOMETRIC_REPRESENTATION_CONTEXT ( 3 ) GLOBAL_UNCERTAINTY_ASSIGNED_CONTEXT ( ( #58553 ) ) GLOBAL_UNIT_ASSIGNED_CONTEXT ( ( #39233, #60449, #7044 ) ) REPRESENTATION_CONTEXT ( 'NONE', 'WORKASPACE' ) );
#14884 = EDGE_CURVE ( 'NONE', #51374, #33533, #10416, .T. ) ;
#14885 = ORIENTED_EDGE ( 'NONE', *, *, #23883, .T. ) ;
#14886 = VERTEX_POINT ( 'NONE', #16071 ) ;
#14887 = DIRECTION ( 'NONE',  ( 1.000000000000000000, 0.000000000000000000, 0.000000000000000000 ) ) ;
#14888 = PLANE ( 'NONE',  #62777 ) ;
#14889 = ORIENTED_EDGE ( 'NONE', *, *, #62178, .T. ) ;
#14890 = AXIS2_PLACEMENT_3D ( 'NONE', #37907, #11703, #58779 ) ;
#14891 = CLOSED_SHELL ( 'NONE', ( #58479, #12250, #9536, #59911, #24618, #35601 ) ) ;
#14892 = ORIENTED_EDGE ( 'NONE', *, *, #18270, .F. ) ;
#14893 = LINE ( 'NONE', #58727, #30857 ) ;
#14894 = CARTESIAN_POINT ( 'NONE',  ( -25.50000000000000355, 0.000000000000000000, -20.24999999999999645 ) ) ;
#14895 = ORIENTED_EDGE ( 'NONE', *, *, #39271, .F. ) ;
#14896 = VECTOR ( 'NONE', #2489, 1000.000000000000000 ) ;
#14897 = CYLINDRICAL_SURFACE ( 'NONE', #47026, 1.224999999999999423 ) ;
#14898 = CARTESIAN_POINT ( 'NONE',  ( -7.250000000000000888, 8.250000000000001776, -18.50000000000000000 ) ) ;
#14900 = EDGE_LOOP ( 'NONE', ( #6809, #63288, #30938, #61077 ) ) ;
#14899 = FILL_AREA_STYLE ('',( #53092 ) ) ;
#14902 = ORIENTED_EDGE ( 'NONE', *, *, #41935, .F. ) ;
#14901 = FACE_OUTER_BOUND ( 'NONE', #26033, .T. ) ;
#14904 = CARTESIAN_POINT ( 'NONE',  ( 15.50000000000000000, -1.037157890325000054, 19.00000000000000000 ) ) ;
#14903 = AXIS2_PLACEMENT_3D ( 'NONE', #59095, #63714, #47784 ) ;
#14905 = DIRECTION ( 'NONE',  ( -1.000000000000000000, 0.000000000000000000, 0.000000000000000000 ) ) ;
#14906 = FACE_BOUND ( 'NONE', #1666, .T. ) ;
#14907 = FACE_OUTER_BOUND ( 'NONE', #16530, .T. ) ;
#14908 = CARTESIAN_POINT ( 'NONE',  ( -7.250000000000000000, -7.449999999999998401, -25.50000000000000355 ) ) ;
#14909 = DIRECTION ( 'NONE',  ( 1.000000000000000000, -5.626525616968433909E-15, -1.836970198721040534E-16 ) ) ;
#14910 = VERTEX_POINT ( 'NONE', #59202 ) ;
#14911 = CARTESIAN_POINT ( 'NONE',  ( 275.0000000000000000, -23.65000000000000568, 12.40000000000000213 ) ) ;
#14912 = ADVANCED_BREP_SHAPE_REPRESENTATION ( '', ( #44296, #45918 ), #52770 ) ;
#14914 = VERTEX_POINT ( 'NONE', #48592 ) ;
#14913 = DIRECTION ( 'NONE',  ( 0.000000000000000000, 0.000000000000000000, 1.000000000000000000 ) ) ;
#14915 = DIRECTION ( 'NONE',  ( 0.000000000000000000, 0.7071067811865474617, 0.7071067811865474617 ) ) ;
#14916 = CARTESIAN_POINT ( 'NONE',  ( 25.90000000000000213, -0.2000000000089119934, 8.909539772616881237E-12 ) ) ;
#14917 = CIRCLE ( 'NONE', #66822, 5.000000000000004441 ) ;
#14918 = LINE ( 'NONE', #36847, #24035 ) ;
#14919 = EDGE_CURVE ( 'NONE', #21874, #64942, #39096, .T. ) ;
#14920 = CARTESIAN_POINT ( 'NONE',  ( -28.00000000000000000, -15.50000000000000000, -20.05051025721700242 ) ) ;
#14921 = EDGE_CURVE ( 'NONE', #14787, #1760, #23294, .T. ) ;
#14922 = ADVANCED_FACE ( 'NONE', ( #22421 ), #38674, .F. ) ;
#14923 = VERTEX_POINT ( 'NONE', #5810 ) ;
#14924 = CARTESIAN_POINT ( 'NONE',  ( -8.250000000000001776, 7.250000000000000888, -11.50000000000000000 ) ) ;
#14925 = CARTESIAN_POINT ( 'NONE',  ( -8.750000000000001776, 7.250000000000000000, -26.00000000000001066 ) ) ;
#14927 = VERTEX_POINT ( 'NONE', #12132 ) ;
#14926 = EDGE_CURVE ( 'NONE', #5249, #8722, #65213, .T. ) ;
#14928 = DIRECTION ( 'NONE',  ( 0.6414496315691645689, 0.7671651518152939886, 0.000000000000000000 ) ) ;
#14929 = FACE_OUTER_BOUND ( 'NONE', #35207, .T. ) ;
#14930 = VECTOR ( 'NONE', #25076, 1000.000000000000000 ) ;
#14931 = CARTESIAN_POINT ( 'NONE',  ( 28.00000000000000000, -17.50000000000000000, 20.05051025721700242 ) ) ;
#14932 = VERTEX_POINT ( 'NONE', #6504 ) ;
#14933 = CARTESIAN_POINT ( 'NONE',  ( 11.18999999999999950, 12.00000000000000178, -4.250000000000000000 ) ) ;
#14934 = ORIENTED_EDGE ( 'NONE', *, *, #62662, .F. ) ;
#14935 = VERTEX_POINT ( 'NONE', #65881 ) ;
#14936 = DIRECTION ( 'NONE',  ( 1.000000000000000000, -0.000000000000000000, 0.000000000000000000 ) ) ;
#14937 = DIRECTION ( 'NONE',  ( 1.836970198721029934E-16, 1.836970198721010706E-16, -1.000000000000000000 ) ) ;
#14938 = DIRECTION ( 'NONE',  ( -1.000000000000000000, 0.000000000000000000, 0.000000000000000000 ) ) ;
#14939 = AXIS2_PLACEMENT_3D ( 'NONE', #54343, #44742, #247 ) ;
#14940 = CARTESIAN_POINT ( 'NONE',  ( 7.000000000000000000, -38.15000000000000568, -14.50000000000000000 ) ) ;
#14941 = CARTESIAN_POINT ( 'NONE',  ( -16.75000000000000000, -2.500000000000000000, 21.77831216351300014 ) ) ;
#14942 = VERTEX_POINT ( 'NONE', #27376 ) ;
#14943 = VERTEX_POINT ( 'NONE', #44305 ) ;
#14945 = ORIENTED_EDGE ( 'NONE', *, *, #50298, .T. ) ;
#14944 = DIRECTION ( 'NONE',  ( 0.000000000000000000, 0.000000000000000000, 1.000000000000000000 ) ) ;
#14946 = AXIS2_PLACEMENT_3D ( 'NONE', #29262, #34573, #61810 ) ;
#14947 = ORIENTED_EDGE ( 'NONE', *, *, #55895, .T. ) ;
#14948 = FACE_OUTER_BOUND ( 'NONE', #50331, .T. ) ;
#14949 = AXIS2_PLACEMENT_3D ( 'NONE', #13698, #35246, #62845 ) ;
#14950 = DIRECTION ( 'NONE',  ( 1.000000000000000000, 0.000000000000000000, 0.000000000000000000 ) ) ;
#14951 = PLANE ( 'NONE',  #60203 ) ;
#14952 = AXIS2_PLACEMENT_3D ( 'NONE', #18727, #24738, #62919 ) ;
#14953 = FACE_OUTER_BOUND ( 'NONE', #30246, .T. ) ;
#14955 = CARTESIAN_POINT ( 'NONE',  ( -6.817976262117261044, 9.897976262117179402, 26.00000000000000711 ) ) ;
#14954 = DIRECTION ( 'NONE',  ( 1.000000000000000000, 0.000000000000000000, -0.000000000000000000 ) ) ;
#14956 = ORIENTED_EDGE ( 'NONE', *, *, #7601, .F. ) ;
#14957 = ORIENTED_EDGE ( 'NONE', *, *, #63145, .T. ) ;
#14958 = ORIENTED_EDGE ( 'NONE', *, *, #3970, .F. ) ;
#14959 = EDGE_LOOP ( 'NONE', ( #64811, #52833, #56719, #59942 ) ) ;
#14960 = DIRECTION ( 'NONE',  ( 1.000000000000000000, 3.016910393003147986E-15, 1.108394896831706469E-30 ) ) ;
#14961 = CARTESIAN_POINT ( 'NONE',  ( 8.835729544836331328, 7.955476262117188391, 54.00000000000000711 ) ) ;
#14962 = EDGE_CURVE ( 'NONE', #27615, #16092, #65545, .T. ) ;
#14963 = PLANE ( 'NONE',  #50058 ) ;
#14964 = EDGE_CURVE ( 'NONE', #51473, #67681, #503, .T. ) ;
#14965 = EDGE_LOOP ( 'NONE', ( #34053, #68781, #42539, #14144 ) ) ;
#14966 = VERTEX_POINT ( 'NONE', #16417 ) ;
#14967 = EDGE_CURVE ( 'NONE', #28585, #31147, #60227, .T. ) ;
#14968 = EDGE_LOOP ( 'NONE', ( #20161, #19548, #27066, #34329 ) ) ;
#14969 = DIRECTION ( 'NONE',  ( -0.000000000000000000, -0.000000000000000000, -1.000000000000000000 ) ) ;
#14970 = VERTEX_POINT ( 'NONE', #16766 ) ;
#14971 = EDGE_CURVE ( 'NONE', #355, #45686, #55286, .T. ) ;
#14972 = ORIENTED_EDGE ( 'NONE', *, *, #24124, .T. ) ;
#14973 = CARTESIAN_POINT ( 'NONE',  ( -7.250000000000000888, 7.450000000000003730, -21.50000000000000000 ) ) ;
#14974 = VECTOR ( 'NONE', #37712, 1000.000000000000000 ) ;
#14976 = VERTEX_POINT ( 'NONE', #870 ) ;
#14975 = EDGE_CURVE ( 'NONE', #60260, #67402, #37992, .T. ) ;
#14977 = VERTEX_POINT ( 'NONE', #33368 ) ;
#14979 = ADVANCED_FACE ( 'NONE', ( #59551 ), #49626, .F. ) ;
#14978 = CARTESIAN_POINT ( 'NONE',  ( 7.450000000000006395, 7.250000000000000888, -18.50000000000000000 ) ) ;
#14980 = EDGE_CURVE ( 'NONE', #16596, #62948, #54952, .T. ) ;
#14981 = VECTOR ( 'NONE', #67434, 1000.000000000000000 ) ;
#14983 = ORIENTED_EDGE ( 'NONE', *, *, #5901, .F. ) ;
#14982 = FACE_OUTER_BOUND ( 'NONE', #69027, .T. ) ;
#14985 = EDGE_LOOP ( 'NONE', ( #69714, #45351 ) ) ;
#14984 = EDGE_CURVE ( 'NONE', #24256, #10988, #18748, .T. ) ;
#14986 = DIRECTION ( 'NONE',  ( 0.000000000000000000, 1.000000000000000000, 0.000000000000000000 ) ) ;
#14987 = DIRECTION ( 'NONE',  ( -1.836970198721029934E-16, -1.836970198721010706E-16, 1.000000000000000000 ) ) ;
#14989 = EDGE_LOOP ( 'NONE', ( #10314, #21586, #21390, #17515 ) ) ;
#14988 = DIRECTION ( 'NONE',  ( 0.000000000000000000, -0.7046037717806115097, -0.7096009616626348659 ) ) ;
#14990 = ORIENTED_EDGE ( 'NONE', *, *, #2993, .F. ) ;
#14991 = CARTESIAN_POINT ( 'NONE',  ( 14.45366306705350112, -0.2717122460102528447, 21.66072723692567692 ) ) ;
#14992 = CARTESIAN_POINT ( 'NONE',  ( -7.250000000000000888, 7.450000000000003730, -20.00000000000000000 ) ) ;
#14993 = LINE ( 'NONE', #68739, #14292 ) ;
#14994 = CARTESIAN_POINT ( 'NONE',  ( 10.74648345035335240, 1.677516549646529409, 455.0000000000000568 ) ) ;
#14995 = ORIENTED_EDGE ( 'NONE', *, *, #63349, .F. ) ;
#14996 = CARTESIAN_POINT ( 'NONE',  ( -29.50000000000000355, -11.50000000000100009, -15.00000000000084910 ) ) ;
#14997 = LINE ( 'NONE', #20294, #10605 ) ;
#14998 = AXIS2_PLACEMENT_3D ( 'NONE', #28402, #60926, #39367 ) ;
#14999 = PLANE ( 'NONE',  #21029 ) ;
#15000 = CARTESIAN_POINT ( 'NONE',  ( -1.466476262117230034, 9.390476262117152473, 54.00000000000000711 ) ) ;
#15002 = CARTESIAN_POINT ( 'NONE',  ( 276.8775010008008053, -25.00000000000000000, 17.50000000000000000 ) ) ;
#15001 = AXIS2_PLACEMENT_3D ( 'NONE', #56468, #25000, #61778 ) ;
#15003 = AXIS2_PLACEMENT_3D ( 'NONE', #35424, #50304, #7515 ) ;
#15004 = CARTESIAN_POINT ( 'NONE',  ( 22.90000000000000213, -0.2000000000089119934, -8.913009219568841313E-12 ) ) ;
#15005 = ORIENTED_EDGE ( 'NONE', *, *, #43223, .T. ) ;
#15006 = VECTOR ( 'NONE', #46636, 1000.000000000000000 ) ;
#15007 = FACE_OUTER_BOUND ( 'NONE', #65051, .T. ) ;
#15008 = AXIS2_PLACEMENT_3D ( 'NONE', #5343, #47407, #16277 ) ;
#15009 = CARTESIAN_POINT ( 'NONE',  ( -11.11351654964671098, 7.793516549646603231, 455.0000000000000568 ) ) ;
#15010 = ORIENTED_EDGE ( 'NONE', *, *, #58692, .T. ) ;
#15011 = FACE_OUTER_BOUND ( 'NONE', #16900, .T. ) ;
#15012 = CARTESIAN_POINT ( 'NONE',  ( 283.0000000000000568, -20.40000000000000213, -17.35424868893542438 ) ) ;
#15013 = CARTESIAN_POINT ( 'NONE',  ( -7.250000000000000888, 8.250000000000001776, -13.50000000000000178 ) ) ;
#15014 = CARTESIAN_POINT ( 'NONE',  ( 24.90000000000000213, -14.06939075806902117, -20.80000000000000426 ) ) ;
#15015 = DIRECTION ( 'NONE',  ( -0.000000000000000000, -0.000000000000000000, -1.000000000000000000 ) ) ;
#15017 = ORIENTED_EDGE ( 'NONE', *, *, #5608, .T. ) ;
#15016 = EDGE_CURVE ( 'NONE', #4682, #38301, #33021, .T. ) ;
#15018 = CARTESIAN_POINT ( 'NONE',  ( 15.50000000000000000, -0.2000000000000000111, 19.19999999702029925 ) ) ;
#15019 = LINE ( 'NONE', #10415, #53165 ) ;
#15020 = AXIS2_PLACEMENT_3D ( 'NONE', #18832, #61962, #51353 ) ;
#15021 = CARTESIAN_POINT ( 'NONE',  ( 49.00000000000000000, -0.2000000000089119934, -8.913009219568841313E-12 ) ) ;
#15022 = DIRECTION ( 'NONE',  ( 0.000000000000000000, 0.000000000000000000, 1.000000000000000000 ) ) ;
#15023 = ADVANCED_FACE ( 'NONE', ( #28393 ), #39012, .F. ) ;
#15024 = LINE ( 'NONE', #41182, #46369 ) ;
#15025 = CIRCLE ( 'NONE', #31994, 0.1999999999999987899 ) ;
#15026 = VERTEX_POINT ( 'NONE', #64054 ) ;
#15028 = ORIENTED_EDGE ( 'NONE', *, *, #66371, .T. ) ;
#15027 = CARTESIAN_POINT ( 'NONE',  ( 11.12648345035340647, 9.093516549646563973, 455.0000000000000568 ) ) ;
#15029 = LINE ( 'NONE', #36586, #11280 ) ;
#15030 = DIRECTION ( 'NONE',  ( -2.135044278125299371E-15, -1.000000000000000000, 0.000000000000000000 ) ) ;
#15031 = CARTESIAN_POINT ( 'NONE',  ( 0.000000000000000000, 0.000000000000000000, -8.000000000000000000 ) ) ;
#15033 = ORIENTED_EDGE ( 'NONE', *, *, #32569, .F. ) ;
#15032 = ADVANCED_FACE ( 'NONE', ( #31524 ), #53435, .F. ) ;
#15034 = VECTOR ( 'NONE', #14445, 1000.000000000000000 ) ;
#15035 = SURFACE_SIDE_STYLE ('',( #53569 ) ) ;
#15036 = CARTESIAN_POINT ( 'NONE',  ( 21.90000000000000213, -0.2000000000089119934, -8.913009219568841313E-12 ) ) ;
#15037 = ORIENTED_EDGE ( 'NONE', *, *, #42969, .F. ) ;
#15038 = ORIENTED_EDGE ( 'NONE', *, *, #67950, .T. ) ;
#15039 = EDGE_CURVE ( 'NONE', #44524, #64431, #4310, .T. ) ;
#15040 = ORIENTED_EDGE ( 'NONE', *, *, #42673, .T. ) ;
#15041 = PLANE ( 'NONE',  #41073 ) ;
#15042 = CARTESIAN_POINT ( 'NONE',  ( -7.250000000000001776, -7.249999999999998224, -25.50000000000000355 ) ) ;
#15043 = FACE_OUTER_BOUND ( 'NONE', #42908, .T. ) ;
#15044 = VECTOR ( 'NONE', #29025, 1000.000000000000114 ) ;
#15045 = ADVANCED_FACE ( 'NONE', ( #21939 ), #47766, .F. ) ;
#15046 = ORIENTED_EDGE ( 'NONE', *, *, #8428, .F. ) ;
#15047 = ORIENTED_EDGE ( 'NONE', *, *, #17340, .F. ) ;
#15048 = DIRECTION ( 'NONE',  ( 0.000000000000000000, 0.000000000000000000, 1.000000000000000000 ) ) ;
#15049 = AXIS2_PLACEMENT_3D ( 'NONE', #36570, #38587, #65458 ) ;
#15050 = LINE ( 'NONE', #36611, #29365 ) ;
#15051 = ORIENTED_EDGE ( 'NONE', *, *, #53665, .T. ) ;
#15052 = AXIS2_PLACEMENT_3D ( 'NONE', #16146, #59279, #26766 ) ;
#15053 = ORIENTED_EDGE ( 'NONE', *, *, #47138, .F. ) ;
#15054 = VERTEX_POINT ( 'NONE', #59075 ) ;
#15055 = ORIENTED_EDGE ( 'NONE', *, *, #57793, .F. ) ;
#15056 = LINE ( 'NONE', #59589, #27130 ) ;
#15057 = AXIS2_PLACEMENT_3D ( 'NONE', #16560, #26828, #42373 ) ;
#15058 = AXIS2_PLACEMENT_3D ( 'NONE', #50466, #56459, #40543 ) ;
#15059 = EDGE_CURVE ( 'NONE', #7017, #41637, #64394, .T. ) ;
#15061 = ORIENTED_EDGE ( 'NONE', *, *, #52068, .F. ) ;
#15060 = DIRECTION ( 'NONE',  ( 1.836970198721029934E-16, -1.836970198721036344E-16, 1.000000000000000000 ) ) ;
#15062 = EDGE_CURVE ( 'NONE', #15345, #26986, #54919, .T. ) ;
#15063 = CARTESIAN_POINT ( 'NONE',  ( -8.250000000000001776, 0.000000000000000000, -23.50000000000000000 ) ) ;
#15064 = DIRECTION ( 'NONE',  ( -1.000000000000000000, 0.000000000000000000, 0.000000000000000000 ) ) ;
#15065 = PLANE ( 'NONE',  #3070 ) ;
#15066 = ORIENTED_EDGE ( 'NONE', *, *, #51215, .F. ) ;
#15067 = ORIENTED_EDGE ( 'NONE', *, *, #54161, .F. ) ;
#15068 = AXIS2_PLACEMENT_3D ( 'NONE', #42847, #11364, #5729 ) ;
#15069 = ADVANCED_FACE ( 'NONE', ( #48128 ), #32207, .F. ) ;
#15070 = FACE_OUTER_BOUND ( 'NONE', #25937, .T. ) ;
#15071 = AXIS2_PLACEMENT_3D ( 'NONE', #12969, #62116, #24297 ) ;
#15072 = LINE ( 'NONE', #58204, #33796 ) ;
#15073 = ORIENTED_EDGE ( 'NONE', *, *, #27013, .F. ) ;
#15074 = DIRECTION ( 'NONE',  ( -1.794541526872559352E-16, -1.000000000000000000, 0.000000000000000000 ) ) ;
#15075 = DIRECTION ( 'NONE',  ( -1.000000000000000000, 0.000000000000000000, 0.000000000000000000 ) ) ;
#15076 = DIRECTION ( 'NONE',  ( 0.000000000000000000, 0.000000000000000000, -1.000000000000000000 ) ) ;
#15077 = ORIENTED_EDGE ( 'NONE', *, *, #49300, .F. ) ;
#15078 = VECTOR ( 'NONE', #44721, 1000.000000000000114 ) ;
#15079 = DIRECTION ( 'NONE',  ( -0.000000000000000000, -0.000000000000000000, -1.000000000000000000 ) ) ;
#15080 = CARTESIAN_POINT ( 'NONE',  ( 0.000000000000000000, -7.449999999999998401, -9.500000000000001776 ) ) ;
#15081 = FACE_OUTER_BOUND ( 'NONE', #760, .T. ) ;
#15082 = DIRECTION ( 'NONE',  ( 1.000000000000000000, 0.000000000000000000, 0.000000000000000000 ) ) ;
#15083 = EDGE_CURVE ( 'NONE', #27322, #42854, #33449, .T. ) ;
#15084 = DIRECTION ( 'NONE',  ( 1.000000000000000000, -1.678252938371784572E-14, 1.836970198720999119E-16 ) ) ;
#15085 = VERTEX_POINT ( 'NONE', #58027 ) ;
#15086 = DIRECTION ( 'NONE',  ( 0.000000000000000000, 0.000000000000000000, -1.000000000000000000 ) ) ;
#15087 = DIRECTION ( 'NONE',  ( -0.7671651518153131954, -0.6414496315691415873, 0.000000000000000000 ) ) ;
#15088 = CARTESIAN_POINT ( 'NONE',  ( 7.450000000000006395, 7.250000000000000888, -24.50000000000000000 ) ) ;
#15089 = EDGE_CURVE ( 'NONE', #67565, #59771, #27258, .T. ) ;
#15090 = DIRECTION ( 'NONE',  ( 0.000000000000000000, 1.000000000000000000, 0.000000000000000000 ) ) ;
#15091 = VECTOR ( 'NONE', #6397, 1000.000000000000000 ) ;
#15092 = VECTOR ( 'NONE', #29187, 1000.000000000000000 ) ;
#15093 = EDGE_LOOP ( 'NONE', ( #64432, #4577, #54458, #42531, #24057, #65944 ) ) ;
#15094 = CARTESIAN_POINT ( 'NONE',  ( 30.00000000000000000, -5.200000000000001066, 9.399999999999998579 ) ) ;
#15095 = CARTESIAN_POINT ( 'NONE',  ( 7.250000000000005329, 8.250000000000001776, -24.50000000000000000 ) ) ;
#15096 = ADVANCED_FACE ( 'NONE', ( #42110, #68987 ), #42811, .T. ) ;
#15097 = VECTOR ( 'NONE', #49793, 1000.000000000000000 ) ;
#15098 = FACE_OUTER_BOUND ( 'NONE', #46517, .T. ) ;
#15099 = CARTESIAN_POINT ( 'NONE',  ( -2.530476262117229425, 9.547976262117158441, 54.00000000000000711 ) ) ;
#15100 = ORIENTED_EDGE ( 'NONE', *, *, #44140, .T. ) ;
#15101 = LINE ( 'NONE', #30311, #52396 ) ;
#15102 = EDGE_CURVE ( 'NONE', #11645, #43624, #63337, .T. ) ;
#15103 = CARTESIAN_POINT ( 'NONE',  ( 4.201500623656039934, 7.259684009079806266, 455.0000000000000568 ) ) ;
#15104 = CARTESIAN_POINT ( 'NONE',  ( 14.75000000000000000, -0.2500000000000020539, 26.75000000000000355 ) ) ;
#15105 = CARTESIAN_POINT ( 'NONE',  ( 283.0000000000000568, -30.80000000000000071, 8.900000000000000355 ) ) ;
#15106 = DIRECTION ( 'NONE',  ( -0.000000000000000000, -0.000000000000000000, -1.000000000000000000 ) ) ;
#15107 = AXIS2_PLACEMENT_3D ( 'NONE', #34307, #33967, #18761 ) ;
#15109 = AXIS2_PLACEMENT_3D ( 'NONE', #18075, #18782, #67221 ) ;
#15108 = CYLINDRICAL_SURFACE ( 'NONE', #6015, 4.000000000000000000 ) ;
#15110 = ADVANCED_FACE ( 'NONE', ( #14901 ), #53787, .F. ) ;
#15111 = CARTESIAN_POINT ( 'NONE',  ( 49.00000000000000000, -21.00000000000000000, 13.86939075806900057 ) ) ;
#15112 = VERTEX_POINT ( 'NONE', #40 ) ;
#15113 = ORIENTED_EDGE ( 'NONE', *, *, #31773, .T. ) ;
#15114 = DIRECTION ( 'NONE',  ( 0.000000000000000000, -0.8206518066484758123, 0.5714285714283042772 ) ) ;
#15115 = CARTESIAN_POINT ( 'NONE',  ( 29.89999999999999858, 20.60000000000000142, 2.370429594502469981E-15 ) ) ;
#15117 = VERTEX_POINT ( 'NONE', #43155 ) ;
#15116 = EDGE_CURVE ( 'NONE', #8498, #61197, #15252, .T. ) ;
#15118 = CARTESIAN_POINT ( 'NONE',  ( -4.188533722949335569, 7.259684009079808931, 195.0000000000000284 ) ) ;
#15119 = EDGE_CURVE ( 'NONE', #20472, #53691, #64730, .T. ) ;
#15120 = LINE ( 'NONE', #37384, #206 ) ;
#15121 = EDGE_LOOP ( 'NONE', ( #42761, #46711, #21669, #62223 ) ) ;
#15122 = EDGE_CURVE ( 'NONE', #9679, #32778, #37863, .T. ) ;
#15123 = EDGE_CURVE ( 'NONE', #48173, #25947, #10989, .T. ) ;
#15124 = LINE ( 'NONE', #32079, #69561 ) ;
#15125 = EDGE_LOOP ( 'NONE', ( #46429, #46341, #31602, #25583, #47323, #23533, #20786 ) ) ;
#15126 = ORIENTED_EDGE ( 'NONE', *, *, #18723, .F. ) ;
#15127 = CARTESIAN_POINT ( 'NONE',  ( 14.89999999999999680, -14.06939075806902117, -20.80000000000000426 ) ) ;
#15128 = ORIENTED_EDGE ( 'NONE', *, *, #60336, .T. ) ;
#15129 = EDGE_CURVE ( 'NONE', #31486, #48338, #38009, .T. ) ;
#15130 = DIRECTION ( 'NONE',  ( 1.000000000000000000, -0.000000000000000000, 0.000000000000000000 ) ) ;
#15131 = LINE ( 'NONE', #63921, #15572 ) ;
#15132 = DIRECTION ( 'NONE',  ( 0.000000000000000000, -1.000000000000000000, 3.819861094142539476E-12 ) ) ;
#15133 = EDGE_LOOP ( 'NONE', ( #68942, #43022, #56198, #26007, #3633, #8329, #32089 ) ) ;
#15134 = DIRECTION ( 'NONE',  ( 0.000000000000000000, -1.000000000000000000, 0.000000000000000000 ) ) ;
#15136 = CARTESIAN_POINT ( 'NONE',  ( 7.000000000000000000, -27.13000000000000611, 15.49999999999930012 ) ) ;
#15135 = CARTESIAN_POINT ( 'NONE',  ( 75.42576880091937142, 0.000000000000000000, 289.4830310981789125 ) ) ;
#15137 = ORIENTED_EDGE ( 'NONE', *, *, #18936, .T. ) ;
#15138 = VERTEX_POINT ( 'NONE', #39569 ) ;
#15139 = ORIENTED_EDGE ( 'NONE', *, *, #1152, .F. ) ;
#15141 = ORIENTED_EDGE ( 'NONE', *, *, #20857, .T. ) ;
#15140 = SHAPE_DEFINITION_REPRESENTATION ( #55550, #60228 ) ;
#15142 =( REPRESENTATION_RELATIONSHIP ('NONE','NONE', #33057, #35 ) REPRESENTATION_RELATIONSHIP_WITH_TRANSFORMATION ( #15829 )SHAPE_REPRESENTATION_RELATIONSHIP( ) );
#15143 = DIRECTION ( 'NONE',  ( -1.000000000000000000, 0.000000000000000000, 0.000000000000000000 ) ) ;
#15144 = EDGE_CURVE ( 'NONE', #66965, #55486, #54970, .T. ) ;
#15146 = VERTEX_POINT ( 'NONE', #59772 ) ;
#15145 = CARTESIAN_POINT ( 'NONE',  ( 16.75000000000000355, -0.2715193793361411756, -22.01281590054916038 ) ) ;
#15147 = EDGE_CURVE ( 'NONE', #12989, #20073, #43498, .T. ) ;
#15148 = CARTESIAN_POINT ( 'NONE',  ( -6.835476262117260227, 10.49297626211718359, 54.00000000000000711 ) ) ;
#15149 = VECTOR ( 'NONE', #55442, 1000.000000000000114 ) ;
#15150 = VECTOR ( 'NONE', #24163, 1000.000000000000000 ) ;
#15151 = DIRECTION ( 'NONE',  ( 0.000000000000000000, 0.000000000000000000, 1.000000000000000000 ) ) ;
#15152 = ORIENTED_EDGE ( 'NONE', *, *, #61100, .T. ) ;
#15153 = ORIENTED_EDGE ( 'NONE', *, *, #2993, .T. ) ;
#15154 = AXIS2_PLACEMENT_3D ( 'NONE', #14240, #23792, #67979 ) ;
#15155 = CIRCLE ( 'NONE', #10654, 3.500000000000000000 ) ;
#15156 = DIRECTION ( 'NONE',  ( -1.000000000000000000, 0.000000000000000000, 0.000000000000000000 ) ) ;
#15157 = ORIENTED_EDGE ( 'NONE', *, *, #31259, .F. ) ;
#15158 = CARTESIAN_POINT ( 'NONE',  ( 7.250000000000005329, -7.249999999999998224, -21.50000000000000000 ) ) ;
#15159 = LINE ( 'NONE', #43407, #35782 ) ;
#15160 = AXIS2_PLACEMENT_3D ( 'NONE', #8853, #36072, #30425 ) ;
#15161 = FACE_OUTER_BOUND ( 'NONE', #30181, .T. ) ;
#15162 = ORIENTED_EDGE ( 'NONE', *, *, #42795, .T. ) ;
#15163 = VECTOR ( 'NONE', #34525, 1000.000000000000000 ) ;
#15164 = EDGE_CURVE ( 'NONE', #19912, #30539, #28945, .T. ) ;
#15165 = DIRECTION ( 'NONE',  ( 0.000000000000000000, 0.000000000000000000, 1.000000000000000000 ) ) ;
#15166 = LINE ( 'NONE', #26126, #19973 ) ;
#15168 = ORIENTED_EDGE ( 'NONE', *, *, #31386, .T. ) ;
#15167 = CARTESIAN_POINT ( 'NONE',  ( 4.622483450353380263, -3.606483450353395792, 195.0000000000000284 ) ) ;
#15170 = ORIENTED_EDGE ( 'NONE', *, *, #23572, .F. ) ;
#15169 = DIRECTION ( 'NONE',  ( -0.000000000000000000, -0.000000000000000000, 1.000000000000000000 ) ) ;
#15171 = AXIS2_PLACEMENT_3D ( 'NONE', #45274, #49897, #23379 ) ;
#15172 = CARTESIAN_POINT ( 'NONE',  ( 34.89999999999999858, 13.66939075806899240, 20.79999999999999361 ) ) ;
#15173 = CYLINDRICAL_SURFACE ( 'NONE', #13795, 1.929199999999998028 ) ;
#15174 = DIRECTION ( 'NONE',  ( 0.000000000000000000, -1.000000000000000000, 0.000000000000000000 ) ) ;
#15175 = DIRECTION ( 'NONE',  ( 1.000000000000000000, -0.000000000000000000, 0.000000000000000000 ) ) ;
#15176 = B_SPLINE_CURVE_WITH_KNOTS ( 'NONE', 3,
 ( #19593, #53197, #10393, #4742, #31963, #15703 ),
 .UNSPECIFIED., .F., .F.,
 ( 4, 2, 4 ),
 ( 1.820537833122030991, 2.555393473688635453, 3.290249114255240137 ),
 .UNSPECIFIED. ) ;
#15177 = PLANE ( 'NONE',  #54539 ) ;
#15178 = ORIENTED_EDGE ( 'NONE', *, *, #17311, .F. ) ;
#15179 = CARTESIAN_POINT ( 'NONE',  ( 7.250000000000004441, 7.450000000000001954, -19.50000000000000000 ) ) ;
#15180 = DIRECTION ( 'NONE',  ( 0.000000000000000000, -3.673940397442059868E-16, 1.000000000000000000 ) ) ;
#15181 = EDGE_CURVE ( 'NONE', #47019, #42883, #16651, .T. ) ;
#15183 = ORIENTED_EDGE ( 'NONE', *, *, #20329, .F. ) ;
#15182 = CARTESIAN_POINT ( 'NONE',  ( 41.09999999999999432, -21.00000000000000000, 14.57806571531351914 ) ) ;
#15184 = DIRECTION ( 'NONE',  ( -1.000000000000000000, 0.000000000000000000, 0.000000000000000000 ) ) ;
#15185 = AXIS2_PLACEMENT_3D ( 'NONE', #49290, #27707, #11774 ) ;
#15186 = CARTESIAN_POINT ( 'NONE',  ( 3.848229544836324845, 7.342976262117209885, 26.00000000000000711 ) ) ;
#15187 = ADVANCED_FACE ( 'NONE', ( #44523 ), #49164, .T. ) ;
#15188 = CARTESIAN_POINT ( 'NONE',  ( 41.09999999999999432, -14.06939075806900163, 20.80000000000000426 ) ) ;
#15189 = ORIENTED_EDGE ( 'NONE', *, *, #10543, .F. ) ;
#15190 = PLANE ( 'NONE',  #36584 ) ;
#15191 = ADVANCED_FACE ( 'NONE', ( #28621 ), #736, .T. ) ;
#15192 = DIRECTION ( 'NONE',  ( 0.000000000000000000, 0.000000000000000000, 1.000000000000000000 ) ) ;
#15193 = CIRCLE ( 'NONE', #12877, 3.499999999999849454 ) ;
#15194 = EDGE_LOOP ( 'NONE', ( #63831, #1330, #56010, #61899, #1416, #31452, #31672, #2602, #43534, #13587 ) ) ;
#15195 = DIRECTION ( 'NONE',  ( 1.000000000000000000, -0.000000000000000000, 0.000000000000000000 ) ) ;
#15196 = CYLINDRICAL_SURFACE ( 'NONE', #47885, 0.5249999999999994671 ) ;
#15197 = EDGE_CURVE ( 'NONE', #38472, #51495, #67215, .T. ) ;
#15198 = CARTESIAN_POINT ( 'NONE',  ( 22.90000000000000213, 0.000000000000000000, 1.508455196501571824E-15 ) ) ;
#15199 = DIRECTION ( 'NONE',  ( -0.000000000000000000, -0.000000000000000000, -1.000000000000000000 ) ) ;
#15200 = VECTOR ( 'NONE', #52221, 1000.000000000000000 ) ;
#15201 = VECTOR ( 'NONE', #47055, 1000.000000000000000 ) ;
#15202 = ORIENTED_EDGE ( 'NONE', *, *, #64387, .F. ) ;
#15203 = ORIENTED_EDGE ( 'NONE', *, *, #29934, .T. ) ;
#15204 = DIRECTION ( 'NONE',  ( 0.6414496315691445849, -0.7671651518153106419, 0.000000000000000000 ) ) ;
#15205 = VERTEX_POINT ( 'NONE', #22635 ) ;
#15206 = ORIENTED_EDGE ( 'NONE', *, *, #5144, .T. ) ;
#15207 = CARTESIAN_POINT ( 'NONE',  ( 7.250000000000005329, 8.250000000000001776, -26.00000000000001066 ) ) ;
#15208 = AXIS2_PLACEMENT_3D ( 'NONE', #43194, #59116, #54174 ) ;
#15209 = VECTOR ( 'NONE', #64156, 1000.000000000000000 ) ;
#15210 = EDGE_CURVE ( 'NONE', #51178, #12885, #28971, .T. ) ;
#15211 = CYLINDRICAL_SURFACE ( 'NONE', #10653, 1.399999999999998579 ) ;
#15212 = AXIS2_PLACEMENT_3D ( 'NONE', #57906, #63210, #15132 ) ;
#15213 = CARTESIAN_POINT ( 'NONE',  ( -7.798499376344157241, -7.272650909786626983, 455.0000000000000568 ) ) ;
#15214 = VERTEX_POINT ( 'NONE', #65428 ) ;
#15215 = ORIENTED_EDGE ( 'NONE', *, *, #46151, .T. ) ;
#15216 = DIRECTION ( 'NONE',  ( 1.000000000000000000, 0.000000000000000000, 0.000000000000000000 ) ) ;
#15217 = VERTEX_POINT ( 'NONE', #38221 ) ;
#15218 = ORIENTED_EDGE ( 'NONE', *, *, #55332, .T. ) ;
#15219 = CARTESIAN_POINT ( 'NONE',  ( 6.849523737882817542, -10.31452373788282095, 54.00000000000000711 ) ) ;
#15220 = DIRECTION ( 'NONE',  ( -1.836970198721029934E-16, 1.836970198721036344E-16, -1.000000000000000000 ) ) ;
#15221 = DIRECTION ( 'NONE',  ( 0.000000000000000000, 1.000000000000000000, 0.000000000000000000 ) ) ;
#15222 = ORIENTED_EDGE ( 'NONE', *, *, #26281, .T. ) ;
#15223 = AXIS2_PLACEMENT_3D ( 'NONE', #6344, #31843, #33210 ) ;
#15224 = CARTESIAN_POINT ( 'NONE',  ( 30.00000000000000000, -5.000000000000000000, -27.00000000000000000 ) ) ;
#15226 = CARTESIAN_POINT ( 'NONE',  ( 36.90000000000000568, -21.00000000000000000, 13.86939075806900057 ) ) ;
#15225 = CARTESIAN_POINT ( 'NONE',  ( 7.000000000000000000, -26.50000000000000000, -9.080000000000000071 ) ) ;
#15227 = ORIENTED_EDGE ( 'NONE', *, *, #3139, .F. ) ;
#15229 = ORIENTED_EDGE ( 'NONE', *, *, #8116, .T. ) ;
#15228 = CARTESIAN_POINT ( 'NONE',  ( -3.663616288757094885, -6.364920264886888113, 54.00000000000000711 ) ) ;
#15230 = ORIENTED_EDGE ( 'NONE', *, *, #51136, .T. ) ;
#15231 = CYLINDRICAL_SURFACE ( 'NONE', #23144, 0.3499999999999614531 ) ;
#15232 = ADVANCED_FACE ( 'NONE', ( #16986 ), #60796, .T. ) ;
#15233 = EDGE_CURVE ( 'NONE', #7480, #9302, #15437, .T. ) ;
#15234 = DIRECTION ( 'NONE',  ( 1.000000000000000000, -0.000000000000000000, 0.000000000000000000 ) ) ;
#15235 = ORIENTED_EDGE ( 'NONE', *, *, #35608, .F. ) ;
#15236 = CIRCLE ( 'NONE', #59242, 1.449999999999996403 ) ;
#15237 = EDGE_CURVE ( 'NONE', #26720, #59384, #31255, .T. ) ;
#15238 = DIRECTION ( 'NONE',  ( 0.000000000000000000, -3.673940397442059868E-16, 1.000000000000000000 ) ) ;
#15239 = CARTESIAN_POINT ( 'NONE',  ( -9.690000000000001279, -9.750000000000001776, -4.250000000000000000 ) ) ;
#15240 = CIRCLE ( 'NONE', #547, 1.000000000000000888 ) ;
#15241 = ORIENTED_EDGE ( 'NONE', *, *, #51903, .F. ) ;
#15242 = EDGE_LOOP ( 'NONE', ( #5061, #13855, #66522, #68320 ) ) ;
#15243 = LINE ( 'NONE', #52741, #28563 ) ;
#15244 = LINE ( 'NONE', #26201, #4591 ) ;
#15245 = ORIENTED_EDGE ( 'NONE', *, *, #39438, .T. ) ;
#15246 = AXIS2_PLACEMENT_3D ( 'NONE', #5002, #65099, #10310 ) ;
#15247 = AXIS2_PLACEMENT_3D ( 'NONE', #14080, #29995, #25051 ) ;
#15248 = CARTESIAN_POINT ( 'NONE',  ( -11.77351654964670935, 7.593516549646604830, 455.0000000000000568 ) ) ;
#15249 = DIRECTION ( 'NONE',  ( 0.000000000000000000, -0.7046037717806115097, -0.7096009616626348659 ) ) ;
#15251 = ORIENTED_EDGE ( 'NONE', *, *, #68668, .F. ) ;
#15250 = CARTESIAN_POINT ( 'NONE',  ( 18.89999999999999858, -14.06939075806900874, 20.80000000000001137 ) ) ;
#15253 = EDGE_LOOP ( 'NONE', ( #21842, #21445, #4673, #31944, #402, #2274, #55051, #3224 ) ) ;
#15252 = LINE ( 'NONE', #21602, #59454 ) ;
#15254 = CARTESIAN_POINT ( 'NONE',  ( 75.42576880091934299, 10.00000000000000000, 327.4830310981788557 ) ) ;
#15255 = VECTOR ( 'NONE', #704, 1000.000000000000000 ) ;
#15256 = VECTOR ( 'NONE', #7347, 1000.000000000000000 ) ;
#15257 = CARTESIAN_POINT ( 'NONE',  ( 8.612468434717241550, -2.005523737882825674, 54.00000000000000711 ) ) ;
#15258 = CARTESIAN_POINT ( 'NONE',  ( 106.4257688009193430, 10.00000000000000000, 330.9830310981789694 ) ) ;
#15259 = FACE_OUTER_BOUND ( 'NONE', #62644, .T. ) ;
#15260 = DIRECTION ( 'NONE',  ( 1.000000000000000000, 0.000000000000000000, 0.000000000000000000 ) ) ;
#15261 = DIRECTION ( 'NONE',  ( 0.7071067811865348052, -0.7071067811865602293, -3.278703137324831017E-30 ) ) ;
#15262 = ORIENTED_EDGE ( 'NONE', *, *, #3751, .F. ) ;
#15263 = DIRECTION ( 'NONE',  ( -0.000000000000000000, 1.000000000000000000, -0.000000000000000000 ) ) ;
#15265 = ORIENTED_EDGE ( 'NONE', *, *, #9587, .T. ) ;
#15264 = SURFACE_STYLE_FILL_AREA ( #42120 ) ;
#15266 = EDGE_CURVE ( 'NONE', #18370, #427, #33493, .T. ) ;
#15267 = CARTESIAN_POINT ( 'NONE',  ( 15.50000000000000000, -0.2038245569916610489, -23.94337567297399971 ) ) ;
#15268 = CARTESIAN_POINT ( 'NONE',  ( 30.00000000000000000, -13.79999999999979998, -17.30000000000000071 ) ) ;
#15269 = DIRECTION ( 'NONE',  ( 0.000000000000000000, 0.000000000000000000, -1.000000000000000000 ) ) ;
#15270 = CARTESIAN_POINT ( 'NONE',  ( 7.250000000000005329, -7.449999999999998401, -12.50000000000000000 ) ) ;
#15271 = ORIENTED_EDGE ( 'NONE', *, *, #22311, .T. ) ;
#15272 = DIRECTION ( 'NONE',  ( 0.000000000000000000, 0.000000000000000000, 1.000000000000000000 ) ) ;
#15273 = EDGE_CURVE ( 'NONE', #36105, #12301, #38887, .T. ) ;
#15274 = CARTESIAN_POINT ( 'NONE',  ( -3.650476262117333892, -10.31452373788281740, 54.00000000000000711 ) ) ;
#15275 = EDGE_CURVE ( 'NONE', #38702, #41857, #16551, .T. ) ;
#15276 = ORIENTED_EDGE ( 'NONE', *, *, #68542, .F. ) ;
#15277 = DIRECTION ( 'NONE',  ( 1.000000000000000000, 0.000000000000000000, 0.000000000000000000 ) ) ;
#15278 = PLANE ( 'NONE',  #26896 ) ;
#15279 = ADVANCED_FACE ( 'NONE', ( #1407 ), #68481, .F. ) ;
#15280 = EDGE_CURVE ( 'NONE', #47767, #14864, #33918, .T. ) ;
#15281 = LINE ( 'NONE', #31207, #40923 ) ;
#15282 = EDGE_CURVE ( 'NONE', #8019, #64293, #66455, .T. ) ;
#15283 = ORIENTED_EDGE ( 'NONE', *, *, #47040, .T. ) ;
#15284 = DIRECTION ( 'NONE',  ( 0.000000000000000000, 0.000000000000000000, -1.000000000000000000 ) ) ;
#15285 = ORIENTED_EDGE ( 'NONE', *, *, #26980, .T. ) ;
#15286 = ORIENTED_EDGE ( 'NONE', *, *, #37741, .T. ) ;
#15287 = DIRECTION ( 'NONE',  ( 1.836970198721029934E-16, 1.836970198721010706E-16, -1.000000000000000000 ) ) ;
#15288 = LINE ( 'NONE', #46399, #25212 ) ;
#15289 = LINE ( 'NONE', #32849, #9689 ) ;
#15290 = CIRCLE ( 'NONE', #3980, 0.1999999999999987899 ) ;
#15291 = CARTESIAN_POINT ( 'NONE',  ( 49.00000000000000000, -0.1999999999911430404, -8.864436962241481021E-12 ) ) ;
#15292 = VECTOR ( 'NONE', #24304, 1000.000000000000000 ) ;
#15293 = CARTESIAN_POINT ( 'NONE',  ( 9.929523737882748335, 0.9414762621171531842, 26.00000000000000711 ) ) ;
#15294 = ORIENTED_EDGE ( 'NONE', *, *, #11451, .F. ) ;
#15295 = ORIENTED_EDGE ( 'NONE', *, *, #28569, .T. ) ;
#15297 = ORIENTED_EDGE ( 'NONE', *, *, #39265, .F. ) ;
#15296 = CARTESIAN_POINT ( 'NONE',  ( 15.50000000000000000, -1.037157890325000054, 22.50000000000000000 ) ) ;
#15298 = VERTEX_POINT ( 'NONE', #50889 ) ;
#15299 = CARTESIAN_POINT ( 'NONE',  ( 176.4833316329832940, 9.000000000000001776, 324.6739988703752715 ) ) ;
#15300 = LINE ( 'NONE', #36881, #60263 ) ;
#15301 = DIRECTION ( 'NONE',  ( 0.000000000000000000, 1.000000000000000000, 0.000000000000000000 ) ) ;
#15302 = PLANE ( 'NONE',  #2922 ) ;
#15303 = AXIS2_PLACEMENT_3D ( 'NONE', #11213, #23204, #27136 ) ;
#15305 = CARTESIAN_POINT ( 'NONE',  ( 1.634292677759859869, -8.241237374594271969, 26.00000000000000000 ) ) ;
#15304 = CARTESIAN_POINT ( 'NONE',  ( 0.000000000000000000, 0.7500000000000000000, 0.000000000000000000 ) ) ;
#15306 = ORIENTED_EDGE ( 'NONE', *, *, #18200, .F. ) ;
#15307 = VERTEX_POINT ( 'NONE', #44536 ) ;
#15308 = VERTEX_POINT ( 'NONE', #8099 ) ;
#15309 = AXIS2_PLACEMENT_3D ( 'NONE', #22192, #16884, #38457 ) ;
#15310 = CARTESIAN_POINT ( 'NONE',  ( -6.500000000000002665, -6.500000000000002665, -1.000000000000000000 ) ) ;
#15311 = EDGE_CURVE ( 'NONE', #33396, #44394, #28981, .T. ) ;
#15312 = MECHANICAL_DESIGN_GEOMETRIC_PRESENTATION_REPRESENTATION (  '', ( #14134 ), #48068 ) ;
#15313 = DIRECTION ( 'NONE',  ( -1.000000000000000000, 0.000000000000000000, 0.000000000000000000 ) ) ;
#15314 = ORIENTED_EDGE ( 'NONE', *, *, #14788, .T. ) ;
#15315 = ORIENTED_EDGE ( 'NONE', *, *, #64373, .T. ) ;
#15316 = ORIENTED_EDGE ( 'NONE', *, *, #33580, .T. ) ;
#15317 = ADVANCED_FACE ( 'NONE', ( #12351 ), #13056, .T. ) ;
#15318 = AXIS2_PLACEMENT_3D ( 'NONE', #43167, #69713, #65773 ) ;
#15319 = EDGE_CURVE ( 'NONE', #4279, #43479, #35312, .T. ) ;
#15320 = DIRECTION ( 'NONE',  ( 1.000000000000000000, -0.000000000000000000, 0.000000000000000000 ) ) ;
#15321 = VERTEX_POINT ( 'NONE', #22981 ) ;
#15322 = CARTESIAN_POINT ( 'NONE',  ( -11.00000000000000000, -17.35230188589299871, 15.35019951917099945 ) ) ;
#15323 = EDGE_CURVE ( 'NONE', #611, #64746, #51242, .T. ) ;
#15324 = VERTEX_POINT ( 'NONE', #18015 ) ;
#15325 = ORIENTED_EDGE ( 'NONE', *, *, #17771, .F. ) ;
#15326 = CARTESIAN_POINT ( 'NONE',  ( 11.48848345035341900, 10.19191654964656202, 455.0000000000000568 ) ) ;
#15328 = ORIENTED_EDGE ( 'NONE', *, *, #7516, .F. ) ;
#15327 = CARTESIAN_POINT ( 'NONE',  ( 290.0000000000000000, -42.00000000000000000, 26.50000000000000000 ) ) ;
#15329 = ORIENTED_EDGE ( 'NONE', *, *, #34464, .T. ) ;
#15330 = DIRECTION ( 'NONE',  ( 0.000000000000000000, 0.000000000000000000, -1.000000000000000000 ) ) ;
#15331 = CARTESIAN_POINT ( 'NONE',  ( 10.92648345035340895, 9.093516549646565750, 455.0000000000000568 ) ) ;
#15332 = VECTOR ( 'NONE', #24637, 1000.000000000000000 ) ;
#15334 = ORIENTED_EDGE ( 'NONE', *, *, #42880, .T. ) ;
#15333 = DIRECTION ( 'NONE',  ( 0.7671651518153006499, -0.6414496315691565753, 0.000000000000000000 ) ) ;
#15335 = EDGE_LOOP ( 'NONE', ( #46690, #62159, #55508, #13641 ) ) ;
#15336 = LINE ( 'NONE', #36919, #34402 ) ;
#15337 = DIRECTION ( 'NONE',  ( -1.836970198721029934E-16, 1.836970198721036344E-16, -1.000000000000000000 ) ) ;
#15338 = VECTOR ( 'NONE', #25368, 1000.000000000000000 ) ;
#15339 = LINE ( 'NONE', #63075, #23843 ) ;
#15340 = CARTESIAN_POINT ( 'NONE',  ( 7.450000000000004619, -1.336933437520057563E-15, -8.500000000000000000 ) ) ;
#15341 = LINE ( 'NONE', #47857, #49670 ) ;
#15342 = AXIS2_PLACEMENT_3D ( 'NONE', #66323, #66658, #43716 ) ;
#15343 = ORIENTED_EDGE ( 'NONE', *, *, #66736, .T. ) ;
#15344 = DIRECTION ( 'NONE',  ( 0.000000000000000000, -1.000000000000000000, 0.000000000000000000 ) ) ;
#15345 = VERTEX_POINT ( 'NONE', #44896 ) ;
#15346 = VECTOR ( 'NONE', #27338, 1000.000000000000000 ) ;
#15347 = AXIS2_PLACEMENT_3D ( 'NONE', #32051, #36301, #57865 ) ;
#15349 = CARTESIAN_POINT ( 'NONE',  ( 0.5000000000000000000, 18.00000000000000355, 21.00000000000000000 ) ) ;
#15348 = CIRCLE ( 'NONE', #17595, 1.000000000000000000 ) ;
#15350 = FILL_AREA_STYLE_COLOUR ( '', #44722 ) ;
#15351 = CARTESIAN_POINT ( 'NONE',  ( -15.50000000000000000, -0.1999999999999999556, -22.50000000000000000 ) ) ;
#15352 = CARTESIAN_POINT ( 'NONE',  ( 9.737023737882804397, 6.817976262117185549, 54.00000000000000711 ) ) ;
#15353 = AXIS2_PLACEMENT_3D ( 'NONE', #16467, #55671, #38046 ) ;
#15354 = AXIS2_PLACEMENT_3D ( 'NONE', #59293, #43372, #22169 ) ;
#15355 = VECTOR ( 'NONE', #10685, 1000.000000000000000 ) ;
#15356 = CARTESIAN_POINT ( 'NONE',  ( 15.00000000000000000, -21.00000000000000000, 0.000000000000000000 ) ) ;
#15357 = ORIENTED_EDGE ( 'NONE', *, *, #50955, .T. ) ;
#15358 = CIRCLE ( 'NONE', #22168, 24.99999999998794920 ) ;
#15359 = CARTESIAN_POINT ( 'NONE',  ( 7.250000000000005329, -8.249999999999998224, -26.00000000000001066 ) ) ;
#15360 = EDGE_CURVE ( 'NONE', #3338, #6044, #8448, .T. ) ;
#15361 =( LENGTH_UNIT ( ) NAMED_UNIT ( * ) SI_UNIT ( .MILLI., .METRE. ) );
#15362 = EDGE_CURVE ( 'NONE', #58695, #67917, #65114, .T. ) ;
#15363 = AXIS2_PLACEMENT_3D ( 'NONE', #18287, #45870, #67451 ) ;
#15364 = ADVANCED_FACE ( 'NONE', ( #56209 ), #66116, .F. ) ;
#15365 = CYLINDRICAL_SURFACE ( 'NONE', #6745, 1.000000000000000000 ) ;
#15366 = VERTEX_POINT ( 'NONE', #2800 ) ;
#15367 = DIRECTION ( 'NONE',  ( 1.000000000000000000, 0.000000000000000000, 0.000000000000000000 ) ) ;
#15368 = LINE ( 'NONE', #31294, #32088 ) ;
#15369 = EDGE_CURVE ( 'NONE', #10245, #61001, #42541, .T. ) ;
#15370 = LINE ( 'NONE', #15716, #28603 ) ;
#15371 = CARTESIAN_POINT ( 'NONE',  ( 27.00000000000000000, 0.000000000000000000, 0.000000000000000000 ) ) ;
#15372 = DIRECTION ( 'NONE',  ( 1.000000000000000000, -0.000000000000000000, -0.000000000000000000 ) ) ;
#15373 = ORIENTED_EDGE ( 'NONE', *, *, #41471, .F. ) ;
#15374 = PLANE ( 'NONE',  #58091 ) ;
#15375 = FACE_OUTER_BOUND ( 'NONE', #15509, .T. ) ;
#15376 = CARTESIAN_POINT ( 'NONE',  ( -8.250000000000001776, -7.249999999999998224, -23.50000000000000000 ) ) ;
#15377 = FILL_AREA_STYLE_COLOUR ( '', #57999 ) ;
#15378 = EDGE_CURVE ( 'NONE', #32123, #66059, #56890, .T. ) ;
#15379 = CARTESIAN_POINT ( 'NONE',  ( 7.811466277050774565, 7.259684009079793832, 455.0000000000000568 ) ) ;
#15380 = ORIENTED_EDGE ( 'NONE', *, *, #38715, .F. ) ;
#15382 = ORIENTED_EDGE ( 'NONE', *, *, #26575, .T. ) ;
#15381 = DIRECTION ( 'NONE',  ( -0.3479852726768751237, 0.000000000000000000, -0.9375000000000004441 ) ) ;
#15383 = EDGE_CURVE ( 'NONE', #19227, #51892, #7489, .T. ) ;
#15384 = CARTESIAN_POINT ( 'NONE',  ( 41.09999999999999432, 13.66939075806899950, 20.80000000000000426 ) ) ;
#15385 = LINE ( 'NONE', #63117, #5194 ) ;
#15386 = DIRECTION ( 'NONE',  ( 0.000000000000000000, 0.000000000000000000, 1.000000000000000000 ) ) ;
#15387 = ORIENTED_EDGE ( 'NONE', *, *, #69626, .T. ) ;
#15388 = VECTOR ( 'NONE', #2992, 1000.000000000000114 ) ;
#15389 = DIRECTION ( 'NONE',  ( -0.000000000000000000, 3.673940397442059868E-16, -1.000000000000000000 ) ) ;
#15390 = DIRECTION ( 'NONE',  ( -0.000000000000000000, 3.673940397442059868E-16, -1.000000000000000000 ) ) ;
#15391 = AXIS2_PLACEMENT_3D ( 'NONE', #60673, #45092, #67715 ) ;
#15392 = ORIENTED_EDGE ( 'NONE', *, *, #41599, .T. ) ;
#15393 = VERTEX_POINT ( 'NONE', #67157 ) ;
#15394 = AXIS2_PLACEMENT_3D ( 'NONE', #40482, #35167, #62751 ) ;
#15395 = ORIENTED_EDGE ( 'NONE', *, *, #19846, .T. ) ;
#15396 = LINE ( 'NONE', #36603, #44433 ) ;
#15397 = DIRECTION ( 'NONE',  ( 0.000000000000000000, 0.000000000000000000, 1.000000000000000000 ) ) ;
#15398 = DIRECTION ( 'NONE',  ( -1.000000000000000000, 0.000000000000000000, 0.000000000000000000 ) ) ;
#15399 = VECTOR ( 'NONE', #12715, 1000.000000000000000 ) ;
#15400 = VECTOR ( 'NONE', #69689, 999.9999999999998863 ) ;
#15401 = ORIENTED_EDGE ( 'NONE', *, *, #46515, .F. ) ;
#15402 = ORIENTED_EDGE ( 'NONE', *, *, #815, .F. ) ;
#15403 = LINE ( 'NONE', #3736, #28263 ) ;
#15404 = CIRCLE ( 'NONE', #63964, 0.1749999999999998224 ) ;
#15405 = VECTOR ( 'NONE', #25572, 1000.000000000000000 ) ;
#15406 = AXIS2_PLACEMENT_3D ( 'NONE', #21908, #48789, #10601 ) ;
#15407 = ORIENTED_EDGE ( 'NONE', *, *, #44659, .F. ) ;
#15408 = EDGE_LOOP ( 'NONE', ( #46697, #25665, #57490, #42571 ) ) ;
#15409 = ADVANCED_FACE ( 'NONE', ( #45944 ), #18718, .T. ) ;
#15410 = ORIENTED_EDGE ( 'NONE', *, *, #25409, .F. ) ;
#15411 = ORIENTED_EDGE ( 'NONE', *, *, #51764, .F. ) ;
#15412 = AXIS2_PLACEMENT_3D ( 'NONE', #42972, #33056, #10790 ) ;
#15413 = LINE ( 'NONE', #53944, #36100 ) ;
#15414 = UNCERTAINTY_MEASURE_WITH_UNIT (LENGTH_MEASURE( 1.000000000000000082E-05 ), #53713, 'distance_accuracy_value', 'NONE');
#15416 = ORIENTED_EDGE ( 'NONE', *, *, #38619, .F. ) ;
#15415 = DIRECTION ( 'NONE',  ( 0.000000000000000000, 0.7096009616570518874, -0.7046037717862339012 ) ) ;
#15417 = CARTESIAN_POINT ( 'NONE',  ( -7.250000000000000888, 7.450000000000003730, -9.000000000000001776 ) ) ;
#15418 = VECTOR ( 'NONE', #23595, 1000.000000000000000 ) ;
#15419 = CARTESIAN_POINT ( 'NONE',  ( -9.942044687070568543, 9.234937905883914055, 455.0000000000000568 ) ) ;
#15420 = CARTESIAN_POINT ( 'NONE',  ( 28.00000000000000000, -17.35230188589299516, -15.35019951917100478 ) ) ;
#15421 = EDGE_LOOP ( 'NONE', ( #60687, #54626, #69198, #2256 ) ) ;
#15422 = ORIENTED_EDGE ( 'NONE', *, *, #64991, .F. ) ;
#15423 = EDGE_CURVE ( 'NONE', #57811, #58579, #40287, .T. ) ;
#15424 = LINE ( 'NONE', #37683, #25550 ) ;
#15425 = EDGE_CURVE ( 'NONE', #49993, #16188, #30028, .T. ) ;
#15426 = DIRECTION ( 'NONE',  ( 0.000000000000000000, 0.000000000000000000, 1.000000000000000000 ) ) ;
#15427 = ORIENTED_EDGE ( 'NONE', *, *, #7771, .T. ) ;
#15428 = DIRECTION ( 'NONE',  ( -0.000000000000000000, -0.000000000000000000, -1.000000000000000000 ) ) ;
#15429 = STYLED_ITEM ( 'NONE', ( #64157 ), #19898 ) ;
#15430 = DIRECTION ( 'NONE',  ( -1.000000000000000000, 0.000000000000000000, 0.000000000000000000 ) ) ;
#15431 = ORIENTED_EDGE ( 'NONE', *, *, #53991, .F. ) ;
#15432 = DIRECTION ( 'NONE',  ( 1.000000000000000000, -0.000000000000000000, -0.000000000000000000 ) ) ;
#15433 = CARTESIAN_POINT ( 'NONE',  ( 7.250000000000005329, 8.250000000000001776, -16.50000000000000000 ) ) ;
#15434 = DIRECTION ( 'NONE',  ( 1.000000000000000000, -0.000000000000000000, 0.000000000000000000 ) ) ;
#15435 = VECTOR ( 'NONE', #67990, 1000.000000000000000 ) ;
#15436 = CARTESIAN_POINT ( 'NONE',  ( -10.30047626211724854, -3.664523737882715348, 54.00000000000000711 ) ) ;
#15437 = CIRCLE ( 'NONE', #67367, 1.929199999999998028 ) ;
#15438 = AXIS2_PLACEMENT_3D ( 'NONE', #42107, #8880, #30454 ) ;
#15439 = DIRECTION ( 'NONE',  ( 1.047444401652940007E-14, 1.000000000000000000, 1.836970198721029934E-16 ) ) ;
#15440 = EDGE_LOOP ( 'NONE', ( #58573, #30053, #54179, #63054 ) ) ;
#15441 = CARTESIAN_POINT ( 'NONE',  ( 0.000000000000000000, 8.250000000000001776, -23.00000000000000000 ) ) ;
#15442 = LINE ( 'NONE', #37023, #60 ) ;
#15443 = SURFACE_STYLE_USAGE ( .BOTH. , #37703 ) ;
#15444 = CARTESIAN_POINT ( 'NONE',  ( 1.634292677759859869, -8.241237374594282628, 54.00000000000000711 ) ) ;
#15445 = EDGE_CURVE ( 'NONE', #50590, #64280, #24380, .T. ) ;
#15446 = VECTOR ( 'NONE', #6580, 1000.000000000000000 ) ;
#15447 = VECTOR ( 'NONE', #5968, 1000.000000000000000 ) ;
#15448 = AXIS2_PLACEMENT_3D ( 'NONE', #61467, #28264, #50176 ) ;
#15449 = EDGE_CURVE ( 'NONE', #7103, #30626, #39143, .T. ) ;
#15450 = VERTEX_POINT ( 'NONE', #28629 ) ;
#15451 = LINE ( 'NONE', #41610, #10059 ) ;
#15452 = EDGE_CURVE ( 'NONE', #7881, #22866, #40638, .T. ) ;
#15453 = DIRECTION ( 'NONE',  ( -0.5773502691896270633, -0.5773502691896270633, 0.5773502691896230665 ) ) ;
#15454 = VECTOR ( 'NONE', #53792, 1000.000000000000000 ) ;
#15455 = CARTESIAN_POINT ( 'NONE',  ( 47.00000000000000000, 0.7500000000000000000, -4.943429983321300014 ) ) ;
#15456 = AXIS2_PLACEMENT_3D ( 'NONE', #2680, #56084, #44757 ) ;
#15457 = DIRECTION ( 'NONE',  ( -4.956352788505168198E-15, -1.000000000000000000, 0.000000000000000000 ) ) ;
#15458 = VERTEX_POINT ( 'NONE', #29318 ) ;
#15459 = CARTESIAN_POINT ( 'NONE',  ( 7.250000000000005329, -8.249999999999998224, -26.00000000000001066 ) ) ;
#15460 = DIRECTION ( 'NONE',  ( -1.000000000000000000, 0.000000000000000000, 0.000000000000000000 ) ) ;
#15461 = EDGE_CURVE ( 'NONE', #24433, #27223, #52671, .T. ) ;
#15462 = LINE ( 'NONE', #16496, #42440 ) ;
#15463 = AXIS2_PLACEMENT_3D ( 'NONE', #21249, #15604, #26546 ) ;
#15464 = LINE ( 'NONE', #21798, #22001 ) ;
#15465 = SURFACE_STYLE_FILL_AREA ( #47977 ) ;
#15466 = EDGE_CURVE ( 'NONE', #67361, #41194, #63622, .T. ) ;
#15467 = CYLINDRICAL_SURFACE ( 'NONE', #54310, 24.99999999998789946 ) ;
#15468 = ORIENTED_EDGE ( 'NONE', *, *, #53616, .T. ) ;
#15469 = EDGE_CURVE ( 'NONE', #12841, #58919, #62912, .T. ) ;
#15470 = VECTOR ( 'NONE', #53098, 1000.000000000000000 ) ;
#15471 = ORIENTED_EDGE ( 'NONE', *, *, #12596, .T. ) ;
#15472 = CARTESIAN_POINT ( 'NONE',  ( 49.00000000000000000, -0.2000000000089119934, 8.909539772616881237E-12 ) ) ;
#15473 = CARTESIAN_POINT ( 'NONE',  ( 169.1780563256071446, -33.83962462487175316, 0.000000000000000000 ) ) ;
#15474 = ORIENTED_EDGE ( 'NONE', *, *, #34639, .T. ) ;
#15475 = CARTESIAN_POINT ( 'NONE',  ( -7.603567055985589462, -8.606483450353362485, 195.0000000000000284 ) ) ;
#15476 = CARTESIAN_POINT ( 'NONE',  ( 10.62249899919925866, -21.00000000000000000, -17.50000000000000000 ) ) ;
#15477 = ADVANCED_FACE ( 'NONE', ( #14476 ), #30735, .F. ) ;
#15478 = ORIENTED_EDGE ( 'NONE', *, *, #35522, .T. ) ;
#15479 = LINE ( 'NONE', #52610, #32257 ) ;
#15480 = ORIENTED_EDGE ( 'NONE', *, *, #52193, .T. ) ;
#15481 = ORIENTED_EDGE ( 'NONE', *, *, #16645, .F. ) ;
#15482 = LINE ( 'NONE', #27125, #15956 ) ;
#15483 = VERTEX_POINT ( 'NONE', #47344 ) ;
#15484 = DIRECTION ( 'NONE',  ( -0.000000000000000000, -0.000000000000000000, 1.000000000000000000 ) ) ;
#15485 = DIRECTION ( 'NONE',  ( 0.000000000000000000, 1.000000000000000000, 3.673940397442059868E-16 ) ) ;
#15486 = CARTESIAN_POINT ( 'NONE',  ( 11.00000000000000000, -10.85999999999999943, -9.350000000000269651 ) ) ;
#15487 = EDGE_CURVE ( 'NONE', #69903, #48157, #20473, .T. ) ;
#15488 = CIRCLE ( 'NONE', #39136, 4.000000000000000888 ) ;
#15489 = ORIENTED_EDGE ( 'NONE', *, *, #40632, .T. ) ;
#15490 = VERTEX_POINT ( 'NONE', #57602 ) ;
#15491 = CARTESIAN_POINT ( 'NONE',  ( 10.74648345035335240, 1.677516549646529409, 455.0000000000000568 ) ) ;
#15493 = CARTESIAN_POINT ( 'NONE',  ( 7.000000000000000000, -53.81370849898476649, -16.03137303340311348 ) ) ;
#15492 = CARTESIAN_POINT ( 'NONE',  ( 15.00000000000000000, -26.42999999999999972, 9.412893218813501051 ) ) ;
#15494 = EDGE_LOOP ( 'NONE', ( #62575, #38516, #35904, #47473 ) ) ;
#15495 = ORIENTED_EDGE ( 'NONE', *, *, #15903, .F. ) ;
#15496 = EDGE_CURVE ( 'NONE', #38093, #69064, #3168, .T. ) ;
#15497 = VERTEX_POINT ( 'NONE', #37100 ) ;
#15498 = AXIS2_PLACEMENT_3D ( 'NONE', #2715, #34880, #23936 ) ;
#15499 = AXIS2_PLACEMENT_3D ( 'NONE', #44435, #50791, #61387 ) ;
#15500 = CARTESIAN_POINT ( 'NONE',  ( 30.00000000000000000, -5.599999999999999645, 27.00000000000000000 ) ) ;
#15502 = ORIENTED_EDGE ( 'NONE', *, *, #42629, .T. ) ;
#15501 = CARTESIAN_POINT ( 'NONE',  ( -9.690000000000001279, -9.750000000000001776, -7.000000000000000000 ) ) ;
#15503 = EDGE_CURVE ( 'NONE', #10975, #49352, #46287, .T. ) ;
#15504 = AXIS2_PLACEMENT_3D ( 'NONE', #6143, #22746, #44301 ) ;
#15505 = CIRCLE ( 'NONE', #32463, 4.000000000000000888 ) ;
#15506 = LINE ( 'NONE', #37074, #45771 ) ;
#15507 = FACE_OUTER_BOUND ( 'NONE', #37058, .T. ) ;
#15508 = AXIS2_PLACEMENT_3D ( 'NONE', #47481, #9307, #15665 ) ;
#15509 = EDGE_LOOP ( 'NONE', ( #39746, #57757, #9966, #39003, #10101, #23207, #63902 ) ) ;
#15510 = ORIENTED_EDGE ( 'NONE', *, *, #18524, .F. ) ;
#15511 = EDGE_CURVE ( 'NONE', #51738, #33976, #25593, .T. ) ;
#15512 = AXIS2_PLACEMENT_3D ( 'NONE', #57853, #56453, #64913 ) ;
#15513 = VECTOR ( 'NONE', #1, 1000.000000000000000 ) ;
#15514 = CARTESIAN_POINT ( 'NONE',  ( 2.706483450353343478, -10.92648345035336632, 195.0000000000000284 ) ) ;
#15515 = ORIENTED_EDGE ( 'NONE', *, *, #43543, .F. ) ;
#15516 = CARTESIAN_POINT ( 'NONE',  ( 14.50000000000000711, -42.00000000000000000, 27.00000000000000355 ) ) ;
#15517 = LINE ( 'NONE', #10197, #62894 ) ;
#15518 = ADVANCED_FACE ( 'NONE', ( #30384 ), #31091, .F. ) ;
#15519 = CARTESIAN_POINT ( 'NONE',  ( 15.50000000000129852, -17.50000000000000000, -22.50000000000000000 ) ) ;
#15520 = ORIENTED_EDGE ( 'NONE', *, *, #43110, .F. ) ;
#15521 = AXIS2_PLACEMENT_3D ( 'NONE', #43505, #48831, #11325 ) ;
#15522 = DIRECTION ( 'NONE',  ( -1.000000000000000000, 0.000000000000000000, 0.000000000000000000 ) ) ;
#15523 = EDGE_CURVE ( 'NONE', #13194, #65447, #52305, .T. ) ;
#15525 = VERTEX_POINT ( 'NONE', #3867 ) ;
#15524 = DIRECTION ( 'NONE',  ( -0.7071067811865474617, -0.7071067811865474617, 0.000000000000000000 ) ) ;
#15527 = ORIENTED_EDGE ( 'NONE', *, *, #66179, .F. ) ;
#15526 = LINE ( 'NONE', #42375, #33214 ) ;
#15528 = EDGE_CURVE ( 'NONE', #44833, #53484, #57950, .T. ) ;
#15529 = CARTESIAN_POINT ( 'NONE',  ( 6.358413763958968623, -4.720772854004779973, 26.00000000000000711 ) ) ;
#15530 = CARTESIAN_POINT ( 'NONE',  ( -5.242976262117280406, -5.257023737882805747, 54.00000000000000711 ) ) ;
#15531 = EDGE_CURVE ( 'NONE', #62094, #44371, #41685, .T. ) ;
#15532 = LINE ( 'NONE', #4911, #43724 ) ;
#15533 = EDGE_CURVE ( 'NONE', #14243, #2424, #4573, .T. ) ;
#15534 = EDGE_CURVE ( 'NONE', #187, #20252, #10217, .T. ) ;
#15535 = CARTESIAN_POINT ( 'NONE',  ( 30.00000000000000000, -16.28999999999999915, 14.50000000000000000 ) ) ;
#15536 = DIRECTION ( 'NONE',  ( 0.4998444328988824181, 0.000000000000000000, -0.8661152018640445593 ) ) ;
#15537 = VERTEX_POINT ( 'NONE', #15179 ) ;
#15538 = DIRECTION ( 'NONE',  ( -1.000000000000000000, 0.000000000000000000, 0.000000000000000000 ) ) ;
#15539 = CARTESIAN_POINT ( 'NONE',  ( 46.39999999999999858, 21.00000000000000000, 0.7500000000000000000 ) ) ;
#15540 = EDGE_CURVE ( 'NONE', #49641, #53142, #57252, .T. ) ;
#15541 = FACE_OUTER_BOUND ( 'NONE', #5100, .T. ) ;
#15543 = ORIENTED_EDGE ( 'NONE', *, *, #60603, .F. ) ;
#15542 = CARTESIAN_POINT ( 'NONE',  ( 41.09999999999999432, -14.06939075806901940, -20.80000000000000426 ) ) ;
#15544 = CARTESIAN_POINT ( 'NONE',  ( 30.00000000000000000, -12.00000000000000000, -12.20000000000000107 ) ) ;
#15545 = ADVANCED_FACE ( 'NONE', ( #9881 ), #47695, .F. ) ;
#15546 = AXIS2_PLACEMENT_3D ( 'NONE', #26145, #47700, #57608 ) ;
#15547 = LINE ( 'NONE', #48402, #25813 ) ;
#15548 = DIRECTION ( 'NONE',  ( -0.000000000000000000, -0.000000000000000000, -1.000000000000000000 ) ) ;
#15549 = ADVANCED_FACE ( 'NONE', ( #69265 ), #25085, .F. ) ;
#15550 = CARTESIAN_POINT ( 'NONE',  ( 283.0000000000000568, -30.80000000000000071, 8.900000000000000355 ) ) ;
#15551 = ORIENTED_EDGE ( 'NONE', *, *, #7950, .F. ) ;
#15552 = CARTESIAN_POINT ( 'NONE',  ( -9.722976262117221324, -2.544523737882721015, 26.00000000000000711 ) ) ;
#15553 = FACE_OUTER_BOUND ( 'NONE', #50002, .T. ) ;
#15554 = ORIENTED_EDGE ( 'NONE', *, *, #463, .F. ) ;
#15555 = DIRECTION ( 'NONE',  ( 0.000000000000000000, 1.000000000000000000, 0.000000000000000000 ) ) ;
#15556 = CARTESIAN_POINT ( 'NONE',  ( -25.50000000000000355, -15.50000000000000000, 20.49999999999999645 ) ) ;
#15557 = CIRCLE ( 'NONE', #68589, 1.399999999999999245 ) ;
#15558 = DIRECTION ( 'NONE',  ( -0.4999999999999832356, 0.000000000000000000, 0.8660254037844483666 ) ) ;
#15559 = ADVANCED_FACE ( 'NONE', ( #53362 ), #54398, .F. ) ;
#15560 = LINE ( 'NONE', #37120, #27154 ) ;
#15561 = EDGE_CURVE ( 'NONE', #19581, #44397, #43421, .T. ) ;
#15562 = VECTOR ( 'NONE', #58773, 1000.000000000000000 ) ;
#15564 = CARTESIAN_POINT ( 'NONE',  ( 4.456444791733522252E-16, 7.450000000000002842, -9.500000000000001776 ) ) ;
#15563 = CIRCLE ( 'NONE', #6516, 0.1999999999999987899 ) ;
#15565 = VERTEX_POINT ( 'NONE', #37786 ) ;
#15566 = ORIENTED_EDGE ( 'NONE', *, *, #62649, .T. ) ;
#15567 = PLANE ( 'NONE',  #46468 ) ;
#15568 = ORIENTED_EDGE ( 'NONE', *, *, #19802, .T. ) ;
#15569 = ORIENTED_EDGE ( 'NONE', *, *, #23491, .T. ) ;
#15570 = DIRECTION ( 'NONE',  ( 0.7071067811865441310, -0.7071067811865510144, -2.597868168706485034E-16 ) ) ;
#15571 = CIRCLE ( 'NONE', #13307, 4.500000000000191847 ) ;
#15572 = VECTOR ( 'NONE', #37055, 1000.000000000000000 ) ;
#15573 = CARTESIAN_POINT ( 'NONE',  ( 21.90000000000000213, 20.60000000000000142, 13.86939075806899702 ) ) ;
#15574 = CARTESIAN_POINT ( 'NONE',  ( 11.50000000000000000, -11.50000000000000000, 15.00000000000000000 ) ) ;
#15575 = ORIENTED_EDGE ( 'NONE', *, *, #53138, .T. ) ;
#15576 = VERTEX_POINT ( 'NONE', #59001 ) ;
#15577 = CYLINDRICAL_SURFACE ( 'NONE', #18293, 1.000000000000000000 ) ;
#15578 = ORIENTED_EDGE ( 'NONE', *, *, #41468, .T. ) ;
#15579 = ORIENTED_EDGE ( 'NONE', *, *, #38462, .T. ) ;
#15580 = VECTOR ( 'NONE', #52204, 1000.000000000000000 ) ;
#15581 = CARTESIAN_POINT ( 'NONE',  ( -7.450000000000001954, 7.250000000000000000, -11.00000000000000000 ) ) ;
#15582 = CARTESIAN_POINT ( 'NONE',  ( 283.0000000000000568, -30.45000000000000639, 15.00000000000000000 ) ) ;
#15583 = CARTESIAN_POINT ( 'NONE',  ( 14.89999999999999680, -0.2000000000089119934, 8.909539772616881237E-12 ) ) ;
#15584 = ORIENTED_EDGE ( 'NONE', *, *, #3509, .T. ) ;
#15585 = CARTESIAN_POINT ( 'NONE',  ( 30.00000000000000000, -5.599999999999379696, 26.60000000000059828 ) ) ;
#15587 = CARTESIAN_POINT ( 'NONE',  ( 11.19000000000000128, -11.25000000000000000, -4.250000000000000000 ) ) ;
#15586 = CARTESIAN_POINT ( 'NONE',  ( 40.90000000000000568, 0.000000000000000000, 3.447897592003593022E-15 ) ) ;
#15588 = ORIENTED_EDGE ( 'NONE', *, *, #68324, .F. ) ;
#15590 = ORIENTED_EDGE ( 'NONE', *, *, #63017, .T. ) ;
#15589 = CARTESIAN_POINT ( 'NONE',  ( 5.257023737882798642, 6.467976262117203667, 26.00000000000000711 ) ) ;
#15591 = EDGE_LOOP ( 'NONE', ( #67673, #12806, #20218, #29618 ) ) ;
#15592 = ADVANCED_FACE ( 'NONE', ( #22561 ), #26837, .F. ) ;
#15593 = LINE ( 'NONE', #65066, #6201 ) ;
#15594 = EDGE_CURVE ( 'NONE', #11358, #27679, #302, .T. ) ;
#15595 = CARTESIAN_POINT ( 'NONE',  ( -8.250000000000001776, -7.249999999999998224, -26.00000000000001066 ) ) ;
#15596 = ORIENTED_EDGE ( 'NONE', *, *, #8172, .F. ) ;
#15597 = EDGE_CURVE ( 'NONE', #22670, #32725, #5273, .T. ) ;
#15598 = FACE_OUTER_BOUND ( 'NONE', #63323, .T. ) ;
#15599 = ADVANCED_FACE ( 'NONE', ( #69623 ), #11925, .F. ) ;
#15600 = LINE ( 'NONE', #31855, #13097 ) ;
#15601 = VERTEX_POINT ( 'NONE', #32819 ) ;
#15602 = ORIENTED_EDGE ( 'NONE', *, *, #3659, .T. ) ;
#15603 = CARTESIAN_POINT ( 'NONE',  ( 4.456444791733522252E-16, 7.450000000000002842, -19.50000000000000000 ) ) ;
#15604 = DIRECTION ( 'NONE',  ( -1.000000000000000000, 0.000000000000000000, 0.000000000000000000 ) ) ;
#15605 = ADVANCED_FACE ( 'NONE', ( #10559 ), #5611, .F. ) ;
#15606 = CARTESIAN_POINT ( 'NONE',  ( -9.791916549646819234, -11.08848345035330496, 195.0000000000000284 ) ) ;
#15607 = EDGE_LOOP ( 'NONE', ( #50161, #47400 ) ) ;
#15608 = DIRECTION ( 'NONE',  ( 1.836970198721029934E-16, 1.836970198721010706E-16, -1.000000000000000000 ) ) ;
#15609 = FACE_OUTER_BOUND ( 'NONE', #14900, .T. ) ;
#15611 = ORIENTED_EDGE ( 'NONE', *, *, #44869, .F. ) ;
#15610 = LINE ( 'NONE', #22297, #61126 ) ;
#15613 = VERTEX_POINT ( 'NONE', #5950 ) ;
#15612 = DIRECTION ( 'NONE',  ( -1.000000000000000000, 0.000000000000000000, 0.000000000000000000 ) ) ;
#15614 = DIRECTION ( 'NONE',  ( 0.000000000000000000, 1.000000000000000000, 0.000000000000000000 ) ) ;
#15615 = AXIS2_PLACEMENT_3D ( 'NONE', #61848, #34955, #19058 ) ;
#15616 = DIRECTION ( 'NONE',  ( -1.000000000000000000, 3.903627567395476653E-15, 1.836970198721037083E-16 ) ) ;
#15617 = CARTESIAN_POINT ( 'NONE',  ( 280.0000000000000000, -20.40000000000000213, -20.00000000000000000 ) ) ;
#15618 = CARTESIAN_POINT ( 'NONE',  ( 46.39999999999999858, 21.00000000000000000, 2.750000000000000444 ) ) ;
#15619 = EDGE_CURVE ( 'NONE', #19590, #24664, #22221, .T. ) ;
#15620 = LINE ( 'NONE', #48833, #58774 ) ;
#15621 = CARTESIAN_POINT ( 'NONE',  ( 9.562023737882812569, -8.144523737882813919, 26.00000000000000000 ) ) ;
#15622 = VERTEX_POINT ( 'NONE', #32131 ) ;
#15623 = FACE_OUTER_BOUND ( 'NONE', #51386, .T. ) ;
#15624 = EDGE_LOOP ( 'NONE', ( #1791, #36698, #7118, #52714 ) ) ;
#15625 = AXIS2_PLACEMENT_3D ( 'NONE', #9708, #30914, #14309 ) ;
#15626 = DIRECTION ( 'NONE',  ( 0.000000000000000000, 0.000000000000000000, 1.000000000000000000 ) ) ;
#15627 = CARTESIAN_POINT ( 'NONE',  ( 11.48848345035334617, -11.08848345035339733, 195.0000000000000284 ) ) ;
#15628 = DIRECTION ( 'NONE',  ( 0.000000000000000000, 0.000000000000000000, -1.000000000000000000 ) ) ;
#15629 = ORIENTED_EDGE ( 'NONE', *, *, #41885, .F. ) ;
#15630 = CARTESIAN_POINT ( 'NONE',  ( 24.90000000000000213, -0.2000000000089119934, -8.913009219568841313E-12 ) ) ;
#15631 = DIRECTION ( 'NONE',  ( 1.000000000000000000, -0.000000000000000000, 0.000000000000000000 ) ) ;
#15632 = ORIENTED_EDGE ( 'NONE', *, *, #38201, .F. ) ;
#15633 = CARTESIAN_POINT ( 'NONE',  ( -7.250000000000000888, 8.250000000000001776, -16.50000000000000000 ) ) ;
#15634 = DIRECTION ( 'NONE',  ( 2.309061475090597584E-14, 1.000000000000000000, 1.836970198721053107E-16 ) ) ;
#15635 = ADVANCED_FACE ( 'NONE', ( #43782 ), #65354, .F. ) ;
#15636 = EDGE_CURVE ( 'NONE', #34243, #18370, #26480, .T. ) ;
#15637 = DIRECTION ( 'NONE',  ( -1.000000000000000000, 0.000000000000000000, 0.000000000000000000 ) ) ;
#15638 = ORIENTED_EDGE ( 'NONE', *, *, #67464, .F. ) ;
#15639 = DIRECTION ( 'NONE',  ( 1.000000000000000000, 0.000000000000000000, 0.000000000000000000 ) ) ;
#15640 = ORIENTED_EDGE ( 'NONE', *, *, #54318, .F. ) ;
#15641 = EDGE_LOOP ( 'NONE', ( #37478, #9410, #27827, #39628 ) ) ;
#15642 = CARTESIAN_POINT ( 'NONE',  ( 8.211283450353352720, 5.993516549646621172, 195.0000000000000284 ) ) ;
#15643 = LINE ( 'NONE', #59808, #18416 ) ;
#15644 = LINE ( 'NONE', #5731, #67118 ) ;
#15645 = CARTESIAN_POINT ( 'NONE',  ( -30.00000000000000000, -8.959999999999999076, 17.04524521594300523 ) ) ;
#15646 = ORIENTED_EDGE ( 'NONE', *, *, #59666, .T. ) ;
#15647 = VERTEX_POINT ( 'NONE', #69958 ) ;
#15649 = ORIENTED_EDGE ( 'NONE', *, *, #4465, .F. ) ;
#15648 = LINE ( 'NONE', #48865, #32913 ) ;
#15650 = VERTEX_POINT ( 'NONE', #44115 ) ;
#15651 = CIRCLE ( 'NONE', #55155, 0.1999999999999987899 ) ;
#15652 = DIRECTION ( 'NONE',  ( 0.000000000000000000, 1.000000000000000000, 0.000000000000000000 ) ) ;
#15653 = LINE ( 'NONE', #58077, #55767 ) ;
#15654 = DIRECTION ( 'NONE',  ( -1.000000000000000000, 1.185108578570163402E-14, 1.836970198721051628E-16 ) ) ;
#15655 = VECTOR ( 'NONE', #45053, 1000.000000000000000 ) ;
#15656 = DIRECTION ( 'NONE',  ( 0.000000000000000000, -0.7046037717859411353, -0.7096009616573427659 ) ) ;
#15658 = DIRECTION ( 'NONE',  ( 1.047444401652939849E-14, 1.000000000000000000, 1.836970198721029934E-16 ) ) ;
#15657 = PLANE ( 'NONE',  #41090 ) ;
#15659 = ORIENTED_EDGE ( 'NONE', *, *, #1441, .T. ) ;
#15660 = ORIENTED_EDGE ( 'NONE', *, *, #59121, .F. ) ;
#15661 = ORIENTED_EDGE ( 'NONE', *, *, #12248, .T. ) ;
#15662 = ORIENTED_EDGE ( 'NONE', *, *, #22049, .F. ) ;
#15663 = DIRECTION ( 'NONE',  ( 1.000000000000000000, 0.000000000000000000, 0.000000000000000000 ) ) ;
#15664 = PLANE ( 'NONE',  #7237 ) ;
#15665 = DIRECTION ( 'NONE',  ( -1.000000000000000000, 1.088018564132653410E-14, -1.768243044173057712E-18 ) ) ;
#15666 = AXIS2_PLACEMENT_3D ( 'NONE', #55949, #66219, #17778 ) ;
#15667 = EDGE_CURVE ( 'NONE', #48443, #9530, #22252, .T. ) ;
#15668 = CARTESIAN_POINT ( 'NONE',  ( 10.50702373788278265, 3.650476262117142934, 54.00000000000000711 ) ) ;
#15669 = ORIENTED_EDGE ( 'NONE', *, *, #14642, .T. ) ;
#15670 = VERTEX_POINT ( 'NONE', #48740 ) ;
#15671 = VERTEX_POINT ( 'NONE', #49442 ) ;
#15672 = EDGE_CURVE ( 'NONE', #51391, #5551, #3066, .T. ) ;
#15673 = CARTESIAN_POINT ( 'NONE',  ( 7.000000000000000000, -31.99999999999889866, -7.899999999997660893 ) ) ;
#15674 = ORIENTED_EDGE ( 'NONE', *, *, #35566, .F. ) ;
#15675 = EDGE_CURVE ( 'NONE', #36429, #59980, #817, .T. ) ;
#15676 = LINE ( 'NONE', #31251, #27704 ) ;
#15677 = EDGE_CURVE ( 'NONE', #31474, #59188, #27868, .T. ) ;
#15678 = ORIENTED_EDGE ( 'NONE', *, *, #3927, .F. ) ;
#15679 = VERTEX_POINT ( 'NONE', #21182 ) ;
#15680 = CARTESIAN_POINT ( 'NONE',  ( 9.417013320880721849, 1.853252480934663771, 195.0000000000000284 ) ) ;
#15681 = ADVANCED_FACE ( 'NONE', ( #64649 ), #10911, .F. ) ;
#15682 = ADVANCED_FACE ( 'NONE', ( #40545 ), #44451, .F. ) ;
#15684 = ORIENTED_EDGE ( 'NONE', *, *, #65886, .F. ) ;
#15683 = DIRECTION ( 'NONE',  ( 1.000000000000000000, -0.000000000000000000, 0.000000000000000000 ) ) ;
#15685 = VERTEX_POINT ( 'NONE', #40192 ) ;
#15686 = DIRECTION ( 'NONE',  ( 0.000000000000000000, 1.000000000000000000, 0.000000000000000000 ) ) ;
#15687 = EDGE_CURVE ( 'NONE', #12012, #58158, #6455, .T. ) ;
#15688 = CARTESIAN_POINT ( 'NONE',  ( 7.000000000000000000, -25.93000000000544958, 9.412893218815410634 ) ) ;
#15690 = EDGE_LOOP ( 'NONE', ( #47157, #59496, #46745, #52179 ) ) ;
#15689 = DIRECTION ( 'NONE',  ( -1.836970198721029934E-16, -1.836970198721010706E-16, 1.000000000000000000 ) ) ;
#15691 = ORIENTED_EDGE ( 'NONE', *, *, #57755, .F. ) ;
#15692 = CARTESIAN_POINT ( 'NONE',  ( 6.849523737882818430, 10.49297626211719603, 54.00000000000000711 ) ) ;
#15693 = CARTESIAN_POINT ( 'NONE',  ( 9.795823737882805915, -9.795823737882811244, 54.00000000000000711 ) ) ;
#15694 = CARTESIAN_POINT ( 'NONE',  ( -30.00000000000000000, -11.50000000000082068, 10.20500000000000007 ) ) ;
#15695 = PLANE ( 'NONE',  #719 ) ;
#15696 = AXIS2_PLACEMENT_3D ( 'NONE', #39456, #56419, #61014 ) ;
#15697 = DIRECTION ( 'NONE',  ( 1.000000000000000000, 0.000000000000000000, 0.000000000000000000 ) ) ;
#15698 = ORIENTED_EDGE ( 'NONE', *, *, #33375, .F. ) ;
#15699 = CARTESIAN_POINT ( 'NONE',  ( -9.249999999999998224, -7.848062532927998269, -5.000000000000000000 ) ) ;
#15700 = CIRCLE ( 'NONE', #24713, 0.2000000000000005107 ) ;
#15701 = ORIENTED_EDGE ( 'NONE', *, *, #13497, .F. ) ;
#15702 = DIRECTION ( 'NONE',  ( -0.1289152302546202611, 1.578756240926647408E-17, 0.9916556173432378163 ) ) ;
#15703 = CARTESIAN_POINT ( 'NONE',  ( 16.75000000000000000, -0.2038245569916320166, 21.77831216351300014 ) ) ;
#15704 = CARTESIAN_POINT ( 'NONE',  ( -8.250000000000001776, -7.249999999999998224, -16.00000000000000000 ) ) ;
#15705 = LINE ( 'NONE', #48232, #34004 ) ;
#15706 = VECTOR ( 'NONE', #28037, 1000.000000000000000 ) ;
#15707 = CARTESIAN_POINT ( 'NONE',  ( -1.620245201994301665, 8.227189898828640935, 54.00000000000000711 ) ) ;
#15708 = ORIENTED_EDGE ( 'NONE', *, *, #8069, .T. ) ;
#15709 = DIRECTION ( 'NONE',  ( 1.836970198721029934E-16, 1.836970198721010706E-16, -1.000000000000000000 ) ) ;
#15710 = LINE ( 'NONE', #69445, #69513 ) ;
#15711 = AXIS2_PLACEMENT_3D ( 'NONE', #55775, #2721, #62112 ) ;
#15712 = EDGE_CURVE ( 'NONE', #52459, #27455, #61771, .T. ) ;
#15713 = VERTEX_POINT ( 'NONE', #23583 ) ;
#15714 = DIRECTION ( 'NONE',  ( 0.000000000000000000, 0.6801302850037830305, 0.7330912599538155217 ) ) ;
#15715 = CARTESIAN_POINT ( 'NONE',  ( 9.955011587777235604, -9.247904806590705462, 195.0000000000000284 ) ) ;
#15716 = CARTESIAN_POINT ( 'NONE',  ( 7.000000000000000000, -53.81370849898476649, 16.03137303340311348 ) ) ;
#15717 = EDGE_CURVE ( 'NONE', #52016, #42601, #12085, .T. ) ;
#15718 = EDGE_CURVE ( 'NONE', #5551, #51391, #47084, .T. ) ;
#15719 = CARTESIAN_POINT ( 'NONE',  ( -30.00000000000000000, -10.85999999999999943, -9.000000000000001776 ) ) ;
#15720 = VECTOR ( 'NONE', #15261, 1000.000000000000000 ) ;
#15721 = CARTESIAN_POINT ( 'NONE',  ( 7.250000000000005329, -7.449999999999998401, -8.500000000000000000 ) ) ;
#15722 = ORIENTED_EDGE ( 'NONE', *, *, #32760, .T. ) ;
#15723 = DIRECTION ( 'NONE',  ( -0.000000000000000000, -0.000000000000000000, -1.000000000000000000 ) ) ;
#15724 = DIRECTION ( 'NONE',  ( 0.000000000000000000, 0.000000000000000000, 1.000000000000000000 ) ) ;
#15725 = DIRECTION ( 'NONE',  ( 0.000000000000000000, 0.000000000000000000, 1.000000000000000000 ) ) ;
#15726 = EDGE_CURVE ( 'NONE', #13793, #39563, #19972, .T. ) ;
#15727 = PLANE ( 'NONE',  #56868 ) ;
#15728 = CARTESIAN_POINT ( 'NONE',  ( 283.0000000000000568, -26.42999999999999972, -9.412893218813501051 ) ) ;
#15729 = ORIENTED_EDGE ( 'NONE', *, *, #39004, .F. ) ;
#15731 = ORIENTED_EDGE ( 'NONE', *, *, #22871, .T. ) ;
#15730 = LINE ( 'NONE', #58159, #40780 ) ;
#15732 = DIRECTION ( 'NONE',  ( -1.000000000000000000, 0.000000000000000000, 0.000000000000000000 ) ) ;
#15733 = CARTESIAN_POINT ( 'NONE',  ( 15.29633693294940677, -0.2717122460100966919, -21.17420925361164308 ) ) ;
#15734 = DIRECTION ( 'NONE',  ( 8.359604446858500663E-15, 1.000000000000000000, 3.673940397442059868E-16 ) ) ;
#15735 = EDGE_LOOP ( 'NONE', ( #65059, #26731, #24282, #57485 ) ) ;
#15736 = CARTESIAN_POINT ( 'NONE',  ( -7.250000000000000888, -8.249999999999998224, -12.00000000000000000 ) ) ;
#15737 = DIRECTION ( 'NONE',  ( -1.836970198721029934E-16, 1.836970198721036344E-16, -1.000000000000000000 ) ) ;
#15738 = EDGE_LOOP ( 'NONE', ( #17632, #55378, #34630, #50602 ) ) ;
#15739 = VERTEX_POINT ( 'NONE', #33845 ) ;
#15740 = AXIS2_PLACEMENT_3D ( 'NONE', #6730, #43180, #65113 ) ;
#15741 = EDGE_LOOP ( 'NONE', ( #35224, #44170, #57479, #53587 ) ) ;
#15742 = CARTESIAN_POINT ( 'NONE',  ( -11.11351654964671098, 7.793516549646603231, 195.0000000000000284 ) ) ;
#15743 = CIRCLE ( 'NONE', #62052, 0.7112000000000124889 ) ;
#15744 = CARTESIAN_POINT ( 'NONE',  ( 10.20488345035338007, -11.48848345035349361, 455.0000000000000568 ) ) ;
#15745 = CARTESIAN_POINT ( 'NONE',  ( 9.795823737882807691, 10.49297626211718537, 54.00000000000000711 ) ) ;
#15746 = ADVANCED_FACE ( 'NONE', ( #67438 ), #24291, .F. ) ;
#15747 = EDGE_LOOP ( 'NONE', ( #48444, #37406, #19384, #19376 ) ) ;
#15748 = ORIENTED_EDGE ( 'NONE', *, *, #47671, .T. ) ;
#15749 = VECTOR ( 'NONE', #23671, 1000.000000000000000 ) ;
#15750 = CARTESIAN_POINT ( 'NONE',  ( 7.250000000000005329, 7.250000000000000888, -8.500000000000000000 ) ) ;
#15751 = EDGE_LOOP ( 'NONE', ( #31310, #24369, #10588, #56697 ) ) ;
#15752 = ORIENTED_EDGE ( 'NONE', *, *, #48964, .T. ) ;
#15753 = EDGE_LOOP ( 'NONE', ( #23271, #15870, #24233, #37132 ) ) ;
#15754 = VERTEX_POINT ( 'NONE', #45851 ) ;
#15755 = CARTESIAN_POINT ( 'NONE',  ( 22.90000000000000213, 20.60000000000000142, -13.86939075806900057 ) ) ;
#15756 = EDGE_CURVE ( 'NONE', #31741, #32653, #55771, .T. ) ;
#15758 = VERTEX_POINT ( 'NONE', #50114 ) ;
#15757 = CARTESIAN_POINT ( 'NONE',  ( -7.250000000000000000, -7.449999999999998401, -15.00000000000000000 ) ) ;
#15759 = VECTOR ( 'NONE', #61330, 1000.000000000000000 ) ;
#15760 = DIRECTION ( 'NONE',  ( 0.000000000000000000, 1.000000000000000000, -1.500535806722257514E-12 ) ) ;
#15761 = DIRECTION ( 'NONE',  ( 0.000000000000000000, 0.000000000000000000, 1.000000000000000000 ) ) ;
#15762 = EDGE_CURVE ( 'NONE', #28788, #16237, #21146, .T. ) ;
#15763 = CARTESIAN_POINT ( 'NONE',  ( 35.89999999999999858, -21.00000000000001421, -13.86939075806900945 ) ) ;
#15764 = EDGE_LOOP ( 'NONE', ( #38969, #23029, #64634, #62267 ) ) ;
#15765 = AXIS2_PLACEMENT_3D ( 'NONE', #23626, #45189, #29271 ) ;
#15766 = CARTESIAN_POINT ( 'NONE',  ( 277.3542486889354564, -25.50000000000000355, -17.00000000000000000 ) ) ;
#15767 = DIRECTION ( 'NONE',  ( 0.000000000000000000, 0.000000000000000000, 1.000000000000000000 ) ) ;
#15768 = ORIENTED_EDGE ( 'NONE', *, *, #22748, .T. ) ;
#15769 = EDGE_CURVE ( 'NONE', #56637, #37049, #50468, .T. ) ;
#15770 = CARTESIAN_POINT ( 'NONE',  ( 11.32648345035338089, 4.393516549646522051, 455.0000000000000568 ) ) ;
#15771 = DIRECTION ( 'NONE',  ( 0.000000000000000000, -3.673940397442059868E-16, 1.000000000000000000 ) ) ;
#15772 = AXIS2_PLACEMENT_3D ( 'NONE', #20525, #63317, #31851 ) ;
#15773 = CARTESIAN_POINT ( 'NONE',  ( 3.682023737882818448, 9.722976262117203561, 54.00000000000000711 ) ) ;
#15774 = ORIENTED_EDGE ( 'NONE', *, *, #40550, .T. ) ;
#15775 = DIRECTION ( 'NONE',  ( 1.836970198721029934E-16, -1.836970198721036344E-16, 1.000000000000000000 ) ) ;
#15776 = CARTESIAN_POINT ( 'NONE',  ( 0.5000000000000000000, -42.50000000000000000, -26.50000000000000000 ) ) ;
#15777 = CARTESIAN_POINT ( 'NONE',  ( 39.00000000000000000, 6.123233995736766282E-16, -5.000000000000000000 ) ) ;
#15778 = FACE_OUTER_BOUND ( 'NONE', #69135, .T. ) ;
#15779 = DIRECTION ( 'NONE',  ( -1.836970198721029934E-16, 1.836970198721036590E-16, -1.000000000000000000 ) ) ;
#15780 = VERTEX_POINT ( 'NONE', #45494 ) ;
#15781 = DIRECTION ( 'NONE',  ( -2.135044278125299371E-15, -1.000000000000000000, -3.673940397442060361E-16 ) ) ;
#15782 = LINE ( 'NONE', #10476, #18088 ) ;
#15783 = CIRCLE ( 'NONE', #25948, 4.500000000000191847 ) ;
#15784 = AXIS2_PLACEMENT_3D ( 'NONE', #11881, #11537, #22175 ) ;
#15785 = LINE ( 'NONE', #48316, #1797 ) ;
#15786 = EDGE_LOOP ( 'NONE', ( #33866, #6886, #47258, #54633 ) ) ;
#15787 = LINE ( 'NONE', #4836, #42805 ) ;
#15788 = DIRECTION ( 'NONE',  ( 0.000000000000000000, 0.000000000000000000, -1.000000000000000000 ) ) ;
#15789 = ADVANCED_FACE ( 'NONE', ( #22898 ), #55095, .F. ) ;
#15790 = AXIS2_PLACEMENT_3D ( 'NONE', #48044, #14825, #26481 ) ;
#15791 = CARTESIAN_POINT ( 'NONE',  ( -6.822336235477446387, -4.149127210878696737, 54.00000000000000711 ) ) ;
#15792 = CARTESIAN_POINT ( 'NONE',  ( 12.90000000000000213, -0.2000000000089119934, -8.913009219568841313E-12 ) ) ;
#15793 = ORIENTED_EDGE ( 'NONE', *, *, #3218, .F. ) ;
#15794 = DIRECTION ( 'NONE',  ( -1.000000000000000000, 0.000000000000000000, 0.000000000000000000 ) ) ;
#15795 = CARTESIAN_POINT ( 'NONE',  ( -8.079219948824906794, 8.697938382363059162, 54.00000000000000711 ) ) ;
#15796 = CARTESIAN_POINT ( 'NONE',  ( 4.740315990920131561, -7.811466277050838514, 455.0000000000000568 ) ) ;
#15797 = ADVANCED_FACE ( 'NONE', ( #2029 ), #39164, .F. ) ;
#15798 = VECTOR ( 'NONE', #56906, 1000.000000000000000 ) ;
#15799 = LINE ( 'NONE', #38081, #31027 ) ;
#15800 = LINE ( 'NONE', #69546, #2619 ) ;
#15801 = CARTESIAN_POINT ( 'NONE',  ( 25.50000000000000355, -5.578999999999999737, -22.50000000000000000 ) ) ;
#15802 = VERTEX_POINT ( 'NONE', #45146 ) ;
#15803 = AXIS2_PLACEMENT_3D ( 'NONE', #14573, #25186, #31209 ) ;
#15804 = B_SPLINE_CURVE_WITH_KNOTS ( 'NONE', 3,
 ( #4396, #36193, #36921, #46801, #14991, #4036 ),
 .UNSPECIFIED., .F., .F.,
 ( 4, 2, 4 ),
 ( 0.0002380763768130567115, 0.7291065797294590256, 1.457975083082104995 ),
 .UNSPECIFIED. ) ;
#15805 = VERTEX_POINT ( 'NONE', #1667 ) ;
#15806 = CARTESIAN_POINT ( 'NONE',  ( 6.836383711242975281, 4.135079735113102117, 54.00000000000000711 ) ) ;
#15807 = LINE ( 'NONE', #35974, #53698 ) ;
#15808 = EDGE_LOOP ( 'NONE', ( #38734, #25856, #35683, #32446 ) ) ;
#15809 = CARTESIAN_POINT ( 'NONE',  ( 9.306483450353379538, -10.92648345035339119, 195.0000000000000284 ) ) ;
#15810 = VECTOR ( 'NONE', #31277, 1000.000000000000000 ) ;
#15811 = DIRECTION ( 'NONE',  ( 0.000000000000000000, 1.000000000000000000, 0.000000000000000000 ) ) ;
#15812 = ORIENTED_EDGE ( 'NONE', *, *, #2909, .F. ) ;
#15813 = ADVANCED_FACE ( 'NONE', ( #66384 ), #39496, .T. ) ;
#15814 = CARTESIAN_POINT ( 'NONE',  ( -7.813516549646711162, 11.77351654964660277, 195.0000000000000284 ) ) ;
#15815 = ORIENTED_EDGE ( 'NONE', *, *, #63833, .T. ) ;
#15816 = ORIENTED_EDGE ( 'NONE', *, *, #8336, .T. ) ;
#15817 = CYLINDRICAL_SURFACE ( 'NONE', #13657, 2.458500000000000796 ) ;
#15818 = ORIENTED_EDGE ( 'NONE', *, *, #50967, .F. ) ;
#15819 = LINE ( 'NONE', #24774, #41018 ) ;
#15820 = CARTESIAN_POINT ( 'NONE',  ( -8.513516549646713116, 11.29351654964659701, 455.0000000000000568 ) ) ;
#15821 = DIRECTION ( 'NONE',  ( 1.062075597536821205E-14, 1.000000000000000000, 0.000000000000000000 ) ) ;
#15822 = ORIENTED_EDGE ( 'NONE', *, *, #58473, .T. ) ;
#15823 = ORIENTED_EDGE ( 'NONE', *, *, #63993, .T. ) ;
#15824 = DIRECTION ( 'NONE',  ( -0.4999999999989361843, 0.000000000000000000, -0.8660254037850529940 ) ) ;
#15826 = LINE ( 'NONE', #32092, #67219 ) ;
#15825 = DIRECTION ( 'NONE',  ( 0.000000000000000000, 0.000000000000000000, -1.000000000000000000 ) ) ;
#15827 = VERTEX_POINT ( 'NONE', #56123 ) ;
#15828 = VERTEX_POINT ( 'NONE', #7668 ) ;
#15830 = ORIENTED_EDGE ( 'NONE', *, *, #41450, .F. ) ;
#15829 = ITEM_DEFINED_TRANSFORMATION ( 'NONE', 'NONE', #5322,  #45918 ) ;
#15831 = DIRECTION ( 'NONE',  ( 0.000000000000000000, -1.000000000000000000, 0.000000000000000000 ) ) ;
#15832 = CIRCLE ( 'NONE', #6780, 0.2000000000000005107 ) ;
#15834 = ORIENTED_EDGE ( 'NONE', *, *, #30121, .F. ) ;
#15833 = CARTESIAN_POINT ( 'NONE',  ( -9.722976262117258628, 7.605476262117193187, 54.00000000000000711 ) ) ;
#15835 = EDGE_CURVE ( 'NONE', #62476, #28935, #29228, .T. ) ;
#15836 = CARTESIAN_POINT ( 'NONE',  ( 6.657023737882818537, -10.31452373788281207, 26.00000000000000000 ) ) ;
#15837 = AXIS2_PLACEMENT_3D ( 'NONE', #38078, #28138, #21796 ) ;
#15838 = DIRECTION ( 'NONE',  ( -0.6414496315691526895, -0.7671651518153038696, 0.000000000000000000 ) ) ;
#15839 = EDGE_CURVE ( 'NONE', #40705, #65652, #68484, .T. ) ;
#15840 = ORIENTED_EDGE ( 'NONE', *, *, #40001, .F. ) ;
#15841 = EDGE_CURVE ( 'NONE', #6549, #13178, #8731, .T. ) ;
#15842 = ORIENTED_EDGE ( 'NONE', *, *, #39443, .T. ) ;
#15843 = CIRCLE ( 'NONE', #55361, 3.500000000000000000 ) ;
#15844 = CARTESIAN_POINT ( 'NONE',  ( 0.000000000000000000, 0.000000000000000000, -17.00000000000000000 ) ) ;
#15845 = EDGE_CURVE ( 'NONE', #56572, #16440, #20731, .T. ) ;
#15846 = ORIENTED_EDGE ( 'NONE', *, *, #67229, .T. ) ;
#15847 = ADVANCED_FACE ( 'NONE', ( #52576 ), #42298, .F. ) ;
#15848 = AXIS2_PLACEMENT_3D ( 'NONE', #15111, #57532, #37376 ) ;
#15849 = LINE ( 'NONE', #57929, #30220 ) ;
#15850 = CARTESIAN_POINT ( 'NONE',  ( 13.00000000000000178, -15.50000000000000000, -14.50000000000000000 ) ) ;
#15851 = EDGE_CURVE ( 'NONE', #49922, #11420, #69709, .T. ) ;
#15852 = EDGE_CURVE ( 'NONE', #42826, #57404, #48247, .T. ) ;
#15853 = CARTESIAN_POINT ( 'NONE',  ( -3.663616288757055806, 4.135079735113128763, 54.00000000000000711 ) ) ;
#15854 = VECTOR ( 'NONE', #33052, 1000.000000000000114 ) ;
#15855 = ORIENTED_EDGE ( 'NONE', *, *, #21022, .F. ) ;
#15856 = ADVANCED_FACE ( 'NONE', ( #30301 ), #3770, .F. ) ;
#15857 = CIRCLE ( 'NONE', #64262, 4.500000000000190958 ) ;
#15858 = CARTESIAN_POINT ( 'NONE',  ( 55.00000000000000000, -21.00000000000000000, -16.96999999999999886 ) ) ;
#15859 = CARTESIAN_POINT ( 'NONE',  ( -11.50000000000000000, -12.00000000000000000, 10.69999999999999929 ) ) ;
#15861 = ORIENTED_EDGE ( 'NONE', *, *, #62189, .T. ) ;
#15860 = DIRECTION ( 'NONE',  ( -0.7071067811865475727, 0.7071067811865475727, 0.000000000000000000 ) ) ;
#15862 = VERTEX_POINT ( 'NONE', #68124 ) ;
#15863 = DIRECTION ( 'NONE',  ( -0.000000000000000000, -1.000000000000000000, -0.000000000000000000 ) ) ;
#15864 = VECTOR ( 'NONE', #65769, 1000.000000000000000 ) ;
#15865 = VECTOR ( 'NONE', #58889, 1000.000000000000000 ) ;
#15866 = LINE ( 'NONE', #69617, #53347 ) ;
#15867 = CARTESIAN_POINT ( 'NONE',  ( -7.252248008019509307, -5.393625297349935011, 455.0000000000000568 ) ) ;
#15868 = CARTESIAN_POINT ( 'NONE',  ( 8.606483450353406894, 7.603567055985405609, 455.0000000000000568 ) ) ;
#15869 = DIRECTION ( 'NONE',  ( 0.000000000000000000, 0.000000000000000000, -1.000000000000000000 ) ) ;
#15870 = ORIENTED_EDGE ( 'NONE', *, *, #6165, .T. ) ;
#15871 = DIRECTION ( 'NONE',  ( -1.000000000000000000, 0.000000000000000000, 0.000000000000000000 ) ) ;
#15872 = DIRECTION ( 'NONE',  ( 0.000000000000000000, 1.000000000000000000, -0.000000000000000000 ) ) ;
#15873 = CARTESIAN_POINT ( 'NONE',  ( -3.663616288757055806, 4.135079735113128763, 54.00000000000000711 ) ) ;
#15875 = ORIENTED_EDGE ( 'NONE', *, *, #17714, .T. ) ;
#15874 = CYLINDRICAL_SURFACE ( 'NONE', #41267, 0.1999999999999987899 ) ;
#15876 = DIRECTION ( 'NONE',  ( 0.000000000000000000, 0.000000000000000000, 1.000000000000000000 ) ) ;
#15877 = AXIS2_PLACEMENT_3D ( 'NONE', #454, #50526, #2082 ) ;
#15878 = CARTESIAN_POINT ( 'NONE',  ( 11.00000000000000000, -5.599999999999999645, 9.000000000000001776 ) ) ;
#15879 = CARTESIAN_POINT ( 'NONE',  ( 11.00000000000000000, -5.599999999999999645, -9.400000000000000355 ) ) ;
#15880 = LINE ( 'NONE', #15550, #6264 ) ;
#15881 = VERTEX_POINT ( 'NONE', #25347 ) ;
#15882 = FACE_OUTER_BOUND ( 'NONE', #24160, .T. ) ;
#15883 = DIRECTION ( 'NONE',  ( 1.000000000000000000, -0.000000000000000000, -0.000000000000000000 ) ) ;
#15884 = ORIENTED_EDGE ( 'NONE', *, *, #5165, .T. ) ;
#15885 = CARTESIAN_POINT ( 'NONE',  ( -7.798499376344062206, -4.740315990920112021, 195.0000000000000284 ) ) ;
#15886 = CARTESIAN_POINT ( 'NONE',  ( -7.250000000000000888, 7.450000000000003730, -19.00000000000000000 ) ) ;
#15887 = CARTESIAN_POINT ( 'NONE',  ( 8.250000000000005329, -7.249999999999998224, -24.00000000000000000 ) ) ;
#15888 = CIRCLE ( 'NONE', #42979, 0.1999999999999987899 ) ;
#15889 = DIRECTION ( 'NONE',  ( -0.000000000000000000, -1.000000000000000000, -0.000000000000000000 ) ) ;
#15890 = AXIS2_PLACEMENT_3D ( 'NONE', #30802, #9585, #25148 ) ;
#15891 = DIRECTION ( 'NONE',  ( -5.981805089575196197E-17, -1.000000000000000000, 0.000000000000000000 ) ) ;
#15892 = VECTOR ( 'NONE', #35044, 1000.000000000000000 ) ;
#15893 = ORIENTED_EDGE ( 'NONE', *, *, #48923, .T. ) ;
#15894 = VERTEX_POINT ( 'NONE', #67771 ) ;
#15895 = LINE ( 'NONE', #21213, #20532 ) ;
#15896 = ORIENTED_EDGE ( 'NONE', *, *, #67493, .F. ) ;
#15897 = ORIENTED_EDGE ( 'NONE', *, *, #56336, .F. ) ;
#15898 = VECTOR ( 'NONE', #39078, 1000.000000000000000 ) ;
#15899 = CARTESIAN_POINT ( 'NONE',  ( 275.0000000000000000, -25.60000000000000142, -15.10000000000000142 ) ) ;
#15900 = EDGE_CURVE ( 'NONE', #18742, #65963, #46197, .T. ) ;
#15901 = AXIS2_PLACEMENT_3D ( 'NONE', #58866, #68416, #36957 ) ;
#15902 = CARTESIAN_POINT ( 'NONE',  ( 11.78648345035337819, -4.406483450353490205, 455.0000000000000568 ) ) ;
#15903 = EDGE_CURVE ( 'NONE', #45362, #3520, #44830, .T. ) ;
#15904 = CARTESIAN_POINT ( 'NONE',  ( -25.50000000000000355, -5.578999999999999737, -22.50000000000000000 ) ) ;
#15905 = ORIENTED_EDGE ( 'NONE', *, *, #48320, .T. ) ;
#15906 = EDGE_LOOP ( 'NONE', ( #64261, #49548, #48341, #31371 ) ) ;
#15907 = LINE ( 'NONE', #42425, #33010 ) ;
#15908 = EDGE_LOOP ( 'NONE', ( #64929, #11133, #44219, #891 ) ) ;
#15909 = AXIS2_PLACEMENT_3D ( 'NONE', #21723, #33373, #27031 ) ;
#15910 = ORIENTED_EDGE ( 'NONE', *, *, #18191, .F. ) ;
#15911 = FACE_OUTER_BOUND ( 'NONE', #32318, .T. ) ;
#15912 = CARTESIAN_POINT ( 'NONE',  ( -29.50000000000000355, -11.50000000000100009, 15.00000000000084910 ) ) ;
#15913 = CARTESIAN_POINT ( 'NONE',  ( 28.90000000000000213, 20.60000000000000142, -13.86939075806900057 ) ) ;
#15914 = EDGE_CURVE ( 'NONE', #49081, #45591, #53909, .T. ) ;
#15915 = ORIENTED_EDGE ( 'NONE', *, *, #58238, .T. ) ;
#15916 = DIRECTION ( 'NONE',  ( 0.000000000000000000, 0.000000000000000000, -1.000000000000000000 ) ) ;
#15917 = CIRCLE ( 'NONE', #45260, 0.1999999999999996503 ) ;
#15919 = DIRECTION ( 'NONE',  ( 9.912705577010336396E-15, 1.000000000000000000, 0.000000000000000000 ) ) ;
#15918 = CYLINDRICAL_SURFACE ( 'NONE', #15223, 1.000000000000000000 ) ;
#15920 = ORIENTED_EDGE ( 'NONE', *, *, #15233, .F. ) ;
#15922 = EDGE_LOOP ( 'NONE', ( #17155, #39043, #58807, #24493 ) ) ;
#15921 = DIRECTION ( 'NONE',  ( -1.836970198721029934E-16, 1.836970198721036344E-16, -1.000000000000000000 ) ) ;
#15923 = VERTEX_POINT ( 'NONE', #3085 ) ;
#15924 = EDGE_CURVE ( 'NONE', #3096, #46362, #67468, .T. ) ;
#15925 = CARTESIAN_POINT ( 'NONE',  ( 30.00000000000000000, -9.199999999999999289, -12.69999999999986073 ) ) ;
#15926 = SHAPE_REPRESENTATION ( '5537T808_T-Slotted Framing_5537T808', ( #45918 ), #44782 ) ;
#15927 = LINE ( 'NONE', #21577, #29268 ) ;
#15928 = AXIS2_PLACEMENT_3D ( 'NONE', #12246, #39133, #39471 ) ;
#15929 = EDGE_CURVE ( 'NONE', #4544, #17779, #69176, .T. ) ;
#15930 = EDGE_LOOP ( 'NONE', ( #2293, #52319, #51263, #57573, #45000, #27880, #39664, #12070 ) ) ;
#15931 = CARTESIAN_POINT ( 'NONE',  ( 158.8349105750994568, -33.83962462487175316, 5.000000000000000000 ) ) ;
#15932 = LINE ( 'NONE', #365, #46979 ) ;
#15933 = ORIENTED_EDGE ( 'NONE', *, *, #20903, .F. ) ;
#15934 = VERTEX_POINT ( 'NONE', #51868 ) ;
#15935 = PLANE ( 'NONE',  #25204 ) ;
#15936 = DIRECTION ( 'NONE',  ( 0.000000000000000000, 0.000000000000000000, 1.000000000000000000 ) ) ;
#15937 = ADVANCED_FACE ( 'NONE', ( #3426 ), #46546, .F. ) ;
#15938 = DIRECTION ( 'NONE',  ( -1.000000000000000000, -2.135044278125299371E-15, 0.000000000000000000 ) ) ;
#15939 = VECTOR ( 'NONE', #19238, 1000.000000000000000 ) ;
#15940 = EDGE_LOOP ( 'NONE', ( #13119, #13565, #3801, #33955 ) ) ;
#15941 = ADVANCED_FACE ( 'NONE', ( #4140 ), #36649, .F. ) ;
#15942 = VECTOR ( 'NONE', #28357, 1000.000000000000000 ) ;
#15943 = CARTESIAN_POINT ( 'NONE',  ( 8.250000000000005329, -7.249999999999998224, -21.50000000000000000 ) ) ;
#15944 = DIRECTION ( 'NONE',  ( 1.000000000000000000, 0.000000000000000000, 0.000000000000000000 ) ) ;
#15946 = VERTEX_POINT ( 'NONE', #8362 ) ;
#15945 = DIRECTION ( 'NONE',  ( -1.000000000000000000, 0.000000000000000000, 0.000000000000000000 ) ) ;
#15948 = ORIENTED_EDGE ( 'NONE', *, *, #36418, .T. ) ;
#15947 = DIRECTION ( 'NONE',  ( 0.000000000000000000, 0.000000000000000000, 1.000000000000000000 ) ) ;
#15949 = AXIS2_PLACEMENT_3D ( 'NONE', #49870, #6727, #66813 ) ;
#15950 = DIRECTION ( 'NONE',  ( 1.000000000000000000, 0.000000000000000000, 0.000000000000000000 ) ) ;
#15951 = DIRECTION ( 'NONE',  ( 0.000000000000000000, -1.000000000000000000, 0.000000000000000000 ) ) ;
#15952 = EDGE_CURVE ( 'NONE', #39001, #44299, #12133, .T. ) ;
#15953 = LINE ( 'NONE', #37523, #51592 ) ;
#15954 = DIRECTION ( 'NONE',  ( -1.000000000000000000, 0.000000000000000000, 0.000000000000000000 ) ) ;
#15955 = AXIS2_PLACEMENT_3D ( 'NONE', #34743, #34378, #13879 ) ;
#15956 = VECTOR ( 'NONE', #42685, 1000.000000000000000 ) ;
#15957 = DIRECTION ( 'NONE',  ( 0.000000000000000000, 1.000000000000000000, -0.000000000000000000 ) ) ;
#15958 = CYLINDRICAL_SURFACE ( 'NONE', #4471, 1.399999999999998579 ) ;
#15959 = VERTEX_POINT ( 'NONE', #47265 ) ;
#15960 = DIRECTION ( 'NONE',  ( 0.000000000000000000, 0.000000000000000000, -1.000000000000000000 ) ) ;
#15961 = TOROIDAL_SURFACE ( 'NONE', #20492, 0.06000000000000080963, 0.7500000000000000000 ) ;
#15962 = ORIENTED_EDGE ( 'NONE', *, *, #1899, .F. ) ;
#15964 = VERTEX_POINT ( 'NONE', #41954 ) ;
#15963 = DIRECTION ( 'NONE',  ( 0.000000000000000000, -1.000000000000000000, 0.000000000000000000 ) ) ;
#15965 = DIRECTION ( 'NONE',  ( -8.728482790395504563E-15, -1.000000000000000000, 0.000000000000000000 ) ) ;
#15966 = DIRECTION ( 'NONE',  ( -7.665540703601096574E-15, -1.000000000000000000, -3.673940397442059868E-16 ) ) ;
#15967 = ORIENTED_EDGE ( 'NONE', *, *, #67389, .F. ) ;
#15968 = DIRECTION ( 'NONE',  ( -0.7071067811865474617, -0.7071067811865474617, -0.000000000000000000 ) ) ;
#15969 = DIRECTION ( 'NONE',  ( 0.000000000000000000, 1.000000000000000000, 0.000000000000000000 ) ) ;
#15970 = ORIENTED_EDGE ( 'NONE', *, *, #57345, .F. ) ;
#15971 = ADVANCED_FACE ( 'NONE', ( #31372 ), #68831, .F. ) ;
#15972 = CARTESIAN_POINT ( 'NONE',  ( 7.450000000000006395, 7.250000000000000888, -7.500000000000000000 ) ) ;
#15973 = CARTESIAN_POINT ( 'NONE',  ( 8.250000000000005329, -7.249999999999998224, -9.500000000000001776 ) ) ;
#15974 = CARTESIAN_POINT ( 'NONE',  ( 10.00000000000000000, 21.00000000000000000, 18.00000000000000355 ) ) ;
#15975 = ADVANCED_FACE ( 'NONE', ( #53973, #48659, #16482 ), #220, .F. ) ;
#15976 = EDGE_LOOP ( 'NONE', ( #11110, #67863, #24176, #58626 ) ) ;
#15977 = CIRCLE ( 'NONE', #67907, 0.3499999999999611200 ) ;
#15978 = DIRECTION ( 'NONE',  ( -1.261617073437657735E-14, -1.000000000000000000, 0.000000000000000000 ) ) ;
#15979 = ORIENTED_EDGE ( 'NONE', *, *, #69083, .F. ) ;
#15980 = EDGE_CURVE ( 'NONE', #34688, #32863, #4830, .T. ) ;
#15981 = ORIENTED_EDGE ( 'NONE', *, *, #40333, .F. ) ;
#15982 = DIRECTION ( 'NONE',  ( -1.000000000000000000, 0.000000000000000000, 0.000000000000000000 ) ) ;
#15983 = CARTESIAN_POINT ( 'NONE',  ( 8.900000000000005684, 14.08845687959340154, 20.99999999999999645 ) ) ;
#15984 = EDGE_CURVE ( 'NONE', #34012, #4795, #63877, .T. ) ;
#15985 = LINE ( 'NONE', #30848, #42246 ) ;
#15986 = EDGE_CURVE ( 'NONE', #57095, #10322, #21783, .T. ) ;
#15987 = CARTESIAN_POINT ( 'NONE',  ( 7.428221114745000797, 3.593516549646565750, 455.0000000000000568 ) ) ;
#15988 = ORIENTED_EDGE ( 'NONE', *, *, #44467, .F. ) ;
#15989 = ORIENTED_EDGE ( 'NONE', *, *, #25163, .F. ) ;
#15990 = VECTOR ( 'NONE', #25248, 1000.000000000000000 ) ;
#15992 = ORIENTED_EDGE ( 'NONE', *, *, #4647, .T. ) ;
#15991 = DIRECTION ( 'NONE',  ( -0.000000000000000000, -0.000000000000000000, -1.000000000000000000 ) ) ;
#15993 = ORIENTED_EDGE ( 'NONE', *, *, #14015, .F. ) ;
#15994 = PRODUCT_DEFINITION_SHAPE ( 'NONE', 'NONE',  #69988 ) ;
#15995 = VECTOR ( 'NONE', #44882, 1000.000000000000000 ) ;
#15996 = CARTESIAN_POINT ( 'NONE',  ( 3.682023737882786918, -9.737023737882811503, 54.00000000000000711 ) ) ;
#15997 = FACE_OUTER_BOUND ( 'NONE', #16789, .T. ) ;
#15998 = CARTESIAN_POINT ( 'NONE',  ( -11.00000000000000000, -13.54524521594299991, 17.53999999999999915 ) ) ;
#15999 = ADVANCED_FACE ( 'NONE', ( #42651 ), #54313, .T. ) ;
#16000 = EDGE_CURVE ( 'NONE', #22473, #14048, #32732, .T. ) ;
#16001 = CARTESIAN_POINT ( 'NONE',  ( 10.90000000000000036, -21.00000000000000000, 13.86939075806900057 ) ) ;
#16003 = LINE ( 'NONE', #21309, #48164 ) ;
#16002 = LINE ( 'NONE', #21996, #2723 ) ;
#16004 = EDGE_LOOP ( 'NONE', ( #40994, #39769, #55904, #30480 ) ) ;
#16006 = ORIENTED_EDGE ( 'NONE', *, *, #40224, .T. ) ;
#16005 = DIRECTION ( 'NONE',  ( -1.000000000000000000, 0.000000000000000000, 0.000000000000000000 ) ) ;
#16007 = VERTEX_POINT ( 'NONE', #53283 ) ;
#16008 = ORIENTED_EDGE ( 'NONE', *, *, #23716, .F. ) ;
#16010 = EDGE_CURVE ( 'NONE', #30669, #50794, #37022, .T. ) ;
#16009 = AXIS2_PLACEMENT_3D ( 'NONE', #29349, #66492, #18047 ) ;
#16011 = EDGE_CURVE ( 'NONE', #55364, #66440, #47960, .T. ) ;
#16012 = CLOSED_SHELL ( 'NONE', ( #40494, #55754, #48275, #41647, #54638, #20062 ) ) ;
#16013 = DIRECTION ( 'NONE',  ( 1.261617073437657735E-14, 1.000000000000000000, 3.673940397442059868E-16 ) ) ;
#16014 = CARTESIAN_POINT ( 'NONE',  ( 2.369523737882815784, 8.821682069070730492, 54.00000000000000711 ) ) ;
#16015 = EDGE_CURVE ( 'NONE', #19298, #6935, #11162, .T. ) ;
#16016 = CARTESIAN_POINT ( 'NONE',  ( 164.0064834503531586, -0.006483450349580488666, 195.0000000000001705 ) ) ;
#16017 = CARTESIAN_POINT ( 'NONE',  ( -25.50000000000000355, -5.578999999999999737, -24.12099999999999866 ) ) ;
#16018 = ORIENTED_EDGE ( 'NONE', *, *, #29548, .T. ) ;
#16019 = ORIENTED_EDGE ( 'NONE', *, *, #32730, .F. ) ;
#16020 = ORIENTED_EDGE ( 'NONE', *, *, #59616, .F. ) ;
#16022 = DIRECTION ( 'NONE',  ( 0.000000000000000000, -5.800915303574361727E-12, 1.000000000000000000 ) ) ;
#16021 = VECTOR ( 'NONE', #60125, 1000.000000000000000 ) ;
#16023 = ORIENTED_EDGE ( 'NONE', *, *, #4074, .T. ) ;
#16024 = DIRECTION ( 'NONE',  ( 1.000000000000000000, 0.000000000000000000, 0.000000000000000000 ) ) ;
#16025 = CARTESIAN_POINT ( 'NONE',  ( -2.355476262117234931, 8.821682069070680754, 54.00000000000000711 ) ) ;
#16026 = ORIENTED_EDGE ( 'NONE', *, *, #46777, .F. ) ;
#16027 = ORIENTED_EDGE ( 'NONE', *, *, #65262, .T. ) ;
#16028 = CARTESIAN_POINT ( 'NONE',  ( 11.12648345035336384, 2.893516549646526048, 455.0000000000000568 ) ) ;
#16029 = EDGE_CURVE ( 'NONE', #24345, #45256, #26855, .T. ) ;
#16030 = CARTESIAN_POINT ( 'NONE',  ( -16.33565937784311828, -0.3156604612129161880, -23.46090750622545684 ) ) ;
#16031 = ORIENTED_EDGE ( 'NONE', *, *, #56553, .T. ) ;
#16032 = ADVANCED_FACE ( 'NONE', ( #22134 ), #5873, .F. ) ;
#16033 = VECTOR ( 'NONE', #46695, 1000.000000000000000 ) ;
#16034 = DIRECTION ( 'NONE',  ( -1.000000000000000000, 0.000000000000000000, 0.000000000000000000 ) ) ;
#16036 = ORIENTED_EDGE ( 'NONE', *, *, #59121, .T. ) ;
#16035 = DIRECTION ( 'NONE',  ( -1.000000000000000000, 0.000000000000000000, 0.000000000000000000 ) ) ;
#16037 = ORIENTED_EDGE ( 'NONE', *, *, #63829, .T. ) ;
#16038 = CARTESIAN_POINT ( 'NONE',  ( 7.500000000000000000, -25.50000000000000355, -20.00000000000000000 ) ) ;
#16039 = FACE_OUTER_BOUND ( 'NONE', #10281, .T. ) ;
#16040 = DIRECTION ( 'NONE',  ( 0.000000000000000000, -1.000000000000000000, 0.000000000000000000 ) ) ;
#16041 = DIRECTION ( 'NONE',  ( 0.000000000000000000, -1.000000000000000000, 0.000000000000000000 ) ) ;
#16042 = CARTESIAN_POINT ( 'NONE',  ( 7.250000000000005329, -7.449999999999998401, -9.500000000000001776 ) ) ;
#16043 = AXIS2_PLACEMENT_3D ( 'NONE', #61133, #49512, #1081 ) ;
#16044 = VERTEX_POINT ( 'NONE', #6215 ) ;
#16045 = FACE_OUTER_BOUND ( 'NONE', #2406, .T. ) ;
#16046 = ORIENTED_EDGE ( 'NONE', *, *, #55043, .T. ) ;
#16047 = DIRECTION ( 'NONE',  ( 0.000000000000000000, -0.7096009616570518874, 0.7046037717862339012 ) ) ;
#16048 = DIRECTION ( 'NONE',  ( -0.7071067811865412445, 0.7071067811865537900, 0.000000000000000000 ) ) ;
#16049 = DIRECTION ( 'NONE',  ( 0.000000000000000000, 0.000000000000000000, -1.000000000000000000 ) ) ;
#16050 = DIRECTION ( 'NONE',  ( 1.000000000000000000, 0.000000000000000000, 0.000000000000000000 ) ) ;
#16051 = FACE_OUTER_BOUND ( 'NONE', #29705, .T. ) ;
#16052 = AXIS2_PLACEMENT_3D ( 'NONE', #68073, #13973, #8679 ) ;
#16053 = AXIS2_PLACEMENT_3D ( 'NONE', #43804, #39779, #66665 ) ;
#16054 = ORIENTED_EDGE ( 'NONE', *, *, #12175, .T. ) ;
#16055 = B_SPLINE_CURVE_WITH_KNOTS ( 'NONE', 3,
 ( #24901, #7223, #29150, #40461 ),
 .UNSPECIFIED., .F., .F.,
 ( 4, 4 ),
 ( -0.001424424334280369533, 0.0007144698416513659174 ),
 .UNSPECIFIED. ) ;
#16056 = LINE ( 'NONE', #58843, #27995 ) ;
#16057 = CIRCLE ( 'NONE', #32854, 0.9999999999984570120 ) ;
#16058 = EDGE_CURVE ( 'NONE', #24181, #37207, #38393, .T. ) ;
#16059 = ORIENTED_EDGE ( 'NONE', *, *, #45284, .T. ) ;
#16060 = CARTESIAN_POINT ( 'NONE',  ( 30.00000000000000000, -9.454754784057099570, 17.53999999999999915 ) ) ;
#16061 = DIRECTION ( 'NONE',  ( -1.000000000000000000, 0.000000000000000000, 0.000000000000000000 ) ) ;
#16062 = EDGE_CURVE ( 'NONE', #59053, #33806, #15557, .T. ) ;
#16063 = EDGE_LOOP ( 'NONE', ( #20338, #15842, #8161, #62231, #24752, #46865 ) ) ;
#16064 = CIRCLE ( 'NONE', #55572, 0.1749999999999989342 ) ;
#16065 = CARTESIAN_POINT ( 'NONE',  ( 11.50000000000000000, -11.50000000000000000, -15.00000000000000000 ) ) ;
#16066 = DIRECTION ( 'NONE',  ( 0.000000000000000000, 1.000000000000000000, 0.000000000000000000 ) ) ;
#16067 = EDGE_LOOP ( 'NONE', ( #56955, #8422, #3984, #65561 ) ) ;
#16068 = CYLINDRICAL_SURFACE ( 'NONE', #45747, 1.000000000000000000 ) ;
#16069 = EDGE_CURVE ( 'NONE', #64431, #3937, #31354, .T. ) ;
#16070 = EDGE_CURVE ( 'NONE', #5714, #22259, #65280, .T. ) ;
#16071 = CARTESIAN_POINT ( 'NONE',  ( 3.606483450353380249, -4.622483450353491286, 455.0000000000000568 ) ) ;
#16072 = CARTESIAN_POINT ( 'NONE',  ( 4.201500623656004407, 4.727349090213385452, 195.0000000000000284 ) ) ;
#16073 = EDGE_CURVE ( 'NONE', #45421, #58100, #25692, .T. ) ;
#16074 = LINE ( 'NONE', #27029, #29461 ) ;
#16075 = EDGE_CURVE ( 'NONE', #30509, #9548, #5526, .T. ) ;
#16076 = ORIENTED_EDGE ( 'NONE', *, *, #63826, .T. ) ;
#16078 = ORIENTED_EDGE ( 'NONE', *, *, #29541, .F. ) ;
#16077 = DIRECTION ( 'NONE',  ( 1.000000000000000000, 0.000000000000000000, 0.000000000000000000 ) ) ;
#16079 = DIRECTION ( 'NONE',  ( 0.000000000000000000, 0.000000000000000000, 1.000000000000000000 ) ) ;
#16080 = CYLINDRICAL_SURFACE ( 'NONE', #47023, 0.2000000000000000944 ) ;
#16081 = CARTESIAN_POINT ( 'NONE',  ( 11.18999999999999950, 12.00000000000000178, -5.000000000000000000 ) ) ;
#16082 = VERTEX_POINT ( 'NONE', #24485 ) ;
#16083 = DIRECTION ( 'NONE',  ( -1.836970198721029934E-16, 1.836970198721036590E-16, -1.000000000000000000 ) ) ;
#16084 = VECTOR ( 'NONE', #3781, 1000.000000000000000 ) ;
#16085 = ORIENTED_EDGE ( 'NONE', *, *, #31499, .T. ) ;
#16086 = EDGE_LOOP ( 'NONE', ( #14403, #17485, #7632, #66234 ) ) ;
#16087 = EDGE_LOOP ( 'NONE', ( #7081, #58548, #14270, #59120 ) ) ;
#16088 = VECTOR ( 'NONE', #68566, 1000.000000000000114 ) ;
#16089 = LINE ( 'NONE', #48616, #43341 ) ;
#16090 = DIRECTION ( 'NONE',  ( -1.000000000000000000, 0.000000000000000000, 0.000000000000000000 ) ) ;
#16091 = CARTESIAN_POINT ( 'NONE',  ( 15.00000000000000000, -42.00000000000000000, 26.50000000000000000 ) ) ;
#16092 = VERTEX_POINT ( 'NONE', #14214 ) ;
#16093 = ORIENTED_EDGE ( 'NONE', *, *, #64123, .T. ) ;
#16094 = CIRCLE ( 'NONE', #295, 0.1999999999999987899 ) ;
#16095 = DIRECTION ( 'NONE',  ( 1.047444401652939849E-14, 1.000000000000000000, 0.000000000000000000 ) ) ;
#16096 = ORIENTED_EDGE ( 'NONE', *, *, #11357, .F. ) ;
#16097 = VERTEX_POINT ( 'NONE', #38727 ) ;
#16098 = VECTOR ( 'NONE', #39027, 1000.000000000000000 ) ;
#16099 = ORIENTED_EDGE ( 'NONE', *, *, #61832, .T. ) ;
#16100 = ORIENTED_EDGE ( 'NONE', *, *, #6566, .F. ) ;
#16101 = FACE_OUTER_BOUND ( 'NONE', #18428, .T. ) ;
#16102 = UNCERTAINTY_MEASURE_WITH_UNIT (LENGTH_MEASURE( 1.000000000000000082E-05 ), #29587, 'distance_accuracy_value', 'NONE');
#16104 = ORIENTED_EDGE ( 'NONE', *, *, #15487, .T. ) ;
#16103 = DIRECTION ( 'NONE',  ( -1.000000000000000000, 0.000000000000000000, 0.000000000000000000 ) ) ;
#16105 = LINE ( 'NONE', #59239, #23260 ) ;
#16106 = EDGE_CURVE ( 'NONE', #53942, #11693, #30221, .T. ) ;
#16108 = CARTESIAN_POINT ( 'NONE',  ( -7.450000000000001954, 7.250000000000000000, -14.50000000000000000 ) ) ;
#16107 = VECTOR ( 'NONE', #41552, 1000.000000000000000 ) ;
#16109 = LINE ( 'NONE', #4467, #43705 ) ;
#16110 = EDGE_CURVE ( 'NONE', #56637, #14683, #69758, .T. ) ;
#16111 = ORIENTED_EDGE ( 'NONE', *, *, #23528, .F. ) ;
#16112 = VECTOR ( 'NONE', #39424, 1000.000000000000000 ) ;
#16113 = CIRCLE ( 'NONE', #29663, 0.7112000000000124889 ) ;
#16114 = DIRECTION ( 'NONE',  ( 0.000000000000000000, 0.000000000000000000, 1.000000000000000000 ) ) ;
#16115 = PLANE ( 'NONE',  #10104 ) ;
#16116 = EDGE_LOOP ( 'NONE', ( #27166, #56349, #12325, #56233 ) ) ;
#16117 = CARTESIAN_POINT ( 'NONE',  ( -6.486996718459931088, 2.617976262117183150, 26.00000000000000711 ) ) ;
#16118 = VECTOR ( 'NONE', #31860, 1000.000000000000000 ) ;
#16119 = DIRECTION ( 'NONE',  ( 1.836970198721029934E-16, -1.836970198721036344E-16, 1.000000000000000000 ) ) ;
#16120 = DIRECTION ( 'NONE',  ( -1.000000000000000000, 0.000000000000000000, 0.000000000000000000 ) ) ;
#16121 = EDGE_LOOP ( 'NONE', ( #17887, #5342, #23515, #41306 ) ) ;
#16122 = CARTESIAN_POINT ( 'NONE',  ( 7.616533956692213003, -8.606483450353492159, 455.0000000000000568 ) ) ;
#16123 = DIRECTION ( 'NONE',  ( 1.000000000000000000, 0.000000000000000000, 0.000000000000000000 ) ) ;
#16124 = CARTESIAN_POINT ( 'NONE',  ( 7.606483450353424658, 11.77351654964657435, 455.0000000000000568 ) ) ;
#16125 = VECTOR ( 'NONE', #58855, 1000.000000000000000 ) ;
#16126 = DIRECTION ( 'NONE',  ( 0.000000000000000000, 1.000000000000000000, 0.000000000000000000 ) ) ;
#16127 = DIRECTION ( 'NONE',  ( 0.000000000000000000, 0.000000000000000000, 1.000000000000000000 ) ) ;
#16128 = CARTESIAN_POINT ( 'NONE',  ( 4.186483450353375879, 11.77351654964663119, 195.0000000000000284 ) ) ;
#16129 = CIRCLE ( 'NONE', #64684, 0.5999999999999989786 ) ;
#16130 = CARTESIAN_POINT ( 'NONE',  ( -29.50000000000000355, -12.00000000000000000, 10.69999999999999929 ) ) ;
#16131 = DIRECTION ( 'NONE',  ( 0.000000000000000000, 0.000000000000000000, 1.000000000000000000 ) ) ;
#16132 = EDGE_CURVE ( 'NONE', #58549, #22374, #24122, .T. ) ;
#16133 = ORIENTED_EDGE ( 'NONE', *, *, #22488, .T. ) ;
#16134 = LINE ( 'NONE', #225, #7759 ) ;
#16135 = LINE ( 'NONE', #64242, #17250 ) ;
#16136 = FACE_OUTER_BOUND ( 'NONE', #11618, .T. ) ;
#16137 = EDGE_CURVE ( 'NONE', #34366, #27404, #46043, .T. ) ;
#16138 = CARTESIAN_POINT ( 'NONE',  ( 6.500000000000002665, 6.500000000000000888, 0.000000000000000000 ) ) ;
#16139 = VERTEX_POINT ( 'NONE', #51341 ) ;
#16140 = LINE ( 'NONE', #21104, #511 ) ;
#16141 = DIRECTION ( 'NONE',  ( -1.000000000000000000, 0.000000000000000000, 0.000000000000000000 ) ) ;
#16142 = EDGE_CURVE ( 'NONE', #23540, #51438, #8759, .T. ) ;
#16143 = ADVANCED_FACE ( 'NONE', ( #22818 ), #44366, .F. ) ;
#16144 = DIRECTION ( 'NONE',  ( 0.000000000000000000, 0.000000000000000000, 1.000000000000000000 ) ) ;
#16145 = CARTESIAN_POINT ( 'NONE',  ( -9.942044687070568543, 2.752095193409294982, 455.0000000000000568 ) ) ;
#16146 = CARTESIAN_POINT ( 'NONE',  ( 0.000000000000000000, 0.000000000000000000, -12.50000000000000000 ) ) ;
#16147 = ADVANCED_FACE ( 'NONE', ( #30130 ), #65937, .T. ) ;
#16148 = CARTESIAN_POINT ( 'NONE',  ( 0.000000000000000000, 8.250000000000001776, -25.00000000000000000 ) ) ;
#16149 = EDGE_CURVE ( 'NONE', #35812, #8571, #3611, .T. ) ;
#16150 = ORIENTED_EDGE ( 'NONE', *, *, #15282, .T. ) ;
#16151 = VECTOR ( 'NONE', #67642, 1000.000000000000000 ) ;
#16152 = EDGE_LOOP ( 'NONE', ( #14444, #34409, #67035, #60254 ) ) ;
#16153 = EDGE_CURVE ( 'NONE', #27405, #30268, #18819, .T. ) ;
#16154 = CARTESIAN_POINT ( 'NONE',  ( 73.77321854994620765, 47.95351654967443977, 20.00000000000000000 ) ) ;
#16155 = CARTESIAN_POINT ( 'NONE',  ( 29.50000000000000355, -11.50000000000100009, -10.50000000000065903 ) ) ;
#16156 = VERTEX_POINT ( 'NONE', #49688 ) ;
#16157 = CARTESIAN_POINT ( 'NONE',  ( -9.781776262117324094, -10.50702373788275779, 54.00000000000000711 ) ) ;
#16158 = VECTOR ( 'NONE', #34651, 1000.000000000000000 ) ;
#16159 = AXIS2_PLACEMENT_3D ( 'NONE', #63550, #58596, #27106 ) ;
#16160 = CARTESIAN_POINT ( 'NONE',  ( 11.34648345035338046, -1.090483450353395334, 195.0000000000000284 ) ) ;
#16161 = ORIENTED_EDGE ( 'NONE', *, *, #63689, .F. ) ;
#16162 = DIRECTION ( 'NONE',  ( 0.000000000000000000, 0.000000000000000000, -1.000000000000000000 ) ) ;
#16163 = ORIENTED_EDGE ( 'NONE', *, *, #63145, .F. ) ;
#16164 = CIRCLE ( 'NONE', #42151, 3.500000000000003109 ) ;
#16165 = VERTEX_POINT ( 'NONE', #56990 ) ;
#16166 = FACE_OUTER_BOUND ( 'NONE', #8999, .T. ) ;
#16167 = ORIENTED_EDGE ( 'NONE', *, *, #26858, .T. ) ;
#16168 = CARTESIAN_POINT ( 'NONE',  ( 9.804883450353409913, 11.07551654964657928, 195.0000000000000284 ) ) ;
#16169 = DIRECTION ( 'NONE',  ( 0.000000000000000000, -1.000000000000000000, 0.000000000000000000 ) ) ;
#16170 = DIRECTION ( 'NONE',  ( 0.000000000000000000, -1.000000000000000000, 0.000000000000000000 ) ) ;
#16171 = VECTOR ( 'NONE', #60787, 1000.000000000000000 ) ;
#16172 = VERTEX_POINT ( 'NONE', #41079 ) ;
#16173 = EDGE_LOOP ( 'NONE', ( #16888, #18937, #14609, #23452, #53511, #38840 ) ) ;
#16174 = CARTESIAN_POINT ( 'NONE',  ( 11.78648345035333200, 4.173516549646566709, 195.0000000000000284 ) ) ;
#16176 = CARTESIAN_POINT ( 'NONE',  ( -7.450000000000001954, 7.250000000000000000, -9.500000000000001776 ) ) ;
#16175 = DIRECTION ( 'NONE',  ( -1.836970198721029934E-16, 1.836970198721036344E-16, -1.000000000000000000 ) ) ;
#16177 = EDGE_LOOP ( 'NONE', ( #31195, #62976 ) ) ;
#16178 = VECTOR ( 'NONE', #55964, 1000.000000000000000 ) ;
#16179 = ORIENTED_EDGE ( 'NONE', *, *, #18461, .F. ) ;
#16180 = ORIENTED_EDGE ( 'NONE', *, *, #13410, .F. ) ;
#16181 = LINE ( 'NONE', #27142, #45759 ) ;
#16182 = CIRCLE ( 'NONE', #35330, 0.5999999999999998668 ) ;
#16184 = VERTEX_POINT ( 'NONE', #6571 ) ;
#16183 = DIRECTION ( 'NONE',  ( 0.000000000000000000, 1.000000000000000000, 0.000000000000000000 ) ) ;
#16185 = DIRECTION ( 'NONE',  ( 0.000000000000000000, 0.000000000000000000, -1.000000000000000000 ) ) ;
#16186 = DIRECTION ( 'NONE',  ( -1.000000000000000000, 0.000000000000000000, 0.000000000000000000 ) ) ;
#16187 = ORIENTED_EDGE ( 'NONE', *, *, #12508, .F. ) ;
#16188 = VERTEX_POINT ( 'NONE', #17509 ) ;
#16189 = EDGE_CURVE ( 'NONE', #8473, #21794, #57316, .T. ) ;
#16190 = EDGE_CURVE ( 'NONE', #33185, #67565, #7846, .T. ) ;
#16191 = EDGE_CURVE ( 'NONE', #17051, #56170, #51708, .T. ) ;
#16192 = DIRECTION ( 'NONE',  ( 1.000000000000000000, 0.000000000000000000, 0.000000000000000000 ) ) ;
#16193 = ORIENTED_EDGE ( 'NONE', *, *, #4315, .F. ) ;
#16194 = EDGE_CURVE ( 'NONE', #68881, #10422, #46009, .T. ) ;
#16195 = CARTESIAN_POINT ( 'NONE',  ( 38.90000000000000568, 0.000000000000000000, 0.000000000000000000 ) ) ;
#16196 = DIRECTION ( 'NONE',  ( -1.000000000000000000, -0.000000000000000000, -0.000000000000000000 ) ) ;
#16197 = ORIENTED_EDGE ( 'NONE', *, *, #22467, .T. ) ;
#16198 = VECTOR ( 'NONE', #17337, 1000.000000000000000 ) ;
#16199 = AXIS2_PLACEMENT_3D ( 'NONE', #21470, #38436, #11880 ) ;
#16200 = CARTESIAN_POINT ( 'NONE',  ( 30.00000000000000000, -14.33999999999999986, -14.50000000000000000 ) ) ;
#16201 = CARTESIAN_POINT ( 'NONE',  ( -17.00000000000000000, -16.28999999999710369, 15.00000000000794920 ) ) ;
#16202 = ORIENTED_EDGE ( 'NONE', *, *, #19130, .T. ) ;
#16203 = ORIENTED_EDGE ( 'NONE', *, *, #35561, .T. ) ;
#16205 = CARTESIAN_POINT ( 'NONE',  ( 4.186483450353422953, 11.77351654964658501, 455.0000000000000568 ) ) ;
#16204 = AXIS2_PLACEMENT_3D ( 'NONE', #19439, #51626, #46659 ) ;
#16207 = AXIS2_PLACEMENT_3D ( 'NONE', #54197, #60171, #11723 ) ;
#16206 = DIRECTION ( 'NONE',  ( 1.000000000000000000, -1.115702204244422993E-14, -1.836970198721050395E-16 ) ) ;
#16208 = DIRECTION ( 'NONE',  ( 8.673617379884051249E-15, 1.000000000000000000, 0.000000000000000000 ) ) ;
#16209 = CYLINDRICAL_SURFACE ( 'NONE', #63361, 1.000000000000000000 ) ;
#16210 = CIRCLE ( 'NONE', #52362, 2.250000000000001776 ) ;
#16211 = DIRECTION ( 'NONE',  ( 1.000000000000000000, 0.000000000000000000, 0.000000000000000000 ) ) ;
#16212 = ORIENTED_EDGE ( 'NONE', *, *, #4662, .F. ) ;
#16213 = DIRECTION ( 'NONE',  ( 0.000000000000000000, 0.000000000000000000, 1.000000000000000000 ) ) ;
#16214 = CARTESIAN_POINT ( 'NONE',  ( 4.622483450353346512, 3.593516549646634584, 195.0000000000000284 ) ) ;
#16215 =( NAMED_UNIT ( * ) SI_UNIT ( $, .STERADIAN. ) SOLID_ANGLE_UNIT ( ) );
#16217 = VERTEX_POINT ( 'NONE', #35778 ) ;
#16216 = CARTESIAN_POINT ( 'NONE',  ( 146.5599459900709860, 5.000000000000000000, 320.8239988703753056 ) ) ;
#16218 = CARTESIAN_POINT ( 'NONE',  ( 25.90000000000000213, 13.66939075806899240, -20.79999999999999361 ) ) ;
#16219 = CARTESIAN_POINT ( 'NONE',  ( 6.832023737882818359, -9.737023737882822161, 54.00000000000000711 ) ) ;
#16220 = FACE_OUTER_BOUND ( 'NONE', #8242, .T. ) ;
#16221 = EDGE_LOOP ( 'NONE', ( #9119, #23496, #38767, #44673 ) ) ;
#16222 = CARTESIAN_POINT ( 'NONE',  ( 8.900000000000002132, -18.00000000000000355, -21.00000000000000000 ) ) ;
#16223 = DIRECTION ( 'NONE',  ( -1.836970198721029934E-16, 1.836970198721036344E-16, -1.000000000000000000 ) ) ;
#16224 = EDGE_LOOP ( 'NONE', ( #62614, #15157, #44580, #32994 ) ) ;
#16225 = CARTESIAN_POINT ( 'NONE',  ( -10.49297626211724754, -3.664523737882706023, 26.00000000000000000 ) ) ;
#16226 = DIRECTION ( 'NONE',  ( -1.000000000000000000, 0.000000000000000000, 0.000000000000000000 ) ) ;
#16227 = DIRECTION ( 'NONE',  ( -1.000000000000000000, 0.000000000000000000, 0.000000000000000000 ) ) ;
#16228 = LINE ( 'NONE', #63638, #55368 ) ;
#16229 = ADVANCED_FACE ( 'NONE', ( #67964 ), #35068, .F. ) ;
#16230 = DIRECTION ( 'NONE',  ( -1.000000000000000000, 0.000000000000000000, 0.000000000000000000 ) ) ;
#16231 = EDGE_LOOP ( 'NONE', ( #13534, #40130, #31145, #41556 ) ) ;
#16232 = EDGE_CURVE ( 'NONE', #63246, #38926, #44029, .T. ) ;
#16233 = VERTEX_POINT ( 'NONE', #8198 ) ;
#16234 = DIRECTION ( 'NONE',  ( -0.000000000000000000, -0.000000000000000000, -1.000000000000000000 ) ) ;
#16235 = ORIENTED_EDGE ( 'NONE', *, *, #47993, .F. ) ;
#16236 = EDGE_CURVE ( 'NONE', #4872, #2943, #50992, .T. ) ;
#16237 = VERTEX_POINT ( 'NONE', #26578 ) ;
#16238 = DIRECTION ( 'NONE',  ( -1.794541526872559352E-16, -1.000000000000000000, 0.000000000000000000 ) ) ;
#16239 = EDGE_CURVE ( 'NONE', #6189, #18842, #10657, .T. ) ;
#16240 = LINE ( 'NONE', #21551, #10704 ) ;
#16241 = DIRECTION ( 'NONE',  ( -0.000000000000000000, 1.000000000000000000, -0.000000000000000000 ) ) ;
#16242 = ORIENTED_EDGE ( 'NONE', *, *, #32361, .F. ) ;
#16243 = EDGE_CURVE ( 'NONE', #24345, #62375, #36852, .T. ) ;
#16244 = ORIENTED_EDGE ( 'NONE', *, *, #61407, .F. ) ;
#16245 = CARTESIAN_POINT ( 'NONE',  ( -15.50000000000000000, -15.50000000000000000, -22.50000000000000000 ) ) ;
#16247 = ORIENTED_EDGE ( 'NONE', *, *, #45910, .T. ) ;
#16246 = ADVANCED_FACE ( 'NONE', ( #42131 ), #31542, .F. ) ;
#16248 = EDGE_LOOP ( 'NONE', ( #69647, #64944, #21574, #64996 ) ) ;
#16249 = CARTESIAN_POINT ( 'NONE',  ( 39.90000000000000568, 0.000000000000000000, 3.500000000000000000 ) ) ;
#16250 = CYLINDRICAL_SURFACE ( 'NONE', #7559, 1.000000000000000000 ) ;
#16251 = VECTOR ( 'NONE', #30748, 1000.000000000000000 ) ;
#16252 = DIRECTION ( 'NONE',  ( 0.000000000000000000, -0.000000000000000000, 1.000000000000000000 ) ) ;
#16253 = ORIENTED_EDGE ( 'NONE', *, *, #66398, .T. ) ;
#16254 = DIRECTION ( 'NONE',  ( 0.000000000000000000, 0.000000000000000000, -1.000000000000000000 ) ) ;
#16256 = DIRECTION ( 'NONE',  ( 0.7671651518152939886, -0.6414496315691644579, -2.587583378555133721E-16 ) ) ;
#16255 = DIRECTION ( 'NONE',  ( -0.000000000000000000, 3.673940397442059868E-16, -1.000000000000000000 ) ) ;
#16257 = ORIENTED_EDGE ( 'NONE', *, *, #25405, .F. ) ;
#16258 = AXIS2_PLACEMENT_3D ( 'NONE', #21372, #26329, #31992 ) ;
#16260 = ORIENTED_EDGE ( 'NONE', *, *, #3136, .T. ) ;
#16259 = VECTOR ( 'NONE', #19405, 1000.000000000000000 ) ;
#16262 = EDGE_LOOP ( 'NONE', ( #28011, #11104, #14536, #7929 ) ) ;
#16261 = DIRECTION ( 'NONE',  ( -1.000000000000000000, 0.000000000000000000, 0.000000000000000000 ) ) ;
#16263 = VERTEX_POINT ( 'NONE', #26228 ) ;
#16264 = VECTOR ( 'NONE', #43075, 1000.000000000000000 ) ;
#16265 = AXIS2_PLACEMENT_3D ( 'NONE', #4692, #10344, #47127 ) ;
#16266 = CIRCLE ( 'NONE', #55622, 1.000000000000000888 ) ;
#16267 = DIRECTION ( 'NONE',  ( 1.000000000000000000, 0.000000000000000000, 0.000000000000000000 ) ) ;
#16268 = DIRECTION ( 'NONE',  ( 0.000000000000000000, -0.000000000000000000, 1.000000000000000000 ) ) ;
#16269 = VERTEX_POINT ( 'NONE', #5010 ) ;
#16270 = ORIENTED_EDGE ( 'NONE', *, *, #28975, .T. ) ;
#16271 = AXIS2_PLACEMENT_3D ( 'NONE', #10686, #437, #32952 ) ;
#16272 = CARTESIAN_POINT ( 'NONE',  ( 7.250000000000005329, -7.449999999999998401, -15.50000000000000000 ) ) ;
#16273 = LINE ( 'NONE', #49149, #66211 ) ;
#16274 = ORIENTED_EDGE ( 'NONE', *, *, #2947, .T. ) ;
#16275 = EDGE_LOOP ( 'NONE', ( #58537, #15215, #40426, #35425 ) ) ;
#16276 = ADVANCED_FACE ( 'NONE', ( #53808 ), #53117, .T. ) ;
#16277 = DIRECTION ( 'NONE',  ( 3.596772705736696467E-15, 1.000000000000000000, 0.000000000000000000 ) ) ;
#16278 = LINE ( 'NONE', #16641, #24487 ) ;
#16279 = LINE ( 'NONE', #43146, #3410 ) ;
#16280 = EDGE_LOOP ( 'NONE', ( #38035, #11832, #21035, #61258 ) ) ;
#16281 = CARTESIAN_POINT ( 'NONE',  ( 11.08848345035336891, 9.791916549646611401, 195.0000000000000284 ) ) ;
#16282 = CARTESIAN_POINT ( 'NONE',  ( -9.897976262117259338, 6.642976262117183950, 54.00000000000000711 ) ) ;
#16283 = CIRCLE ( 'NONE', #55794, 24.99999999998784972 ) ;
#16285 = ORIENTED_EDGE ( 'NONE', *, *, #35241, .F. ) ;
#16284 = DIRECTION ( 'NONE',  ( -1.000000000000000000, 0.000000000000000000, 0.000000000000000000 ) ) ;
#16287 = EDGE_LOOP ( 'NONE', ( #43026, #62205, #19694, #37467 ) ) ;
#16286 = DIRECTION ( 'NONE',  ( -0.000000000000000000, -0.000000000000000000, -1.000000000000000000 ) ) ;
#16288 = CARTESIAN_POINT ( 'NONE',  ( -7.250000000000001776, -7.249999999999998224, -8.500000000000000000 ) ) ;
#16289 = EDGE_CURVE ( 'NONE', #22077, #61234, #63009, .T. ) ;
#16290 = CARTESIAN_POINT ( 'NONE',  ( 11.00000000000000000, -13.79999999999979998, -17.30000000000000071 ) ) ;
#16291 = VECTOR ( 'NONE', #3886, 1000.000000000000000 ) ;
#16292 = CARTESIAN_POINT ( 'NONE',  ( -16.75000000000000000, -0.3156864504677179273, -22.74361999681790536 ) ) ;
#16293 = CARTESIAN_POINT ( 'NONE',  ( 14.75000000000000178, -0.2500000000000059952, 26.75000000000000000 ) ) ;
#16294 = CARTESIAN_POINT ( 'NONE',  ( 8.900000000000002132, -18.00000000000000355, -21.00000000000000000 ) ) ;
#16295 = ADVANCED_FACE ( 'NONE', ( #41782 ), #3964, .F. ) ;
#16296 = CARTESIAN_POINT ( 'NONE',  ( -5.993516549646711766, 5.993516549646603409, 455.0000000000000568 ) ) ;
#16297 = ORIENTED_EDGE ( 'NONE', *, *, #31252, .T. ) ;
#16298 = CARTESIAN_POINT ( 'NONE',  ( -29.50000000000000355, -12.00000000000000000, -10.52786404500095863 ) ) ;
#16300 = VERTEX_POINT ( 'NONE', #14924 ) ;
#16299 = CARTESIAN_POINT ( 'NONE',  ( -9.942044687070668019, -9.247904806590694804, 455.0000000000000568 ) ) ;
#16302 = VERTEX_POINT ( 'NONE', #69360 ) ;
#16301 = CARTESIAN_POINT ( 'NONE',  ( -7.450000000000001954, 7.250000000000000000, -10.00000000000000000 ) ) ;
#16303 = VECTOR ( 'NONE', #57447, 1000.000000000000000 ) ;
#16304 = VECTOR ( 'NONE', #11721, 1000.000000000000000 ) ;
#16305 = FACE_OUTER_BOUND ( 'NONE', #69777, .T. ) ;
#16306 = FACE_OUTER_BOUND ( 'NONE', #15408, .T. ) ;
#16307 = CIRCLE ( 'NONE', #67117, 0.1749999999999989342 ) ;
#16308 = AXIS2_PLACEMENT_3D ( 'NONE', #57713, #9281, #31220 ) ;
#16309 = VECTOR ( 'NONE', #26302, 1000.000000000000000 ) ;
#16310 = ORIENTED_EDGE ( 'NONE', *, *, #68248, .F. ) ;
#16311 = CARTESIAN_POINT ( 'NONE',  ( 7.000000000000000000, -25.93000000000544958, -9.412893218815410634 ) ) ;
#16312 = DIRECTION ( 'NONE',  ( -0.000000000000000000, 3.673940397442059868E-16, -1.000000000000000000 ) ) ;
#16313 = EDGE_CURVE ( 'NONE', #37811, #48332, #47099, .T. ) ;
#16314 = VERTEX_POINT ( 'NONE', #68672 ) ;
#16315 = CYLINDRICAL_SURFACE ( 'NONE', #62825, 24.99999999998784972 ) ;
#16316 = CARTESIAN_POINT ( 'NONE',  ( -7.450000000000001954, -7.249999999999998224, -14.50000000000000000 ) ) ;
#16317 = VECTOR ( 'NONE', #33549, 1000.000000000000000 ) ;
#16318 = DIRECTION ( 'NONE',  ( 0.000000000000000000, -1.000000000000000000, 0.000000000000000000 ) ) ;
#16319 = ORIENTED_EDGE ( 'NONE', *, *, #53046, .T. ) ;
#16320 = EDGE_CURVE ( 'NONE', #34995, #62860, #408, .T. ) ;
#16321 = CYLINDRICAL_SURFACE ( 'NONE', #65373, 0.1749999999999989342 ) ;
#16322 = ORIENTED_EDGE ( 'NONE', *, *, #41065, .T. ) ;
#16323 = VECTOR ( 'NONE', #51319, 1000.000000000000000 ) ;
#16324 = ORIENTED_EDGE ( 'NONE', *, *, #35797, .T. ) ;
#16325 = VECTOR ( 'NONE', #3563, 1000.000000000000000 ) ;
#16326 = DIRECTION ( 'NONE',  ( 0.000000000000000000, -1.000000000000000000, 2.854859206170826497E-12 ) ) ;
#16327 = CARTESIAN_POINT ( 'NONE',  ( 283.0000000000000568, -27.13000000000000611, 15.49999999999930012 ) ) ;
#16328 = PLANE ( 'NONE',  #24223 ) ;
#16329 = FACE_BOUND ( 'NONE', #12225, .T. ) ;
#16330 = ORIENTED_EDGE ( 'NONE', *, *, #48959, .T. ) ;
#16331 = EDGE_CURVE ( 'NONE', #68520, #33439, #36480, .T. ) ;
#16332 = VERTEX_POINT ( 'NONE', #42830 ) ;
#16334 = ORIENTED_EDGE ( 'NONE', *, *, #20849, .F. ) ;
#16333 = DIRECTION ( 'NONE',  ( -0.000000000000000000, -0.000000000000000000, -1.000000000000000000 ) ) ;
#16336 = ORIENTED_EDGE ( 'NONE', *, *, #13643, .T. ) ;
#16335 = EDGE_CURVE ( 'NONE', #32863, #27141, #53458, .T. ) ;
#16337 = CARTESIAN_POINT ( 'NONE',  ( 7.272650909786598561, -4.201500623656027500, 195.0000000000000284 ) ) ;
#16338 = FACE_OUTER_BOUND ( 'NONE', #42606, .T. ) ;
#16339 = CARTESIAN_POINT ( 'NONE',  ( -7.250000000000000888, 7.250000000000001776, -17.00000000000000000 ) ) ;
#16340 = CIRCLE ( 'NONE', #43428, 2.204799999999997429 ) ;
#16342 = DIRECTION ( 'NONE',  ( -0.8660254037844400399, -0.4999999999999973910, 6.723777587268495961E-17 ) ) ;
#16341 = CARTESIAN_POINT ( 'NONE',  ( 11.00000000000000000, -14.04000000000000092, -17.04524521594300523 ) ) ;
#16343 = ORIENTED_EDGE ( 'NONE', *, *, #57969, .F. ) ;
#16345 = ORIENTED_EDGE ( 'NONE', *, *, #21587, .T. ) ;
#16344 = DIRECTION ( 'NONE',  ( 0.000000000000000000, 0.000000000000000000, 1.000000000000000000 ) ) ;
#16346 = VECTOR ( 'NONE', #25362, 1000.000000000000000 ) ;
#16347 = EDGE_LOOP ( 'NONE', ( #53156, #49609 ) ) ;
#16348 = ORIENTED_EDGE ( 'NONE', *, *, #52733, .F. ) ;
#16349 = CARTESIAN_POINT ( 'NONE',  ( 15.50000000000000000, -1.037157890325000054, 22.50000000000000000 ) ) ;
#16350 = DIRECTION ( 'NONE',  ( 0.000000000000000000, 0.000000000000000000, 1.000000000000000000 ) ) ;
#16351 = AXIS2_PLACEMENT_3D ( 'NONE', #18018, #39924, #18358 ) ;
#16353 = FACE_OUTER_BOUND ( 'NONE', #6627, .T. ) ;
#16352 = CIRCLE ( 'NONE', #42343, 4.500000000000190958 ) ;
#16354 = VERTEX_POINT ( 'NONE', #37197 ) ;
#16355 = EDGE_CURVE ( 'NONE', #67088, #4595, #66063, .T. ) ;
#16356 = ORIENTED_EDGE ( 'NONE', *, *, #67900, .T. ) ;
#16357 = ORIENTED_EDGE ( 'NONE', *, *, #11207, .T. ) ;
#16358 = LINE ( 'NONE', #56519, #49729 ) ;
#16359 = COLOUR_RGB ( '', 0.09019608, 0.27058824, 0.51372549) ;
#16360 = CARTESIAN_POINT ( 'NONE',  ( 275.0000000000000000, -25.00000000000299849, -9.079999998829670460 ) ) ;
#16361 = DIRECTION ( 'NONE',  ( 0.000000000000000000, -1.000000000000000000, 0.000000000000000000 ) ) ;
#16362 = ORIENTED_EDGE ( 'NONE', *, *, #48263, .F. ) ;
#16363 = EDGE_CURVE ( 'NONE', #57794, #22125, #58049, .T. ) ;
#16364 = ORIENTED_EDGE ( 'NONE', *, *, #9407, .T. ) ;
#16365 = CYLINDRICAL_SURFACE ( 'NONE', #39548, 0.3499999999999302558 ) ;
#16366 = AXIS2_PLACEMENT_3D ( 'NONE', #15486, #39375, #33039 ) ;
#16367 = PLANE ( 'NONE',  #62775 ) ;
#16368 = EDGE_LOOP ( 'NONE', ( #62412, #37777, #65324, #17471 ) ) ;
#16369 = EDGE_CURVE ( 'NONE', #14861, #44485, #65899, .T. ) ;
#16370 = CIRCLE ( 'NONE', #17514, 0.1749999999999989342 ) ;
#16371 = LINE ( 'NONE', #48905, #8768 ) ;
#16372 = EDGE_CURVE ( 'NONE', #51717, #23171, #3774, .T. ) ;
#16374 = ORIENTED_EDGE ( 'NONE', *, *, #2570, .T. ) ;
#16373 = CYLINDRICAL_SURFACE ( 'NONE', #33983, 0.9999999999984552357 ) ;
#16375 = CIRCLE ( 'NONE', #33332, 3.499999999999850342 ) ;
#16376 = ORIENTED_EDGE ( 'NONE', *, *, #11601, .F. ) ;
#16377 = LINE ( 'NONE', #21336, #46844 ) ;
#16378 = DIRECTION ( 'NONE',  ( -0.000000000000000000, 3.673940397442059868E-16, -1.000000000000000000 ) ) ;
#16379 = EDGE_CURVE ( 'NONE', #68417, #33912, #24109, .T. ) ;
#16380 = DIRECTION ( 'NONE',  ( -1.836970198721029934E-16, -1.836970198721010706E-16, 1.000000000000000000 ) ) ;
#16381 = DIRECTION ( 'NONE',  ( 1.000000000000000000, 0.000000000000000000, 0.000000000000000000 ) ) ;
#16382 = DIRECTION ( 'NONE',  ( -0.000000000000000000, -0.000000000000000000, -1.000000000000000000 ) ) ;
#16383 = ADVANCED_FACE ( 'NONE', ( #46732 ), #48846, .T. ) ;
#16384 = VERTEX_POINT ( 'NONE', #44207 ) ;
#16385 = DIRECTION ( 'NONE',  ( -1.000000000000000000, 8.339399738404099512E-15, -1.836970198721014650E-16 ) ) ;
#16386 = VERTEX_POINT ( 'NONE', #400 ) ;
#16387 = FACE_OUTER_BOUND ( 'NONE', #14965, .T. ) ;
#16388 = CARTESIAN_POINT ( 'NONE',  ( -11.00000000000000000, -9.454754784057099570, -17.53999999999999915 ) ) ;
#16389 = ADVANCED_FACE ( 'NONE', ( #26933 ), #54152, .F. ) ;
#16390 = DIRECTION ( 'NONE',  ( -2.135044278125299371E-15, 1.000000000000000000, -0.000000000000000000 ) ) ;
#16391 = EDGE_CURVE ( 'NONE', #53316, #69042, #27502, .T. ) ;
#16392 = DIRECTION ( 'NONE',  ( 0.000000000000000000, -1.000000000000000000, 1.540434446669787085E-12 ) ) ;
#16393 = CARTESIAN_POINT ( 'NONE',  ( -1.853252480934758584, 9.404046420173985510, 455.0000000000000568 ) ) ;
#16394 = EDGE_CURVE ( 'NONE', #10593, #7152, #65448, .T. ) ;
#16395 = VECTOR ( 'NONE', #23089, 1000.000000000000000 ) ;
#16396 = EDGE_CURVE ( 'NONE', #40390, #60302, #32921, .T. ) ;
#16397 = EDGE_CURVE ( 'NONE', #48542, #17390, #38912, .T. ) ;
#16398 = ORIENTED_EDGE ( 'NONE', *, *, #3305, .F. ) ;
#16399 = CARTESIAN_POINT ( 'NONE',  ( -6.817976262117261044, 9.722976262117182245, 54.00000000000000711 ) ) ;
#16400 = SURFACE_SIDE_STYLE ('',( #27014 ) ) ;
#16401 = ADVANCED_FACE ( 'NONE', ( #12022 ), #39257, .T. ) ;
#16402 = AXIS2_PLACEMENT_3D ( 'NONE', #61738, #56431, #7982 ) ;
#16403 = CIRCLE ( 'NONE', #35556, 0.5999999999999998668 ) ;
#16404 = CIRCLE ( 'NONE', #55909, 0.1999999999999987899 ) ;
#16405 = ORIENTED_EDGE ( 'NONE', *, *, #31971, .F. ) ;
#16406 = EDGE_CURVE ( 'NONE', #21711, #1336, #33270, .T. ) ;
#16407 = DIRECTION ( 'NONE',  ( -1.000000000000000000, 0.000000000000000000, 0.000000000000000000 ) ) ;
#16408 = FACE_OUTER_BOUND ( 'NONE', #24871, .T. ) ;
#16409 = ORIENTED_EDGE ( 'NONE', *, *, #37463, .F. ) ;
#16410 = EDGE_CURVE ( 'NONE', #33631, #2837, #46676, .T. ) ;
#16411 = CARTESIAN_POINT ( 'NONE',  ( 75.42576880091934299, 0.000000000000000000, 330.9830310981789694 ) ) ;
#16412 = DIRECTION ( 'NONE',  ( -1.000000000000000000, 8.540177112501197482E-15, 3.137610169492823463E-30 ) ) ;
#16413 = VECTOR ( 'NONE', #22865, 1000.000000000000000 ) ;
#16414 = VECTOR ( 'NONE', #54266, 1000.000000000000000 ) ;
#16415 = ORIENTED_EDGE ( 'NONE', *, *, #51817, .T. ) ;
#16416 = CARTESIAN_POINT ( 'NONE',  ( 32.89999999999999858, -0.1999999999911795112, 8.826273045769999343E-12 ) ) ;
#16417 = CARTESIAN_POINT ( 'NONE',  ( 11.50000000000000000, -11.50000000000000000, -19.00000000000000000 ) ) ;
#16418 = AXIS2_PLACEMENT_3D ( 'NONE', #48407, #53719, #69971 ) ;
#16419 = CARTESIAN_POINT ( 'NONE',  ( 75.42576880091937142, 10.00000000000000000, 282.4830310981789125 ) ) ;
#16420 = CARTESIAN_POINT ( 'NONE',  ( 7.000000000000000000, -26.50000000000000000, -5.530822723609929881 ) ) ;
#16421 = EDGE_CURVE ( 'NONE', #16514, #67467, #64751, .T. ) ;
#16422 = ORIENTED_EDGE ( 'NONE', *, *, #29845, .T. ) ;
#16424 = EDGE_LOOP ( 'NONE', ( #19138, #33965, #37929, #20076 ) ) ;
#16423 = DIRECTION ( 'NONE',  ( -1.000000000000000000, -1.570596175624152290E-15, 0.000000000000000000 ) ) ;
#16425 = EDGE_CURVE ( 'NONE', #45166, #6666, #22326, .T. ) ;
#16426 = AXIS2_PLACEMENT_3D ( 'NONE', #52491, #29860, #41526 ) ;
#16427 = DIRECTION ( 'NONE',  ( -1.000000000000000000, 1.828336019306068695E-14, -1.836970198720996407E-16 ) ) ;
#16428 = CARTESIAN_POINT ( 'NONE',  ( -4.193516549646675529, 11.11351654964658842, 455.0000000000000568 ) ) ;
#16429 = LINE ( 'NONE', #69471, #1402 ) ;
#16430 = ORIENTED_EDGE ( 'NONE', *, *, #66758, .F. ) ;
#16431 = PRESENTATION_LAYER_ASSIGNMENT (  '', '', ( #46891 ) ) ;
#16432 = CARTESIAN_POINT ( 'NONE',  ( 9.703773737882817940, 10.03972626211715280, 54.00000000000000711 ) ) ;
#16433 = LINE ( 'NONE', #54615, #56716 ) ;
#16434 = ORIENTED_EDGE ( 'NONE', *, *, #28797, .T. ) ;
#16435 = VERTEX_POINT ( 'NONE', #59449 ) ;
#16436 = ORIENTED_EDGE ( 'NONE', *, *, #47893, .F. ) ;
#16437 = DIRECTION ( 'NONE',  ( 0.4999999999999973910, -0.8660254037844401509, -2.509347957447878791E-16 ) ) ;
#16438 = LINE ( 'NONE', #38692, #59749 ) ;
#16439 = SHAPE_REPRESENTATION_RELATIONSHIP ( 'NONE' , 'NONE' ,  #62481, #28414 ) ;
#16440 = VERTEX_POINT ( 'NONE', #21627 ) ;
#16441 = ORIENTED_EDGE ( 'NONE', *, *, #55038, .F. ) ;
#16442 = AXIS2_PLACEMENT_3D ( 'NONE', #32803, #49068, #994 ) ;
#16443 = VERTEX_POINT ( 'NONE', #38241 ) ;
#16444 = DIRECTION ( 'NONE',  ( 0.000000000000000000, 0.000000000000000000, -1.000000000000000000 ) ) ;
#16445 = VERTEX_POINT ( 'NONE', #27613 ) ;
#16446 = AXIS2_PLACEMENT_3D ( 'NONE', #8214, #41093, #62658 ) ;
#16447 = ORIENTED_EDGE ( 'NONE', *, *, #62194, .F. ) ;
#16448 = ORIENTED_EDGE ( 'NONE', *, *, #13941, .T. ) ;
#16449 = ORIENTED_EDGE ( 'NONE', *, *, #17579, .F. ) ;
#16450 = AXIS2_PLACEMENT_3D ( 'NONE', #44045, #1272, #50398 ) ;
#16451 = CYLINDRICAL_SURFACE ( 'NONE', #66587, 4.000000000000000000 ) ;
#16453 = ORIENTED_EDGE ( 'NONE', *, *, #46788, .T. ) ;
#16452 = CARTESIAN_POINT ( 'NONE',  ( -30.00000000000000000, -9.199999999999999289, -12.69999999999986073 ) ) ;
#16454 = EDGE_CURVE ( 'NONE', #42459, #32586, #49186, .T. ) ;
#16455 = DIRECTION ( 'NONE',  ( 0.000000000000000000, -0.1111111111108840643, -0.9938079899999319178 ) ) ;
#16456 = CIRCLE ( 'NONE', #5153, 0.3499999999999597877 ) ;
#16457 = AXIS2_PLACEMENT_3D ( 'NONE', #21867, #4576, #69627 ) ;
#16458 = VECTOR ( 'NONE', #59500, 1000.000000000000000 ) ;
#16459 = DIRECTION ( 'NONE',  ( 1.000000000000000000, -0.000000000000000000, -0.000000000000000000 ) ) ;
#16460 = CARTESIAN_POINT ( 'NONE',  ( 15.00000000000000000, -21.00000000000000000, 0.000000000000000000 ) ) ;
#16461 = EDGE_CURVE ( 'NONE', #42683, #46897, #41072, .T. ) ;
#16462 = ORIENTED_EDGE ( 'NONE', *, *, #980, .T. ) ;
#16463 = AXIS2_PLACEMENT_3D ( 'NONE', #26464, #52646, #59330 ) ;
#16464 = AXIS2_PLACEMENT_3D ( 'NONE', #28922, #24325, #14053 ) ;
#16465 = VECTOR ( 'NONE', #60845, 1000.000000000000000 ) ;
#16466 = EDGE_CURVE ( 'NONE', #3957, #67695, #38576, .T. ) ;
#16467 = CARTESIAN_POINT ( 'NONE',  ( -7.517976262117247899, -3.848229544836279992, 26.00000000000000711 ) ) ;
#16468 = VECTOR ( 'NONE', #21489, 1000.000000000000000 ) ;
#16469 = EDGE_CURVE ( 'NONE', #17972, #25470, #27963, .T. ) ;
#16470 = ORIENTED_EDGE ( 'NONE', *, *, #27800, .T. ) ;
#16471 = FACE_BOUND ( 'NONE', #48150, .T. ) ;
#16472 = AXIS2_PLACEMENT_3D ( 'NONE', #44632, #39342, #60902 ) ;
#16473 = CARTESIAN_POINT ( 'NONE',  ( -7.450000000000001954, 0.000000000000000000, -16.50000000000000000 ) ) ;
#16474 = CARTESIAN_POINT ( 'NONE',  ( -8.250000000000001776, 0.000000000000000000, -16.50000000000000000 ) ) ;
#16475 = ORIENTED_EDGE ( 'NONE', *, *, #11771, .F. ) ;
#16476 = CIRCLE ( 'NONE', #55985, 24.99999999998789946 ) ;
#16477 = CARTESIAN_POINT ( 'NONE',  ( 0.5000000000000000000, 18.00000000000000355, 21.00000000000000000 ) ) ;
#16478 = FACE_OUTER_BOUND ( 'NONE', #32337, .T. ) ;
#16479 = DIRECTION ( 'NONE',  ( 0.000000000000000000, -1.000000000000000000, 0.000000000000000000 ) ) ;
#16480 = EDGE_CURVE ( 'NONE', #20953, #7495, #1095, .T. ) ;
#16481 = FACE_OUTER_BOUND ( 'NONE', #13306, .T. ) ;
#16482 = FACE_OUTER_BOUND ( 'NONE', #42699, .T. ) ;
#16483 = LINE ( 'NONE', #55018, #14729 ) ;
#16484 = CARTESIAN_POINT ( 'NONE',  ( 8.241237374594247100, 1.620245201994230611, 54.00000000000000711 ) ) ;
#16485 = DIRECTION ( 'NONE',  ( 0.6414496315691619044, -0.7671651518152962090, 0.000000000000000000 ) ) ;
#16486 = VERTEX_POINT ( 'NONE', #60474 ) ;
#16487 = DIRECTION ( 'NONE',  ( 0.000000000000000000, 0.000000000000000000, 1.000000000000000000 ) ) ;
#16488 = AXIS2_PLACEMENT_3D ( 'NONE', #51779, #2628, #23848 ) ;
#16489 = CARTESIAN_POINT ( 'NONE',  ( -30.00000000000000000, -15.46862696659690073, -14.50000000000000000 ) ) ;
#16490 = FACE_OUTER_BOUND ( 'NONE', #61099, .T. ) ;
#16491 = DIRECTION ( 'NONE',  ( -1.000000000000000000, 0.000000000000000000, 0.000000000000000000 ) ) ;
#16492 = EDGE_LOOP ( 'NONE', ( #65045, #5562, #54377, #32769 ) ) ;
#16493 = CARTESIAN_POINT ( 'NONE',  ( 31.89999999999999858, -14.06939075806900874, 20.80000000000001137 ) ) ;
#16494 = DIRECTION ( 'NONE',  ( -1.000000000000000000, 0.000000000000000000, 0.000000000000000000 ) ) ;
#16495 = AXIS2_PLACEMENT_3D ( 'NONE', #28480, #61003, #12563 ) ;
#16496 = CARTESIAN_POINT ( 'NONE',  ( 290.0000000000000000, -0.5000000000000000000, 26.50000000000000000 ) ) ;
#16497 = CARTESIAN_POINT ( 'NONE',  ( 3.157023737882805214, 6.486996718459879574, 54.00000000000000711 ) ) ;
#16498 = VECTOR ( 'NONE', #6824, 1000.000000000000000 ) ;
#16499 = CARTESIAN_POINT ( 'NONE',  ( 151.5599459900709860, 0.000000000000000000, 278.4149360882130395 ) ) ;
#16500 = CYLINDRICAL_SURFACE ( 'NONE', #58814, 0.3999999999999993006 ) ;
#16501 = EDGE_CURVE ( 'NONE', #25138, #33710, #55709, .T. ) ;
#16502 = VERTEX_POINT ( 'NONE', #22991 ) ;
#16503 = ADVANCED_FACE ( 'NONE', ( #1771, #34636 ), #35323, .T. ) ;
#16504 = CIRCLE ( 'NONE', #68441, 0.5000000000000000000 ) ;
#16505 = AXIS2_PLACEMENT_3D ( 'NONE', #68896, #36007, #25408 ) ;
#16506 = VERTEX_POINT ( 'NONE', #8110 ) ;
#16507 = CARTESIAN_POINT ( 'NONE',  ( 7.606483450353424658, 11.77351654964657435, 455.0000000000000568 ) ) ;
#16508 = LINE ( 'NONE', #244, #8601 ) ;
#16509 = ORIENTED_EDGE ( 'NONE', *, *, #45677, .F. ) ;
#16510 = EDGE_CURVE ( 'NONE', #6826, #13374, #52346, .T. ) ;
#16511 = AXIS2_PLACEMENT_3D ( 'NONE', #68813, #58907, #52919 ) ;
#16512 = AXIS2_PLACEMENT_3D ( 'NONE', #56506, #29627, #23625 ) ;
#16513 = CYLINDRICAL_SURFACE ( 'NONE', #11530, 0.7112000000000124889 ) ;
#16514 = VERTEX_POINT ( 'NONE', #8460 ) ;
#16515 = VECTOR ( 'NONE', #49664, 1000.000000000000000 ) ;
#16516 = CARTESIAN_POINT ( 'NONE',  ( -15.50000000000000000, 0.000000000000000000, 22.50000000000000000 ) ) ;
#16517 = ORIENTED_EDGE ( 'NONE', *, *, #60886, .F. ) ;
#16518 = ORIENTED_EDGE ( 'NONE', *, *, #17384, .F. ) ;
#16519 = CARTESIAN_POINT ( 'NONE',  ( -30.00000000000000000, -11.85423089348099879, 9.852125413066602277 ) ) ;
#16520 = VERTEX_POINT ( 'NONE', #50570 ) ;
#16521 = DIRECTION ( 'NONE',  ( 0.000000000000000000, 0.000000000000000000, 1.000000000000000000 ) ) ;
#16522 = DIRECTION ( 'NONE',  ( 1.000000000000000000, 0.000000000000000000, 0.000000000000000000 ) ) ;
#16523 = DIRECTION ( 'NONE',  ( 0.000000000000000000, -1.000000000000000000, 0.000000000000000000 ) ) ;
#16524 = VECTOR ( 'NONE', #39510, 1000.000000000000000 ) ;
#16525 = VERTEX_POINT ( 'NONE', #56221 ) ;
#16526 = EDGE_LOOP ( 'NONE', ( #25562, #1134, #30132, #60537 ) ) ;
#16527 = DIRECTION ( 'NONE',  ( 0.000000000000000000, 0.000000000000000000, 1.000000000000000000 ) ) ;
#16529 = DIRECTION ( 'NONE',  ( 0.000000000000000000, -1.000000000000000000, 0.000000000000000000 ) ) ;
#16528 = CYLINDRICAL_SURFACE ( 'NONE', #65479, 25.39999999999999858 ) ;
#16530 = EDGE_LOOP ( 'NONE', ( #9629, #47628, #41732, #6184 ) ) ;
#16531 = ORIENTED_EDGE ( 'NONE', *, *, #20942, .T. ) ;
#16533 = ORIENTED_EDGE ( 'NONE', *, *, #6896, .F. ) ;
#16532 = ITEM_DEFINED_TRANSFORMATION ( 'NONE', 'NONE', #12094,  #45918 ) ;
#16534 = CARTESIAN_POINT ( 'NONE',  ( 1.690483450353344352, -10.74648345035345720, 455.0000000000000568 ) ) ;
#16536 = ORIENTED_EDGE ( 'NONE', *, *, #5120, .T. ) ;
#16535 = CARTESIAN_POINT ( 'NONE',  ( 7.450000000000003730, -7.249999999999997335, -14.50000000000000000 ) ) ;
#16537 = EDGE_CURVE ( 'NONE', #50609, #37532, #28991, .T. ) ;
#16538 = CARTESIAN_POINT ( 'NONE',  ( 41.09999999999999432, -21.00000000000000000, 13.86939075806900057 ) ) ;
#16539 = CARTESIAN_POINT ( 'NONE',  ( 7.250000000000005329, -7.249999999999998224, -23.00000000000000000 ) ) ;
#16540 = ORIENTED_EDGE ( 'NONE', *, *, #53113, .F. ) ;
#16541 =( GEOMETRIC_REPRESENTATION_CONTEXT ( 3 ) GLOBAL_UNCERTAINTY_ASSIGNED_CONTEXT ( ( #30968 ) ) GLOBAL_UNIT_ASSIGNED_CONTEXT ( ( #9341, #58837, #63083 ) ) REPRESENTATION_CONTEXT ( 'NONE', 'WORKASPACE' ) );
#16542 = ORIENTED_EDGE ( 'NONE', *, *, #27632, .T. ) ;
#16543 = ADVANCED_FACE ( 'NONE', ( #30042 ), #61154, .T. ) ;
#16544 = DIRECTION ( 'NONE',  ( -1.000000000000000000, 0.000000000000000000, 0.000000000000000000 ) ) ;
#16545 = CIRCLE ( 'NONE', #24461, 1.000000000000000000 ) ;
#16546 = EDGE_CURVE ( 'NONE', #23407, #47795, #66473, .T. ) ;
#16547 = ADVANCED_FACE ( 'NONE', ( #23679 ), #24742, .F. ) ;
#16548 = EDGE_LOOP ( 'NONE', ( #5491, #38442, #57729, #36394 ) ) ;
#16549 = LINE ( 'NONE', #11559, #45055 ) ;
#16550 = DIRECTION ( 'NONE',  ( 1.836970198721029934E-16, 1.836970198721010706E-16, -1.000000000000000000 ) ) ;
#16551 = CIRCLE ( 'NONE', #66252, 1.224999999999999423 ) ;
#16552 = VECTOR ( 'NONE', #32894, 1000.000000000000000 ) ;
#16553 = EDGE_CURVE ( 'NONE', #23324, #20521, #19617, .T. ) ;
#16554 = EDGE_CURVE ( 'NONE', #32897, #2702, #34983, .T. ) ;
#16555 = ORIENTED_EDGE ( 'NONE', *, *, #5131, .F. ) ;
#16556 = CIRCLE ( 'NONE', #4096, 1.000000000000000000 ) ;
#16557 = VECTOR ( 'NONE', #48850, 999.9999999999998863 ) ;
#16558 = EDGE_CURVE ( 'NONE', #17972, #46144, #26398, .T. ) ;
#16559 = CARTESIAN_POINT ( 'NONE',  ( 7.250000000000005329, 8.250000000000001776, -12.50000000000000000 ) ) ;
#16561 = ORIENTED_EDGE ( 'NONE', *, *, #65586, .F. ) ;
#16560 = CARTESIAN_POINT ( 'NONE',  ( 290.0000000000000000, 3.233000000000000096, 0.000000000000000000 ) ) ;
#16562 = ORIENTED_EDGE ( 'NONE', *, *, #10860, .T. ) ;
#16563 = CARTESIAN_POINT ( 'NONE',  ( -29.50000000000000355, -11.50000000000100009, 15.00000000000084910 ) ) ;
#16564 = AXIS2_PLACEMENT_3D ( 'NONE', #38643, #17408, #60544 ) ;
#16565 = CIRCLE ( 'NONE', #12045, 0.3499999999999996447 ) ;
#16566 = CARTESIAN_POINT ( 'NONE',  ( 283.0000000000000568, -26.28355339059299922, 9.766446609406699508 ) ) ;
#16567 = CARTESIAN_POINT ( 'NONE',  ( 9.737023737882804397, 6.817976262117185549, 54.00000000000000711 ) ) ;
#16568 = DIRECTION ( 'NONE',  ( 0.000000000000000000, 0.000000000000000000, -1.000000000000000000 ) ) ;
#16569 = AXIS2_PLACEMENT_3D ( 'NONE', #59761, #48814, #11313 ) ;
#16570 = CARTESIAN_POINT ( 'NONE',  ( -1.466476262117230034, 9.390476262117152473, 54.00000000000000711 ) ) ;
#16571 = ORIENTED_EDGE ( 'NONE', *, *, #18681, .T. ) ;
#16572 = DIRECTION ( 'NONE',  ( 0.000000000000000000, 1.000000000000000000, 0.000000000000000000 ) ) ;
#16573 = DIRECTION ( 'NONE',  ( 1.836970198721029934E-16, 1.836970198721010706E-16, -1.000000000000000000 ) ) ;
#16574 = DIRECTION ( 'NONE',  ( 1.836970198721029934E-16, 1.836970198721010706E-16, -1.000000000000000000 ) ) ;
#16576 = ORIENTED_EDGE ( 'NONE', *, *, #40898, .T. ) ;
#16575 = LINE ( 'NONE', #32822, #69500 ) ;
#16577 = AXIS2_PLACEMENT_3D ( 'NONE', #5697, #66108, #21607 ) ;
#16578 = CARTESIAN_POINT ( 'NONE',  ( 30.00000000000000000, -13.54524521594299991, 17.53999999999999915 ) ) ;
#16579 = LINE ( 'NONE', #11931, #52922 ) ;
#16580 = DIRECTION ( 'NONE',  ( 0.000000000000000000, 0.000000000000000000, 1.000000000000000000 ) ) ;
#16581 = DIRECTION ( 'NONE',  ( 0.000000000000000000, 0.7071067811865454633, 0.7071067811865496822 ) ) ;
#16582 = VERTEX_POINT ( 'NONE', #46299 ) ;
#16583 = LINE ( 'NONE', #665, #9487 ) ;
#16584 = CARTESIAN_POINT ( 'NONE',  ( 49.00000000000000000, -21.00000000000000000, 13.86939075806900057 ) ) ;
#16585 = ORIENTED_EDGE ( 'NONE', *, *, #5113, .T. ) ;
#16587 = DIRECTION ( 'NONE',  ( 0.000000000000000000, 0.7278708115913771204, 0.6857142857147648929 ) ) ;
#16586 = B_SPLINE_CURVE_WITH_KNOTS ( 'NONE', 3,
 ( #65002, #17582, #22217, #49438, #6290, #17926 ),
 .UNSPECIFIED., .F., .F.,
 ( 4, 2, 4 ),
 ( 0.0002380763768129734448, 0.7291065797294591366, 1.457975083082105439 ),
 .UNSPECIFIED. ) ;
#16588 = FACE_OUTER_BOUND ( 'NONE', #40572, .T. ) ;
#16589 = DIRECTION ( 'NONE',  ( -1.610765207321970913E-14, -1.000000000000000000, -1.836970198721006761E-16 ) ) ;
#16590 = LINE ( 'NONE', #23264, #48613 ) ;
#16591 = CARTESIAN_POINT ( 'NONE',  ( 0.000000000000000000, -21.00000000000000000, 0.000000000000000000 ) ) ;
#16592 = EDGE_CURVE ( 'NONE', #373, #43590, #18367, .T. ) ;
#16593 = VERTEX_POINT ( 'NONE', #40991 ) ;
#16594 = ORIENTED_EDGE ( 'NONE', *, *, #49192, .F. ) ;
#16595 = CARTESIAN_POINT ( 'NONE',  ( -2.277516549646682709, 9.828310488885916740, 455.0000000000000568 ) ) ;
#16596 = VERTEX_POINT ( 'NONE', #34279 ) ;
#16597 = CARTESIAN_POINT ( 'NONE',  ( 8.711985858128693749, -8.093267424590470327, 54.00000000000000711 ) ) ;
#16598 = AXIS2_PLACEMENT_3D ( 'NONE', #55178, #1421, #6720 ) ;
#16599 = VERTEX_POINT ( 'NONE', #61501 ) ;
#16600 = EDGE_CURVE ( 'NONE', #60100, #60377, #53517, .T. ) ;
#16601 = CARTESIAN_POINT ( 'NONE',  ( 15.50000000000000000, -1.037157890325000054, -22.50000000000000000 ) ) ;
#16602 = EDGE_CURVE ( 'NONE', #15679, #35535, #23003, .T. ) ;
#16603 = VECTOR ( 'NONE', #10897, 1000.000000000000114 ) ;
#16604 = EDGE_CURVE ( 'NONE', #7028, #57266, #7766, .T. ) ;
#16605 = CARTESIAN_POINT ( 'NONE',  ( 3.857023737882783188, -9.912023737882810437, 54.00000000000000711 ) ) ;
#16606 = VECTOR ( 'NONE', #27179, 1000.000000000000000 ) ;
#16607 = AXIS2_PLACEMENT_3D ( 'NONE', #59685, #69941, #64301 ) ;
#16608 = CARTESIAN_POINT ( 'NONE',  ( 15.50000000000000000, -17.50000000000000000, -22.50000000000000000 ) ) ;
#16609 = VERTEX_POINT ( 'NONE', #67169 ) ;
#16610 = EDGE_LOOP ( 'NONE', ( #21556, #15602, #63803, #26514, #16006, #29617, #18176, #18660, #38945, #27742, #27673, #32545, #22146, #42238, #58853, #36482, #29033, #30783, #47655, #11745 ) ) ;
#16611 = CARTESIAN_POINT ( 'NONE',  ( 8.930623737882818602, -9.703773737882825046, 54.00000000000000711 ) ) ;
#16612 = EDGE_LOOP ( 'NONE', ( #46337, #55972, #53731, #12129, #30791, #317, #5263, #10516 ) ) ;
#16613 = ORIENTED_EDGE ( 'NONE', *, *, #19080, .T. ) ;
#16614 = CIRCLE ( 'NONE', #69665, 0.2000000000000005107 ) ;
#16615 = AXIS2_PLACEMENT_3D ( 'NONE', #10617, #43481, #65075 ) ;
#16616 = CARTESIAN_POINT ( 'NONE',  ( 26.90000000000000213, -14.06939075806900163, -20.80000000000000426 ) ) ;
#16617 = DIRECTION ( 'NONE',  ( -1.000000000000000000, 0.000000000000000000, 0.000000000000000000 ) ) ;
#16618 = CARTESIAN_POINT ( 'NONE',  ( -7.593516549646831315, -11.32648345035340931, 455.0000000000000568 ) ) ;
#16619 = PRODUCT_DEFINITION_FORMATION_WITH_SPECIFIED_SOURCE ( 'ANY', '', #67289, .NOT_KNOWN. ) ;
#16620 = ORIENTED_EDGE ( 'NONE', *, *, #37530, .T. ) ;
#16621 = DIRECTION ( 'NONE',  ( -0.000000000000000000, 3.673940397442059868E-16, -1.000000000000000000 ) ) ;
#16622 = AXIS2_PLACEMENT_3D ( 'NONE', #52202, #22977, #51510 ) ;
#16623 = VECTOR ( 'NONE', #17968, 1000.000000000000000 ) ;
#16625 = PLANE ( 'NONE',  #38957 ) ;
#16624 = DIRECTION ( 'NONE',  ( -1.000000000000000000, 0.000000000000000000, 0.000000000000000000 ) ) ;
#16626 = ORIENTED_EDGE ( 'NONE', *, *, #42574, .F. ) ;
#16627 = ORIENTED_EDGE ( 'NONE', *, *, #15718, .T. ) ;
#16629 = EDGE_LOOP ( 'NONE', ( #17173, #44263, #9659, #58119 ) ) ;
#16628 = DIRECTION ( 'NONE',  ( 1.836970198721029934E-16, 1.836970198721010706E-16, -1.000000000000000000 ) ) ;
#16630 = ORIENTED_EDGE ( 'NONE', *, *, #53658, .T. ) ;
#16631 = AXIS2_PLACEMENT_3D ( 'NONE', #23569, #60709, #12598 ) ;
#16632 = CARTESIAN_POINT ( 'NONE',  ( 8.250000000000005329, 0.000000000000000000, -7.500000000000000000 ) ) ;
#16633 = CIRCLE ( 'NONE', #42612, 1.399999999999998579 ) ;
#16634 = DIRECTION ( 'NONE',  ( -1.000000000000000000, 0.000000000000000000, 0.000000000000000000 ) ) ;
#16635 = ORIENTED_EDGE ( 'NONE', *, *, #50212, .T. ) ;
#16636 = VERTEX_POINT ( 'NONE', #18731 ) ;
#16637 = DIRECTION ( 'NONE',  ( 0.000000000000000000, -3.673940397442059868E-16, 1.000000000000000000 ) ) ;
#16638 = CARTESIAN_POINT ( 'NONE',  ( -14.25000000000000000, -2.500000000000000000, -23.22168783648699986 ) ) ;
#16639 = ORIENTED_EDGE ( 'NONE', *, *, #63248, .T. ) ;
#16640 = CARTESIAN_POINT ( 'NONE',  ( -7.250000000000000000, -7.449999999999998401, -16.50000000000000000 ) ) ;
#16641 = CARTESIAN_POINT ( 'NONE',  ( -11.00000000000000000, -8.959999999999999076, 12.95475478405700009 ) ) ;
#16642 = DIRECTION ( 'NONE',  ( 0.000000000000000000, 1.000000000000000000, -1.500535806722257514E-12 ) ) ;
#16643 = EDGE_CURVE ( 'NONE', #42714, #12586, #40298, .T. ) ;
#16644 = ORIENTED_EDGE ( 'NONE', *, *, #36231, .F. ) ;
#16645 = EDGE_CURVE ( 'NONE', #46863, #51495, #56563, .T. ) ;
#16646 = PLANE ( 'NONE',  #7490 ) ;
#16647 = CARTESIAN_POINT ( 'NONE',  ( 50.83090410532631864, 63.65740854044500452, 10.00000000000000000 ) ) ;
#16648 =( GEOMETRIC_REPRESENTATION_CONTEXT ( 3 ) GLOBAL_UNCERTAINTY_ASSIGNED_CONTEXT ( ( #9048 ) ) GLOBAL_UNIT_ASSIGNED_CONTEXT ( ( #29858, #50723, #30223 ) ) REPRESENTATION_CONTEXT ( 'NONE', 'WORKASPACE' ) );
#16650 = ORIENTED_EDGE ( 'NONE', *, *, #7023, .T. ) ;
#16649 = DIRECTION ( 'NONE',  ( -0.000000000000000000, 3.673940397442059868E-16, -1.000000000000000000 ) ) ;
#16652 = ORIENTED_EDGE ( 'NONE', *, *, #47282, .T. ) ;
#16651 = LINE ( 'NONE', #27590, #14328 ) ;
#16653 = FACE_OUTER_BOUND ( 'NONE', #37410, .T. ) ;
#16654 = LINE ( 'NONE', #20900, #60031 ) ;
#16655 = DIRECTION ( 'NONE',  ( -1.000000000000000000, 0.000000000000000000, 0.000000000000000000 ) ) ;
#16656 = FACE_OUTER_BOUND ( 'NONE', #25776, .T. ) ;
#16657 = CARTESIAN_POINT ( 'NONE',  ( 9.689999999999999503, -10.50000000000000178, -4.250000000000000000 ) ) ;
#16658 = VECTOR ( 'NONE', #10818, 1000.000000000000000 ) ;
#16659 = VECTOR ( 'NONE', #39484, 1000.000000000000000 ) ;
#16660 = CARTESIAN_POINT ( 'NONE',  ( 6.358413763958955300, 5.779227145995228021, 26.00000000000000711 ) ) ;
#16661 = EDGE_LOOP ( 'NONE', ( #3820, #53255, #23229, #36490 ) ) ;
#16662 = LINE ( 'NONE', #22645, #46264 ) ;
#16664 = ORIENTED_EDGE ( 'NONE', *, *, #29456, .T. ) ;
#16663 = CARTESIAN_POINT ( 'NONE',  ( -5.779227145995285753, 6.344366288193340253, 26.00000000000000711 ) ) ;
#16665 = CIRCLE ( 'NONE', #11049, 1.000000000000000000 ) ;
#16668 = ORIENTED_EDGE ( 'NONE', *, *, #47533, .F. ) ;
#16667 = CARTESIAN_POINT ( 'NONE',  ( 7.357023737882817827, -5.552858015815587578, 54.00000000000000711 ) ) ;
#16666 = VECTOR ( 'NONE', #38040, 1000.000000000000000 ) ;
#16669 = CARTESIAN_POINT ( 'NONE',  ( 10.92648345035340895, 9.293516549646565039, 455.0000000000000568 ) ) ;
#16670 = ORIENTED_EDGE ( 'NONE', *, *, #30793, .F. ) ;
#16671 = CARTESIAN_POINT ( 'NONE',  ( 4.149127210878726935, -3.677663764522648204, 54.00000000000000711 ) ) ;
#16672 = VECTOR ( 'NONE', #38722, 1000.000000000000000 ) ;
#16673 = VECTOR ( 'NONE', #42341, 1000.000000000000114 ) ;
#16674 = EDGE_LOOP ( 'NONE', ( #16856, #38623, #48489, #14343 ) ) ;
#16675 = CARTESIAN_POINT ( 'NONE',  ( 8.406483450353398723, 5.655420232009111814, 455.0000000000000568 ) ) ;
#16676 = LINE ( 'NONE', #37889, #63339 ) ;
#16677 = ORIENTED_EDGE ( 'NONE', *, *, #21981, .T. ) ;
#16678 = DIRECTION ( 'NONE',  ( -1.000000000000000000, 0.000000000000000000, 0.000000000000000000 ) ) ;
#16679 = CARTESIAN_POINT ( 'NONE',  ( -7.798499376344067535, 7.259684009079840017, 195.0000000000000284 ) ) ;
#16680 = DIRECTION ( 'NONE',  ( 0.000000000000000000, 0.000000000000000000, 1.000000000000000000 ) ) ;
#16681 = CARTESIAN_POINT ( 'NONE',  ( 7.450000000000003730, -7.249999999999997335, -15.50000000000000000 ) ) ;
#16682 = AXIS2_PLACEMENT_3D ( 'NONE', #11497, #21082, #16825 ) ;
#16683 = ORIENTED_EDGE ( 'NONE', *, *, #41042, .F. ) ;
#16684 = FACE_OUTER_BOUND ( 'NONE', #8515, .T. ) ;
#16685 = ORIENTED_EDGE ( 'NONE', *, *, #15561, .T. ) ;
#16686 = ORIENTED_EDGE ( 'NONE', *, *, #35755, .F. ) ;
#16687 = FACE_OUTER_BOUND ( 'NONE', #49250, .T. ) ;
#16688 = LINE ( 'NONE', #48860, #60226 ) ;
#16689 = EDGE_CURVE ( 'NONE', #39691, #50336, #19084, .T. ) ;
#16690 = DIRECTION ( 'NONE',  ( 0.000000000000000000, -1.000000000000000000, 6.036837696397648868E-13 ) ) ;
#16691 = DIRECTION ( 'NONE',  ( 0.000000000000000000, -1.000000000000000000, 0.000000000000000000 ) ) ;
#16692 = VERTEX_POINT ( 'NONE', #53376 ) ;
#16693 = ORIENTED_EDGE ( 'NONE', *, *, #42767, .T. ) ;
#16695 = ORIENTED_EDGE ( 'NONE', *, *, #1685, .T. ) ;
#16694 = CARTESIAN_POINT ( 'NONE',  ( 9.247904806590677040, 9.942044687070474396, 195.0000000000000284 ) ) ;
#16696 = VERTEX_POINT ( 'NONE', #4927 ) ;
#16697 = DIRECTION ( 'NONE',  ( 0.000000000000000000, 0.000000000000000000, 1.000000000000000000 ) ) ;
#16698 = CARTESIAN_POINT ( 'NONE',  ( 41.09999999999999432, 13.66939075806899950, -20.80000000000000426 ) ) ;
#16699 = DIRECTION ( 'NONE',  ( -1.000000000000000000, 0.000000000000000000, 0.000000000000000000 ) ) ;
#16700 = AXIS2_PLACEMENT_3D ( 'NONE', #42917, #37280, #64498 ) ;
#16701 = ADVANCED_FACE ( 'NONE', ( #31109 ), #62921, .T. ) ;
#16703 = DIRECTION ( 'NONE',  ( 0.000000000000000000, 1.000000000000000000, 0.000000000000000000 ) ) ;
#16702 = LINE ( 'NONE', #38269, #68204 ) ;
#16704 = VERTEX_POINT ( 'NONE', #15552 ) ;
#16706 = EDGE_LOOP ( 'NONE', ( #31787, #9427 ) ) ;
#16705 = DIRECTION ( 'NONE',  ( -0.000000000000000000, 0.000000000000000000, -1.000000000000000000 ) ) ;
#16707 = ORIENTED_EDGE ( 'NONE', *, *, #38202, .F. ) ;
#16708 = ORIENTED_EDGE ( 'NONE', *, *, #5484, .T. ) ;
#16709 = EDGE_CURVE ( 'NONE', #7460, #1302, #64327, .T. ) ;
#16710 = CARTESIAN_POINT ( 'NONE',  ( -8.227189898828745740, 1.620245201994245043, 54.00000000000000711 ) ) ;
#16711 = CARTESIAN_POINT ( 'NONE',  ( 30.00000000000000000, -17.00000000000000000, 15.70499999999969809 ) ) ;
#16712 = VECTOR ( 'NONE', #34295, 1000.000000000000000 ) ;
#16713 = VECTOR ( 'NONE', #43240, 1000.000000000000000 ) ;
#16714 = CARTESIAN_POINT ( 'NONE',  ( -1.077516549646825750, -10.74648345035347852, 455.0000000000000568 ) ) ;
#16715 = ORIENTED_EDGE ( 'NONE', *, *, #24261, .T. ) ;
#16717 = ORIENTED_EDGE ( 'NONE', *, *, #56385, .F. ) ;
#16716 = AXIS2_PLACEMENT_3D ( 'NONE', #12693, #33248, #22973 ) ;
#16718 = VERTEX_POINT ( 'NONE', #31466 ) ;
#16719 = PLANE ( 'NONE',  #30558 ) ;
#16720 = AXIS2_PLACEMENT_3D ( 'NONE', #40385, #61942, #23430 ) ;
#16721 = LINE ( 'NONE', #59840, #41084 ) ;
#16722 = LINE ( 'NONE', #5763, #63901 ) ;
#16723 = ORIENTED_EDGE ( 'NONE', *, *, #52385, .T. ) ;
#16724 = ORIENTED_EDGE ( 'NONE', *, *, #8172, .T. ) ;
#16725 = DIRECTION ( 'NONE',  ( -1.000000000000000000, 0.000000000000000000, 0.000000000000000000 ) ) ;
#16726 = DIRECTION ( 'NONE',  ( 1.000000000000000000, 0.000000000000000000, 0.000000000000000000 ) ) ;
#16727 = ORIENTED_EDGE ( 'NONE', *, *, #52894, .T. ) ;
#16728 = EDGE_CURVE ( 'NONE', #29102, #56223, #9179, .T. ) ;
#16729 = AXIS2_PLACEMENT_3D ( 'NONE', #1582, #39756, #67351 ) ;
#16730 = EDGE_CURVE ( 'NONE', #65451, #64280, #63988, .T. ) ;
#16731 = LINE ( 'NONE', #6463, #33601 ) ;
#16732 = ADVANCED_FACE ( 'NONE', ( #57961 ), #36395, .F. ) ;
#16734 = VERTEX_POINT ( 'NONE', #9531 ) ;
#16733 = DIRECTION ( 'NONE',  ( -0.000000000000000000, 1.000000000000000000, -0.000000000000000000 ) ) ;
#16735 = ORIENTED_EDGE ( 'NONE', *, *, #5079, .F. ) ;
#16736 = CARTESIAN_POINT ( 'NONE',  ( -8.000000000000000000, -6.879816696376141572, 0.000000000000000000 ) ) ;
#16737 = CARTESIAN_POINT ( 'NONE',  ( 10.92648345035340895, 9.093516549646565750, 455.0000000000000568 ) ) ;
#16738 = EDGE_CURVE ( 'NONE', #32965, #49465, #48058, .T. ) ;
#16739 = DIRECTION ( 'NONE',  ( -1.000000000000000000, 0.000000000000000000, 0.000000000000000000 ) ) ;
#16740 = DIRECTION ( 'NONE',  ( -0.6414496315691617934, -0.7671651518152962090, -2.818519042763987834E-16 ) ) ;
#16741 = DIRECTION ( 'NONE',  ( 1.000000000000000000, 0.000000000000000000, 0.000000000000000000 ) ) ;
#16742 = EDGE_CURVE ( 'NONE', #40491, #38948, #68221, .T. ) ;
#16743 = ORIENTED_EDGE ( 'NONE', *, *, #24275, .F. ) ;
#16744 = CARTESIAN_POINT ( 'NONE',  ( 8.711985858128644011, 2.406732575409517239, 54.00000000000000711 ) ) ;
#16745 = ADVANCED_FACE ( 'NONE', ( #47006 ), #21195, .T. ) ;
#16746 = ORIENTED_EDGE ( 'NONE', *, *, #21042, .F. ) ;
#16747 = CARTESIAN_POINT ( 'NONE',  ( 181.4833316329832940, 9.000000000000001776, 284.4801873289890182 ) ) ;
#16748 = DIRECTION ( 'NONE',  ( 1.836970198721029934E-16, 1.836970198721010706E-16, -1.000000000000000000 ) ) ;
#16749 = AXIS2_PLACEMENT_3D ( 'NONE', #57703, #30834, #3968 ) ;
#16750 = CARTESIAN_POINT ( 'NONE',  ( 17.24945551514599984, -15.50000000000000000, -25.53140320652400064 ) ) ;
#16751 = DIRECTION ( 'NONE',  ( 1.836970198721029934E-16, 1.836970198721010706E-16, -1.000000000000000000 ) ) ;
#16752 = CARTESIAN_POINT ( 'NONE',  ( -11.07551654964683330, -11.48848345035333907, 455.0000000000000568 ) ) ;
#16753 = ORIENTED_EDGE ( 'NONE', *, *, #41560, .F. ) ;
#16754 = LINE ( 'NONE', #33008, #35858 ) ;
#16755 = AXIS2_PLACEMENT_3D ( 'NONE', #39523, #66746, #61084 ) ;
#16756 = ORIENTED_EDGE ( 'NONE', *, *, #34652, .F. ) ;
#16757 = CARTESIAN_POINT ( 'NONE',  ( 7.250000000000005329, -7.249999999999998224, -22.50000000000000000 ) ) ;
#16758 = EDGE_CURVE ( 'NONE', #27322, #5636, #41122, .T. ) ;
#16759 = DIRECTION ( 'NONE',  ( 1.000000000000000000, -0.000000000000000000, 0.000000000000000000 ) ) ;
#16760 = ORIENTED_EDGE ( 'NONE', *, *, #59966, .F. ) ;
#16761 = VECTOR ( 'NONE', #34614, 1000.000000000000000 ) ;
#16762 = CARTESIAN_POINT ( 'NONE',  ( -7.450000000000001954, 7.250000000000000000, -20.00000000000000000 ) ) ;
#16763 = DIRECTION ( 'NONE',  ( 0.000000000000000000, 0.000000000000000000, 1.000000000000000000 ) ) ;
#16764 = ORIENTED_EDGE ( 'NONE', *, *, #42126, .T. ) ;
#16765 = DIRECTION ( 'NONE',  ( -0.000000000000000000, 3.673940397442059868E-16, -1.000000000000000000 ) ) ;
#16766 = CARTESIAN_POINT ( 'NONE',  ( -7.250000000000000888, 7.450000000000003730, -18.50000000000000000 ) ) ;
#16767 = EDGE_CURVE ( 'NONE', #7560, #37330, #37113, .T. ) ;
#16768 = FILL_AREA_STYLE_COLOUR ( '', #50104 ) ;
#16769 = CYLINDRICAL_SURFACE ( 'NONE', #4651, 0.2000000000000000944 ) ;
#16770 = VERTEX_POINT ( 'NONE', #58675 ) ;
#16772 = VERTEX_POINT ( 'NONE', #20829 ) ;
#16771 = CARTESIAN_POINT ( 'NONE',  ( 10.50000000000000178, 9.690000000000001279, -5.000000000000000000 ) ) ;
#16773 = CIRCLE ( 'NONE', #27015, 7.800000000000000711 ) ;
#16774 = CARTESIAN_POINT ( 'NONE',  ( 7.000000000000000000, -24.99999999999915090, 9.080000000000110205 ) ) ;
#16775 = CARTESIAN_POINT ( 'NONE',  ( 14.45313394609757296, -0.2715358723599907709, -21.66103272505201005 ) ) ;
#16776 = FACE_OUTER_BOUND ( 'NONE', #47588, .T. ) ;
#16777 = EDGE_LOOP ( 'NONE', ( #5991, #16670, #10113, #15669 ) ) ;
#16778 = CARTESIAN_POINT ( 'NONE',  ( 8.406483450353348985, 5.655420232009159776, 195.0000000000000284 ) ) ;
#16779 = CARTESIAN_POINT ( 'NONE',  ( -7.250000000000000888, 8.250000000000001776, -25.50000000000000355 ) ) ;
#16780 = ORIENTED_EDGE ( 'NONE', *, *, #24857, .F. ) ;
#16781 = ORIENTED_EDGE ( 'NONE', *, *, #57492, .T. ) ;
#16782 = ORIENTED_EDGE ( 'NONE', *, *, #38279, .F. ) ;
#16783 = EDGE_CURVE ( 'NONE', #62655, #33710, #25444, .T. ) ;
#16784 = DIRECTION ( 'NONE',  ( 0.000000000000000000, 0.000000000000000000, -1.000000000000000000 ) ) ;
#16785 = DIRECTION ( 'NONE',  ( 1.000000000000000000, 0.000000000000000000, 0.000000000000000000 ) ) ;
#16786 = LINE ( 'NONE', #64197, #26998 ) ;
#16787 = SHAPE_REPRESENTATION_RELATIONSHIP ( 'NONE' , 'NONE' ,  #60228, #36842 ) ;
#16788 = EDGE_LOOP ( 'NONE', ( #41806, #49507, #55560, #4216 ) ) ;
#16790 = EDGE_CURVE ( 'NONE', #37085, #8763, #25282, .T. ) ;
#16789 = EDGE_LOOP ( 'NONE', ( #68367, #34776, #51288, #20697 ) ) ;
#16791 = VERTEX_POINT ( 'NONE', #63273 ) ;
#16792 = EDGE_CURVE ( 'NONE', #11614, #66887, #42750, .T. ) ;
#16793 = DIRECTION ( 'NONE',  ( 1.000000000000000000, 0.000000000000000000, 0.000000000000000000 ) ) ;
#16794 = ORIENTED_EDGE ( 'NONE', *, *, #12046, .F. ) ;
#16795 = ADVANCED_FACE ( 'NONE', ( #63631 ), #15190, .F. ) ;
#16796 = VERTEX_POINT ( 'NONE', #51965 ) ;
#16797 = EDGE_CURVE ( 'NONE', #45889, #2965, #47707, .T. ) ;
#16798 = EDGE_CURVE ( 'NONE', #8221, #64619, #5003, .T. ) ;
#16799 = VERTEX_POINT ( 'NONE', #49093 ) ;
#16800 = CIRCLE ( 'NONE', #39385, 1.000000000000000000 ) ;
#16801 = ORIENTED_EDGE ( 'NONE', *, *, #60194, .F. ) ;
#16802 = DIRECTION ( 'NONE',  ( -0.000000000000000000, 0.000000000000000000, -1.000000000000000000 ) ) ;
#16803 = UNCERTAINTY_MEASURE_WITH_UNIT (LENGTH_MEASURE( 1.000000000000000082E-05 ), #34449, 'distance_accuracy_value', 'NONE');
#16805 = VERTEX_POINT ( 'NONE', #59013 ) ;
#16804 = CARTESIAN_POINT ( 'NONE',  ( 3.857023737882783188, -9.912023737882801555, 26.00000000000000000 ) ) ;
#16806 = EDGE_CURVE ( 'NONE', #10944, #21570, #11937, .T. ) ;
#16807 = DIRECTION ( 'NONE',  ( 0.000000000000000000, 0.7046037717862339012, -0.7096009616570518874 ) ) ;
#16808 = CARTESIAN_POINT ( 'NONE',  ( -10.19191654964671301, 11.47551654964660450, 195.0000000000000284 ) ) ;
#16809 = EDGE_CURVE ( 'NONE', #48070, #67547, #5285, .T. ) ;
#16810 = DIRECTION ( 'NONE',  ( 0.000000000000000000, 0.000000000000000000, -1.000000000000000000 ) ) ;
#16811 = ORIENTED_EDGE ( 'NONE', *, *, #19955, .F. ) ;
#16812 = EDGE_CURVE ( 'NONE', #57801, #11904, #53563, .T. ) ;
#16813 = CIRCLE ( 'NONE', #22466, 4.000000000000000888 ) ;
#16814 = LINE ( 'NONE', #39401, #4103 ) ;
#16815 = ADVANCED_FACE ( 'NONE', ( #15882 ), #16921, .F. ) ;
#16816 = ORIENTED_EDGE ( 'NONE', *, *, #40814, .T. ) ;
#16817 = DIRECTION ( 'NONE',  ( 0.000000000000000000, 0.000000000000000000, -1.000000000000000000 ) ) ;
#16818 = EDGE_CURVE ( 'NONE', #4894, #7633, #37799, .T. ) ;
#16819 = CARTESIAN_POINT ( 'NONE',  ( 9.689999999999999503, -9.750000000000001776, -4.250000000000000000 ) ) ;
#16820 = CARTESIAN_POINT ( 'NONE',  ( 275.0000000000000000, -32.44999999999905071, -14.49999999999906031 ) ) ;
#16821 = LINE ( 'NONE', #38051, #26856 ) ;
#16822 = VERTEX_POINT ( 'NONE', #48409 ) ;
#16823 = DIRECTION ( 'NONE',  ( -1.000000000000000000, 0.000000000000000000, 0.000000000000000000 ) ) ;
#16824 = DIRECTION ( 'NONE',  ( 0.000000000000000000, 0.7071067811865470176, 0.7071067811865480168 ) ) ;
#16825 = DIRECTION ( 'NONE',  ( 0.000000000000000000, 0.000000000000000000, -1.000000000000000000 ) ) ;
#16826 = CARTESIAN_POINT ( 'NONE',  ( 7.250000000000005329, -7.249999999999998224, -9.000000000000001776 ) ) ;
#16827 = CARTESIAN_POINT ( 'NONE',  ( 10.31452373788281562, -3.664523737882826815, 54.00000000000000711 ) ) ;
#16828 = CARTESIAN_POINT ( 'NONE',  ( 9.417013320880792904, -1.866219381641466057, 195.0000000000000284 ) ) ;
#16829 = LINE ( 'NONE', #64926, #59267 ) ;
#16830 = CARTESIAN_POINT ( 'NONE',  ( -15.50000000000000000, -2.500000000000000000, 23.94337567297399971 ) ) ;
#16831 = ORIENTED_EDGE ( 'NONE', *, *, #3376, .F. ) ;
#16832 = CARTESIAN_POINT ( 'NONE',  ( 11.50000000000000000, -15.46862696659690073, -14.50000000000000000 ) ) ;
#16833 = DIRECTION ( 'NONE',  ( -0.7071067811865474617, 0.000000000000000000, 0.7071067811865474617 ) ) ;
#16834 = CARTESIAN_POINT ( 'NONE',  ( 39.90000000000000568, -14.06939075806900874, 20.80000000000001137 ) ) ;
#16835 = FACE_OUTER_BOUND ( 'NONE', #30485, .T. ) ;
#16836 = ORIENTED_EDGE ( 'NONE', *, *, #60550, .T. ) ;
#16837 = DIRECTION ( 'NONE',  ( -0.000000000000000000, 3.673940397442059868E-16, -1.000000000000000000 ) ) ;
#16838 = CARTESIAN_POINT ( 'NONE',  ( -7.342976262117253405, -3.848229544836288429, 54.00000000000000711 ) ) ;
#16839 = DIRECTION ( 'NONE',  ( 0.000000000000000000, 0.000000000000000000, -1.000000000000000000 ) ) ;
#16840 = VECTOR ( 'NONE', #23211, 1000.000000000000000 ) ;
#16841 = ADVANCED_FACE ( 'NONE', ( #22910 ), #17253, .T. ) ;
#16842 = DIRECTION ( 'NONE',  ( -1.000000000000000000, 1.828336019306068695E-14, -1.836970198720996407E-16 ) ) ;
#16843 = FACE_OUTER_BOUND ( 'NONE', #67646, .T. ) ;
#16844 = DIRECTION ( 'NONE',  ( 0.000000000000000000, 0.000000000000000000, 1.000000000000000000 ) ) ;
#16845 = VERTEX_POINT ( 'NONE', #16222 ) ;
#16846 = CIRCLE ( 'NONE', #68787, 2.215251240775983899 ) ;
#16847 = EDGE_CURVE ( 'NONE', #10498, #7825, #16583, .T. ) ;
#16848 = VERTEX_POINT ( 'NONE', #60378 ) ;
#16849 = CARTESIAN_POINT ( 'NONE',  ( 7.250000000000005329, -7.449999999999998401, -7.500000000000000000 ) ) ;
#16850 = CARTESIAN_POINT ( 'NONE',  ( -30.00000000000000000, -11.50000000000082068, -10.20500000000000007 ) ) ;
#16851 = ORIENTED_EDGE ( 'NONE', *, *, #53715, .F. ) ;
#16852 = ADVANCED_FACE ( 'NONE', ( #22235 ), #27528, .T. ) ;
#16853 = VECTOR ( 'NONE', #18805, 1000.000000000000000 ) ;
#16854 = DIRECTION ( 'NONE',  ( -1.000000000000000000, 3.491481338843132961E-15, 0.000000000000000000 ) ) ;
#16855 = EDGE_CURVE ( 'NONE', #68245, #43115, #65941, .T. ) ;
#16856 = ORIENTED_EDGE ( 'NONE', *, *, #64283, .T. ) ;
#16857 = AXIS2_PLACEMENT_3D ( 'NONE', #61752, #40529, #22884 ) ;
#16858 = FACE_OUTER_BOUND ( 'NONE', #23020, .T. ) ;
#16859 = ORIENTED_EDGE ( 'NONE', *, *, #32941, .F. ) ;
#16860 = EDGE_CURVE ( 'NONE', #6937, #11406, #51758, .T. ) ;
#16861 = ORIENTED_EDGE ( 'NONE', *, *, #44466, .T. ) ;
#16862 = FACE_OUTER_BOUND ( 'NONE', #66184, .T. ) ;
#16863 = VERTEX_POINT ( 'NONE', #59707 ) ;
#16864 = LINE ( 'NONE', #27127, #30892 ) ;
#16865 = AXIS2_PLACEMENT_3D ( 'NONE', #69808, #60219, #15714 ) ;
#16866 = CARTESIAN_POINT ( 'NONE',  ( -7.813516549646791098, -12.00648345035336284, 195.0000000000000284 ) ) ;
#16867 = LINE ( 'NONE', #65649, #35883 ) ;
#16868 = VERTEX_POINT ( 'NONE', #44461 ) ;
#16869 = EDGE_CURVE ( 'NONE', #4107, #4626, #37455, .T. ) ;
#16870 = VERTEX_POINT ( 'NONE', #10924 ) ;
#16871 = CARTESIAN_POINT ( 'NONE',  ( 41.09999999999999432, -0.2000000000000000111, 0.000000000000000000 ) ) ;
#16872 = EDGE_CURVE ( 'NONE', #67635, #26989, #11256, .T. ) ;
#16874 = CARTESIAN_POINT ( 'NONE',  ( -15.50000000000000000, 0.000000000000000000, -26.50000000000000000 ) ) ;
#16873 = CIRCLE ( 'NONE', #2171, 1.000000000000000000 ) ;
#16875 = ORIENTED_EDGE ( 'NONE', *, *, #31040, .F. ) ;
#16876 = VERTEX_POINT ( 'NONE', #5624 ) ;
#16877 = ADVANCED_FACE ( 'NONE', ( #33175 ), #65368, .F. ) ;
#16878 = ADVANCED_FACE ( 'NONE', ( #32832 ), #54412, .F. ) ;
#16879 = ORIENTED_EDGE ( 'NONE', *, *, #36628, .F. ) ;
#16880 = FACE_OUTER_BOUND ( 'NONE', #55484, .T. ) ;
#16882 = ORIENTED_EDGE ( 'NONE', *, *, #41933, .F. ) ;
#16881 = CARTESIAN_POINT ( 'NONE',  ( 7.450000000000006395, 7.250000000000000888, -13.50000000000000178 ) ) ;
#16883 = EDGE_CURVE ( 'NONE', #8452, #62514, #3831, .T. ) ;
#16884 = DIRECTION ( 'NONE',  ( -0.000000000000000000, -0.000000000000000000, 1.000000000000000000 ) ) ;
#16885 = CARTESIAN_POINT ( 'NONE',  ( -11.00000000000000000, -17.35230188589299871, -15.35019951917099945 ) ) ;
#16886 = CIRCLE ( 'NONE', #27076, 0.2000000000000000944 ) ;
#16887 = ORIENTED_EDGE ( 'NONE', *, *, #19970, .T. ) ;
#16888 = ORIENTED_EDGE ( 'NONE', *, *, #12538, .T. ) ;
#16889 = EDGE_LOOP ( 'NONE', ( #53109, #15055, #29342, #67810, #68772, #47785, #27332, #43367 ) ) ;
#16890 = DIRECTION ( 'NONE',  ( 0.000000000000000000, 1.000000000000000000, 0.000000000000000000 ) ) ;
#16891 = CARTESIAN_POINT ( 'NONE',  ( 7.000000000000000000, -37.61196062927500350, -8.008708659369300875 ) ) ;
#16892 = EDGE_CURVE ( 'NONE', #55579, #62792, #45507, .T. ) ;
#16893 = ORIENTED_EDGE ( 'NONE', *, *, #30659, .T. ) ;
#16894 = AXIS2_PLACEMENT_3D ( 'NONE', #48334, #63903, #63556 ) ;
#16895 = VECTOR ( 'NONE', #56500, 1000.000000000000114 ) ;
#16896 = EDGE_CURVE ( 'NONE', #60141, #49441, #12277, .T. ) ;
#16897 = CARTESIAN_POINT ( 'NONE',  ( 16.89999999999999858, -0.2000000000089119934, -8.913009219568841313E-12 ) ) ;
#16898 = DIRECTION ( 'NONE',  ( 0.000000000000000000, 0.000000000000000000, 1.000000000000000000 ) ) ;
#16900 = EDGE_LOOP ( 'NONE', ( #27648, #12667, #31752, #17094 ) ) ;
#16899 = LINE ( 'NONE', #48383, #22964 ) ;
#16901 = ORIENTED_EDGE ( 'NONE', *, *, #16537, .F. ) ;
#16902 = PLANE ( 'NONE',  #24965 ) ;
#16903 = AXIS2_PLACEMENT_3D ( 'NONE', #30736, #7756, #61860 ) ;
#16904 = LINE ( 'NONE', #46540, #26282 ) ;
#16905 = DIRECTION ( 'NONE',  ( -1.000000000000000000, 0.000000000000000000, 0.000000000000000000 ) ) ;
#16906 = CARTESIAN_POINT ( 'NONE',  ( 30.00000000000000000, -11.50000000000082068, 10.20500000000000007 ) ) ;
#16907 = AXIS2_PLACEMENT_3D ( 'NONE', #52325, #61509, #9187 ) ;
#16908 = CARTESIAN_POINT ( 'NONE',  ( -3.142976262117262998, -4.046023737882823212, 26.00000000000000711 ) ) ;
#16909 = ORIENTED_EDGE ( 'NONE', *, *, #59209, .F. ) ;
#16910 = CARTESIAN_POINT ( 'NONE',  ( 11.90000000000000036, 20.60000000000000142, -13.86939075806900057 ) ) ;
#16911 = CARTESIAN_POINT ( 'NONE',  ( 151.5599459900709860, 9.000000000000001776, 280.6301873289890523 ) ) ;
#16912 = LINE ( 'NONE', #64317, #53786 ) ;
#16913 = CIRCLE ( 'NONE', #16968, 0.5000000000001362244 ) ;
#16914 = CARTESIAN_POINT ( 'NONE',  ( 15.50000000000000000, -5.000000000000000000, 22.50000000000000000 ) ) ;
#16915 = CARTESIAN_POINT ( 'NONE',  ( 15.00000000000000000, 0.000000000000000000, 26.50000000000000000 ) ) ;
#16916 = CARTESIAN_POINT ( 'NONE',  ( -9.722976262117297708, -7.969523737882751924, 26.00000000000000000 ) ) ;
#16917 = CARTESIAN_POINT ( 'NONE',  ( 8.606483450353380249, -4.396432944014657451, 455.0000000000000568 ) ) ;
#16918 = VECTOR ( 'NONE', #62154, 1000.000000000000000 ) ;
#16919 = DIRECTION ( 'NONE',  ( -1.000000000000000000, 0.000000000000000000, 0.000000000000000000 ) ) ;
#16920 = VERTEX_POINT ( 'NONE', #44812 ) ;
#16921 = PLANE ( 'NONE',  #39937 ) ;
#16922 = PLANE ( 'NONE',  #48550 ) ;
#16923 = EDGE_LOOP ( 'NONE', ( #35781, #61833, #38844, #47672 ) ) ;
#16924 = CARTESIAN_POINT ( 'NONE',  ( -7.342976262117259623, 4.947141984184421304, 54.00000000000000711 ) ) ;
#16925 = CARTESIAN_POINT ( 'NONE',  ( 157.4206970127263787, -35.25383818724481699, 5.000000000000000000 ) ) ;
#16926 = DIRECTION ( 'NONE',  ( -1.000000000000000000, 0.000000000000000000, 0.000000000000000000 ) ) ;
#16927 = CARTESIAN_POINT ( 'NONE',  ( -4.188533722949335569, 4.727349090213398775, 455.0000000000000568 ) ) ;
#16928 = CARTESIAN_POINT ( 'NONE',  ( -9.897976262117257562, 3.667976262117184749, 54.00000000000000711 ) ) ;
#16929 = EDGE_CURVE ( 'NONE', #52471, #40712, #54662, .T. ) ;
#16930 = CARTESIAN_POINT ( 'NONE',  ( -7.450000000000001954, 0.000000000000000000, -17.00000000000000000 ) ) ;
#16931 = EDGE_LOOP ( 'NONE', ( #10839, #38297, #41422, #65642, #34575, #10043, #21661, #46452 ) ) ;
#16932 = CARTESIAN_POINT ( 'NONE',  ( 7.250000000000005329, 7.250000000000000888, -9.500000000000001776 ) ) ;
#16933 = AXIS2_PLACEMENT_3D ( 'NONE', #46171, #24960, #40866 ) ;
#16934 = FACE_OUTER_BOUND ( 'NONE', #33896, .T. ) ;
#16935 = ORIENTED_EDGE ( 'NONE', *, *, #69083, .T. ) ;
#16936 = EDGE_CURVE ( 'NONE', #52952, #1231, #12836, .T. ) ;
#16937 = CARTESIAN_POINT ( 'NONE',  ( -6.651770455163775964, -7.357023737882784964, 26.00000000000000000 ) ) ;
#16938 = ADVANCED_FACE ( 'NONE', ( #17941 ), #66032, .F. ) ;
#16939 = EDGE_CURVE ( 'NONE', #9220, #47996, #61068, .T. ) ;
#16940 = CARTESIAN_POINT ( 'NONE',  ( 290.0000000000000000, 0.000000000000000000, -27.00000000000000000 ) ) ;
#16941 = DIRECTION ( 'NONE',  ( -0.000000000000000000, -0.000000000000000000, -1.000000000000000000 ) ) ;
#16942 = ORIENTED_EDGE ( 'NONE', *, *, #50905, .F. ) ;
#16943 = ADVANCED_FACE ( 'NONE', ( #2383 ), #45156, .T. ) ;
#16944 = ORIENTED_EDGE ( 'NONE', *, *, #56914, .F. ) ;
#16945 = EDGE_CURVE ( 'NONE', #47930, #10503, #56473, .T. ) ;
#16946 = CARTESIAN_POINT ( 'NONE',  ( 49.00000000000000000, -0.2000000000089119934, -8.913009219568841313E-12 ) ) ;
#16947 = AXIS2_PLACEMENT_3D ( 'NONE', #69469, #68775, #3721 ) ;
#16948 = EDGE_LOOP ( 'NONE', ( #60126, #22786, #4468, #65748 ) ) ;
#16949 = AXIS2_PLACEMENT_3D ( 'NONE', #50839, #55809, #50507 ) ;
#16950 = VERTEX_POINT ( 'NONE', #23255 ) ;
#16951 = LINE ( 'NONE', #65731, #33789 ) ;
#16952 = CARTESIAN_POINT ( 'NONE',  ( 7.000000000000000000, -25.60000000000000142, 17.60000000000000142 ) ) ;
#16954 = PLANE ( 'NONE',  #17410 ) ;
#16953 = CIRCLE ( 'NONE', #43038, 0.5000000000079367624 ) ;
#16955 = ORIENTED_EDGE ( 'NONE', *, *, #23480, .T. ) ;
#16956 = CIRCLE ( 'NONE', #66605, 0.5000000000009441337 ) ;
#16957 = VECTOR ( 'NONE', #69266, 1000.000000000000000 ) ;
#16958 = CARTESIAN_POINT ( 'NONE',  ( 283.0000000000000568, -25.50000000000000355, 17.00000000000000000 ) ) ;
#16960 = CARTESIAN_POINT ( 'NONE',  ( -8.250000000000000000, 7.250000000000001776, -15.00000000000000000 ) ) ;
#16959 = CYLINDRICAL_SURFACE ( 'NONE', #49074, 1.224999999999999423 ) ;
#16961 = EDGE_LOOP ( 'NONE', ( #64947, #40514, #69053, #4565 ) ) ;
#16962 = ORIENTED_EDGE ( 'NONE', *, *, #15445, .F. ) ;
#16964 = ORIENTED_EDGE ( 'NONE', *, *, #9938, .F. ) ;
#16963 = CARTESIAN_POINT ( 'NONE',  ( -4.173516549646666185, 11.99351654964658920, 455.0000000000000568 ) ) ;
#16965 = ORIENTED_EDGE ( 'NONE', *, *, #52848, .T. ) ;
#16966 = AXIS2_PLACEMENT_3D ( 'NONE', #55787, #62842, #7333 ) ;
#16967 = CARTESIAN_POINT ( 'NONE',  ( 78.77321854994620765, 47.95351654967443977, 40.00000000000000000 ) ) ;
#16968 = AXIS2_PLACEMENT_3D ( 'NONE', #51714, #67971, #30141 ) ;
#16969 = CARTESIAN_POINT ( 'NONE',  ( 5.793274621760814647, 4.141586236041038482, 54.00000000000000711 ) ) ;
#16970 = ORIENTED_EDGE ( 'NONE', *, *, #40632, .F. ) ;
#16971 = ORIENTED_EDGE ( 'NONE', *, *, #29356, .F. ) ;
#16972 = AXIS2_PLACEMENT_3D ( 'NONE', #27052, #38698, #17132 ) ;
#16973 = CARTESIAN_POINT ( 'NONE',  ( -8.130476262117310782, -8.835729544836288696, 26.00000000000000000 ) ) ;
#16974 = CARTESIAN_POINT ( 'NONE',  ( 24.00000000000000000, -17.50000000000000000, -15.70500000000000007 ) ) ;
#16975 = ORIENTED_EDGE ( 'NONE', *, *, #67861, .T. ) ;
#16976 = FACE_OUTER_BOUND ( 'NONE', #13171, .T. ) ;
#16977 = LINE ( 'NONE', #56874, #44745 ) ;
#16978 = DIRECTION ( 'NONE',  ( 0.000000000000000000, 0.000000000000000000, -1.000000000000000000 ) ) ;
#16979 = ORIENTED_EDGE ( 'NONE', *, *, #36737, .F. ) ;
#16980 = EDGE_CURVE ( 'NONE', #54503, #37771, #24299, .T. ) ;
#16981 = DIRECTION ( 'NONE',  ( 1.000000000000000000, 0.000000000000000000, 0.000000000000000000 ) ) ;
#16982 = CARTESIAN_POINT ( 'NONE',  ( 3.848229544836322180, -7.532023737882811432, 54.00000000000000711 ) ) ;
#16985 = ORIENTED_EDGE ( 'NONE', *, *, #53970, .F. ) ;
#16984 = EDGE_CURVE ( 'NONE', #21951, #17134, #18635, .T. ) ;
#16983 = CARTESIAN_POINT ( 'NONE',  ( 69.92576880110368620, 10.00000000000000000, 281.4830310981151911 ) ) ;
#16987 = ORIENTED_EDGE ( 'NONE', *, *, #12445, .T. ) ;
#16986 = FACE_OUTER_BOUND ( 'NONE', #41758, .T. ) ;
#16988 = CARTESIAN_POINT ( 'NONE',  ( 29.50000000000000355, -11.50000000000000000, 11.00000000000000000 ) ) ;
#16989 = DIRECTION ( 'NONE',  ( -1.836970198721029934E-16, 1.836970198721036344E-16, -1.000000000000000000 ) ) ;
#16990 = CARTESIAN_POINT ( 'NONE',  ( -16.75000000000000000, -0.2038245569916330158, -23.22168783648699986 ) ) ;
#16991 = LINE ( 'NONE', #11664, #778 ) ;
#16992 = EDGE_CURVE ( 'NONE', #28094, #26202, #39174, .T. ) ;
#16993 = CARTESIAN_POINT ( 'NONE',  ( -7.250000000000000888, 8.250000000000001776, -26.00000000000001066 ) ) ;
#16994 = VECTOR ( 'NONE', #21605, 1000.000000000000000 ) ;
#16995 = CARTESIAN_POINT ( 'NONE',  ( -6.817976262117325881, -9.737023737882786634, 54.00000000000000711 ) ) ;
#16996 = ORIENTED_EDGE ( 'NONE', *, *, #57837, .T. ) ;
#16997 = CYLINDRICAL_SURFACE ( 'NONE', #46206, 1.000000000000000000 ) ;
#16998 = AXIS2_PLACEMENT_3D ( 'NONE', #60789, #6699, #12334 ) ;
#17000 = ORIENTED_EDGE ( 'NONE', *, *, #43585, .F. ) ;
#16999 = CARTESIAN_POINT ( 'NONE',  ( -9.880476262117236175, 7.447976262117216528, 54.00000000000000711 ) ) ;
#17002 = ORIENTED_EDGE ( 'NONE', *, *, #40431, .T. ) ;
#17001 = DIRECTION ( 'NONE',  ( 1.000000000000000000, 0.000000000000000000, 0.000000000000000000 ) ) ;
#17003 = VECTOR ( 'NONE', #3709, 1000.000000000000000 ) ;
#17004 = DIRECTION ( 'NONE',  ( 0.000000000000000000, 1.000000000000000000, 0.000000000000000000 ) ) ;
#17005 = ORIENTED_EDGE ( 'NONE', *, *, #67855, .F. ) ;
#17006 = DIRECTION ( 'NONE',  ( -1.000000000000000000, 2.602085213965213008E-15, 0.000000000000000000 ) ) ;
#17007 = LINE ( 'NONE', #6398, #29452 ) ;
#17008 = ORIENTED_EDGE ( 'NONE', *, *, #14793, .F. ) ;
#17009 = AXIS2_PLACEMENT_3D ( 'NONE', #4846, #4506, #31728 ) ;
#17010 = FACE_BOUND ( 'NONE', #2829, .T. ) ;
#17011 = DIRECTION ( 'NONE',  ( 0.000000000000000000, 0.000000000000000000, -1.000000000000000000 ) ) ;
#17012 = CARTESIAN_POINT ( 'NONE',  ( -16.89194109070750116, -5.000000000000000000, 26.25000000000000000 ) ) ;
#17013 = CARTESIAN_POINT ( 'NONE',  ( -7.593516549646711411, 11.77351654964660277, 195.0000000000000284 ) ) ;
#17014 = ADVANCED_FACE ( 'NONE', ( #18996 ), #1678, .T. ) ;
#17015 = FACE_OUTER_BOUND ( 'NONE', #37323, .T. ) ;
#17016 = ORIENTED_EDGE ( 'NONE', *, *, #39673, .F. ) ;
#17017 = DIRECTION ( 'NONE',  ( -0.7071067811865474617, 0.7071067811865474617, 0.000000000000000000 ) ) ;
#17018 = VERTEX_POINT ( 'NONE', #13339 ) ;
#17019 = ORIENTED_EDGE ( 'NONE', *, *, #17731, .T. ) ;
#17020 = DIRECTION ( 'NONE',  ( 0.000000000000000000, 0.000000000000000000, -1.000000000000000000 ) ) ;
#17021 = AXIS2_PLACEMENT_3D ( 'NONE', #55851, #44890, #18012 ) ;
#17022 = CARTESIAN_POINT ( 'NONE',  ( 283.0000000000000568, -20.50000000000000000, -17.00000000000000000 ) ) ;
#17023 = CARTESIAN_POINT ( 'NONE',  ( 8.250000000000005329, -8.249999999999998224, -26.00000000000001066 ) ) ;
#17024 = CARTESIAN_POINT ( 'NONE',  ( -7.250000000000000888, 7.450000000000003730, -10.50000000000000000 ) ) ;
#17025 = ORIENTED_EDGE ( 'NONE', *, *, #15852, .T. ) ;
#17026 = EDGE_CURVE ( 'NONE', #10751, #7480, #34548, .T. ) ;
#17027 = ORIENTED_EDGE ( 'NONE', *, *, #43630, .T. ) ;
#17028 = ADVANCED_FACE ( 'NONE', ( #40556 ), #62118, .F. ) ;
#17030 = ORIENTED_EDGE ( 'NONE', *, *, #35927, .F. ) ;
#17029 = CARTESIAN_POINT ( 'NONE',  ( 28.00000000000000000, -15.50000000000000000, -20.05051025721700242 ) ) ;
#17031 = ORIENTED_EDGE ( 'NONE', *, *, #27655, .T. ) ;
#17032 = LINE ( 'NONE', #66497, #5546 ) ;
#17033 = CARTESIAN_POINT ( 'NONE',  ( 39.90000000000000568, -21.00000000000001421, -13.86939075806900945 ) ) ;
#17034 = EDGE_CURVE ( 'NONE', #29317, #64891, #61782, .T. ) ;
#17035 = VECTOR ( 'NONE', #62079, 1000.000000000000000 ) ;
#17036 = DIRECTION ( 'NONE',  ( 0.000000000000000000, 0.000000000000000000, 1.000000000000000000 ) ) ;
#17037 = FACE_OUTER_BOUND ( 'NONE', #636, .T. ) ;
#17039 = DIRECTION ( 'NONE',  ( 0.000000000000000000, 0.000000000000000000, -1.000000000000000000 ) ) ;
#17038 = DIRECTION ( 'NONE',  ( -0.000000000000000000, -0.000000000000000000, 1.000000000000000000 ) ) ;
#17040 = ORIENTED_EDGE ( 'NONE', *, *, #65712, .F. ) ;
#17042 = ORIENTED_EDGE ( 'NONE', *, *, #39700, .F. ) ;
#17041 = CARTESIAN_POINT ( 'NONE',  ( -6.642976262117260333, 10.30047626211718104, 54.00000000000000711 ) ) ;
#17043 = ORIENTED_EDGE ( 'NONE', *, *, #5237, .F. ) ;
#17044 = VERTEX_POINT ( 'NONE', #13688 ) ;
#17045 = CARTESIAN_POINT ( 'NONE',  ( 24.00000000000000000, -17.50000000000000000, 19.33772233983200195 ) ) ;
#17046 = CARTESIAN_POINT ( 'NONE',  ( -11.77351654964674132, -4.186483450353323477, 455.0000000000000568 ) ) ;
#17047 = AXIS2_PLACEMENT_3D ( 'NONE', #50364, #29491, #61302 ) ;
#17048 = CARTESIAN_POINT ( 'NONE',  ( 15.50000000000000000, -2.500000000000000000, 23.94337567297399971 ) ) ;
#17049 = CARTESIAN_POINT ( 'NONE',  ( 10.05377373788281581, 8.916576262117182239, 54.00000000000000711 ) ) ;
#17050 = VERTEX_POINT ( 'NONE', #51168 ) ;
#17051 = VERTEX_POINT ( 'NONE', #2726 ) ;
#17052 = VECTOR ( 'NONE', #64752, 1000.000000000000000 ) ;
#17053 = DIRECTION ( 'NONE',  ( -0.000000000000000000, -1.000000000000000000, 0.000000000000000000 ) ) ;
#17054 = DIRECTION ( 'NONE',  ( -0.000000000000000000, -0.000000000000000000, -1.000000000000000000 ) ) ;
#17055 = VERTEX_POINT ( 'NONE', #30658 ) ;
#17056 = VECTOR ( 'NONE', #1523, 1000.000000000000000 ) ;
#17057 = VECTOR ( 'NONE', #26428, 1000.000000000000000 ) ;
#17058 = ORIENTED_EDGE ( 'NONE', *, *, #2611, .T. ) ;
#17059 = CARTESIAN_POINT ( 'NONE',  ( 32.89999999999999858, -0.1999999999911430404, -8.864436962241481021E-12 ) ) ;
#17060 = DIRECTION ( 'NONE',  ( -0.000000000000000000, -0.000000000000000000, -1.000000000000000000 ) ) ;
#17061 = ORIENTED_EDGE ( 'NONE', *, *, #36832, .F. ) ;
#17062 = VECTOR ( 'NONE', #46491, 1000.000000000000000 ) ;
#17063 = DIRECTION ( 'NONE',  ( -4.336808689942043768E-15, -1.000000000000000000, 0.000000000000000000 ) ) ;
#17066 = ORIENTED_EDGE ( 'NONE', *, *, #61297, .F. ) ;
#17065 = EDGE_CURVE ( 'NONE', #59731, #9744, #15101, .T. ) ;
#17064 = CARTESIAN_POINT ( 'NONE',  ( 7.250000000000004441, 7.450000000000001954, -22.00000000000000000 ) ) ;
#17067 = EDGE_LOOP ( 'NONE', ( #65601, #16794, #50583, #27116 ) ) ;
#17068 = EDGE_CURVE ( 'NONE', #10448, #39282, #63545, .T. ) ;
#17069 = ADVANCED_FACE ( 'NONE', ( #57524 ), #3784, .T. ) ;
#17070 = DIRECTION ( 'NONE',  ( -1.836970198721029934E-16, 1.836970198721036590E-16, -1.000000000000000000 ) ) ;
#17071 = LINE ( 'NONE', #11748, #31204 ) ;
#17072 = DIRECTION ( 'NONE',  ( 1.000000000000000000, 0.000000000000000000, 0.000000000000000000 ) ) ;
#17073 = PLANE ( 'NONE',  #16564 ) ;
#17074 = EDGE_CURVE ( 'NONE', #31922, #29982, #46209, .T. ) ;
#17075 = DIRECTION ( 'NONE',  ( 0.000000000000000000, 1.000000000000000000, 0.000000000000000000 ) ) ;
#17076 = ORIENTED_EDGE ( 'NONE', *, *, #66513, .F. ) ;
#17077 = DIRECTION ( 'NONE',  ( 0.7671651518153029814, 0.6414496315691537998, 0.000000000000000000 ) ) ;
#17078 = ORIENTED_EDGE ( 'NONE', *, *, #39085, .F. ) ;
#17079 = DIRECTION ( 'NONE',  ( 0.000000000000000000, 0.000000000000000000, -1.000000000000000000 ) ) ;
#17080 = CARTESIAN_POINT ( 'NONE',  ( -7.593516549646831315, -11.32648345035340931, 455.0000000000000568 ) ) ;
#17081 = VECTOR ( 'NONE', #40521, 1000.000000000000000 ) ;
#17082 = CARTESIAN_POINT ( 'NONE',  ( -11.00000000000000000, -17.00000000000000000, -15.70499999999969809 ) ) ;
#17083 = CARTESIAN_POINT ( 'NONE',  ( 19.90000000000000213, 0.000000000000000000, 1.292961597001347137E-15 ) ) ;
#17084 = LINE ( 'NONE', #31970, #60808 ) ;
#17085 = ORIENTED_EDGE ( 'NONE', *, *, #62125, .F. ) ;
#17086 = ORIENTED_EDGE ( 'NONE', *, *, #36112, .T. ) ;
#17087 = CARTESIAN_POINT ( 'NONE',  ( 29.50000000000000355, -11.50000000000000000, 15.00000000000000000 ) ) ;
#17088 = VECTOR ( 'NONE', #66541, 1000.000000000000000 ) ;
#17089 = FACE_OUTER_BOUND ( 'NONE', #46155, .T. ) ;
#17090 =( GEOMETRIC_REPRESENTATION_CONTEXT ( 3 ) GLOBAL_UNCERTAINTY_ASSIGNED_CONTEXT ( ( #22455 ) ) GLOBAL_UNIT_ASSIGNED_CONTEXT ( ( #1482, #7127, #18085 ) ) REPRESENTATION_CONTEXT ( 'NONE', 'WORKASPACE' ) );
#17091 = VERTEX_POINT ( 'NONE', #25357 ) ;
#17092 = DIRECTION ( 'NONE',  ( -1.836970198721029934E-16, 1.836970198721036344E-16, -1.000000000000000000 ) ) ;
#17093 = DIRECTION ( 'NONE',  ( -1.000000000000000000, 0.000000000000000000, 0.000000000000000000 ) ) ;
#17094 = ORIENTED_EDGE ( 'NONE', *, *, #53600, .T. ) ;
#17095 = CARTESIAN_POINT ( 'NONE',  ( -7.450000000000001954, 0.000000000000000000, -10.50000000000000000 ) ) ;
#17096 = DIRECTION ( 'NONE',  ( 1.000000000000000000, 0.000000000000000000, 0.000000000000000000 ) ) ;
#17097 = ORIENTED_EDGE ( 'NONE', *, *, #39820, .T. ) ;
#17098 = DIRECTION ( 'NONE',  ( 1.000000000000000000, 0.000000000000000000, 0.000000000000000000 ) ) ;
#17099 = DIRECTION ( 'NONE',  ( 1.000000000000000000, 0.000000000000000000, 0.000000000000000000 ) ) ;
#17100 = AXIS2_PLACEMENT_3D ( 'NONE', #15987, #5732, #33287 ) ;
#17101 = DIRECTION ( 'NONE',  ( 0.000000000000000000, 0.000000000000000000, -1.000000000000000000 ) ) ;
#17102 = CARTESIAN_POINT ( 'NONE',  ( -7.450000000000001954, 0.000000000000000000, -23.50000000000000000 ) ) ;
#17103 = ORIENTED_EDGE ( 'NONE', *, *, #64960, .F. ) ;
#17105 = VERTEX_POINT ( 'NONE', #52947 ) ;
#17104 = DIRECTION ( 'NONE',  ( -0.7671651518153006499, 0.6414496315691565753, -0.000000000000000000 ) ) ;
#17106 = VECTOR ( 'NONE', #7090, 1000.000000000000000 ) ;
#17107 = ADVANCED_FACE ( 'NONE', ( #10143, #26069 ), #14404, .T. ) ;
#17108 = FACE_OUTER_BOUND ( 'NONE', #54032, .T. ) ;
#17109 = EDGE_CURVE ( 'NONE', #38679, #10292, #21954, .T. ) ;
#17110 = DIRECTION ( 'NONE',  ( 0.000000000000000000, -0.7071067811865475727, 0.7071067811865475727 ) ) ;
#17111 = DIRECTION ( 'NONE',  ( 1.115702204244423151E-14, 1.000000000000000000, 1.836970198721016129E-16 ) ) ;
#17112 = ORIENTED_EDGE ( 'NONE', *, *, #65745, .F. ) ;
#17113 = ADVANCED_FACE ( 'NONE', ( #58231 ), #62834, .T. ) ;
#17114 = VECTOR ( 'NONE', #18449, 1000.000000000000000 ) ;
#17115 = CARTESIAN_POINT ( 'NONE',  ( -11.00000000000000000, -5.599999999999999645, -27.00000000000000000 ) ) ;
#17116 = DIRECTION ( 'NONE',  ( -0.000000000000000000, 3.673940397442059868E-16, -1.000000000000000000 ) ) ;
#17117 = EDGE_CURVE ( 'NONE', #51101, #21439, #35960, .T. ) ;
#17118 = ORIENTED_EDGE ( 'NONE', *, *, #4600, .F. ) ;
#17119 = VERTEX_POINT ( 'NONE', #68845 ) ;
#17120 = PRODUCT_DEFINITION ( 'UNKNOWN', '', #35823, #40234 ) ;
#17121 = EDGE_LOOP ( 'NONE', ( #13597, #39695, #34, #15168 ) ) ;
#17122 = FACE_OUTER_BOUND ( 'NONE', #15242, .T. ) ;
#17123 = EDGE_CURVE ( 'NONE', #44788, #14276, #20745, .T. ) ;
#17124 = LINE ( 'NONE', #49643, #3832 ) ;
#17125 = EDGE_CURVE ( 'NONE', #26101, #1993, #13717, .T. ) ;
#17126 = DIRECTION ( 'NONE',  ( -1.000000000000000000, 0.000000000000000000, 0.000000000000000000 ) ) ;
#17127 =( NAMED_UNIT ( * ) PLANE_ANGLE_UNIT ( ) SI_UNIT ( $, .RADIAN. ) );
#17128 = VECTOR ( 'NONE', #11481, 1000.000000000000000 ) ;
#17129 = ORIENTED_EDGE ( 'NONE', *, *, #57412, .F. ) ;
#17130 = ORIENTED_EDGE ( 'NONE', *, *, #15528, .T. ) ;
#17131 = VERTEX_POINT ( 'NONE', #40905 ) ;
#17132 = DIRECTION ( 'NONE',  ( -1.000000000000000000, 0.000000000000000000, 0.000000000000000000 ) ) ;
#17133 = VERTEX_POINT ( 'NONE', #9090 ) ;
#17134 = VERTEX_POINT ( 'NONE', #46907 ) ;
#17135 = ORIENTED_EDGE ( 'NONE', *, *, #65360, .F. ) ;
#17136 = ORIENTED_EDGE ( 'NONE', *, *, #42730, .T. ) ;
#17137 = DIRECTION ( 'NONE',  ( 0.000000000000000000, 1.000000000000000000, 0.000000000000000000 ) ) ;
#17138 = VECTOR ( 'NONE', #15616, 1000.000000000000000 ) ;
#17140 = VERTEX_POINT ( 'NONE', #31722 ) ;
#17139 = LINE ( 'NONE', #42970, #23198 ) ;
#17141 = DIRECTION ( 'NONE',  ( -1.000000000000000000, 1.047444401652940007E-14, -1.836970198721010706E-16 ) ) ;
#17142 = PRODUCT_DEFINITION_SHAPE ( 'NONE', 'NONE',  #69994 ) ;
#17143 = CARTESIAN_POINT ( 'NONE',  ( 9.106483450353380249, -10.09643294401465852, 455.0000000000000568 ) ) ;
#17144 = LINE ( 'NONE', #204, #5370 ) ;
#17145 = VERTEX_POINT ( 'NONE', #41615 ) ;
#17146 = CARTESIAN_POINT ( 'NONE',  ( 0.000000000000000000, 0.000000000000000000, -20.00000000000000000 ) ) ;
#17147 = AXIS2_PLACEMENT_3D ( 'NONE', #47637, #21121, #64260 ) ;
#17148 = CLOSED_SHELL ( 'NONE', ( #60638, #53205, #51983, #51181, #24773, #19438, #7199, #5948, #13627, #54003, #65363, #46058 ) ) ;
#17149 = LINE ( 'NONE', #11486, #68448 ) ;
#17150 = CARTESIAN_POINT ( 'NONE',  ( 290.0000000000000000, -21.00000000000000000, -5.000000000000000000 ) ) ;
#17151 = ORIENTED_EDGE ( 'NONE', *, *, #42005, .F. ) ;
#17152 = DIRECTION ( 'NONE',  ( 0.000000000000000000, -1.000000000000000000, 0.000000000000000000 ) ) ;
#17153 = DIRECTION ( 'NONE',  ( -1.000000000000000000, 0.000000000000000000, 0.000000000000000000 ) ) ;
#17154 = LINE ( 'NONE', #22479, #67309 ) ;
#17155 = ORIENTED_EDGE ( 'NONE', *, *, #45062, .T. ) ;
#17156 = LINE ( 'NONE', #6888, #16672 ) ;
#17157 = AXIS2_PLACEMENT_3D ( 'NONE', #43869, #27960, #38572 ) ;
#17158 = EDGE_CURVE ( 'NONE', #25138, #18463, #58590, .T. ) ;
#17159 = CARTESIAN_POINT ( 'NONE',  ( 46.39999999999999858, 33.00000000000000000, 0.7500000000000000000 ) ) ;
#17160 = DIRECTION ( 'NONE',  ( 0.000000000000000000, 0.000000000000000000, 1.000000000000000000 ) ) ;
#17161 = EDGE_CURVE ( 'NONE', #14602, #24174, #6155, .T. ) ;
#17162 = PLANE ( 'NONE',  #25252 ) ;
#17163 = DIRECTION ( 'NONE',  ( 1.000000000000000000, 0.000000000000000000, 0.000000000000000000 ) ) ;
#17164 = DIRECTION ( 'NONE',  ( 0.000000000000000000, -1.000000000000000000, 0.000000000000000000 ) ) ;
#17165 = CARTESIAN_POINT ( 'NONE',  ( 3.664523737882820598, 10.49297626211720491, 54.00000000000000711 ) ) ;
#17166 = CARTESIAN_POINT ( 'NONE',  ( -8.250000000000001776, -8.249999999999998224, -26.00000000000001066 ) ) ;
#17167 = ORIENTED_EDGE ( 'NONE', *, *, #67397, .T. ) ;
#17168 = CARTESIAN_POINT ( 'NONE',  ( -30.00000000000000000, -11.50000000000100009, -19.50000000000103739 ) ) ;
#17169 = EDGE_CURVE ( 'NONE', #38450, #59333, #31008, .T. ) ;
#17170 = CARTESIAN_POINT ( 'NONE',  ( -10.30047626211725742, 6.642976262117184838, 26.00000000000000711 ) ) ;
#17171 = CARTESIAN_POINT ( 'NONE',  ( -11.00000000000000000, -12.00000000000000000, -11.03137303340310282 ) ) ;
#17172 = CARTESIAN_POINT ( 'NONE',  ( 25.50000000000000355, 0.000000000000000000, 24.12099999999999866 ) ) ;
#17173 = ORIENTED_EDGE ( 'NONE', *, *, #52298, .T. ) ;
#17174 = DIRECTION ( 'NONE',  ( 0.8660254037844435926, 0.4999999999999913958, 2.509347957447859069E-16 ) ) ;
#17175 = CARTESIAN_POINT ( 'NONE',  ( -10.91351654964666373, -2.706483450353290632, 195.0000000000000284 ) ) ;
#17176 = CIRCLE ( 'NONE', #68012, 5.000000000000000000 ) ;
#17177 = EDGE_CURVE ( 'NONE', #39723, #29071, #64867, .T. ) ;
#17178 = LINE ( 'NONE', #39433, #49207 ) ;
#17179 = CARTESIAN_POINT ( 'NONE',  ( 176.4833316329832940, 9.000000000000001776, 326.8892501111512843 ) ) ;
#17180 = LINE ( 'NONE', #948, #12492 ) ;
#17181 = VECTOR ( 'NONE', #18348, 1000.000000000000000 ) ;
#17182 = ORIENTED_EDGE ( 'NONE', *, *, #40628, .T. ) ;
#17183 = ORIENTED_EDGE ( 'NONE', *, *, #11300, .F. ) ;
#17184 = DIRECTION ( 'NONE',  ( 0.000000000000000000, 1.000000000000000000, 0.000000000000000000 ) ) ;
#17185 = EDGE_CURVE ( 'NONE', #9319, #1040, #4842, .T. ) ;
#17186 = DIRECTION ( 'NONE',  ( 0.000000000000000000, 0.000000000000000000, 1.000000000000000000 ) ) ;
#17187 = VERTEX_POINT ( 'NONE', #33446 ) ;
#17188 = AXIS2_PLACEMENT_3D ( 'NONE', #23723, #66850, #29370 ) ;
#17189 = PLANE ( 'NONE',  #20531 ) ;
#17190 = ORIENTED_EDGE ( 'NONE', *, *, #66183, .T. ) ;
#17191 = VECTOR ( 'NONE', #9378, 1000.000000000000000 ) ;
#17192 = CARTESIAN_POINT ( 'NONE',  ( 30.00000000000000000, -16.28999999999999915, -14.50000000000000000 ) ) ;
#17193 = ORIENTED_EDGE ( 'NONE', *, *, #60108, .F. ) ;
#17194 = ORIENTED_EDGE ( 'NONE', *, *, #38807, .T. ) ;
#17196 = EDGE_CURVE ( 'NONE', #21626, #22860, #27099, .T. ) ;
#17195 = CARTESIAN_POINT ( 'NONE',  ( -11.29351654964668583, 8.513516549646642062, 455.0000000000000568 ) ) ;
#17197 = ORIENTED_EDGE ( 'NONE', *, *, #25331, .F. ) ;
#17198 = CARTESIAN_POINT ( 'NONE',  ( 11.90000000000000036, -0.1999999999911430404, -8.864436962241481021E-12 ) ) ;
#17199 = ADVANCED_FACE ( 'NONE', ( #55032 ), #53985, .F. ) ;
#17200 = LINE ( 'NONE', #38438, #44033 ) ;
#17201 = CARTESIAN_POINT ( 'NONE',  ( 2.290483450353350658, -9.841277389592804070, 455.0000000000000568 ) ) ;
#17202 = VECTOR ( 'NONE', #57535, 1000.000000000000000 ) ;
#17203 = ORIENTED_EDGE ( 'NONE', *, *, #30536, .T. ) ;
#17204 = EDGE_LOOP ( 'NONE', ( #29439, #39522, #29152, #43388 ) ) ;
#17205 = DIRECTION ( 'NONE',  ( 0.000000000000000000, 1.000000000000000000, 0.000000000000000000 ) ) ;
#17206 = VECTOR ( 'NONE', #64656, 1000.000000000000000 ) ;
#17207 = DIRECTION ( 'NONE',  ( 1.000000000000000000, -0.000000000000000000, 0.000000000000000000 ) ) ;
#17208 = ORIENTED_EDGE ( 'NONE', *, *, #59192, .F. ) ;
#17209 = ADVANCED_FACE ( 'NONE', ( #49021 ), #65293, .F. ) ;
#17210 = ORIENTED_EDGE ( 'NONE', *, *, #51159, .F. ) ;
#17211 = EDGE_LOOP ( 'NONE', ( #67264, #65171, #46583, #40182 ) ) ;
#17212 = FACE_OUTER_BOUND ( 'NONE', #33667, .T. ) ;
#17214 = VERTEX_POINT ( 'NONE', #48671 ) ;
#17213 = LINE ( 'NONE', #16535, #57918 ) ;
#17215 = LINE ( 'NONE', #22538, #14182 ) ;
#17216 = CARTESIAN_POINT ( 'NONE',  ( 7.450000000000006395, 7.250000000000000888, -14.50000000000000000 ) ) ;
#17217 = ORIENTED_EDGE ( 'NONE', *, *, #53069, .T. ) ;
#17218 = ORIENTED_EDGE ( 'NONE', *, *, #48686, .T. ) ;
#17219 = AXIS2_PLACEMENT_3D ( 'NONE', #46133, #50040, #67700 ) ;
#17220 = ADVANCED_FACE ( 'NONE', ( #59629 ), #54328, .F. ) ;
#17221 = PLANE ( 'NONE',  #41523 ) ;
#17222 = FACE_OUTER_BOUND ( 'NONE', #26685, .T. ) ;
#17223 = AXIS2_PLACEMENT_3D ( 'NONE', #60285, #56379, #13595 ) ;
#17224 = EDGE_CURVE ( 'NONE', #62302, #49054, #32416, .T. ) ;
#17225 = DIRECTION ( 'NONE',  ( -1.836970198721029934E-16, 1.836970198721036344E-16, -1.000000000000000000 ) ) ;
#17226 = CYLINDRICAL_SURFACE ( 'NONE', #48296, 24.99999999998784972 ) ;
#17228 = VERTEX_POINT ( 'NONE', #16493 ) ;
#17227 = DIRECTION ( 'NONE',  ( 0.000000000000000000, -1.000000000000000000, 0.000000000000000000 ) ) ;
#17229 = ORIENTED_EDGE ( 'NONE', *, *, #5137, .T. ) ;
#17230 = EDGE_CURVE ( 'NONE', #40228, #28168, #43395, .T. ) ;
#17231 = CIRCLE ( 'NONE', #9377, 1.399999999999998579 ) ;
#17232 = FACE_OUTER_BOUND ( 'NONE', #31836, .T. ) ;
#17233 = DIRECTION ( 'NONE',  ( -1.000000000000000000, 0.000000000000000000, 0.000000000000000000 ) ) ;
#17234 = EDGE_CURVE ( 'NONE', #44081, #992, #38077, .T. ) ;
#17235 = CARTESIAN_POINT ( 'NONE',  ( -3.667976262117228714, 9.722976262117169810, 26.00000000000000711 ) ) ;
#17236 = DIRECTION ( 'NONE',  ( 0.000000000000000000, 0.7046037717862339012, -0.7096009616570518874 ) ) ;
#17237 = EDGE_CURVE ( 'NONE', #4729, #55345, #12883, .T. ) ;
#17238 = DIRECTION ( 'NONE',  ( 1.000000000000000000, 0.000000000000000000, -0.000000000000000000 ) ) ;
#17239 = ORIENTED_EDGE ( 'NONE', *, *, #4549, .F. ) ;
#17240 = DIRECTION ( 'NONE',  ( 1.280238727658158432E-15, 1.000000000000000000, -0.000000000000000000 ) ) ;
#17241 = CARTESIAN_POINT ( 'NONE',  ( 15.00000000000000000, -21.00000000000000000, 0.000000000000000000 ) ) ;
#17242 = CARTESIAN_POINT ( 'NONE',  ( 25.50000000000000355, 0.000000000000000000, 22.50000000000000000 ) ) ;
#17243 = DIRECTION ( 'NONE',  ( 0.000000000000000000, 1.000000000000000000, 0.000000000000000000 ) ) ;
#17244 = FACE_OUTER_BOUND ( 'NONE', #39970, .T. ) ;
#17245 = VECTOR ( 'NONE', #14339, 1000.000000000000000 ) ;
#17246 = LINE ( 'NONE', #38487, #7704 ) ;
#17247 = EDGE_CURVE ( 'NONE', #39291, #33489, #36632, .T. ) ;
#17248 = LINE ( 'NONE', #28212, #45410 ) ;
#17249 = ADVANCED_FACE ( 'NONE', ( #5192 ), #38408, .T. ) ;
#17250 = VECTOR ( 'NONE', #69877, 1000.000000000000000 ) ;
#17251 = CYLINDRICAL_SURFACE ( 'NONE', #39724, 0.5250000000000011324 ) ;
#17252 = VERTEX_POINT ( 'NONE', #11173 ) ;
#17253 = CYLINDRICAL_SURFACE ( 'NONE', #50152, 4.000000000000000000 ) ;
#17254 = CARTESIAN_POINT ( 'NONE',  ( -14.10805890929250239, -5.000000000000000000, -26.25000000000000000 ) ) ;
#17255 = ADVANCED_FACE ( 'NONE', ( #64246 ), #5537, .F. ) ;
#17256 = ORIENTED_EDGE ( 'NONE', *, *, #33725, .T. ) ;
#17257 = FACE_OUTER_BOUND ( 'NONE', #30713, .T. ) ;
#17258 = EDGE_CURVE ( 'NONE', #26986, #39386, #32747, .T. ) ;
#17259 = EDGE_CURVE ( 'NONE', #523, #69426, #48325, .T. ) ;
#17260 = CARTESIAN_POINT ( 'NONE',  ( 49.00000000000000000, -14.06939075806900163, -20.80000000000000426 ) ) ;
#17261 = DIRECTION ( 'NONE',  ( -1.000000000000000000, 0.000000000000000000, 0.000000000000000000 ) ) ;
#17263 = AXIS2_PLACEMENT_3D ( 'NONE', #22218, #43780, #59345 ) ;
#17262 = LINE ( 'NONE', #1355, #30847 ) ;
#17264 = LINE ( 'NONE', #5972, #31664 ) ;
#17265 = EDGE_CURVE ( 'NONE', #17842, #60006, #16140, .T. ) ;
#17266 = DIRECTION ( 'NONE',  ( -0.000000000000000000, -0.000000000000000000, 1.000000000000000000 ) ) ;
#17267 = AXIS2_PLACEMENT_3D ( 'NONE', #10980, #54466, #726 ) ;
#17268 = ORIENTED_EDGE ( 'NONE', *, *, #23613, .F. ) ;
#17269 = DIRECTION ( 'NONE',  ( 0.7671651518153006499, -0.6414496315691565753, 0.000000000000000000 ) ) ;
#17270 = ORIENTED_EDGE ( 'NONE', *, *, #13085, .F. ) ;
#17271 = CARTESIAN_POINT ( 'NONE',  ( 6.665817930929297752, -7.532023737882823866, 54.00000000000000711 ) ) ;
#17272 = VECTOR ( 'NONE', #14322, 999.9999999999998863 ) ;
#17273 = DIRECTION ( 'NONE',  ( 0.000000000000000000, 1.000000000000000000, 0.000000000000000000 ) ) ;
#17274 = DIRECTION ( 'NONE',  ( 1.000000000000000000, -0.000000000000000000, 0.000000000000000000 ) ) ;
#17275 = ORIENTED_EDGE ( 'NONE', *, *, #46390, .T. ) ;
#17276 = ORIENTED_EDGE ( 'NONE', *, *, #4065, .T. ) ;
#17277 = VECTOR ( 'NONE', #12077, 1000.000000000000000 ) ;
#17279 = EDGE_CURVE ( 'NONE', #39563, #56637, #58931, .T. ) ;
#17278 = DIRECTION ( 'NONE',  ( 1.000000000000000000, -0.000000000000000000, -0.000000000000000000 ) ) ;
#17280 = EDGE_LOOP ( 'NONE', ( #69325, #51977, #53422, #46500, #14417, #1929, #46436, #14273, #19761, #45888, #44085, #16668, #63769, #40161, #54535, #50511 ) ) ;
#17281 = ORIENTED_EDGE ( 'NONE', *, *, #26621, .T. ) ;
#17282 = EDGE_CURVE ( 'NONE', #33288, #44820, #69881, .T. ) ;
#17283 = DIRECTION ( 'NONE',  ( 0.000000000000000000, 1.000000000000000000, 0.000000000000000000 ) ) ;
#17284 = CARTESIAN_POINT ( 'NONE',  ( 8.750000000000005329, 7.250000000000000888, -30.00000000000001066 ) ) ;
#17285 = PLANE ( 'NONE',  #44504 ) ;
#17286 = ORIENTED_EDGE ( 'NONE', *, *, #6514, .T. ) ;
#17287 = CARTESIAN_POINT ( 'NONE',  ( 28.00000000000000000, -16.28999999999710369, 15.00000000000794920 ) ) ;
#17289 = DIRECTION ( 'NONE',  ( -1.000000000000000000, -0.000000000000000000, -0.000000000000000000 ) ) ;
#17288 = PLANE ( 'NONE',  #1658 ) ;
#17290 = ORIENTED_EDGE ( 'NONE', *, *, #30941, .T. ) ;
#17292 = ORIENTED_EDGE ( 'NONE', *, *, #61110, .F. ) ;
#17291 = DIRECTION ( 'NONE',  ( 1.000000000000000000, 0.000000000000000000, 0.000000000000000000 ) ) ;
#17293 = ORIENTED_EDGE ( 'NONE', *, *, #18680, .T. ) ;
#17294 = DIRECTION ( 'NONE',  ( -5.981805089575196197E-17, -1.000000000000000000, 0.000000000000000000 ) ) ;
#17295 = DIRECTION ( 'NONE',  ( 0.8660254037844322683, -0.5000000000000111022, 6.723777587268230953E-17 ) ) ;
#17296 = VECTOR ( 'NONE', #35096, 1000.000000000000000 ) ;
#17297 = VERTEX_POINT ( 'NONE', #37715 ) ;
#17298 = VERTEX_POINT ( 'NONE', #59275 ) ;
#17299 = CIRCLE ( 'NONE', #362, 25.39999999999999858 ) ;
#17301 = CARTESIAN_POINT ( 'NONE',  ( 0.000000000000000000, -8.749999999999998224, -30.00000000000001066 ) ) ;
#17300 = AXIS2_PLACEMENT_3D ( 'NONE', #54334, #44382, #17876 ) ;
#17302 = VECTOR ( 'NONE', #15313, 1000.000000000000000 ) ;
#17303 = CARTESIAN_POINT ( 'NONE',  ( 8.250000000000005329, 7.250000000000000888, -26.00000000000001066 ) ) ;
#17304 = EDGE_LOOP ( 'NONE', ( #23643, #45948, #25243, #12907 ) ) ;
#17305 = LINE ( 'NONE', #60437, #7109 ) ;
#17306 = DIRECTION ( 'NONE',  ( 0.000000000000000000, 0.000000000000000000, -1.000000000000000000 ) ) ;
#17307 = AXIS2_PLACEMENT_3D ( 'NONE', #28195, #45132, #11914 ) ;
#17308 = AXIS2_PLACEMENT_3D ( 'NONE', #21782, #59617, #11161 ) ;
#17309 = CARTESIAN_POINT ( 'NONE',  ( 4.456444791733522252E-16, 7.450000000000002842, -13.50000000000000178 ) ) ;
#17310 = VERTEX_POINT ( 'NONE', #49704 ) ;
#17311 = EDGE_CURVE ( 'NONE', #29254, #60848, #13611, .T. ) ;
#17312 = CARTESIAN_POINT ( 'NONE',  ( -11.18999999999999950, 11.18999999999999950, -5.000000000000000000 ) ) ;
#17313 = FACE_OUTER_BOUND ( 'NONE', #17533, .T. ) ;
#17315 = ORIENTED_EDGE ( 'NONE', *, *, #22534, .F. ) ;
#17314 = CARTESIAN_POINT ( 'NONE',  ( 10.50702373788280219, 6.835476262117187396, 26.00000000000000711 ) ) ;
#17317 = VERTEX_POINT ( 'NONE', #12208 ) ;
#17316 = DIRECTION ( 'NONE',  ( 0.000000000000000000, -0.8188976377952759123, 0.5739395950910837207 ) ) ;
#17318 = EDGE_CURVE ( 'NONE', #43516, #52725, #60993, .T. ) ;
#17319 = DIRECTION ( 'NONE',  ( 0.000000000000000000, -1.000000000000000000, 0.000000000000000000 ) ) ;
#17320 = CARTESIAN_POINT ( 'NONE',  ( -23.48000000000000043, -17.50000000000000000, -26.00000000000000355 ) ) ;
#17321 = EDGE_CURVE ( 'NONE', #55345, #50247, #45785, .T. ) ;
#17322 = CIRCLE ( 'NONE', #6037, 0.8099999999999999423 ) ;
#17323 = DIRECTION ( 'NONE',  ( 0.000000000000000000, -0.9938079899998859545, 0.1111111111112941946 ) ) ;
#17324 = LINE ( 'NONE', #42817, #15454 ) ;
#17325 = CARTESIAN_POINT ( 'NONE',  ( 283.0000000000000568, -23.65000000000000568, -12.40000000000000213 ) ) ;
#17326 = ADVANCED_FACE ( 'NONE', ( #28814 ), #61336, .F. ) ;
#17327 = CARTESIAN_POINT ( 'NONE',  ( 12.00648345035337883, -11.19368345035338308, 195.0000000000000284 ) ) ;
#17328 = VERTEX_POINT ( 'NONE', #23871 ) ;
#17329 = CARTESIAN_POINT ( 'NONE',  ( 9.841277389592693936, 1.677516549646539623, 455.0000000000000568 ) ) ;
#17331 = VERTEX_POINT ( 'NONE', #34460 ) ;
#17330 = CARTESIAN_POINT ( 'NONE',  ( -9.791916549646712653, 11.07551654964660415, 195.0000000000000284 ) ) ;
#17333 = ORIENTED_EDGE ( 'NONE', *, *, #2864, .F. ) ;
#17332 = LINE ( 'NONE', #28632, #58138 ) ;
#17334 = PRESENTATION_STYLE_ASSIGNMENT (( #26929 ) ) ;
#17335 = CARTESIAN_POINT ( 'NONE',  ( 7.000000000000000000, -28.94999999999999929, 13.50000000000000000 ) ) ;
#17336 = VERTEX_POINT ( 'NONE', #18924 ) ;
#17337 = DIRECTION ( 'NONE',  ( -1.000000000000000000, 0.000000000000000000, 0.000000000000000000 ) ) ;
#17338 = CARTESIAN_POINT ( 'NONE',  ( 15.00000000000000000, -20.40000000000000213, -17.60000000000000142 ) ) ;
#17339 = ORIENTED_EDGE ( 'NONE', *, *, #31834, .F. ) ;
#17340 = EDGE_CURVE ( 'NONE', #39153, #59373, #39098, .T. ) ;
#17341 = CARTESIAN_POINT ( 'NONE',  ( -11.18071654964669648, 11.18071654964658812, 195.0000000000000284 ) ) ;
#17342 = DIRECTION ( 'NONE',  ( 1.000000000000000000, -0.000000000000000000, -0.000000000000000000 ) ) ;
#17343 = DIRECTION ( 'NONE',  ( 1.000000000000000000, 0.000000000000000000, 0.000000000000000000 ) ) ;
#17344 = CARTESIAN_POINT ( 'NONE',  ( -8.250000000000001776, -8.249999999999998224, -26.00000000000001066 ) ) ;
#17345 = CARTESIAN_POINT ( 'NONE',  ( 11.08848345035334404, -10.20488345035343336, 195.0000000000000284 ) ) ;
#17346 = AXIS2_PLACEMENT_3D ( 'NONE', #9266, #58422, #9977 ) ;
#17347 = ORIENTED_EDGE ( 'NONE', *, *, #2078, .T. ) ;
#17348 = LINE ( 'NONE', #60483, #4411 ) ;
#17349 = ORIENTED_EDGE ( 'NONE', *, *, #58388, .T. ) ;
#17350 = ORIENTED_EDGE ( 'NONE', *, *, #16602, .F. ) ;
#17351 = DIRECTION ( 'NONE',  ( -0.000000000000000000, -0.000000000000000000, 1.000000000000000000 ) ) ;
#17352 = CARTESIAN_POINT ( 'NONE',  ( 8.930623737882839919, 8.566576262117191476, 26.00000000000000711 ) ) ;
#17353 = CIRCLE ( 'NONE', #10551, 7.800000000000000711 ) ;
#17354 = CIRCLE ( 'NONE', #11750, 0.5249999999999994671 ) ;
#17355 = VECTOR ( 'NONE', #63963, 999.9999999999998863 ) ;
#17356 = LINE ( 'NONE', #38930, #5007 ) ;
#17357 = AXIS2_PLACEMENT_3D ( 'NONE', #26257, #36506, #3640 ) ;
#17358 = VECTOR ( 'NONE', #25500, 1000.000000000000000 ) ;
#17359 = FACE_OUTER_BOUND ( 'NONE', #54612, .T. ) ;
#17360 = EDGE_LOOP ( 'NONE', ( #14713, #64245, #4395, #16975, #66475, #2670, #10453, #48347 ) ) ;
#17361 = VERTEX_POINT ( 'NONE', #35165 ) ;
#17364 = EDGE_LOOP ( 'NONE', ( #51597, #58737, #37414, #47368 ) ) ;
#17363 = ADVANCED_FACE ( 'NONE', ( #6583 ), #62039, .F. ) ;
#17362 = CARTESIAN_POINT ( 'NONE',  ( -8.689999999999999503, -8.750000000000000000, -5.000000000000000000 ) ) ;
#17365 = ORIENTED_EDGE ( 'NONE', *, *, #46194, .F. ) ;
#17366 = EDGE_CURVE ( 'NONE', #35441, #57821, #40479, .T. ) ;
#17367 = FACE_OUTER_BOUND ( 'NONE', #20138, .T. ) ;
#17368 = DIRECTION ( 'NONE',  ( 0.000000000000000000, -0.9938079899998859545, 0.1111111111112941946 ) ) ;
#17369 = CARTESIAN_POINT ( 'NONE',  ( 7.450000000000003730, -7.249999999999997335, -20.50000000000000000 ) ) ;
#17370 = ADVANCED_FACE ( 'NONE', ( #39770 ), #2647, .F. ) ;
#17371 = SURFACE_STYLE_FILL_AREA ( #33970 ) ;
#17373 = DIRECTION ( 'NONE',  ( 1.836970198721029934E-16, -1.836970198721036344E-16, 1.000000000000000000 ) ) ;
#17372 = CARTESIAN_POINT ( 'NONE',  ( 0.000000000000000000, -8.249999999999998224, -13.00000000000000178 ) ) ;
#17374 = ORIENTED_EDGE ( 'NONE', *, *, #13891, .T. ) ;
#17376 = ORIENTED_EDGE ( 'NONE', *, *, #58776, .F. ) ;
#17375 = CARTESIAN_POINT ( 'NONE',  ( -7.281754163448141526, 8.000000000000000000, 5.000000000000000000 ) ) ;
#17377 = EDGE_LOOP ( 'NONE', ( #30040, #58550, #21594, #55961 ) ) ;
#17378 = ORIENTED_EDGE ( 'NONE', *, *, #69396, .F. ) ;
#17379 = FACE_OUTER_BOUND ( 'NONE', #12305, .T. ) ;
#17380 = DIRECTION ( 'NONE',  ( 1.000000000000000000, -0.000000000000000000, -0.000000000000000000 ) ) ;
#17381 = DIRECTION ( 'NONE',  ( -3.304235192336781428E-15, -1.000000000000000000, 0.000000000000000000 ) ) ;
#17382 = DIRECTION ( 'NONE',  ( -1.000000000000000000, 0.000000000000000000, 0.000000000000000000 ) ) ;
#17384 = EDGE_CURVE ( 'NONE', #59658, #6660, #39985, .T. ) ;
#17383 = ORIENTED_EDGE ( 'NONE', *, *, #35709, .T. ) ;
#17385 = ORIENTED_EDGE ( 'NONE', *, *, #37772, .F. ) ;
#17386 = DIRECTION ( 'NONE',  ( -1.000000000000000000, 0.000000000000000000, -0.000000000000000000 ) ) ;
#17387 = DIRECTION ( 'NONE',  ( -0.000000000000000000, -0.000000000000000000, 1.000000000000000000 ) ) ;
#17388 = VECTOR ( 'NONE', #36400, 1000.000000000000000 ) ;
#17389 = ORIENTED_EDGE ( 'NONE', *, *, #9919, .T. ) ;
#17390 = VERTEX_POINT ( 'NONE', #44378 ) ;
#17391 = LINE ( 'NONE', #6105, #324 ) ;
#17392 = DIRECTION ( 'NONE',  ( 0.000000000000000000, 1.000000000000000000, 0.000000000000000000 ) ) ;
#17393 = ORIENTED_EDGE ( 'NONE', *, *, #62750, .F. ) ;
#17394 = EDGE_CURVE ( 'NONE', #17018, #68958, #65953, .T. ) ;
#17395 = AXIS2_PLACEMENT_3D ( 'NONE', #65702, #32142, #27193 ) ;
#17396 = VECTOR ( 'NONE', #25220, 1000.000000000000000 ) ;
#17397 = DIRECTION ( 'NONE',  ( -1.000000000000000000, 0.000000000000000000, 0.000000000000000000 ) ) ;
#17399 = VERTEX_POINT ( 'NONE', #39091 ) ;
#17398 = CARTESIAN_POINT ( 'NONE',  ( 41.09999999999999432, -14.06939075806901940, -20.80000000000000426 ) ) ;
#17400 = ORIENTED_EDGE ( 'NONE', *, *, #51134, .F. ) ;
#17401 = CARTESIAN_POINT ( 'NONE',  ( -2.617976262117293285, -6.501044194225502615, 54.00000000000000711 ) ) ;
#17402 = CARTESIAN_POINT ( 'NONE',  ( -7.342976262117259623, 5.538810540049946773, 54.00000000000000711 ) ) ;
#17403 = AXIS2_PLACEMENT_3D ( 'NONE', #59533, #11085, #16047 ) ;
#17404 = CARTESIAN_POINT ( 'NONE',  ( 275.2499999999998295, -42.24999999999996447, 26.75000000000008527 ) ) ;
#17405 = EDGE_CURVE ( 'NONE', #46897, #52634, #33781, .T. ) ;
#17406 = DIRECTION ( 'NONE',  ( -4.336808689942025625E-15, -1.000000000000000000, 0.000000000000000000 ) ) ;
#17407 = EDGE_CURVE ( 'NONE', #44960, #17538, #23172, .T. ) ;
#17408 = DIRECTION ( 'NONE',  ( 0.000000000000000000, 0.000000000000000000, -1.000000000000000000 ) ) ;
#17409 = FACE_BOUND ( 'NONE', #4700, .T. ) ;
#17410 = AXIS2_PLACEMENT_3D ( 'NONE', #21231, #64354, #64022 ) ;
#17411 = ADVANCED_FACE ( 'NONE', ( #44727 ), #12894, .F. ) ;
#17412 = EDGE_CURVE ( 'NONE', #41539, #66591, #7607, .T. ) ;
#17413 = EDGE_LOOP ( 'NONE', ( #47758, #17587, #4100, #55326 ) ) ;
#17414 = DIRECTION ( 'NONE',  ( 8.951101527228106186E-17, 1.000000000000000000, -0.000000000000000000 ) ) ;
#17416 = ORIENTED_EDGE ( 'NONE', *, *, #5216, .T. ) ;
#17415 = DIRECTION ( 'NONE',  ( 1.356437060717834182E-15, 1.000000000000000000, 1.836970198721034125E-16 ) ) ;
#17417 = CYLINDRICAL_SURFACE ( 'NONE', #7246, 0.5249999999999994671 ) ;
#17418 = DIRECTION ( 'NONE',  ( 0.000000000000000000, 0.000000000000000000, -1.000000000000000000 ) ) ;
#17419 = VECTOR ( 'NONE', #29574, 1000.000000000000000 ) ;
#17420 = ADVANCED_FACE ( 'NONE', ( #12552 ), #55700, .F. ) ;
#17421 = LINE ( 'NONE', #32656, #8774 ) ;
#17422 = CIRCLE ( 'NONE', #35484, 0.3499999999999285905 ) ;
#17423 = CARTESIAN_POINT ( 'NONE',  ( 5.393625297349902148, 4.734785091273877811, 195.0000000000000284 ) ) ;
#17424 = DIRECTION ( 'NONE',  ( 3.491481338843133355E-15, 1.000000000000000000, 1.836970198721029934E-16 ) ) ;
#17425 = VERTEX_POINT ( 'NONE', #9000 ) ;
#17426 = VERTEX_POINT ( 'NONE', #30578 ) ;
#17427 = DIRECTION ( 'NONE',  ( -0.000000000000000000, -0.000000000000000000, -1.000000000000000000 ) ) ;
#17428 = DIRECTION ( 'NONE',  ( 0.000000000000000000, -1.000000000000000000, -0.000000000000000000 ) ) ;
#17429 = EDGE_LOOP ( 'NONE', ( #64795, #51645 ) ) ;
#17430 = CARTESIAN_POINT ( 'NONE',  ( -7.252248008019455128, 6.606374702650072983, 195.0000000000000284 ) ) ;
#17431 = ORIENTED_EDGE ( 'NONE', *, *, #27621, .F. ) ;
#17432 = VERTEX_POINT ( 'NONE', #30239 ) ;
#17433 = DIRECTION ( 'NONE',  ( 0.000000000000000000, 0.000000000000000000, 1.000000000000000000 ) ) ;
#17434 = CARTESIAN_POINT ( 'NONE',  ( -11.77351654964670935, 7.813516549646603693, 195.0000000000000284 ) ) ;
#17435 = ORIENTED_EDGE ( 'NONE', *, *, #65569, .T. ) ;
#17436 = DIRECTION ( 'NONE',  ( 0.000000000000000000, 0.000000000000000000, 1.000000000000000000 ) ) ;
#17437 = VECTOR ( 'NONE', #36546, 1000.000000000000000 ) ;
#17438 = CARTESIAN_POINT ( 'NONE',  ( 1.000000000000000000, -21.00000000000000000, 0.000000000000000000 ) ) ;
#17439 = FACE_OUTER_BOUND ( 'NONE', #64683, .T. ) ;
#17440 = CARTESIAN_POINT ( 'NONE',  ( 10.20488345035345645, 11.07551654964652954, 455.0000000000000568 ) ) ;
#17441 = ORIENTED_EDGE ( 'NONE', *, *, #49220, .T. ) ;
#17443 = ORIENTED_EDGE ( 'NONE', *, *, #13369, .F. ) ;
#17442 = DIRECTION ( 'NONE',  ( -0.000000000000000000, -0.000000000000000000, 1.000000000000000000 ) ) ;
#17444 = EDGE_CURVE ( 'NONE', #47285, #9687, #25638, .T. ) ;
#17445 = VECTOR ( 'NONE', #56394, 1000.000000000000000 ) ;
#17446 = VECTOR ( 'NONE', #61908, 1000.000000000000114 ) ;
#17447 = LINE ( 'NONE', #28399, #65358 ) ;
#17448 = DIRECTION ( 'NONE',  ( 0.000000000000000000, 0.000000000000000000, -1.000000000000000000 ) ) ;
#17449 = PLANE ( 'NONE',  #13137 ) ;
#17450 = CARTESIAN_POINT ( 'NONE',  ( -8.452095193409402185, 4.242044687070461784, 455.0000000000000568 ) ) ;
#17451 = ORIENTED_EDGE ( 'NONE', *, *, #40277, .T. ) ;
#17452 = ADVANCED_FACE ( 'NONE', ( #67702 ), #63459, .F. ) ;
#17453 = EDGE_CURVE ( 'NONE', #56866, #18784, #25986, .T. ) ;
#17454 = DIRECTION ( 'NONE',  ( 0.000000000000000000, -0.9938079899998859545, 0.1111111111112941946 ) ) ;
#17455 = CIRCLE ( 'NONE', #32107, 1.000000000000003553 ) ;
#17456 = CARTESIAN_POINT ( 'NONE',  ( 49.00000000000000000, -21.00000000000000000, 13.86939075806900057 ) ) ;
#17457 = CIRCLE ( 'NONE', #69410, 2.215251240775983899 ) ;
#17458 = ORIENTED_EDGE ( 'NONE', *, *, #18482, .F. ) ;
#17459 = ORIENTED_EDGE ( 'NONE', *, *, #2570, .F. ) ;
#17460 = ADVANCED_FACE ( 'NONE', ( #42229 ), #41177, .F. ) ;
#17462 = ORIENTED_EDGE ( 'NONE', *, *, #35862, .F. ) ;
#17461 = VECTOR ( 'NONE', #17463, 1000.000000000000000 ) ;
#17463 = DIRECTION ( 'NONE',  ( 0.7071067811865487940, 0.7071067811865463515, -0.000000000000000000 ) ) ;
#17464 = LINE ( 'NONE', #33726, #46727 ) ;
#17465 = DIRECTION ( 'NONE',  ( 0.000000000000000000, 0.000000000000000000, 1.000000000000000000 ) ) ;
#17466 =( NAMED_UNIT ( * ) SI_UNIT ( $, .STERADIAN. ) SOLID_ANGLE_UNIT ( ) );
#17467 = VECTOR ( 'NONE', #5528, 1000.000000000000000 ) ;
#17468 = AXIS2_PLACEMENT_3D ( 'NONE', #5444, #24975, #59162 ) ;
#17469 = ORIENTED_EDGE ( 'NONE', *, *, #14109, .F. ) ;
#17470 = EDGE_LOOP ( 'NONE', ( #22877, #53654, #10680, #62884 ) ) ;
#17471 = ORIENTED_EDGE ( 'NONE', *, *, #5702, .T. ) ;
#17472 = AXIS2_PLACEMENT_3D ( 'NONE', #19804, #20171, #30781 ) ;
#17473 = LINE ( 'NONE', #39039, #14747 ) ;
#17474 = ORIENTED_EDGE ( 'NONE', *, *, #15511, .T. ) ;
#17475 = VERTEX_POINT ( 'NONE', #63811 ) ;
#17476 = ORIENTED_EDGE ( 'NONE', *, *, #14208, .T. ) ;
#17477 = VERTEX_POINT ( 'NONE', #15018 ) ;
#17478 = CARTESIAN_POINT ( 'NONE',  ( 55.00000000000000000, 21.00000000000000000, 16.96999999999999886 ) ) ;
#17480 = ORIENTED_EDGE ( 'NONE', *, *, #14197, .F. ) ;
#17479 = LINE ( 'NONE', #55325, #58242 ) ;
#17481 = CARTESIAN_POINT ( 'NONE',  ( 7.428221114744952835, 3.593516549646614155, 195.0000000000000284 ) ) ;
#17482 = DIRECTION ( 'NONE',  ( 0.7071067811865463515, -0.7071067811865487940, 0.000000000000000000 ) ) ;
#17483 = FACE_OUTER_BOUND ( 'NONE', #6605, .T. ) ;
#17484 = VECTOR ( 'NONE', #11276, 1000.000000000000000 ) ;
#17485 = ORIENTED_EDGE ( 'NONE', *, *, #16643, .T. ) ;
#17486 = AXIS2_PLACEMENT_3D ( 'NONE', #33020, #39696, #17098 ) ;
#17487 = LINE ( 'NONE', #53000, #68980 ) ;
#17488 = LINE ( 'NONE', #59599, #37972 ) ;
#17489 = FACE_OUTER_BOUND ( 'NONE', #53387, .T. ) ;
#17490 = ADVANCED_FACE ( 'NONE', ( #46832 ), #15374, .F. ) ;
#17491 = ORIENTED_EDGE ( 'NONE', *, *, #6029, .T. ) ;
#17492 = DIRECTION ( 'NONE',  ( 0.000000000000000000, 0.000000000000000000, 1.000000000000000000 ) ) ;
#17493 = AXIS2_PLACEMENT_3D ( 'NONE', #20911, #69002, #43515 ) ;
#17495 = CARTESIAN_POINT ( 'NONE',  ( 7.357023737882817827, -4.961189459950063885, 54.00000000000000711 ) ) ;
#17494 = VECTOR ( 'NONE', #18683, 1000.000000000000000 ) ;
#17496 = CARTESIAN_POINT ( 'NONE',  ( 38.90000000000000568, 13.66939075806899240, 20.79999999999999361 ) ) ;
#17497 = EDGE_CURVE ( 'NONE', #1158, #47752, #19709, .T. ) ;
#17498 = VECTOR ( 'NONE', #68259, 1000.000000000000114 ) ;
#17499 = ADVANCED_FACE ( 'NONE', ( #41540 ), #8294, .T. ) ;
#17500 = ORIENTED_EDGE ( 'NONE', *, *, #16554, .T. ) ;
#17501 = FACE_OUTER_BOUND ( 'NONE', #39885, .T. ) ;
#17502 = VECTOR ( 'NONE', #1720, 1000.000000000000000 ) ;
#17503 = AXIS2_PLACEMENT_3D ( 'NONE', #16432, #9737, #42604 ) ;
#17504 = FACE_OUTER_BOUND ( 'NONE', #63465, .T. ) ;
#17505 = CARTESIAN_POINT ( 'NONE',  ( -8.697938382363185283, -8.093267424590415260, 54.00000000000000711 ) ) ;
#17506 = VERTEX_POINT ( 'NONE', #36226 ) ;
#17507 = VECTOR ( 'NONE', #51033, 1000.000000000000114 ) ;
#17508 = DIRECTION ( 'NONE',  ( 0.000000000000000000, -0.7071067811865475727, -0.7071067811865475727 ) ) ;
#17509 = CARTESIAN_POINT ( 'NONE',  ( 283.0000000000000568, -25.60000000000000142, 15.10000000000000142 ) ) ;
#17510 = CARTESIAN_POINT ( 'NONE',  ( -4.141586236041100655, 4.706725378239165813, 54.00000000000000711 ) ) ;
#17512 = EDGE_CURVE ( 'NONE', #58882, #5244, #10697, .T. ) ;
#17511 = CARTESIAN_POINT ( 'NONE',  ( -8.821682069070780230, 2.530476262117183683, 54.00000000000000711 ) ) ;
#17513 = CARTESIAN_POINT ( 'NONE',  ( -10.30047626211725742, 6.835476262117182955, 26.00000000000000711 ) ) ;
#17514 = AXIS2_PLACEMENT_3D ( 'NONE', #10478, #64237, #64576 ) ;
#17515 = ORIENTED_EDGE ( 'NONE', *, *, #22951, .T. ) ;
#17516 = PLANE ( 'NONE',  #51889 ) ;
#17517 = DIRECTION ( 'NONE',  ( 1.000000000000000000, -0.000000000000000000, -0.000000000000000000 ) ) ;
#17518 = AXIS2_PLACEMENT_3D ( 'NONE', #29412, #61575, #13148 ) ;
#17519 = DIRECTION ( 'NONE',  ( 0.000000000000000000, 0.7071067811865475727, 0.7071067811865475727 ) ) ;
#17520 = DIRECTION ( 'NONE',  ( -1.000000000000000000, 0.000000000000000000, 0.000000000000000000 ) ) ;
#17521 = ORIENTED_EDGE ( 'NONE', *, *, #24120, .T. ) ;
#17522 = CARTESIAN_POINT ( 'NONE',  ( 4.406483450353335662, -11.78648345035347766, 455.0000000000000568 ) ) ;
#17523 = CARTESIAN_POINT ( 'NONE',  ( 8.000000000000000000, 7.281754163448145079, 5.000000000000000000 ) ) ;
#17524 = CARTESIAN_POINT ( 'NONE',  ( 15.00000000000000000, -21.00000000000000000, 0.000000000000000000 ) ) ;
#17525 = DIRECTION ( 'NONE',  ( -0.000000000000000000, -0.000000000000000000, 1.000000000000000000 ) ) ;
#17526 = CARTESIAN_POINT ( 'NONE',  ( 7.250000000000005329, -7.249999999999998224, -18.00000000000000000 ) ) ;
#17527 = ORIENTED_EDGE ( 'NONE', *, *, #42, .F. ) ;
#17528 = DIRECTION ( 'NONE',  ( 0.000000000000000000, 0.000000000000000000, 1.000000000000000000 ) ) ;
#17529 = PLANE ( 'NONE',  #34527 ) ;
#17530 = ORIENTED_EDGE ( 'NONE', *, *, #21595, .F. ) ;
#17531 = CARTESIAN_POINT ( 'NONE',  ( 27.90000000000000213, 20.60000000000000142, -13.86939075806900057 ) ) ;
#17532 = AXIS2_PLACEMENT_3D ( 'NONE', #61423, #45168, #67803 ) ;
#17533 = EDGE_LOOP ( 'NONE', ( #4720, #17708, #51546, #23615 ) ) ;
#17534 = EDGE_CURVE ( 'NONE', #56499, #34373, #9721, .T. ) ;
#17535 = VECTOR ( 'NONE', #62217, 1000.000000000000000 ) ;
#17536 = DIRECTION ( 'NONE',  ( 0.000000000000000000, 0.000000000000000000, -1.000000000000000000 ) ) ;
#17537 = ORIENTED_EDGE ( 'NONE', *, *, #27414, .F. ) ;
#17538 = VERTEX_POINT ( 'NONE', #29872 ) ;
#17539 = DIRECTION ( 'NONE',  ( -0.8660254037844482555, 0.000000000000000000, -0.4999999999999831801 ) ) ;
#17540 = LINE ( 'NONE', #32442, #63663 ) ;
#17541 = FACE_OUTER_BOUND ( 'NONE', #54040, .T. ) ;
#17542 = CARTESIAN_POINT ( 'NONE',  ( 30.00000000000000000, -16.28999999999710369, 15.00000000000794920 ) ) ;
#17543 = AXIS2_PLACEMENT_3D ( 'NONE', #26026, #68096, #47579 ) ;
#17544 = VECTOR ( 'NONE', #1341, 1000.000000000000000 ) ;
#17545 = VECTOR ( 'NONE', #6612, 1000.000000000000000 ) ;
#17546 = ORIENTED_EDGE ( 'NONE', *, *, #46633, .F. ) ;
#17547 = VERTEX_POINT ( 'NONE', #46136 ) ;
#17548 = CARTESIAN_POINT ( 'NONE',  ( 17.51999999999999957, -15.50000000000000000, 26.00000000000000355 ) ) ;
#17549 = LINE ( 'NONE', #59992, #27712 ) ;
#17550 = VECTOR ( 'NONE', #29613, 1000.000000000000000 ) ;
#17551 = VECTOR ( 'NONE', #69750, 1000.000000000000000 ) ;
#17552 = EDGE_CURVE ( 'NONE', #52724, #34676, #4426, .T. ) ;
#17553 = ORIENTED_EDGE ( 'NONE', *, *, #23665, .T. ) ;
#17554 = ORIENTED_EDGE ( 'NONE', *, *, #1802, .T. ) ;
#17555 = VERTEX_POINT ( 'NONE', #35514 ) ;
#17556 = VECTOR ( 'NONE', #12589, 1000.000000000000000 ) ;
#17557 = EDGE_CURVE ( 'NONE', #30268, #22923, #49150, .T. ) ;
#17558 = CARTESIAN_POINT ( 'NONE',  ( -7.450000000000001954, 7.250000000000000000, -14.00000000000000000 ) ) ;
#17559 = CARTESIAN_POINT ( 'NONE',  ( 30.00000000000000000, -11.70000000000000284, 12.50000000000000000 ) ) ;
#17561 = ORIENTED_EDGE ( 'NONE', *, *, #52383, .T. ) ;
#17560 = CARTESIAN_POINT ( 'NONE',  ( -6.350872789121373430, -6.836383711242974393, 26.00000000000000711 ) ) ;
#17562 = CARTESIAN_POINT ( 'NONE',  ( 9.804883450353379715, -11.08848345035339733, 195.0000000000000284 ) ) ;
#17563 = CARTESIAN_POINT ( 'NONE',  ( -2.693516549646682190, 10.08346604330774454, 195.0000000000000284 ) ) ;
#17564 = VERTEX_POINT ( 'NONE', #52502 ) ;
#17565 = CIRCLE ( 'NONE', #69518, 0.1749999999999998224 ) ;
#17566 = ORIENTED_EDGE ( 'NONE', *, *, #2429, .T. ) ;
#17567 = DIRECTION ( 'NONE',  ( 0.000000000000000000, 1.000000000000000000, 0.000000000000000000 ) ) ;
#17568 = DIRECTION ( 'NONE',  ( 1.000000000000000000, 0.000000000000000000, 0.000000000000000000 ) ) ;
#17569 = LINE ( 'NONE', #44777, #61965 ) ;
#17570 = EDGE_CURVE ( 'NONE', #19917, #55314, #68325, .T. ) ;
#17571 = DIRECTION ( 'NONE',  ( 0.8660254037844363761, -0.5000000000000038858, -1.836970198721044232E-16 ) ) ;
#17572 = EDGE_CURVE ( 'NONE', #2931, #51393, #36738, .T. ) ;
#17573 = ADVANCED_FACE ( 'NONE', ( #52871 ), #63106, .T. ) ;
#17574 = VECTOR ( 'NONE', #60635, 1000.000000000000000 ) ;
#17575 = ORIENTED_EDGE ( 'NONE', *, *, #3846, .T. ) ;
#17576 = ORIENTED_EDGE ( 'NONE', *, *, #11354, .T. ) ;
#17577 = DIRECTION ( 'NONE',  ( 1.000000000000000000, 0.000000000000000000, 0.000000000000000000 ) ) ;
#17578 = LINE ( 'NONE', #38803, #22836 ) ;
#17579 = EDGE_CURVE ( 'NONE', #33956, #11076, #31988, .T. ) ;
#17580 = AXIS2_PLACEMENT_3D ( 'NONE', #44738, #61347, #39105 ) ;
#17581 = CARTESIAN_POINT ( 'NONE',  ( 49.00000000000000000, 13.66939075806899950, 20.80000000000000426 ) ) ;
#17582 = CARTESIAN_POINT ( 'NONE',  ( -15.70313394609756585, -0.2715358723600081459, 21.17390376548697262 ) ) ;
#17583 = ADVANCED_FACE ( 'NONE', ( #27026 ), #37290, .T. ) ;
#17584 = AXIS2_PLACEMENT_3D ( 'NONE', #9448, #31012, #64586 ) ;
#17585 = CARTESIAN_POINT ( 'NONE',  ( 35.89999999999999858, 20.60000000000000142, -13.86939075806900057 ) ) ;
#17586 = ADVANCED_FACE ( 'NONE', ( #5111 ), #43968, .F. ) ;
#17587 = ORIENTED_EDGE ( 'NONE', *, *, #24974, .F. ) ;
#17588 = DIRECTION ( 'NONE',  ( -1.000000000000000000, 0.000000000000000000, 0.000000000000000000 ) ) ;
#17589 = PLANE ( 'NONE',  #29344 ) ;
#17591 = EDGE_CURVE ( 'NONE', #19691, #33306, #43483, .T. ) ;
#17590 = DIRECTION ( 'NONE',  ( 1.000000000000000000, -0.000000000000000000, 0.000000000000000000 ) ) ;
#17592 = DIRECTION ( 'NONE',  ( -0.000000000000000000, -0.000000000000000000, -1.000000000000000000 ) ) ;
#17593 = VECTOR ( 'NONE', #25233, 1000.000000000000000 ) ;
#17594 = AXIS2_PLACEMENT_3D ( 'NONE', #17166, #11165, #39419 ) ;
#17595 = AXIS2_PLACEMENT_3D ( 'NONE', #13474, #17387, #23040 ) ;
#17596 = DIRECTION ( 'NONE',  ( -1.000000000000000000, 0.000000000000000000, 0.000000000000000000 ) ) ;
#17597 = DIRECTION ( 'NONE',  ( 1.000000000000000000, -0.000000000000000000, 0.000000000000000000 ) ) ;
#17598 = AXIS2_PLACEMENT_3D ( 'NONE', #65972, #44395, #17536 ) ;
#17599 = VECTOR ( 'NONE', #51652, 1000.000000000000000 ) ;
#17600 = LINE ( 'NONE', #54066, #66990 ) ;
#17601 = VERTEX_POINT ( 'NONE', #47883 ) ;
#17602 = CARTESIAN_POINT ( 'NONE',  ( -11.00000000000000000, -14.04000000000000092, 14.80000000000000071 ) ) ;
#17603 = CARTESIAN_POINT ( 'NONE',  ( -3.593516549646714520, -4.622483450353405132, 195.0000000000000284 ) ) ;
#17604 = VERTEX_POINT ( 'NONE', #59200 ) ;
#17605 = CARTESIAN_POINT ( 'NONE',  ( 15.00000000000000000, -42.50000000000000000, -26.50000000000000000 ) ) ;
#17606 = LINE ( 'NONE', #7682, #61704 ) ;
#17607 = VECTOR ( 'NONE', #37679, 999.9999999999998863 ) ;
#17608 = DIRECTION ( 'NONE',  ( 1.000000000000000000, 0.000000000000000000, 0.000000000000000000 ) ) ;
#17609 = CARTESIAN_POINT ( 'NONE',  ( 7.272650909786597673, 7.798499376343980494, 195.0000000000000284 ) ) ;
#17610 = FACE_OUTER_BOUND ( 'NONE', #40695, .T. ) ;
#17611 = ORIENTED_EDGE ( 'NONE', *, *, #46640, .F. ) ;
#17612 = CARTESIAN_POINT ( 'NONE',  ( 0.000000000000000000, -8.249999999999998224, -9.500000000000001776 ) ) ;
#17613 = VECTOR ( 'NONE', #28383, 1000.000000000000000 ) ;
#17614 = EDGE_LOOP ( 'NONE', ( #22362, #52332, #36894, #5355 ) ) ;
#17615 = LINE ( 'NONE', #43449, #27745 ) ;
#17616 = EDGE_CURVE ( 'NONE', #35460, #58904, #14106, .T. ) ;
#17617 = ORIENTED_EDGE ( 'NONE', *, *, #35341, .T. ) ;
#17618 = VECTOR ( 'NONE', #42738, 1000.000000000000000 ) ;
#17619 = CARTESIAN_POINT ( 'NONE',  ( -7.342976262117282715, -5.552858015815545834, 54.00000000000000711 ) ) ;
#17620 = ADVANCED_FACE ( 'NONE', ( #10414 ), #65544, .F. ) ;
#17621 = CARTESIAN_POINT ( 'NONE',  ( 25.50000000000000355, 0.000000000000000000, -22.50000000000000000 ) ) ;
#17622 = ORIENTED_EDGE ( 'NONE', *, *, #9158, .F. ) ;
#17623 = EDGE_LOOP ( 'NONE', ( #64345, #44022, #50954, #5759 ) ) ;
#17624 = LINE ( 'NONE', #13002, #9288 ) ;
#17625 = ORIENTED_EDGE ( 'NONE', *, *, #22120, .F. ) ;
#17626 = EDGE_CURVE ( 'NONE', #325, #44836, #69817, .T. ) ;
#17627 = ORIENTED_EDGE ( 'NONE', *, *, #49625, .F. ) ;
#17628 = DIRECTION ( 'NONE',  ( 0.000000000000000000, 1.000000000000000000, -0.000000000000000000 ) ) ;
#17629 = CARTESIAN_POINT ( 'NONE',  ( -7.450000000000001954, 7.250000000000000000, -12.50000000000000000 ) ) ;
#17630 = CARTESIAN_POINT ( 'NONE',  ( -9.689726262117227762, 8.566576262117216345, 54.00000000000000711 ) ) ;
#17631 = AXIS2_PLACEMENT_3D ( 'NONE', #7840, #66889, #66213 ) ;
#17632 = ORIENTED_EDGE ( 'NONE', *, *, #13202, .F. ) ;
#17633 = FACE_OUTER_BOUND ( 'NONE', #19547, .T. ) ;
#17635 = DIRECTION ( 'NONE',  ( -1.836970198721029934E-16, 1.836970198721036590E-16, -1.000000000000000000 ) ) ;
#17634 = DIRECTION ( 'NONE',  ( 1.000000000000000000, -9.050731179009442381E-15, 0.000000000000000000 ) ) ;
#17636 = ORIENTED_EDGE ( 'NONE', *, *, #25504, .T. ) ;
#17638 = VERTEX_POINT ( 'NONE', #58857 ) ;
#17637 = CARTESIAN_POINT ( 'NONE',  ( 47.00000000000000000, -0.7500000000000000000, -4.943429983321300014 ) ) ;
#17639 = VECTOR ( 'NONE', #58874, 1000.000000000000000 ) ;
#17640 = ORIENTED_EDGE ( 'NONE', *, *, #4732, .T. ) ;
#17641 = DIRECTION ( 'NONE',  ( 1.000000000000000000, 0.000000000000000000, 0.000000000000000000 ) ) ;
#17642 = AXIS2_PLACEMENT_3D ( 'NONE', #20320, #53908, #57797 ) ;
#17643 = EDGE_CURVE ( 'NONE', #268, #23882, #18637, .T. ) ;
#17644 = FACE_OUTER_BOUND ( 'NONE', #51818, .T. ) ;
#17645 = AXIS2_PLACEMENT_3D ( 'NONE', #44272, #5078, #5779 ) ;
#17646 = VECTOR ( 'NONE', #66, 1000.000000000000000 ) ;
#17647 = VECTOR ( 'NONE', #43139, 1000.000000000000000 ) ;
#17648 = DIRECTION ( 'NONE',  ( -0.7071067811865486830, -0.7071067811865464625, 0.000000000000000000 ) ) ;
#17649 = ORIENTED_EDGE ( 'NONE', *, *, #24208, .T. ) ;
#17650 = EDGE_CURVE ( 'NONE', #51110, #9490, #10070, .T. ) ;
#17651 = ORIENTED_EDGE ( 'NONE', *, *, #62506, .F. ) ;
#17652 = EDGE_CURVE ( 'NONE', #41347, #20252, #21014, .T. ) ;
#17653 = AXIS2_PLACEMENT_3D ( 'NONE', #28033, #6793, #49593 ) ;
#17654 = AXIS2_PLACEMENT_3D ( 'NONE', #27231, #26184, #21235 ) ;
#17655 = CIRCLE ( 'NONE', #16512, 0.1749999999999998224 ) ;
#17656 = DIRECTION ( 'NONE',  ( -1.000000000000000000, 0.000000000000000000, 0.000000000000000000 ) ) ;
#17657 = LINE ( 'NONE', #55493, #21047 ) ;
#17658 = EDGE_CURVE ( 'NONE', #44658, #4958, #27715, .T. ) ;
#17659 = ADVANCED_FACE ( 'NONE', ( #42584 ), #16068, .T. ) ;
#17660 = EDGE_CURVE ( 'NONE', #56266, #37419, #31641, .T. ) ;
#17661 = VERTEX_POINT ( 'NONE', #48941 ) ;
#17662 = CARTESIAN_POINT ( 'NONE',  ( 22.90000000000000213, -21.00000000000000000, 13.86939075806900057 ) ) ;
#17664 = AXIS2_PLACEMENT_3D ( 'NONE', #2610, #24184, #24543 ) ;
#17663 = CARTESIAN_POINT ( 'NONE',  ( -7.261609891743268541, -8.000000000000000000, -1.000000000000000000 ) ) ;
#17665 = CARTESIAN_POINT ( 'NONE',  ( 3.606483450353369147, -7.428221114745098497, 455.0000000000000568 ) ) ;
#17666 = ORIENTED_EDGE ( 'NONE', *, *, #33628, .T. ) ;
#17667 = EDGE_CURVE ( 'NONE', #63525, #23322, #869, .T. ) ;
#17668 = CARTESIAN_POINT ( 'NONE',  ( -4.734785091274032354, -5.393625297349961656, 455.0000000000000568 ) ) ;
#17669 = EDGE_CURVE ( 'NONE', #62844, #23208, #48591, .T. ) ;
#17670 = DIRECTION ( 'NONE',  ( 1.000000000000000000, -6.508391731846280553E-15, -1.836970198721042260E-16 ) ) ;
#17672 = ORIENTED_EDGE ( 'NONE', *, *, #34487, .T. ) ;
#17671 = DIRECTION ( 'NONE',  ( 1.000000000000000000, 0.000000000000000000, 0.000000000000000000 ) ) ;
#17674 = EDGE_LOOP ( 'NONE', ( #67475, #41583, #37656, #65747 ) ) ;
#17673 = CARTESIAN_POINT ( 'NONE',  ( 49.00000000000000000, 0.000000000000000000, 0.000000000000000000 ) ) ;
#17675 = CARTESIAN_POINT ( 'NONE',  ( -6.331612867284154511, 8.393516549646601987, 455.0000000000000568 ) ) ;
#17676 = DIRECTION ( 'NONE',  ( 0.000000000000000000, 1.000000000000000000, 0.000000000000000000 ) ) ;
#17677 = DIRECTION ( 'NONE',  ( 0.000000000000000000, 0.000000000000000000, 1.000000000000000000 ) ) ;
#17678 = PLANE ( 'NONE',  #63308 ) ;
#17679 = CARTESIAN_POINT ( 'NONE',  ( -0.9414762621173187185, -9.404523737882845680, 26.00000000000000711 ) ) ;
#17680 = EDGE_CURVE ( 'NONE', #8070, #17836, #15290, .T. ) ;
#17681 = EDGE_LOOP ( 'NONE', ( #20775, #59882, #24668, #2456 ) ) ;
#17682 = DIRECTION ( 'NONE',  ( 0.000000000000000000, 0.000000000000000000, -1.000000000000000000 ) ) ;
#17683 = CARTESIAN_POINT ( 'NONE',  ( 12.00648345035338060, -4.186483450353492231, 455.0000000000000568 ) ) ;
#17685 = EDGE_CURVE ( 'NONE', #31223, #23962, #43634, .T. ) ;
#17684 = FILL_AREA_STYLE_COLOUR ( '', #34456 ) ;
#17687 = ORIENTED_EDGE ( 'NONE', *, *, #22054, .F. ) ;
#17686 = CARTESIAN_POINT ( 'NONE',  ( 283.0000000000000568, -26.42999999999999972, -9.412893218813501051 ) ) ;
#17688 = CARTESIAN_POINT ( 'NONE',  ( 7.899999999999999467, -21.00000000000000000, -14.57806571531351914 ) ) ;
#17689 = CIRCLE ( 'NONE', #47073, 3.499999999999040323 ) ;
#17690 = DIRECTION ( 'NONE',  ( 0.000000000000000000, 1.000000000000000000, 0.000000000000000000 ) ) ;
#17691 = AXIS2_PLACEMENT_3D ( 'NONE', #11453, #54960, #60235 ) ;
#17692 = ORIENTED_EDGE ( 'NONE', *, *, #68349, .F. ) ;
#17693 = CARTESIAN_POINT ( 'NONE',  ( 41.09999999999999432, 13.66939075806899950, -20.80000000000000426 ) ) ;
#17694 = CARTESIAN_POINT ( 'NONE',  ( -1.853252480934834745, -9.417013320880835536, 195.0000000000000284 ) ) ;
#17695 = EDGE_CURVE ( 'NONE', #37001, #4376, #54801, .T. ) ;
#17696 = ORIENTED_EDGE ( 'NONE', *, *, #16239, .T. ) ;
#17697 = CARTESIAN_POINT ( 'NONE',  ( 275.0000000000000000, -25.60000000000000142, -17.60000000000000142 ) ) ;
#17698 = DIRECTION ( 'NONE',  ( -1.000000000000000000, 0.000000000000000000, 0.000000000000000000 ) ) ;
#17699 = AXIS2_PLACEMENT_3D ( 'NONE', #4643, #26207, #42467 ) ;
#17700 = AXIS2_PLACEMENT_3D ( 'NONE', #60102, #27586, #49159 ) ;
#17701 = DIRECTION ( 'NONE',  ( -0.000000000000000000, -0.000000000000000000, 1.000000000000000000 ) ) ;
#17702 = CARTESIAN_POINT ( 'NONE',  ( 17.89999999999999858, 13.66939075806899240, -20.79999999999999361 ) ) ;
#17703 = CIRCLE ( 'NONE', #41427, 0.5000000000001386669 ) ;
#17705 = CARTESIAN_POINT ( 'NONE',  ( -5.242976262117259978, 7.172176262117182510, 54.00000000000000711 ) ) ;
#17704 = AXIS2_PLACEMENT_3D ( 'NONE', #364, #16637, #26540 ) ;
#17706 = VERTEX_POINT ( 'NONE', #44647 ) ;
#17707 = FACE_OUTER_BOUND ( 'NONE', #6087, .T. ) ;
#17708 = ORIENTED_EDGE ( 'NONE', *, *, #25504, .F. ) ;
#17709 = ORIENTED_EDGE ( 'NONE', *, *, #5439, .T. ) ;
#17710 = CARTESIAN_POINT ( 'NONE',  ( -5.380658396643233310, 7.252248008019342329, 455.0000000000000568 ) ) ;
#17712 = CARTESIAN_POINT ( 'NONE',  ( 8.250000000000005329, 7.250000000000000888, -15.50000000000000000 ) ) ;
#17711 = CIRCLE ( 'NONE', #41433, 0.1749999999999998224 ) ;
#17713 = AXIS2_PLACEMENT_3D ( 'NONE', #29193, #67399, #18953 ) ;
#17714 = EDGE_CURVE ( 'NONE', #58012, #1031, #60225, .T. ) ;
#17715 = CIRCLE ( 'NONE', #65188, 4.000000000000000000 ) ;
#17716 = LINE ( 'NONE', #30679, #32959 ) ;
#17717 = EDGE_LOOP ( 'NONE', ( #12576, #62345, #56512, #8730 ) ) ;
#17718 = ORIENTED_EDGE ( 'NONE', *, *, #55206, .T. ) ;
#17719 = CARTESIAN_POINT ( 'NONE',  ( 30.00000000000000000, -10.85999999999999943, 9.350000000000269651 ) ) ;
#17720 = EDGE_LOOP ( 'NONE', ( #2725, #54906, #48114, #36626 ) ) ;
#17721 = EDGE_CURVE ( 'NONE', #67547, #8948, #18470, .T. ) ;
#17722 = PRODUCT ( 'END CAP_6266N13', 'END CAP_6266N13', '', ( #37409 ) ) ;
#17723 = DIRECTION ( 'NONE',  ( 0.000000000000000000, 1.000000000000000000, 0.000000000000000000 ) ) ;
#17724 = LINE ( 'NONE', #8137, #18456 ) ;
#17725 = CARTESIAN_POINT ( 'NONE',  ( 5.257023737882801306, 6.467976262117199227, 54.00000000000000711 ) ) ;
#17726 = ADVANCED_FACE ( 'NONE', ( #39011 ), #61250, .F. ) ;
#17727 = CYLINDRICAL_SURFACE ( 'NONE', #62729, 1.000000000000000000 ) ;
#17729 = CARTESIAN_POINT ( 'NONE',  ( 290.0000000000000000, -21.00000000000000000, 0.000000000000000000 ) ) ;
#17728 = FACE_OUTER_BOUND ( 'NONE', #13485, .T. ) ;
#17730 = ORIENTED_EDGE ( 'NONE', *, *, #41863, .F. ) ;
#17731 = EDGE_CURVE ( 'NONE', #43147, #2261, #50248, .T. ) ;
#17733 = ORIENTED_EDGE ( 'NONE', *, *, #46302, .F. ) ;
#17732 = CYLINDRICAL_SURFACE ( 'NONE', #26244, 1.224999999999999423 ) ;
#17734 = ORIENTED_EDGE ( 'NONE', *, *, #6868, .F. ) ;
#17735 = EDGE_LOOP ( 'NONE', ( #62653, #52151, #19919, #43200 ) ) ;
#17736 = EDGE_CURVE ( 'NONE', #57882, #31408, #51008, .T. ) ;
#17737 = DIRECTION ( 'NONE',  ( 0.7071067811865474617, -0.7071067811865474617, -2.597868168706479611E-16 ) ) ;
#17738 = DIRECTION ( 'NONE',  ( 1.000000000000000000, -0.000000000000000000, -0.000000000000000000 ) ) ;
#17739 = DIRECTION ( 'NONE',  ( -1.836970198721029934E-16, 1.836970198721036344E-16, -1.000000000000000000 ) ) ;
#17740 = ORIENTED_EDGE ( 'NONE', *, *, #31428, .T. ) ;
#17741 = CIRCLE ( 'NONE', #10986, 5.000000000000000000 ) ;
#17742 = EDGE_LOOP ( 'NONE', ( #9546, #42734, #37942, #8250 ) ) ;
#17743 = CARTESIAN_POINT ( 'NONE',  ( -2.693516549646820746, -10.09643294401462832, 455.0000000000000568 ) ) ;
#17744 = DIRECTION ( 'NONE',  ( -1.000000000000000000, 0.000000000000000000, 0.000000000000000000 ) ) ;
#17745 = ORIENTED_EDGE ( 'NONE', *, *, #13231, .T. ) ;
#17746 = EDGE_CURVE ( 'NONE', #22764, #36489, #60576, .T. ) ;
#17747 = ORIENTED_EDGE ( 'NONE', *, *, #9658, .T. ) ;
#17748 = AXIS2_PLACEMENT_3D ( 'NONE', #19330, #14025, #47609 ) ;
#17749 = FACE_OUTER_BOUND ( 'NONE', #44408, .T. ) ;
#17750 = CARTESIAN_POINT ( 'NONE',  ( -11.19000000000000128, -11.25000000000000000, -4.250000000000000000 ) ) ;
#17751 = EDGE_LOOP ( 'NONE', ( #60511, #8262, #35100, #7517 ) ) ;
#17752 = VECTOR ( 'NONE', #24495, 1000.000000000000000 ) ;
#17753 = CIRCLE ( 'NONE', #30174, 0.5000000000079362072 ) ;
#17754 =( GEOMETRIC_REPRESENTATION_CONTEXT ( 3 ) GLOBAL_UNCERTAINTY_ASSIGNED_CONTEXT ( ( #65730 ) ) GLOBAL_UNIT_ASSIGNED_CONTEXT ( ( #62162, #19720, #29994 ) ) REPRESENTATION_CONTEXT ( 'NONE', 'WORKASPACE' ) );
#17755 = DIRECTION ( 'NONE',  ( -0.000000000000000000, -0.000000000000000000, 1.000000000000000000 ) ) ;
#17757 = VERTEX_POINT ( 'NONE', #45001 ) ;
#17756 = CARTESIAN_POINT ( 'NONE',  ( -3.663616288757090445, -4.149127210878730487, 54.00000000000000711 ) ) ;
#17758 = VERTEX_POINT ( 'NONE', #28066 ) ;
#17759 = CARTESIAN_POINT ( 'NONE',  ( 9.247904806590689475, -9.955011587777349291, 455.0000000000000568 ) ) ;
#17760 = VECTOR ( 'NONE', #27428, 1000.000000000000000 ) ;
#17761 = LINE ( 'NONE', #13071, #40196 ) ;
#17762 = CONICAL_SURFACE ( 'NONE', #8726, 1.621000000000000885, 0.7853981633974518317 ) ;
#17763 = DIRECTION ( 'NONE',  ( 0.000000000000000000, 0.000000000000000000, 1.000000000000000000 ) ) ;
#17764 = CYLINDRICAL_SURFACE ( 'NONE', #2162, 1.500000000000849543 ) ;
#17765 = DIRECTION ( 'NONE',  ( 0.000000000000000000, 0.000000000000000000, -1.000000000000000000 ) ) ;
#17766 = CARTESIAN_POINT ( 'NONE',  ( -10.30047626211725742, 3.650476262117184234, 54.00000000000000711 ) ) ;
#17767 = ADVANCED_FACE ( 'NONE', ( #23448 ), #60915, .F. ) ;
#17768 = ORIENTED_EDGE ( 'NONE', *, *, #54033, .T. ) ;
#17769 = DIRECTION ( 'NONE',  ( 1.000000000000000000, -0.000000000000000000, -0.000000000000000000 ) ) ;
#17772 = VERTEX_POINT ( 'NONE', #49958 ) ;
#17771 = EDGE_CURVE ( 'NONE', #16082, #7775, #22750, .T. ) ;
#17770 = DIRECTION ( 'NONE',  ( 0.7071067811865398012, -0.7071067811865552333, 0.000000000000000000 ) ) ;
#17773 = CIRCLE ( 'NONE', #33568, 0.1999999999999996503 ) ;
#17774 = CARTESIAN_POINT ( 'NONE',  ( 11.08848345035342042, 11.47551654964652812, 455.0000000000000568 ) ) ;
#17775 = FACE_OUTER_BOUND ( 'NONE', #16275, .T. ) ;
#17776 = CARTESIAN_POINT ( 'NONE',  ( 40.90000000000000568, 13.66939075806899950, 20.80000000000000426 ) ) ;
#17777 = CYLINDRICAL_SURFACE ( 'NONE', #176, 0.1999999999999987899 ) ;
#17778 = DIRECTION ( 'NONE',  ( 0.000000000000000000, 0.000000000000000000, -1.000000000000000000 ) ) ;
#17779 = VERTEX_POINT ( 'NONE', #12813 ) ;
#17780 = ORIENTED_EDGE ( 'NONE', *, *, #60881, .F. ) ;
#17781 = PLANE ( 'NONE',  #8754 ) ;
#17782 = LINE ( 'NONE', #858, #21005 ) ;
#17783 = FACE_OUTER_BOUND ( 'NONE', #14482, .T. ) ;
#17784 = ORIENTED_EDGE ( 'NONE', *, *, #53930, .T. ) ;
#17785 = CARTESIAN_POINT ( 'NONE',  ( 25.50000000000000355, -15.50000000000000000, 22.50000000000000000 ) ) ;
#17786 = ORIENTED_EDGE ( 'NONE', *, *, #49275, .F. ) ;
#17787 = ORIENTED_EDGE ( 'NONE', *, *, #20059, .T. ) ;
#17788 = PLANE ( 'NONE',  #52816 ) ;
#17789 = FACE_BOUND ( 'NONE', #63864, .T. ) ;
#17790 = ORIENTED_EDGE ( 'NONE', *, *, #28756, .F. ) ;
#17791 = DIRECTION ( 'NONE',  ( 0.000000000000000000, 1.000000000000000000, 0.000000000000000000 ) ) ;
#17792 = VECTOR ( 'NONE', #50093, 1000.000000000000000 ) ;
#17793 = AXIS2_PLACEMENT_3D ( 'NONE', #60288, #19167, #39077 ) ;
#17794 = VECTOR ( 'NONE', #8350, 1000.000000000000000 ) ;
#17795 = FACE_OUTER_BOUND ( 'NONE', #22051, .T. ) ;
#17796 = CARTESIAN_POINT ( 'NONE',  ( 2.706483450353418085, 10.08346604330775875, 455.0000000000000568 ) ) ;
#17797 = VERTEX_POINT ( 'NONE', #65879 ) ;
#17799 = ORIENTED_EDGE ( 'NONE', *, *, #13141, .F. ) ;
#17798 = CARTESIAN_POINT ( 'NONE',  ( 283.0000000000000568, -32.00000000000000000, 8.400000000000000355 ) ) ;
#17800 = VECTOR ( 'NONE', #65127, 1000.000000000000000 ) ;
#17801 = EDGE_CURVE ( 'NONE', #23311, #2132, #38673, .T. ) ;
#17802 = CIRCLE ( 'NONE', #3120, 0.1999999999999996503 ) ;
#17803 = CYLINDRICAL_SURFACE ( 'NONE', #17893, 2.204799999999998761 ) ;
#17804 = CARTESIAN_POINT ( 'NONE',  ( 289.9999999999998295, -0.5000000000000426326, -26.49999999999991829 ) ) ;
#17805 = LINE ( 'NONE', #1206, #52696 ) ;
#17806 = DIRECTION ( 'NONE',  ( 0.000000000000000000, -3.673940397442059868E-16, 1.000000000000000000 ) ) ;
#17807 = ORIENTED_EDGE ( 'NONE', *, *, #28893, .F. ) ;
#17808 = EDGE_CURVE ( 'NONE', #5431, #58583, #7524, .T. ) ;
#17809 = CIRCLE ( 'NONE', #39254, 0.1999999999999996503 ) ;
#17811 = CARTESIAN_POINT ( 'NONE',  ( 83.77321854994620765, 47.95351654967443977, 0.000000000000000000 ) ) ;
#17810 = AXIS2_PLACEMENT_3D ( 'NONE', #39457, #27825, #59988 ) ;
#17812 = CARTESIAN_POINT ( 'NONE',  ( 4.201500623656003519, -4.740315990920191069, 195.0000000000000284 ) ) ;
#17813 = ADVANCED_FACE ( 'NONE', ( #12471, #1520 ), #66235, .F. ) ;
#17814 = ORIENTED_EDGE ( 'NONE', *, *, #12368, .F. ) ;
#17815 = ORIENTED_EDGE ( 'NONE', *, *, #32220, .T. ) ;
#17816 = EDGE_CURVE ( 'NONE', #14532, #46696, #34741, .T. ) ;
#17817 = ORIENTED_EDGE ( 'NONE', *, *, #20728, .T. ) ;
#17818 = CARTESIAN_POINT ( 'NONE',  ( -11.75000000000000000, -5.000000000000000000, 21.10805890929250239 ) ) ;
#17819 = APPLICATION_CONTEXT ( 'automotive_design' ) ;
#17820 = ADVANCED_FACE ( 'NONE', ( #7166 ), #66576, .F. ) ;
#17821 = ADVANCED_FACE ( 'NONE', ( #29435 ), #18129, .F. ) ;
#17822 = CARTESIAN_POINT ( 'NONE',  ( -25.50000000000000355, 0.000000000000000000, 22.50000000000000000 ) ) ;
#17823 = DIRECTION ( 'NONE',  ( 0.000000000000000000, 0.000000000000000000, 1.000000000000000000 ) ) ;
#17824 = AXIS2_PLACEMENT_3D ( 'NONE', #4825, #47955, #33432 ) ;
#17825 = EDGE_CURVE ( 'NONE', #4470, #53071, #66915, .T. ) ;
#17826 = VERTEX_POINT ( 'NONE', #52420 ) ;
#17827 = VERTEX_POINT ( 'NONE', #3629 ) ;
#17828 = EDGE_LOOP ( 'NONE', ( #61613, #39626, #25049, #56110 ) ) ;
#17829 = DIRECTION ( 'NONE',  ( 0.000000000000000000, -5.800915303574361727E-12, 1.000000000000000000 ) ) ;
#17830 = ORIENTED_EDGE ( 'NONE', *, *, #17680, .F. ) ;
#17831 = ORIENTED_EDGE ( 'NONE', *, *, #65904, .F. ) ;
#17832 = ORIENTED_EDGE ( 'NONE', *, *, #47042, .F. ) ;
#17833 = VERTEX_POINT ( 'NONE', #25192 ) ;
#17834 = LINE ( 'NONE', #6542, #15854 ) ;
#17836 = VERTEX_POINT ( 'NONE', #57005 ) ;
#17835 = DIRECTION ( 'NONE',  ( 0.000000000000000000, 0.000000000000000000, -1.000000000000000000 ) ) ;
#17837 = CARTESIAN_POINT ( 'NONE',  ( 7.250000000000005329, 8.250000000000001776, -13.00000000000000178 ) ) ;
#17838 = DIRECTION ( 'NONE',  ( 1.000000000000000000, -0.000000000000000000, 0.000000000000000000 ) ) ;
#17839 = CARTESIAN_POINT ( 'NONE',  ( 7.826483450353421745, 11.99351654964657499, 455.0000000000000568 ) ) ;
#17840 = VECTOR ( 'NONE', #1777, 1000.000000000000000 ) ;
#17842 = VERTEX_POINT ( 'NONE', #41800 ) ;
#17841 = DIRECTION ( 'NONE',  ( -1.000000000000000000, 0.000000000000000000, -0.000000000000000000 ) ) ;
#17843 = DIRECTION ( 'NONE',  ( 0.000000000000000000, 0.000000000000000000, 1.000000000000000000 ) ) ;
#17844 = LINE ( 'NONE', #39063, #42450 ) ;
#17845 = DIRECTION ( 'NONE',  ( -1.000000000000000000, 0.000000000000000000, 0.000000000000000000 ) ) ;
#17846 = VERTEX_POINT ( 'NONE', #13527 ) ;
#17847 = FACE_BOUND ( 'NONE', #64816, .T. ) ;
#17848 = VECTOR ( 'NONE', #685, 1000.000000000000000 ) ;
#17849 = EDGE_CURVE ( 'NONE', #68247, #4520, #37849, .T. ) ;
#17850 = LINE ( 'NONE', #29498, #62516 ) ;
#17851 = DIRECTION ( 'NONE',  ( 0.000000000000000000, 0.000000000000000000, -1.000000000000000000 ) ) ;
#17852 = ORIENTED_EDGE ( 'NONE', *, *, #51681, .T. ) ;
#17853 = EDGE_CURVE ( 'NONE', #69858, #45036, #19527, .T. ) ;
#17854 = DIRECTION ( 'NONE',  ( 0.000000000000000000, 0.000000000000000000, -1.000000000000000000 ) ) ;
#17855 = EDGE_CURVE ( 'NONE', #2815, #24537, #51354, .T. ) ;
#17856 = CIRCLE ( 'NONE', #26915, 0.2000000000000005107 ) ;
#17857 = CARTESIAN_POINT ( 'NONE',  ( -30.00000000000000000, 0.000000000000000000, -27.00000000000000000 ) ) ;
#17858 = CARTESIAN_POINT ( 'NONE',  ( -7.250000000000000888, 7.250000000000001776, -15.00000000000000000 ) ) ;
#17859 = ADVANCED_FACE ( 'NONE', ( #51720 ), #52790, .F. ) ;
#17860 = ORIENTED_EDGE ( 'NONE', *, *, #68876, .T. ) ;
#17861 = CARTESIAN_POINT ( 'NONE',  ( 0.000000000000000000, 8.250000000000001776, -13.50000000000000178 ) ) ;
#17862 = DIRECTION ( 'NONE',  ( -1.000000000000000000, 2.135044278125299371E-15, 0.000000000000000000 ) ) ;
#17863 = SURFACE_SIDE_STYLE ('',( #18202 ) ) ;
#17864 = DIRECTION ( 'NONE',  ( 0.000000000000000000, 0.7046037717862339012, -0.7096009616570518874 ) ) ;
#17865 = AXIS2_PLACEMENT_3D ( 'NONE', #32317, #37626, #10736 ) ;
#17866 = VERTEX_POINT ( 'NONE', #2923 ) ;
#17867 = DIRECTION ( 'NONE',  ( -0.000000000000000000, 1.000000000000000000, 3.673940397442059868E-16 ) ) ;
#17868 = CARTESIAN_POINT ( 'NONE',  ( 24.00000000000000000, -16.28999999999999915, 14.50000000000000000 ) ) ;
#17869 = DIRECTION ( 'NONE',  ( 0.000000000000000000, 0.000000000000000000, 1.000000000000000000 ) ) ;
#17870 = CYLINDRICAL_SURFACE ( 'NONE', #8671, 0.3499999999999996447 ) ;
#17871 = CARTESIAN_POINT ( 'NONE',  ( 7.250000000000005329, 7.250000000000000888, -7.500000000000000000 ) ) ;
#17872 = ORIENTED_EDGE ( 'NONE', *, *, #15275, .T. ) ;
#17873 = CARTESIAN_POINT ( 'NONE',  ( 4.456444791733522252E-16, 7.450000000000002842, -24.00000000000000000 ) ) ;
#17874 = LINE ( 'NONE', #59630, #57624 ) ;
#17875 = FACE_OUTER_BOUND ( 'NONE', #25509, .T. ) ;
#17876 = DIRECTION ( 'NONE',  ( 1.000000000000000000, 0.000000000000000000, 0.000000000000000000 ) ) ;
#17877 = DIRECTION ( 'NONE',  ( 1.901462112903059913E-14, 1.000000000000000000, 1.836970198721045958E-16 ) ) ;
#17878 = ORIENTED_EDGE ( 'NONE', *, *, #4217, .T. ) ;
#17879 = VERTEX_POINT ( 'NONE', #57364 ) ;
#17880 = ADVANCED_FACE ( 'NONE', ( #36494 ), #40750, .F. ) ;
#17881 = CARTESIAN_POINT ( 'NONE',  ( 10.09643294401457858, 9.093516549646567526, 455.0000000000000568 ) ) ;
#17882 = CARTESIAN_POINT ( 'NONE',  ( 7.250000000000005329, -7.249999999999998224, -26.00000000000001066 ) ) ;
#17883 = ORIENTED_EDGE ( 'NONE', *, *, #69547, .F. ) ;
#17884 = DIRECTION ( 'NONE',  ( 0.6414496315691645689, 0.7671651518152939886, 2.309356642088551606E-17 ) ) ;
#17885 = ORIENTED_EDGE ( 'NONE', *, *, #13674, .F. ) ;
#17886 = LINE ( 'NONE', #40138, #48109 ) ;
#17887 = ORIENTED_EDGE ( 'NONE', *, *, #29698, .F. ) ;
#17888 = ORIENTED_EDGE ( 'NONE', *, *, #12007, .F. ) ;
#17889 = DIRECTION ( 'NONE',  ( 0.000000000000000000, 0.000000000000000000, 1.000000000000000000 ) ) ;
#17890 = EDGE_CURVE ( 'NONE', #6488, #54299, #19883, .T. ) ;
#17891 = EDGE_CURVE ( 'NONE', #5599, #43126, #8917, .T. ) ;
#17892 = PLANE ( 'NONE',  #56864 ) ;
#17893 = AXIS2_PLACEMENT_3D ( 'NONE', #27117, #48683, #34046 ) ;
#17894 = CYLINDRICAL_SURFACE ( 'NONE', #7780, 0.3499999999999614531 ) ;
#17895 = CARTESIAN_POINT ( 'NONE',  ( -4.141586236041125524, -5.793274621760837739, 26.00000000000000711 ) ) ;
#17896 = EDGE_CURVE ( 'NONE', #41587, #68671, #35432, .T. ) ;
#17897 = ORIENTED_EDGE ( 'NONE', *, *, #34988, .T. ) ;
#17898 = ORIENTED_EDGE ( 'NONE', *, *, #38792, .T. ) ;
#17899 = DIRECTION ( 'NONE',  ( 0.000000000000000000, 0.000000000000000000, 1.000000000000000000 ) ) ;
#17900 = CIRCLE ( 'NONE', #49557, 2.458500000000000796 ) ;
#17901 = DIRECTION ( 'NONE',  ( -1.000000000000000000, 8.540177112501197482E-15, 3.137610169492823463E-30 ) ) ;
#17902 = ORIENTED_EDGE ( 'NONE', *, *, #38579, .T. ) ;
#17903 = ORIENTED_EDGE ( 'NONE', *, *, #62111, .F. ) ;
#17904 = ORIENTED_EDGE ( 'NONE', *, *, #45486, .F. ) ;
#17905 = DIRECTION ( 'NONE',  ( 1.000000000000000000, -0.000000000000000000, -0.000000000000000000 ) ) ;
#17907 = ORIENTED_EDGE ( 'NONE', *, *, #42443, .F. ) ;
#17906 = CARTESIAN_POINT ( 'NONE',  ( 11.12648345035337982, -4.206483450353396769, 195.0000000000000284 ) ) ;
#17908 = AXIS2_PLACEMENT_3D ( 'NONE', #37278, #69800, #21357 ) ;
#17909 = DIRECTION ( 'NONE',  ( -1.000000000000000000, 0.000000000000000000, 0.000000000000000000 ) ) ;
#17910 = LINE ( 'NONE', #61032, #140 ) ;
#17911 = ORIENTED_EDGE ( 'NONE', *, *, #15540, .F. ) ;
#17912 = VERTEX_POINT ( 'NONE', #20232 ) ;
#17913 = LINE ( 'NONE', #24631, #23604 ) ;
#17914 = DIRECTION ( 'NONE',  ( -0.7071067811865486830, -0.7071067811865464625, -2.597868168706476160E-16 ) ) ;
#17915 = DIRECTION ( 'NONE',  ( -9.799566706031580591E-15, -1.000000000000000000, 0.000000000000000000 ) ) ;
#17916 = FACE_OUTER_BOUND ( 'NONE', #35326, .T. ) ;
#17917 = CYLINDRICAL_SURFACE ( 'NONE', #13246, 0.2000000000000005107 ) ;
#17919 = ORIENTED_EDGE ( 'NONE', *, *, #50701, .T. ) ;
#17918 = CARTESIAN_POINT ( 'NONE',  ( -4.188533722949421723, -7.272650909786664286, 455.0000000000000568 ) ) ;
#17920 = ORIENTED_EDGE ( 'NONE', *, *, #3145, .T. ) ;
#17921 = EDGE_CURVE ( 'NONE', #57822, #64699, #14579, .T. ) ;
#17922 = LINE ( 'NONE', #49435, #37719 ) ;
#17923 = EDGE_CURVE ( 'NONE', #31847, #59233, #27697, .T. ) ;
#17924 = CARTESIAN_POINT ( 'NONE',  ( 8.930623737882818602, -10.05377373788282469, 54.00000000000000711 ) ) ;
#17925 = DIRECTION ( 'NONE',  ( -0.000000000000000000, -1.000000000000000000, -0.000000000000000000 ) ) ;
#17926 = CARTESIAN_POINT ( 'NONE',  ( -16.75000000000000000, -0.2038245569916330158, 21.77831216351300014 ) ) ;
#17927 = EDGE_CURVE ( 'NONE', #31474, #15026, #9633, .T. ) ;
#17928 = AXIS2_PLACEMENT_3D ( 'NONE', #30955, #42255, #15397 ) ;
#17929 = CARTESIAN_POINT ( 'NONE',  ( 289.7500000000000000, -0.2500000000000106581, -26.74999999999999645 ) ) ;
#17930 = ORIENTED_EDGE ( 'NONE', *, *, #58569, .F. ) ;
#17931 = DIRECTION ( 'NONE',  ( 0.000000000000000000, 0.000000000000000000, 1.000000000000000000 ) ) ;
#17932 = PLANE ( 'NONE',  #54219 ) ;
#17933 = FILL_AREA_STYLE ('',( #55097 ) ) ;
#17934 = AXIS2_PLACEMENT_3D ( 'NONE', #53837, #87, #63741 ) ;
#17935 = CARTESIAN_POINT ( 'NONE',  ( 9.929523737882751888, 0.9414762621171479662, 54.00000000000000711 ) ) ;
#17936 = FACE_BOUND ( 'NONE', #29030, .T. ) ;
#17937 = DIRECTION ( 'NONE',  ( 1.000000000000000000, -1.047444401652940007E-14, 1.836970198721010706E-16 ) ) ;
#17938 = VECTOR ( 'NONE', #54921, 1000.000000000000000 ) ;
#17939 = DIRECTION ( 'NONE',  ( 1.000000000000000000, 0.000000000000000000, 0.000000000000000000 ) ) ;
#17940 = VERTEX_POINT ( 'NONE', #19184 ) ;
#17941 = FACE_OUTER_BOUND ( 'NONE', #41223, .T. ) ;
#17942 = FACE_OUTER_BOUND ( 'NONE', #26878, .T. ) ;
#17943 = VERTEX_POINT ( 'NONE', #24842 ) ;
#17944 = LINE ( 'NONE', #12627, #57191 ) ;
#17945 = CARTESIAN_POINT ( 'NONE',  ( -7.250000000000001776, -7.249999999999998224, -22.50000000000000000 ) ) ;
#17946 = VECTOR ( 'NONE', #34167, 1000.000000000000000 ) ;
#17947 = CARTESIAN_POINT ( 'NONE',  ( 11.08848345035334404, -10.20488345035352928, 455.0000000000000568 ) ) ;
#17948 = EDGE_CURVE ( 'NONE', #59852, #34424, #61583, .T. ) ;
#17949 = DIRECTION ( 'NONE',  ( -0.000000000000000000, -0.000000000000000000, 1.000000000000000000 ) ) ;
#17950 = PLANE ( 'NONE',  #56458 ) ;
#17951 = ORIENTED_EDGE ( 'NONE', *, *, #42870, .F. ) ;
#17953 = CIRCLE ( 'NONE', #57487, 0.7112000000000124889 ) ;
#17952 = AXIS2_PLACEMENT_3D ( 'NONE', #52214, #3777, #20045 ) ;
#17954 = LINE ( 'NONE', #38502, #15097 ) ;
#17955 = EDGE_LOOP ( 'NONE', ( #45350, #48731, #26799, #68399 ) ) ;
#17956 = DIRECTION ( 'NONE',  ( 1.000000000000000000, -0.000000000000000000, -0.000000000000000000 ) ) ;
#17957 = ORIENTED_EDGE ( 'NONE', *, *, #63946, .F. ) ;
#17958 = DIRECTION ( 'NONE',  ( -1.000000000000000000, 0.000000000000000000, 0.000000000000000000 ) ) ;
#17959 = CIRCLE ( 'NONE', #13426, 3.999999999999993339 ) ;
#17960 = CARTESIAN_POINT ( 'NONE',  ( 5.393625297349901260, -4.747751991980658559, 195.0000000000000284 ) ) ;
#17961 = ORIENTED_EDGE ( 'NONE', *, *, #46835, .T. ) ;
#17962 = ORIENTED_EDGE ( 'NONE', *, *, #31515, .T. ) ;
#17963 = CARTESIAN_POINT ( 'NONE',  ( 7.450000000000006395, 7.250000000000000888, -18.50000000000000000 ) ) ;
#17964 = ORIENTED_EDGE ( 'NONE', *, *, #61710, .F. ) ;
#17965 = ORIENTED_EDGE ( 'NONE', *, *, #13885, .F. ) ;
#17966 = ADVANCED_FACE ( 'NONE', ( #31218 ), #56663, .T. ) ;
#17967 = DIRECTION ( 'NONE',  ( 0.000000000000000000, 0.000000000000000000, -1.000000000000000000 ) ) ;
#17968 = DIRECTION ( 'NONE',  ( 0.000000000000000000, -1.000000000000000000, 0.000000000000000000 ) ) ;
#17969 = CARTESIAN_POINT ( 'NONE',  ( 7.826483450353380000, -11.78648345035349010, 455.0000000000000568 ) ) ;
#17970 = EDGE_CURVE ( 'NONE', #35311, #43920, #4346, .T. ) ;
#17971 = EDGE_CURVE ( 'NONE', #51926, #62351, #8501, .T. ) ;
#17972 = VERTEX_POINT ( 'NONE', #25554 ) ;
#17973 = FACE_OUTER_BOUND ( 'NONE', #11227, .T. ) ;
#17975 = FACE_OUTER_BOUND ( 'NONE', #2196, .T. ) ;
#17974 = PLANE ( 'NONE',  #32176 ) ;
#17976 = EDGE_LOOP ( 'NONE', ( #9993, #35905, #61168, #5704 ) ) ;
#17979 = VERTEX_POINT ( 'NONE', #1030 ) ;
#17978 = EDGE_CURVE ( 'NONE', #23956, #65820, #47116, .T. ) ;
#17977 = DIRECTION ( 'NONE',  ( -1.836970198721029934E-16, 1.836970198721036344E-16, -1.000000000000000000 ) ) ;
#17980 = VERTEX_POINT ( 'NONE', #6324 ) ;
#17981 = VECTOR ( 'NONE', #27968, 1000.000000000000000 ) ;
#17982 = EDGE_CURVE ( 'NONE', #58549, #5389, #63891, .T. ) ;
#17983 = EDGE_CURVE ( 'NONE', #34294, #42050, #55115, .T. ) ;
#17984 = DIRECTION ( 'NONE',  ( -0.7071067811865480168, 0.000000000000000000, 0.7071067811865470176 ) ) ;
#17985 = AXIS2_PLACEMENT_3D ( 'NONE', #32072, #57885, #52601 ) ;
#17986 = ADVANCED_FACE ( 'NONE', ( #48768 ), #329, .F. ) ;
#17987 = AXIS2_PLACEMENT_3D ( 'NONE', #44488, #57204, #14060 ) ;
#17988 = ORIENTED_EDGE ( 'NONE', *, *, #63786, .T. ) ;
#17989 = DIRECTION ( 'NONE',  ( -1.836970198721029934E-16, 1.836970198721036590E-16, -1.000000000000000000 ) ) ;
#17990 = DIRECTION ( 'NONE',  ( 1.000000000000000000, -0.000000000000000000, -0.000000000000000000 ) ) ;
#17991 = VERTEX_POINT ( 'NONE', #28227 ) ;
#17992 = ORIENTED_EDGE ( 'NONE', *, *, #62195, .F. ) ;
#17993 = DIRECTION ( 'NONE',  ( 0.000000000000000000, 1.000000000000000000, 0.000000000000000000 ) ) ;
#17994 = CARTESIAN_POINT ( 'NONE',  ( -10.49297626211726175, 3.650476262117184234, 26.00000000000000711 ) ) ;
#17995 = ORIENTED_EDGE ( 'NONE', *, *, #6722, .F. ) ;
#17996 = CIRCLE ( 'NONE', #42848, 0.3999999999999993006 ) ;
#17997 = LINE ( 'NONE', #65078, #53430 ) ;
#17998 = CARTESIAN_POINT ( 'NONE',  ( 0.000000000000000000, 0.000000000000000000, -19.50000000000000000 ) ) ;
#17999 = CARTESIAN_POINT ( 'NONE',  ( 289.7500000000000000, -42.25000000000000000, 26.75000000000000000 ) ) ;
#18000 = ORIENTED_EDGE ( 'NONE', *, *, #34549, .T. ) ;
#18001 = CIRCLE ( 'NONE', #28160, 1.000000000000000000 ) ;
#18002 = DIRECTION ( 'NONE',  ( 0.000000000000000000, 1.000000000000000000, 0.000000000000000000 ) ) ;
#18003 = CARTESIAN_POINT ( 'NONE',  ( 7.000000000000000000, -25.50000000000000355, -16.03137303340311348 ) ) ;
#18005 = ORIENTED_EDGE ( 'NONE', *, *, #55227, .F. ) ;
#18004 = CARTESIAN_POINT ( 'NONE',  ( -6.500000000000002665, -6.500000000000002665, -1.000000000000000000 ) ) ;
#18007 = ORIENTED_EDGE ( 'NONE', *, *, #10475, .T. ) ;
#18006 = CARTESIAN_POINT ( 'NONE',  ( -4.383466043307920224, -8.406483450353396947, 195.0000000000000284 ) ) ;
#18008 = LINE ( 'NONE', #49166, #53963 ) ;
#18009 = AXIS2_PLACEMENT_3D ( 'NONE', #39403, #17845, #2279 ) ;
#18010 = DIRECTION ( 'NONE',  ( 0.000000000000000000, 1.000000000000000000, 0.000000000000000000 ) ) ;
#18011 = DIRECTION ( 'NONE',  ( -0.7142857142857395036, 0.000000000000000000, -0.6998542122237394469 ) ) ;
#18012 = DIRECTION ( 'NONE',  ( -0.7071067811865446862, -0.7071067811865503483, 0.000000000000000000 ) ) ;
#18013 = LINE ( 'NONE', #30026, #12698 ) ;
#18014 = ORIENTED_EDGE ( 'NONE', *, *, #11518, .F. ) ;
#18015 = CARTESIAN_POINT ( 'NONE',  ( 0.9555237378827827754, -9.929523737882782086, 26.00000000000000000 ) ) ;
#18016 = DIRECTION ( 'NONE',  ( -1.000000000000000000, 0.000000000000000000, 0.000000000000000000 ) ) ;
#18017 = DIRECTION ( 'NONE',  ( -1.836970198721029934E-16, 1.836970198721036344E-16, -1.000000000000000000 ) ) ;
#18019 = ORIENTED_EDGE ( 'NONE', *, *, #16883, .T. ) ;
#18018 = CARTESIAN_POINT ( 'NONE',  ( -9.722976262117237312, 7.605476262117214503, 25.99999580000000421 ) ) ;
#18020 = CARTESIAN_POINT ( 'NONE',  ( 49.00000000000000000, -21.00000000000000000, 13.86939075806900057 ) ) ;
#18021 = AXIS2_PLACEMENT_3D ( 'NONE', #21241, #4288, #47399 ) ;
#18022 = DIRECTION ( 'NONE',  ( 1.000000000000000000, -0.000000000000000000, -0.000000000000000000 ) ) ;
#18023 = EDGE_CURVE ( 'NONE', #56320, #27398, #54764, .T. ) ;
#18024 = EDGE_LOOP ( 'NONE', ( #35344, #43830, #19210, #19702 ) ) ;
#18025 = DIRECTION ( 'NONE',  ( -1.000000000000000000, 0.000000000000000000, 0.000000000000000000 ) ) ;
#18026 = CARTESIAN_POINT ( 'NONE',  ( -11.50000000000000000, -12.00000000000000000, 11.00000000000000000 ) ) ;
#18027 = EDGE_LOOP ( 'NONE', ( #43758, #28251, #39680, #956 ) ) ;
#18028 = DIRECTION ( 'NONE',  ( 1.000000000000000000, -0.000000000000000000, 0.000000000000000000 ) ) ;
#18029 = LINE ( 'NONE', #29333, #50410 ) ;
#18030 = FACE_BOUND ( 'NONE', #20599, .T. ) ;
#18031 = EDGE_CURVE ( 'NONE', #66711, #55626, #15289, .T. ) ;
#18032 = DIRECTION ( 'NONE',  ( 0.000000000000000000, 0.000000000000000000, -1.000000000000000000 ) ) ;
#18033 = CIRCLE ( 'NONE', #50786, 1.500000000000850875 ) ;
#18034 = VECTOR ( 'NONE', #7355, 1000.000000000000000 ) ;
#18035 = DIRECTION ( 'NONE',  ( 0.000000000000000000, 1.000000000000000000, 3.673940397442059868E-16 ) ) ;
#18036 = VECTOR ( 'NONE', #25005, 1000.000000000000000 ) ;
#18037 = VERTEX_POINT ( 'NONE', #20581 ) ;
#18038 = DIRECTION ( 'NONE',  ( -0.6414496315691617934, -0.7671651518152962090, 0.000000000000000000 ) ) ;
#18039 = ORIENTED_EDGE ( 'NONE', *, *, #20460, .T. ) ;
#18040 = EDGE_CURVE ( 'NONE', #8437, #68001, #21888, .T. ) ;
#18041 = ORIENTED_EDGE ( 'NONE', *, *, #24197, .T. ) ;
#18042 = AXIS2_PLACEMENT_3D ( 'NONE', #48396, #37442, #47345 ) ;
#18043 = CARTESIAN_POINT ( 'NONE',  ( -16.75000000000000000, -2.500000000000000000, -23.22168783648699986 ) ) ;
#18044 = EDGE_CURVE ( 'NONE', #26989, #46007, #17615, .T. ) ;
#18045 = CIRCLE ( 'NONE', #42903, 1.000000000000000000 ) ;
#18046 = PLANE ( 'NONE',  #47952 ) ;
#18047 = DIRECTION ( 'NONE',  ( 0.000000000000000000, 0.000000000000000000, -1.000000000000000000 ) ) ;
#18048 = ORIENTED_EDGE ( 'NONE', *, *, #37514, .T. ) ;
#18049 = ORIENTED_EDGE ( 'NONE', *, *, #21872, .F. ) ;
#18050 = CIRCLE ( 'NONE', #27109, 4.000000000000000888 ) ;
#18051 = CARTESIAN_POINT ( 'NONE',  ( -11.50000000000000000, -15.46862696659690073, 14.50000000000000000 ) ) ;
#18052 = ORIENTED_EDGE ( 'NONE', *, *, #56447, .F. ) ;
#18053 = VECTOR ( 'NONE', #7856, 1000.000000000000000 ) ;
#18054 = DIRECTION ( 'NONE',  ( 0.000000000000000000, 0.7071067811865495711, 0.7071067811865455743 ) ) ;
#18055 = CARTESIAN_POINT ( 'NONE',  ( 275.0000000000000000, -42.00000000000000000, 7.000000000000000000 ) ) ;
#18056 = ADVANCED_FACE ( 'NONE', ( #65036 ), #6996, .T. ) ;
#18057 = DIRECTION ( 'NONE',  ( 0.000000000000000000, -1.000000000000000000, 0.000000000000000000 ) ) ;
#18058 = DIRECTION ( 'NONE',  ( -1.000000000000000000, -0.000000000000000000, -0.000000000000000000 ) ) ;
#18059 = VECTOR ( 'NONE', #44615, 1000.000000000000000 ) ;
#18060 = AXIS2_PLACEMENT_3D ( 'NONE', #51476, #13639, #55736 ) ;
#18062 = LINE ( 'NONE', #49228, #69615 ) ;
#18061 = CARTESIAN_POINT ( 'NONE',  ( 283.0000000000000568, -30.45000000000094786, 14.49999999999906031 ) ) ;
#18063 = VERTEX_POINT ( 'NONE', #38171 ) ;
#18065 = VERTEX_POINT ( 'NONE', #9990 ) ;
#18064 = DIRECTION ( 'NONE',  ( -1.000000000000000000, 0.000000000000000000, -0.000000000000000000 ) ) ;
#18066 = ORIENTED_EDGE ( 'NONE', *, *, #32679, .F. ) ;
#18067 = VERTEX_POINT ( 'NONE', #16597 ) ;
#18068 = EDGE_CURVE ( 'NONE', #11057, #17477, #30004, .T. ) ;
#18069 = DIRECTION ( 'NONE',  ( 0.000000000000000000, 0.000000000000000000, 1.000000000000000000 ) ) ;
#18070 = EDGE_CURVE ( 'NONE', #8587, #34946, #63732, .T. ) ;
#18071 = DIRECTION ( 'NONE',  ( 0.000000000000000000, 0.000000000000000000, 1.000000000000000000 ) ) ;
#18072 = CARTESIAN_POINT ( 'NONE',  ( 10.70000000000000107, -20.40000000000000213, -17.60000000000000142 ) ) ;
#18073 = VERTEX_POINT ( 'NONE', #49109 ) ;
#18074 = ORIENTED_EDGE ( 'NONE', *, *, #65103, .F. ) ;
#18075 = CARTESIAN_POINT ( 'NONE',  ( 7.000000000000000000, -21.00000000000000000, 0.000000000000000000 ) ) ;
#18076 = CARTESIAN_POINT ( 'NONE',  ( 7.450000000000004619, -1.336933437520057563E-15, -17.50000000000000000 ) ) ;
#18077 = ORIENTED_EDGE ( 'NONE', *, *, #15511, .F. ) ;
#18078 = VERTEX_POINT ( 'NONE', #681 ) ;
#18079 = DIRECTION ( 'NONE',  ( -5.981805089575196197E-17, -1.000000000000000000, 0.000000000000000000 ) ) ;
#18080 = FACE_OUTER_BOUND ( 'NONE', #22361, .T. ) ;
#18081 = VECTOR ( 'NONE', #61207, 1000.000000000000000 ) ;
#18082 = ORIENTED_EDGE ( 'NONE', *, *, #8478, .T. ) ;
#18083 = CONICAL_SURFACE ( 'NONE', #50841, 2.000000000000001776, 0.7853981633974503884 ) ;
#18084 = DIRECTION ( 'NONE',  ( -1.000000000000000000, 0.000000000000000000, 0.000000000000000000 ) ) ;
#18086 = ORIENTED_EDGE ( 'NONE', *, *, #33156, .T. ) ;
#18085 =( NAMED_UNIT ( * ) SI_UNIT ( $, .STERADIAN. ) SOLID_ANGLE_UNIT ( ) );
#18087 = ORIENTED_EDGE ( 'NONE', *, *, #45756, .T. ) ;
#18088 = VECTOR ( 'NONE', #32049, 1000.000000000000000 ) ;
#18089 = LINE ( 'NONE', #60539, #5173 ) ;
#18090 = CARTESIAN_POINT ( 'NONE',  ( 283.0000000000000568, -23.70411739045900390, -12.50000000000000000 ) ) ;
#18091 = CARTESIAN_POINT ( 'NONE',  ( -7.250000000000000000, -8.749999999999998224, -26.00000000000001066 ) ) ;
#18092 = LINE ( 'NONE', #23059, #29244 ) ;
#18093 = LINE ( 'NONE', #39660, #35775 ) ;
#18094 = VECTOR ( 'NONE', #19688, 1000.000000000000000 ) ;
#18095 = ADVANCED_FACE ( 'NONE', ( #16934 ), #32240, .T. ) ;
#18096 = CARTESIAN_POINT ( 'NONE',  ( -7.450000000000001954, -7.249999999999998224, -13.50000000000000178 ) ) ;
#18098 = AXIS2_PLACEMENT_3D ( 'NONE', #5433, #58816, #37944 ) ;
#18097 = LINE ( 'NONE', #55940, #51850 ) ;
#18099 = ORIENTED_EDGE ( 'NONE', *, *, #18323, .F. ) ;
#18100 = DIRECTION ( 'NONE',  ( 0.7071067811865527908, 0.7071067811865422437, 2.597868168706460875E-16 ) ) ;
#18101 = ADVANCED_FACE ( 'NONE', ( #22924 ), #54426, .T. ) ;
#18103 = ORIENTED_EDGE ( 'NONE', *, *, #66920, .T. ) ;
#18102 = DIRECTION ( 'NONE',  ( -0.000000000000000000, 1.000000000000000000, -0.000000000000000000 ) ) ;
#18104 = CARTESIAN_POINT ( 'NONE',  ( -7.394232575409651176, -6.789561617636906909, 54.00000000000000711 ) ) ;
#18105 = CARTESIAN_POINT ( 'NONE',  ( 5.793274621760843957, -6.358413763958971288, 26.00000000000000711 ) ) ;
#18107 = EDGE_CURVE ( 'NONE', #26426, #57275, #33870, .T. ) ;
#18106 = DIRECTION ( 'NONE',  ( -1.000000000000000000, 2.602085213965213008E-15, 0.000000000000000000 ) ) ;
#18108 = CARTESIAN_POINT ( 'NONE',  ( -1.620245201994301665, 8.227189898828640935, 26.00000000000000711 ) ) ;
#18109 = VECTOR ( 'NONE', #45663, 1000.000000000000000 ) ;
#18110 = AXIS2_PLACEMENT_3D ( 'NONE', #59581, #38361, #11130 ) ;
#18111 = LINE ( 'NONE', #6808, #59714 ) ;
#18112 = EDGE_CURVE ( 'NONE', #25346, #2156, #39185, .T. ) ;
#18113 = ORIENTED_EDGE ( 'NONE', *, *, #23779, .F. ) ;
#18114 = ORIENTED_EDGE ( 'NONE', *, *, #61325, .T. ) ;
#18115 = CYLINDRICAL_SURFACE ( 'NONE', #913, 5.000000000000004441 ) ;
#18116 = EDGE_CURVE ( 'NONE', #67984, #2683, #10781, .T. ) ;
#18117 = FILL_AREA_STYLE ('',( #44293 ) ) ;
#18118 = DIRECTION ( 'NONE',  ( -1.000000000000000000, 0.000000000000000000, -0.000000000000000000 ) ) ;
#18119 = ORIENTED_EDGE ( 'NONE', *, *, #17444, .T. ) ;
#18120 = AXIS2_PLACEMENT_3D ( 'NONE', #59839, #5426, #26981 ) ;
#18121 = CARTESIAN_POINT ( 'NONE',  ( 7.250000000000005329, -7.249999999999998224, -26.00000000000001066 ) ) ;
#18122 = ORIENTED_EDGE ( 'NONE', *, *, #52638, .T. ) ;
#18123 = EDGE_CURVE ( 'NONE', #16599, #5747, #69024, .T. ) ;
#18124 = ORIENTED_EDGE ( 'NONE', *, *, #33711, .F. ) ;
#18125 = EDGE_CURVE ( 'NONE', #49745, #51892, #50137, .T. ) ;
#18126 = DIRECTION ( 'NONE',  ( 0.000000000000000000, 0.000000000000000000, 1.000000000000000000 ) ) ;
#18127 = CARTESIAN_POINT ( 'NONE',  ( 0.7669999999999959073, 0.000000000000000000, -3.999999999999977351 ) ) ;
#18128 = EDGE_LOOP ( 'NONE', ( #67181, #42851, #66485, #36685 ) ) ;
#18129 = PLANE ( 'NONE',  #28783 ) ;
#18130 = ADVANCED_FACE ( 'NONE', ( #44823 ), #34204, .T. ) ;
#18131 = EDGE_CURVE ( 'NONE', #52921, #51395, #23188, .T. ) ;
#18132 = DIRECTION ( 'NONE',  ( -1.000000000000000000, 0.000000000000000000, 0.000000000000000000 ) ) ;
#18133 = CARTESIAN_POINT ( 'NONE',  ( -7.250000000000001776, -7.249999999999998224, -19.50000000000000000 ) ) ;
#18134 = VERTEX_POINT ( 'NONE', #12638 ) ;
#18135 = AXIS2_PLACEMENT_3D ( 'NONE', #36015, #30719, #57584 ) ;
#18137 = ORIENTED_EDGE ( 'NONE', *, *, #2230, .T. ) ;
#18136 = LINE ( 'NONE', #17798, #66707 ) ;
#18138 = EDGE_CURVE ( 'NONE', #20091, #36899, #13356, .T. ) ;
#18139 = VECTOR ( 'NONE', #26909, 1000.000000000000000 ) ;
#18140 = DIRECTION ( 'NONE',  ( 0.000000000000000000, 0.000000000000000000, 1.000000000000000000 ) ) ;
#18141 = DIRECTION ( 'NONE',  ( 1.000000000000000000, 0.000000000000000000, 0.000000000000000000 ) ) ;
#18142 = CARTESIAN_POINT ( 'NONE',  ( -7.517976262117252340, -3.848229544836285321, 54.00000000000000711 ) ) ;
#18143 = CARTESIAN_POINT ( 'NONE',  ( -5.993516549646711766, 5.993516549646603409, 195.0000000000000284 ) ) ;
#18144 = CIRCLE ( 'NONE', #68989, 7.799999999999999822 ) ;
#18145 = CARTESIAN_POINT ( 'NONE',  ( 277.1811023147819810, -20.65270074880750073, 17.15270074880750784 ) ) ;
#18146 = LINE ( 'NONE', #66931, #69142 ) ;
#18147 = ORIENTED_EDGE ( 'NONE', *, *, #37622, .T. ) ;
#18148 = ORIENTED_EDGE ( 'NONE', *, *, #6154, .F. ) ;
#18149 = VECTOR ( 'NONE', #50047, 1000.000000000000000 ) ;
#18150 = VECTOR ( 'NONE', #23278, 1000.000000000000000 ) ;
#18151 = VERTEX_POINT ( 'NONE', #62475 ) ;
#18152 = DIRECTION ( 'NONE',  ( 1.000000000000000000, -0.000000000000000000, 0.000000000000000000 ) ) ;
#18153 = EDGE_CURVE ( 'NONE', #4089, #29817, #55792, .T. ) ;
#18154 = CARTESIAN_POINT ( 'NONE',  ( 283.0000000000000568, -28.95000000000155183, -14.49999999999845990 ) ) ;
#18155 = AXIS2_PLACEMENT_3D ( 'NONE', #39017, #37647, #43640 ) ;
#18156 = CARTESIAN_POINT ( 'NONE',  ( -10.49297626211726175, 3.650476262117184234, 54.00000000000000711 ) ) ;
#18158 = EDGE_CURVE ( 'NONE', #51358, #31939, #56831, .T. ) ;
#18157 =( LENGTH_UNIT ( ) NAMED_UNIT ( * ) SI_UNIT ( .MILLI., .METRE. ) );
#18159 = ORIENTED_EDGE ( 'NONE', *, *, #14066, .F. ) ;
#18160 = VERTEX_POINT ( 'NONE', #29607 ) ;
#18161 = EDGE_LOOP ( 'NONE', ( #36473, #55317 ) ) ;
#18163 = CARTESIAN_POINT ( 'NONE',  ( -7.250000000000000888, 7.250000000000001776, -16.00000000000000000 ) ) ;
#18162 = AXIS2_PLACEMENT_3D ( 'NONE', #65685, #27514, #16568 ) ;
#18164 = EDGE_LOOP ( 'NONE', ( #35112, #11779, #31225, #43629 ) ) ;
#18165 = ORIENTED_EDGE ( 'NONE', *, *, #23247, .F. ) ;
#18166 = ORIENTED_EDGE ( 'NONE', *, *, #20103, .T. ) ;
#18167 = ORIENTED_EDGE ( 'NONE', *, *, #38239, .T. ) ;
#18168 = CYLINDRICAL_SURFACE ( 'NONE', #17, 0.2000000000000005107 ) ;
#18170 = ORIENTED_EDGE ( 'NONE', *, *, #16194, .T. ) ;
#18169 = DIRECTION ( 'NONE',  ( 1.000000000000000000, -0.000000000000000000, 0.000000000000000000 ) ) ;
#18171 = FACE_OUTER_BOUND ( 'NONE', #22506, .T. ) ;
#18172 = CARTESIAN_POINT ( 'NONE',  ( -9.689999999999999503, -10.50000000000000178, -4.250000000000000000 ) ) ;
#18173 = VECTOR ( 'NONE', #54715, 1000.000000000000000 ) ;
#18174 = CARTESIAN_POINT ( 'NONE',  ( 289.5000000000000000, -0.5000000000000000000, -27.00000000000000000 ) ) ;
#18176 = ORIENTED_EDGE ( 'NONE', *, *, #64061, .F. ) ;
#18175 = CARTESIAN_POINT ( 'NONE',  ( -1.677516549646826061, -10.74648345035347141, 455.0000000000000568 ) ) ;
#18177 = ORIENTED_EDGE ( 'NONE', *, *, #51394, .F. ) ;
#18178 = CARTESIAN_POINT ( 'NONE',  ( 0.000000000000000000, 8.250000000000001776, -20.00000000000000000 ) ) ;
#18179 = CARTESIAN_POINT ( 'NONE',  ( -7.250000000000000888, -8.249999999999998224, -26.00000000000001066 ) ) ;
#18180 = CARTESIAN_POINT ( 'NONE',  ( 6.832023737882818359, -9.737023737882822161, 54.00000000000000711 ) ) ;
#18181 = VECTOR ( 'NONE', #58121, 1000.000000000000000 ) ;
#18182 = ORIENTED_EDGE ( 'NONE', *, *, #28102, .T. ) ;
#18183 = DIRECTION ( 'NONE',  ( 0.000000000000000000, 0.000000000000000000, 1.000000000000000000 ) ) ;
#18184 = ADVANCED_FACE ( 'NONE', ( #18650 ), #35610, .F. ) ;
#18185 = FACE_OUTER_BOUND ( 'NONE', #20713, .T. ) ;
#18186 = COLOUR_RGB ( '', 0.08235294, 0.09019608, 0.10196078) ;
#18187 = DIRECTION ( 'NONE',  ( 0.000000000000000000, 0.000000000000000000, 1.000000000000000000 ) ) ;
#18188 = ORIENTED_EDGE ( 'NONE', *, *, #58314, .T. ) ;
#18191 = EDGE_CURVE ( 'NONE', #45736, #38019, #37904, .T. ) ;
#18190 = CARTESIAN_POINT ( 'NONE',  ( 25.57999999999999829, 0.000000000000000000, 0.000000000000000000 ) ) ;
#18189 = AXIS2_PLACEMENT_3D ( 'NONE', #69541, #26762, #43008 ) ;
#18192 = CARTESIAN_POINT ( 'NONE',  ( 3.664523737882815269, 10.49297626211721024, 26.00000000000000711 ) ) ;
#18193 = CARTESIAN_POINT ( 'NONE',  ( -1.466476262117323737, -9.404523737882843903, 54.00000000000000711 ) ) ;
#18194 = EDGE_CURVE ( 'NONE', #35617, #57481, #40919, .T. ) ;
#18195 = EDGE_CURVE ( 'NONE', #7564, #4698, #8034, .T. ) ;
#18196 = VECTOR ( 'NONE', #52423, 1000.000000000000000 ) ;
#18197 = VECTOR ( 'NONE', #45101, 1000.000000000000000 ) ;
#18198 = ORIENTED_EDGE ( 'NONE', *, *, #20613, .T. ) ;
#18199 = CARTESIAN_POINT ( 'NONE',  ( 41.09999999999999432, 20.60000000000000142, -13.86939075806900057 ) ) ;
#18200 = EDGE_CURVE ( 'NONE', #44308, #46469, #58234, .T. ) ;
#18201 = EDGE_CURVE ( 'NONE', #22677, #2326, #39521, .T. ) ;
#18202 = SURFACE_STYLE_FILL_AREA ( #33772 ) ;
#18203 = CIRCLE ( 'NONE', #62268, 0.1749999999999980738 ) ;
#18204 = CARTESIAN_POINT ( 'NONE',  ( -7.450000000000001954, 0.000000000000000000, -9.000000000000001776 ) ) ;
#18205 = ORIENTED_EDGE ( 'NONE', *, *, #22531, .T. ) ;
#18206 = DIRECTION ( 'NONE',  ( 1.000000000000000000, -0.000000000000000000, 0.000000000000000000 ) ) ;
#18207 = DIRECTION ( 'NONE',  ( 0.000000000000000000, 0.000000000000000000, -1.000000000000000000 ) ) ;
#18208 = CARTESIAN_POINT ( 'NONE',  ( -9.722976262117237312, 7.605476262117214503, 54.00000000000000711 ) ) ;
#18209 = VECTOR ( 'NONE', #12448, 1000.000000000000000 ) ;
#18210 = LINE ( 'NONE', #33443, #9799 ) ;
#18211 = LINE ( 'NONE', #39768, #56744 ) ;
#18212 = ORIENTED_EDGE ( 'NONE', *, *, #4899, .F. ) ;
#18213 = CARTESIAN_POINT ( 'NONE',  ( 7.250000000000005329, -7.449999999999998401, -22.50000000000000000 ) ) ;
#18214 = DIRECTION ( 'NONE',  ( -1.000000000000000000, 0.000000000000000000, 0.000000000000000000 ) ) ;
#18215 = CARTESIAN_POINT ( 'NONE',  ( 10.05377373788278739, -9.703773737882814387, 26.00000000000000000 ) ) ;
#18216 = DIRECTION ( 'NONE',  ( -0.8660254037844485886, 0.000000000000000000, -0.4999999999999827360 ) ) ;
#18217 = DIRECTION ( 'NONE',  ( 0.000000000000000000, 0.000000000000000000, 1.000000000000000000 ) ) ;
#18218 = EDGE_LOOP ( 'NONE', ( #39993, #44209, #29458, #43362 ) ) ;
#18220 = ORIENTED_EDGE ( 'NONE', *, *, #68443, .F. ) ;
#18219 = PLANE ( 'NONE',  #4752 ) ;
#18221 = CARTESIAN_POINT ( 'NONE',  ( -10.73351654964671198, 1.077516549646603483, 195.0000000000000284 ) ) ;
#18222 = VECTOR ( 'NONE', #35558, 1000.000000000000000 ) ;
#18223 = CARTESIAN_POINT ( 'NONE',  ( -11.50000000000000000, -15.97213595500069871, -14.50000000000000000 ) ) ;
#18224 = ORIENTED_EDGE ( 'NONE', *, *, #6431, .T. ) ;
#18225 = DIRECTION ( 'NONE',  ( -0.000000000000000000, -1.000000000000000000, -0.000000000000000000 ) ) ;
#18226 = ORIENTED_EDGE ( 'NONE', *, *, #15273, .F. ) ;
#18227 = FACE_OUTER_BOUND ( 'NONE', #19835, .T. ) ;
#18228 = ORIENTED_EDGE ( 'NONE', *, *, #332, .T. ) ;
#18229 = EDGE_LOOP ( 'NONE', ( #24883, #39404, #47727, #4340 ) ) ;
#18230 = DIRECTION ( 'NONE',  ( 1.000000000000000000, -5.120954910632640039E-15, 0.000000000000000000 ) ) ;
#18231 = AXIS2_PLACEMENT_3D ( 'NONE', #59079, #49169, #21264 ) ;
#18232 = CARTESIAN_POINT ( 'NONE',  ( -7.603567055985634759, -8.406483450353409381, 455.0000000000000568 ) ) ;
#18233 = DIRECTION ( 'NONE',  ( -0.000000000000000000, -0.000000000000000000, -1.000000000000000000 ) ) ;
#18235 = EDGE_CURVE ( 'NONE', #44371, #30033, #66743, .T. ) ;
#18234 = DIRECTION ( 'NONE',  ( 0.000000000000000000, 0.000000000000000000, 1.000000000000000000 ) ) ;
#18236 = MECHANICAL_DESIGN_GEOMETRIC_PRESENTATION_REPRESENTATION (  '', ( #43086 ), #52124 ) ;
#18237 = VERTEX_POINT ( 'NONE', #45880 ) ;
#18239 = ADVANCED_FACE ( 'NONE', ( #7692 ), #40220, .T. ) ;
#18238 = VERTEX_POINT ( 'NONE', #45519 ) ;
#18240 = CARTESIAN_POINT ( 'NONE',  ( -11.99351654964669756, -4.186483450353271074, 195.0000000000000284 ) ) ;
#18241 = FACE_OUTER_BOUND ( 'NONE', #49656, .T. ) ;
#18242 = ORIENTED_EDGE ( 'NONE', *, *, #23443, .F. ) ;
#18243 = EDGE_LOOP ( 'NONE', ( #27285, #23541, #27920, #7238 ) ) ;
#18244 = ORIENTED_EDGE ( 'NONE', *, *, #45580, .F. ) ;
#18245 = DIRECTION ( 'NONE',  ( -1.836970198721029934E-16, 1.836970198721036344E-16, -1.000000000000000000 ) ) ;
#18247 = ORIENTED_EDGE ( 'NONE', *, *, #1113, .T. ) ;
#18246 = DIRECTION ( 'NONE',  ( -1.000000000000000000, 0.000000000000000000, 0.000000000000000000 ) ) ;
#18248 = AXIS2_PLACEMENT_3D ( 'NONE', #36785, #68952, #62577 ) ;
#18249 = DIRECTION ( 'NONE',  ( -1.794541526872559352E-16, -1.000000000000000000, 0.000000000000000000 ) ) ;
#18250 = CARTESIAN_POINT ( 'NONE',  ( 50.83090410532631864, 3.657408540445007628, 2.000000000000000000 ) ) ;
#18251 = ORIENTED_EDGE ( 'NONE', *, *, #24047, .F. ) ;
#18252 = EDGE_LOOP ( 'NONE', ( #53568, #14598, #48057, #20186, #10744, #17451, #4841, #56162, #57143, #68753, #62856, #7677, #63232, #59747, #28418, #35267, #48318, #37851, #9329, #18019, #28408, #4417, #17275, #3150, #24318, #26842, #18957, #59843, #22990, #69686, #35914, #30062, #28261, #34606, #5710, #64415, #10242, #19823, #34572, #43655, #29178, #52703, #30331, #22266, #63764, #66623, #32384, #18771, #43057, #16434, #67558, #14247, #53743, #40351, #56073, #27492, #16727, #54536, #62964, #20255, #24815, #68067, #44303, #14600, #68731, #7797, #21933, #39789, #26584, #37171, #45244, #29857, #24094, #7459, #64251, #5692, #13342, #1495, #3217, #66428, #23839, #36436, #18865, #26208, #16781, #61460, #55782, #3326, #49463, #5032, #66454, #54791, #58683, #61453, #22210, #34157, #1834, #69403, #2687, #19287, #63275, #54130, #34682, #41353, #57978, #40963, #25400, #37824, #34002, #8199, #67649, #4187, #14572, #67000, #23280, #8108, #62336, #58856, #30554, #12829, #46566, #15768, #30294, #16448, #41500, #20780, #47451, #10151, #5365, #7225, #69744, #20006, #5979, #56575, #56293, #54, #1226, #40941, #41741, #776, #14505, #11234, #12866, #50101, #51723, #25073, #25296, #18510, #61174, #39778, #53822, #3636, #617, #37099, #13762, #33512, #37348, #24500, #21810, #60140, #56835, #10439, #47922, #37671, #266, #900, #42719, #65909, #53227, #531, #4459, #39016, #61364, #31620, #27133, #36619, #50697, #25591, #20354, #20730, #27709, #67972, #20608, #59313, #60213, #40260, #24390, #39446, #56672, #360, #751, #57752, #60428, #63042, #30569, #59287, #42335, #28985, #54375, #53023, #38325, #26751, #61534, #4951, #64012, #23977, #47041, #64464, #63150, #44094, #10933, #25145, #43740, #49804 ) ) ;
#18253 = VECTOR ( 'NONE', #48491, 1000.000000000000000 ) ;
#18254 = CARTESIAN_POINT ( 'NONE',  ( 6.006483450353379716, -6.006483450353394815, 195.0000000000000284 ) ) ;
#18255 = DIRECTION ( 'NONE',  ( 0.000000000000000000, 1.000000000000000000, 0.000000000000000000 ) ) ;
#18256 = DIRECTION ( 'NONE',  ( -0.000000000000000000, 3.673940397442059868E-16, -1.000000000000000000 ) ) ;
#18257 = EDGE_CURVE ( 'NONE', #45713, #33646, #61795, .T. ) ;
#18258 = DIRECTION ( 'NONE',  ( 0.000000000000000000, 0.000000000000000000, 1.000000000000000000 ) ) ;
#18259 = DIRECTION ( 'NONE',  ( 1.000000000000000000, 0.000000000000000000, 0.000000000000000000 ) ) ;
#18260 = VECTOR ( 'NONE', #43680, 1000.000000000000000 ) ;
#18262 = ORIENTED_EDGE ( 'NONE', *, *, #53131, .T. ) ;
#18261 = FACE_OUTER_BOUND ( 'NONE', #38018, .T. ) ;
#18263 = EDGE_LOOP ( 'NONE', ( #11208, #10948, #8682, #49639 ) ) ;
#18264 = DIRECTION ( 'NONE',  ( 1.000000000000000000, 0.000000000000000000, 0.000000000000000000 ) ) ;
#18265 = DIRECTION ( 'NONE',  ( 0.7071067811865474617, -0.7071067811865474617, 0.000000000000000000 ) ) ;
#18266 = PLANE ( 'NONE',  #49429 ) ;
#18267 = EDGE_CURVE ( 'NONE', #57192, #25545, #33401, .T. ) ;
#18268 = EDGE_CURVE ( 'NONE', #52552, #52916, #24670, .T. ) ;
#18269 = DIRECTION ( 'NONE',  ( 1.836970198721029934E-16, -1.836970198721036344E-16, 1.000000000000000000 ) ) ;
#18271 = ORIENTED_EDGE ( 'NONE', *, *, #15469, .F. ) ;
#18270 = EDGE_CURVE ( 'NONE', #11023, #49648, #7379, .T. ) ;
#18272 = DIRECTION ( 'NONE',  ( 0.000000000000000000, -0.000000000000000000, -1.000000000000000000 ) ) ;
#18273 = EDGE_CURVE ( 'NONE', #29536, #39983, #64256, .T. ) ;
#18274 = CYLINDRICAL_SURFACE ( 'NONE', #46316, 0.5000000000079367624 ) ;
#18275 = VECTOR ( 'NONE', #62537, 1000.000000000000000 ) ;
#18276 = CARTESIAN_POINT ( 'NONE',  ( 7.357023737882806280, 6.651770455163672935, 54.00000000000000711 ) ) ;
#18277 = PRODUCT_DEFINITION_SHAPE ( 'NONE', 'NONE',  #17120 ) ;
#18278 = EDGE_CURVE ( 'NONE', #60747, #61956, #69555, .T. ) ;
#18279 = CARTESIAN_POINT ( 'NONE',  ( 16.75000000000000000, -2.500000000000000000, 21.77831216351300014 ) ) ;
#18280 = DIRECTION ( 'NONE',  ( 1.836970198721029934E-16, 1.836970198721010706E-16, -1.000000000000000000 ) ) ;
#18281 = AXIS2_PLACEMENT_3D ( 'NONE', #3380, #41198, #65148 ) ;
#18282 = LINE ( 'NONE', #50811, #69125 ) ;
#18283 = ORIENTED_EDGE ( 'NONE', *, *, #8149, .F. ) ;
#18284 = CARTESIAN_POINT ( 'NONE',  ( -2.277516549646768418, -9.841277389592759661, 195.0000000000000284 ) ) ;
#18285 = DIRECTION ( 'NONE',  ( -1.000000000000000000, 5.120954910632640039E-15, 0.000000000000000000 ) ) ;
#18286 = ORIENTED_EDGE ( 'NONE', *, *, #61797, .T. ) ;
#18287 = CARTESIAN_POINT ( 'NONE',  ( -25.50000000000000355, -15.50000000000000000, -22.50000000000000000 ) ) ;
#18288 = VECTOR ( 'NONE', #10428, 1000.000000000000000 ) ;
#18289 = DIRECTION ( 'NONE',  ( 0.000000000000000000, -0.7071067811865460184, -0.7071067811865489050 ) ) ;
#18290 = LINE ( 'NONE', #33528, #5043 ) ;
#18291 = DIRECTION ( 'NONE',  ( 1.000000000000000000, -5.981805089575194965E-17, 0.000000000000000000 ) ) ;
#18292 = DIRECTION ( 'NONE',  ( 0.000000000000000000, -1.000000000000000000, 0.000000000000000000 ) ) ;
#18293 = AXIS2_PLACEMENT_3D ( 'NONE', #37477, #4611, #47729 ) ;
#18294 = ORIENTED_EDGE ( 'NONE', *, *, #23883, .F. ) ;
#18295 = CARTESIAN_POINT ( 'NONE',  ( 8.900000000000002132, -18.00000000000000355, -21.00000000000000000 ) ) ;
#18296 = VECTOR ( 'NONE', #37122, 1000.000000000000000 ) ;
#18297 = ORIENTED_EDGE ( 'NONE', *, *, #41991, .F. ) ;
#18298 = DIRECTION ( 'NONE',  ( 1.000000000000000000, -0.000000000000000000, -0.000000000000000000 ) ) ;
#18299 = VERTEX_POINT ( 'NONE', #26078 ) ;
#18300 = CARTESIAN_POINT ( 'NONE',  ( 11.50000000000000000, -11.50000000000100009, -10.50000000000065903 ) ) ;
#18301 = AXIS2_PLACEMENT_3D ( 'NONE', #16917, #60039, #11587 ) ;
#18302 = CARTESIAN_POINT ( 'NONE',  ( 2.706483450353350584, -10.09643294401463365, 455.0000000000000568 ) ) ;
#18303 = CARTESIAN_POINT ( 'NONE',  ( 7.826483450353421745, 11.99351654964657499, 455.0000000000000568 ) ) ;
#18304 = VERTEX_POINT ( 'NONE', #63557 ) ;
#18305 = ORIENTED_EDGE ( 'NONE', *, *, #23080, .F. ) ;
#18306 = DIRECTION ( 'NONE',  ( 1.000000000000000000, -0.000000000000000000, -0.000000000000000000 ) ) ;
#18307 = EDGE_LOOP ( 'NONE', ( #54616, #30140, #52190, #12859, #15401, #48293, #10945, #38774, #42829, #64038, #36908, #11465, #43215, #60042, #26581, #26890 ) ) ;
#18308 = ORIENTED_EDGE ( 'NONE', *, *, #1602, .F. ) ;
#18309 = LINE ( 'NONE', #40235, #2198 ) ;
#18310 = CARTESIAN_POINT ( 'NONE',  ( -7.450000000000001954, 0.000000000000000000, -23.00000000000000000 ) ) ;
#18311 = CARTESIAN_POINT ( 'NONE',  ( 39.90000000000000568, 21.00000000000000355, 13.98999642601812354 ) ) ;
#18312 = ORIENTED_EDGE ( 'NONE', *, *, #11665, .T. ) ;
#18313 = EDGE_CURVE ( 'NONE', #44242, #67236, #46572, .T. ) ;
#18314 = DIRECTION ( 'NONE',  ( 0.6785983445458448893, 0.2810846377148217834, -0.6785983445458485530 ) ) ;
#18315 = ADVANCED_FACE ( 'NONE', ( #58247 ), #46924, .F. ) ;
#18317 = DIRECTION ( 'NONE',  ( 1.000000000000000000, 0.000000000000000000, 0.000000000000000000 ) ) ;
#18316 = FACE_OUTER_BOUND ( 'NONE', #52121, .T. ) ;
#18318 = ORIENTED_EDGE ( 'NONE', *, *, #29679, .F. ) ;
#18320 = ORIENTED_EDGE ( 'NONE', *, *, #68938, .T. ) ;
#18319 = CARTESIAN_POINT ( 'NONE',  ( 10.05377373788281581, 9.689726262117151379, 54.00000000000000711 ) ) ;
#18321 = CIRCLE ( 'NONE', #29634, 0.1999999999999996503 ) ;
#18322 = EDGE_LOOP ( 'NONE', ( #24159, #20635, #63016, #20317, #25003, #30501, #57386, #19363 ) ) ;
#18323 = EDGE_CURVE ( 'NONE', #60266, #16172, #9458, .T. ) ;
#18324 = DIRECTION ( 'NONE',  ( 0.000000000000000000, 0.000000000000000000, 1.000000000000000000 ) ) ;
#18325 = CARTESIAN_POINT ( 'NONE',  ( 8.835729544836338434, -2.369523737882826886, 54.00000000000000711 ) ) ;
#18326 = AXIS2_PLACEMENT_3D ( 'NONE', #21080, #69171, #32728 ) ;
#18327 = ORIENTED_EDGE ( 'NONE', *, *, #10469, .T. ) ;
#18328 = DIRECTION ( 'NONE',  ( -0.000000000000000000, -0.000000000000000000, 1.000000000000000000 ) ) ;
#18329 = DIRECTION ( 'NONE',  ( 0.000000000000000000, -2.206568261432184716E-12, 1.000000000000000000 ) ) ;
#18330 = VERTEX_POINT ( 'NONE', #3454 ) ;
#18331 = ORIENTED_EDGE ( 'NONE', *, *, #54716, .T. ) ;
#18332 = VECTOR ( 'NONE', #40500, 1000.000000000000000 ) ;
#18333 = DIRECTION ( 'NONE',  ( -1.836970198721029934E-16, 1.836970198721036590E-16, -1.000000000000000000 ) ) ;
#18334 = DIRECTION ( 'NONE',  ( -1.000000000000000000, 1.047444401652940007E-14, -1.836970198721010706E-16 ) ) ;
#18335 = ORIENTED_EDGE ( 'NONE', *, *, #47040, .F. ) ;
#18336 = DIRECTION ( 'NONE',  ( 9.912705577010336396E-15, 1.000000000000000000, 0.000000000000000000 ) ) ;
#18337 = DIRECTION ( 'NONE',  ( 0.000000000000000000, 0.000000000000000000, -1.000000000000000000 ) ) ;
#18338 = DIRECTION ( 'NONE',  ( 1.000000000000000000, -0.000000000000000000, 0.000000000000000000 ) ) ;
#18339 = VERTEX_POINT ( 'NONE', #14415 ) ;
#18340 = AXIS2_PLACEMENT_3D ( 'NONE', #40417, #33378, #49972 ) ;
#18341 = CARTESIAN_POINT ( 'NONE',  ( 34.89999999999999858, -14.06939075806902117, -20.80000000000000426 ) ) ;
#18342 = DIRECTION ( 'NONE',  ( 1.214636490590110272E-14, 1.000000000000000000, 1.836970198721032892E-16 ) ) ;
#18343 = ORIENTED_EDGE ( 'NONE', *, *, #61674, .T. ) ;
#18345 = ORIENTED_EDGE ( 'NONE', *, *, #59371, .F. ) ;
#18344 = CARTESIAN_POINT ( 'NONE',  ( 15.50000000000000000, -0.1999999999999999556, 23.94999999999999574 ) ) ;
#18347 = DIRECTION ( 'NONE',  ( 1.130039751537442024E-14, 1.000000000000000000, 1.836970198721015636E-16 ) ) ;
#18346 = AXIS2_PLACEMENT_3D ( 'NONE', #29590, #18280, #51162 ) ;
#18348 = DIRECTION ( 'NONE',  ( -1.000000000000000000, 3.491481338843133355E-15, 1.836970198721036344E-16 ) ) ;
#18349 = PLANE ( 'NONE',  #6480 ) ;
#18350 = FACE_OUTER_BOUND ( 'NONE', #34452, .T. ) ;
#18351 = VECTOR ( 'NONE', #43079, 1000.000000000000000 ) ;
#18352 = CARTESIAN_POINT ( 'NONE',  ( 11.00000000000000000, -17.35230188589299516, -15.35019951917100478 ) ) ;
#18353 = EDGE_LOOP ( 'NONE', ( #59361, #38148, #29885, #18228 ) ) ;
#18354 = CARTESIAN_POINT ( 'NONE',  ( 30.00000000000000000, -12.00000000000000000, 12.20000000000000107 ) ) ;
#18355 = CARTESIAN_POINT ( 'NONE',  ( 1.480523737882811552, 9.390476262117216422, 26.00000000000000711 ) ) ;
#18356 = EDGE_CURVE ( 'NONE', #30792, #36191, #51622, .T. ) ;
#18357 = CARTESIAN_POINT ( 'NONE',  ( 5.668387132715920096, 8.393516549646628633, 195.0000000000000284 ) ) ;
#18359 = ORIENTED_EDGE ( 'NONE', *, *, #69112, .F. ) ;
#18358 = DIRECTION ( 'NONE',  ( -0.7071067811865530128, -0.7071067811865421326, 0.000000000000000000 ) ) ;
#18360 = CARTESIAN_POINT ( 'NONE',  ( -11.00000000000000000, -5.200000000000001066, -26.59999999999999787 ) ) ;
#18361 = VECTOR ( 'NONE', #63325, 1000.000000000000000 ) ;
#18362 = EDGE_CURVE ( 'NONE', #30827, #64746, #63905, .T. ) ;
#18363 = EDGE_CURVE ( 'NONE', #43564, #36247, #15807, .T. ) ;
#18364 = PLANE ( 'NONE',  #51025 ) ;
#18365 = EDGE_CURVE ( 'NONE', #57368, #47821, #57538, .T. ) ;
#18366 = ORIENTED_EDGE ( 'NONE', *, *, #43131, .F. ) ;
#18367 = LINE ( 'NONE', #39929, #13966 ) ;
#18368 = DIRECTION ( 'NONE',  ( -1.000000000000000000, 0.000000000000000000, 0.000000000000000000 ) ) ;
#18369 = VECTOR ( 'NONE', #15015, 1000.000000000000000 ) ;
#18370 = VERTEX_POINT ( 'NONE', #69200 ) ;
#18371 = PRODUCT_DEFINITION ( 'UNKNOWN', '', #4253, #38845 ) ;
#18372 = PLANE ( 'NONE',  #69607 ) ;
#18373 = CARTESIAN_POINT ( 'NONE',  ( 15.00000000000000000, -42.00000000000000000, 27.00000000000000000 ) ) ;
#18374 = SURFACE_STYLE_USAGE ( .BOTH. , #39263 ) ;
#18375 = ADVANCED_FACE ( 'NONE', ( #8753 ), #20064, .F. ) ;
#18376 = VECTOR ( 'NONE', #63164, 1000.000000000000000 ) ;
#18377 = CARTESIAN_POINT ( 'NONE',  ( 283.0000000000000568, -38.64999999999999858, 12.69999999999999929 ) ) ;
#18378 = ADVANCED_FACE ( 'NONE', ( #41271 ), #25023, .F. ) ;
#18379 = CARTESIAN_POINT ( 'NONE',  ( -9.547976262117222390, -2.369523737882729186, 54.00000000000000711 ) ) ;
#18380 = ORIENTED_EDGE ( 'NONE', *, *, #8236, .T. ) ;
#18381 = DIRECTION ( 'NONE',  ( 0.000000000000000000, 0.000000000000000000, -1.000000000000000000 ) ) ;
#18382 = EDGE_LOOP ( 'NONE', ( #58694, #65988, #25084, #9676 ) ) ;
#18383 = ORIENTED_EDGE ( 'NONE', *, *, #55114, .T. ) ;
#18384 = CARTESIAN_POINT ( 'NONE',  ( 30.00000000000000000, -5.599999999999999645, -9.000000000000001776 ) ) ;
#18385 = DIRECTION ( 'NONE',  ( 0.000000000000000000, 0.000000000000000000, -1.000000000000000000 ) ) ;
#18387 = FACE_OUTER_BOUND ( 'NONE', #21157, .T. ) ;
#18386 = LINE ( 'NONE', #45611, #28394 ) ;
#18388 = ORIENTED_EDGE ( 'NONE', *, *, #855, .T. ) ;
#18389 = ORIENTED_EDGE ( 'NONE', *, *, #36402, .T. ) ;
#18390 = CARTESIAN_POINT ( 'NONE',  ( 30.00000000000000000, -16.28999999999710369, 15.00000000000794920 ) ) ;
#18391 = EDGE_LOOP ( 'NONE', ( #8959, #47874 ) ) ;
#18392 = DIRECTION ( 'NONE',  ( -0.000000000000000000, 3.673940397442059868E-16, -1.000000000000000000 ) ) ;
#18393 = VECTOR ( 'NONE', #22684, 1000.000000000000000 ) ;
#18394 = CARTESIAN_POINT ( 'NONE',  ( 9.737023737882775976, 3.667976262117157660, 26.00000000000000711 ) ) ;
#18395 = FACE_OUTER_BOUND ( 'NONE', #35451, .T. ) ;
#18396 = CIRCLE ( 'NONE', #57940, 0.1750000000000002387 ) ;
#18397 = CARTESIAN_POINT ( 'NONE',  ( -7.172176262117259782, 5.242976262117182706, 54.00000000000000711 ) ) ;
#18399 = LINE ( 'NONE', #2846, #41221 ) ;
#18398 = DIRECTION ( 'NONE',  ( 1.836970198721029934E-16, -1.836970198721036344E-16, 1.000000000000000000 ) ) ;
#18400 = VECTOR ( 'NONE', #29956, 1000.000000000000000 ) ;
#18401 = ORIENTED_EDGE ( 'NONE', *, *, #24803, .T. ) ;
#18403 = ORIENTED_EDGE ( 'NONE', *, *, #29577, .F. ) ;
#18402 = LINE ( 'NONE', #45277, #23943 ) ;
#18404 = ORIENTED_EDGE ( 'NONE', *, *, #1657, .T. ) ;
#18405 = ORIENTED_EDGE ( 'NONE', *, *, #42787, .T. ) ;
#18406 = EDGE_CURVE ( 'NONE', #47285, #55064, #4165, .T. ) ;
#18407 = COLOUR_RGB ( '', 0.40784314, 0.44705882, 0.49803922) ;
#18408 = CIRCLE ( 'NONE', #27467, 0.5249999999999990230 ) ;
#18409 = FACE_OUTER_BOUND ( 'NONE', #14000, .T. ) ;
#18410 = DIRECTION ( 'NONE',  ( 0.000000000000000000, -0.000000000000000000, 1.000000000000000000 ) ) ;
#18411 = EDGE_LOOP ( 'NONE', ( #14305, #64112, #66896, #31247 ) ) ;
#18412 = ORIENTED_EDGE ( 'NONE', *, *, #69529, .T. ) ;
#18413 = EDGE_CURVE ( 'NONE', #34664, #46063, #4087, .T. ) ;
#18414 = DIRECTION ( 'NONE',  ( -1.000000000000000000, -0.000000000000000000, -0.000000000000000000 ) ) ;
#18415 = CYLINDRICAL_SURFACE ( 'NONE', #2912, 0.3500000000009988455 ) ;
#18416 = VECTOR ( 'NONE', #59113, 1000.000000000000000 ) ;
#18417 = ORIENTED_EDGE ( 'NONE', *, *, #25892, .F. ) ;
#18418 = ORIENTED_EDGE ( 'NONE', *, *, #48827, .F. ) ;
#18419 = CARTESIAN_POINT ( 'NONE',  ( -11.00000000000000000, -5.200000000000001066, 60.00000000000000000 ) ) ;
#18420 = EDGE_CURVE ( 'NONE', #9547, #11897, #10153, .T. ) ;
#18421 = CIRCLE ( 'NONE', #45476, 0.1749999999999998224 ) ;
#18422 = DIRECTION ( 'NONE',  ( -1.000000000000000000, 0.000000000000000000, 0.000000000000000000 ) ) ;
#18423 = ORIENTED_EDGE ( 'NONE', *, *, #1842, .F. ) ;
#18424 = DIRECTION ( 'NONE',  ( -1.000000000000000000, 0.000000000000000000, 0.000000000000000000 ) ) ;
#18425 = DIRECTION ( 'NONE',  ( -1.836970198721029934E-16, 1.836970198721036344E-16, -1.000000000000000000 ) ) ;
#18426 = CIRCLE ( 'NONE', #57980, 25.39999999999999858 ) ;
#18428 = EDGE_LOOP ( 'NONE', ( #55471, #55284, #15638, #34315, #8905, #55779, #46581 ) ) ;
#18427 = CARTESIAN_POINT ( 'NONE',  ( 7.272650909786644746, 7.798499376343933420, 455.0000000000000568 ) ) ;
#18429 = ORIENTED_EDGE ( 'NONE', *, *, #24047, .T. ) ;
#18430 = DIRECTION ( 'NONE',  ( 0.000000000000000000, 1.000000000000000000, 0.000000000000000000 ) ) ;
#18431 = LINE ( 'NONE', #39995, #23299 ) ;
#18432 = DIRECTION ( 'NONE',  ( 0.000000000000000000, 0.000000000000000000, 1.000000000000000000 ) ) ;
#18433 = CARTESIAN_POINT ( 'NONE',  ( 8.711985858128638682, 2.406732575409522568, 26.00000000000000711 ) ) ;
#18434 = EDGE_CURVE ( 'NONE', #36010, #31923, #21118, .T. ) ;
#18435 = DIRECTION ( 'NONE',  ( 0.000000000000000000, 1.000000000000000000, 0.000000000000000000 ) ) ;
#18436 = CARTESIAN_POINT ( 'NONE',  ( -30.00000000000000000, -17.14999999999999858, -27.00000000000000000 ) ) ;
#18437 = DIRECTION ( 'NONE',  ( -4.336808689942006692E-15, -1.000000000000000000, 0.000000000000000000 ) ) ;
#18438 = ORIENTED_EDGE ( 'NONE', *, *, #62573, .F. ) ;
#18439 = CARTESIAN_POINT ( 'NONE',  ( 276.8775010008008053, -21.00000000000000000, -17.50000000000000000 ) ) ;
#18441 = ORIENTED_EDGE ( 'NONE', *, *, #12560, .T. ) ;
#18440 = CARTESIAN_POINT ( 'NONE',  ( 146.5599459900709860, 9.000000000000001776, 320.8239988703753056 ) ) ;
#18442 = DIRECTION ( 'NONE',  ( -1.836970198721029934E-16, 1.836970198721036344E-16, -1.000000000000000000 ) ) ;
#18443 = VECTOR ( 'NONE', #63363, 1000.000000000000000 ) ;
#18444 = AXIS2_PLACEMENT_3D ( 'NONE', #67027, #62063, #56417 ) ;
#18445 = DIRECTION ( 'NONE',  ( -0.000000000000000000, -0.000000000000000000, -1.000000000000000000 ) ) ;
#18446 = ADVANCED_FACE ( 'NONE', ( #4853, #26419 ), #17529, .T. ) ;
#18447 = FACE_OUTER_BOUND ( 'NONE', #39869, .T. ) ;
#18449 = DIRECTION ( 'NONE',  ( 1.000000000000000000, -0.000000000000000000, 0.000000000000000000 ) ) ;
#18448 = CIRCLE ( 'NONE', #26256, 1.000000000000001776 ) ;
#18450 = STYLED_ITEM ( 'NONE', ( #50740 ), #66174 ) ;
#18451 = CARTESIAN_POINT ( 'NONE',  ( 25.90000000000000213, 0.000000000000000000, 0.000000000000000000 ) ) ;
#18452 = AXIS2_PLACEMENT_3D ( 'NONE', #1466, #17738, #12407 ) ;
#18453 = EDGE_CURVE ( 'NONE', #41857, #45178, #5208, .T. ) ;
#18454 = VERTEX_POINT ( 'NONE', #59640 ) ;
#18455 = EDGE_LOOP ( 'NONE', ( #38775, #5088, #6714, #62563 ) ) ;
#18456 = VECTOR ( 'NONE', #29359, 1000.000000000000000 ) ;
#18457 = DIRECTION ( 'NONE',  ( -0.000000000000000000, 3.673940397442059868E-16, -1.000000000000000000 ) ) ;
#18458 = VECTOR ( 'NONE', #61551, 1000.000000000000000 ) ;
#18459 = EDGE_CURVE ( 'NONE', #59802, #40034, #13083, .T. ) ;
#18460 = FILL_AREA_STYLE ('',( #63276 ) ) ;
#18461 = EDGE_CURVE ( 'NONE', #1371, #61947, #33104, .T. ) ;
#18462 = CARTESIAN_POINT ( 'NONE',  ( 276.8000000000000682, -20.40000000000000213, -17.60000000000000142 ) ) ;
#18463 = VERTEX_POINT ( 'NONE', #6590 ) ;
#18464 = CARTESIAN_POINT ( 'NONE',  ( 7.250000000000005329, 7.250000000000000888, -14.00000000000000000 ) ) ;
#18465 = ORIENTED_EDGE ( 'NONE', *, *, #24942, .F. ) ;
#18466 = EDGE_LOOP ( 'NONE', ( #46785, #7341, #50584, #8667 ) ) ;
#18467 = DIRECTION ( 'NONE',  ( -0.000000000000000000, -0.000000000000000000, 1.000000000000000000 ) ) ;
#18468 = CARTESIAN_POINT ( 'NONE',  ( -7.250000000000001776, -7.249999999999998224, -26.00000000000001066 ) ) ;
#18469 = ORIENTED_EDGE ( 'NONE', *, *, #47204, .F. ) ;
#18470 = LINE ( 'NONE', #55968, #33349 ) ;
#18471 = EDGE_CURVE ( 'NONE', #35907, #60253, #65631, .T. ) ;
#18472 = DIRECTION ( 'NONE',  ( -1.000000000000000000, 3.016910393003147986E-15, 1.108394896831706469E-30 ) ) ;
#18473 = CARTESIAN_POINT ( 'NONE',  ( 4.740315990920125344, 7.798499376343988487, 195.0000000000000284 ) ) ;
#18474 = ORIENTED_EDGE ( 'NONE', *, *, #4275, .F. ) ;
#18475 = EDGE_LOOP ( 'NONE', ( #36146, #24501, #34778, #25885 ) ) ;
#18477 = VERTEX_POINT ( 'NONE', #11186 ) ;
#18476 = CARTESIAN_POINT ( 'NONE',  ( -28.00000000000000000, -17.50000000000000000, 15.70499999999969809 ) ) ;
#18478 = VERTEX_POINT ( 'NONE', #65303 ) ;
#18479 = DIRECTION ( 'NONE',  ( -1.000000000000000000, 0.000000000000000000, 0.000000000000000000 ) ) ;
#18480 = CARTESIAN_POINT ( 'NONE',  ( 49.00000000000000000, -0.1999999999911795112, 8.826273045769999343E-12 ) ) ;
#18481 = CARTESIAN_POINT ( 'NONE',  ( 8.241237374594247100, 1.620245201994230611, 54.00000000000000711 ) ) ;
#18482 = EDGE_CURVE ( 'NONE', #34056, #4079, #33457, .T. ) ;
#18483 = DIRECTION ( 'NONE',  ( -0.000000000000000000, -0.000000000000000000, -1.000000000000000000 ) ) ;
#18484 = CIRCLE ( 'NONE', #37691, 0.2000000000000005107 ) ;
#18485 = DIRECTION ( 'NONE',  ( 1.000000000000000000, 0.000000000000000000, 0.000000000000000000 ) ) ;
#18486 = LINE ( 'NONE', #19199, #25133 ) ;
#18487 = VERTEX_POINT ( 'NONE', #55045 ) ;
#18488 = VERTEX_POINT ( 'NONE', #64594 ) ;
#18489 = ORIENTED_EDGE ( 'NONE', *, *, #66694, .T. ) ;
#18490 = EDGE_CURVE ( 'NONE', #69553, #52350, #28148, .T. ) ;
#18491 = ORIENTED_EDGE ( 'NONE', *, *, #57412, .T. ) ;
#18492 = DIRECTION ( 'NONE',  ( -1.000000000000000000, 0.000000000000000000, 0.000000000000000000 ) ) ;
#18493 = DIRECTION ( 'NONE',  ( 0.000000000000000000, 0.000000000000000000, 1.000000000000000000 ) ) ;
#18494 = EDGE_CURVE ( 'NONE', #32668, #69381, #21457, .T. ) ;
#18495 = DIRECTION ( 'NONE',  ( 1.836970198721029934E-16, 1.836970198721010706E-16, -1.000000000000000000 ) ) ;
#18496 = AXIS2_PLACEMENT_3D ( 'NONE', #6310, #48754, #43432 ) ;
#18498 = LINE ( 'NONE', #14267, #44545 ) ;
#18497 = CIRCLE ( 'NONE', #54663, 2.250000000000001776 ) ;
#18499 = ORIENTED_EDGE ( 'NONE', *, *, #14551, .F. ) ;
#18500 = ORIENTED_EDGE ( 'NONE', *, *, #20368, .F. ) ;
#18501 = VERTEX_POINT ( 'NONE', #49714 ) ;
#18502 = EDGE_CURVE ( 'NONE', #27132, #62471, #60541, .T. ) ;
#18503 = CARTESIAN_POINT ( 'NONE',  ( -15.50000000000000000, -0.4000000000005236034, -22.50000000000000000 ) ) ;
#18504 = VERTEX_POINT ( 'NONE', #16155 ) ;
#18505 = VECTOR ( 'NONE', #54253, 1000.000000000000000 ) ;
#18506 = VECTOR ( 'NONE', #12529, 1000.000000000000000 ) ;
#18507 = EDGE_CURVE ( 'NONE', #3987, #7623, #68427, .T. ) ;
#18508 = EDGE_LOOP ( 'NONE', ( #9380, #40857 ) ) ;
#18509 = ORIENTED_EDGE ( 'NONE', *, *, #35292, .F. ) ;
#18510 = ORIENTED_EDGE ( 'NONE', *, *, #62600, .T. ) ;
#18511 = DIRECTION ( 'NONE',  ( 0.000000000000000000, -0.9921567416492215186, 0.1249999999999996531 ) ) ;
#18512 = AXIS2_PLACEMENT_3D ( 'NONE', #15583, #37483, #32173 ) ;
#18513 = EDGE_CURVE ( 'NONE', #30760, #15934, #16508, .T. ) ;
#18515 = EDGE_LOOP ( 'NONE', ( #29477, #64620, #19098, #59311 ) ) ;
#18514 = CARTESIAN_POINT ( 'NONE',  ( 30.90000000000000213, -14.06939075806902117, -20.80000000000000426 ) ) ;
#18516 = ORIENTED_EDGE ( 'NONE', *, *, #60432, .T. ) ;
#18517 = LINE ( 'NONE', #34420, #40211 ) ;
#18518 = LINE ( 'NONE', #67670, #25056 ) ;
#18519 = CARTESIAN_POINT ( 'NONE',  ( 7.450000000000004619, -1.336933437520057563E-15, -7.000000000000000000 ) ) ;
#18520 = EDGE_CURVE ( 'NONE', #61558, #611, #36850, .T. ) ;
#18522 = ORIENTED_EDGE ( 'NONE', *, *, #7853, .T. ) ;
#18521 = FACE_OUTER_BOUND ( 'NONE', #66688, .T. ) ;
#18524 = EDGE_CURVE ( 'NONE', #64510, #35812, #5895, .T. ) ;
#18523 = AXIS2_PLACEMENT_3D ( 'NONE', #37923, #26962, #65480 ) ;
#18525 = EDGE_LOOP ( 'NONE', ( #67594, #66974, #47765, #35237 ) ) ;
#18526 = EDGE_CURVE ( 'NONE', #59410, #31564, #954, .T. ) ;
#18527 = DIRECTION ( 'NONE',  ( -6.508391731846281342E-15, -1.000000000000000000, -1.836970198721024757E-16 ) ) ;
#18528 = ADVANCED_FACE ( 'NONE', ( #10845 ), #32429, .F. ) ;
#18529 = ADVANCED_FACE ( 'NONE', ( #11525 ), #38088, .F. ) ;
#18530 = DIRECTION ( 'NONE',  ( -1.000000000000000000, 0.000000000000000000, 0.000000000000000000 ) ) ;
#18531 = CARTESIAN_POINT ( 'NONE',  ( -3.834182069070763976, 7.517976262117170627, 54.00000000000000711 ) ) ;
#18532 = ORIENTED_EDGE ( 'NONE', *, *, #58977, .T. ) ;
#18533 = DIRECTION ( 'NONE',  ( -1.000000000000000000, 0.000000000000000000, 0.000000000000000000 ) ) ;
#18534 = ADVANCED_FACE ( 'NONE', ( #22508 ), #38756, .T. ) ;
#18535 = CARTESIAN_POINT ( 'NONE',  ( 283.0000000000000568, -26.50000000000000000, -9.080000000000000071 ) ) ;
#18536 = CARTESIAN_POINT ( 'NONE',  ( -8.079219948824906794, 8.697938382363059162, 26.00000000000000711 ) ) ;
#18537 = ADVANCED_FACE ( 'NONE', ( #45795 ), #61707, .T. ) ;
#18538 = VERTEX_POINT ( 'NONE', #12220 ) ;
#18539 = VECTOR ( 'NONE', #10063, 1000.000000000000000 ) ;
#18540 = DIRECTION ( 'NONE',  ( 1.000000000000000000, 1.570596175624152093E-15, 0.000000000000000000 ) ) ;
#18541 = EDGE_CURVE ( 'NONE', #58826, #21251, #69599, .T. ) ;
#18542 = CARTESIAN_POINT ( 'NONE',  ( -7.250000000000001776, -7.249999999999998224, -17.50000000000000000 ) ) ;
#18543 = CARTESIAN_POINT ( 'NONE',  ( -7.250000000000000888, 8.250000000000001776, -16.00000000000000000 ) ) ;
#18544 = VECTOR ( 'NONE', #49789, 1000.000000000000000 ) ;
#18545 = VERTEX_POINT ( 'NONE', #34128 ) ;
#18546 = FILL_AREA_STYLE ('',( #51076 ) ) ;
#18547 = ADVANCED_FACE ( 'NONE', ( #1611 ), #51457, .F. ) ;
#18548 = CARTESIAN_POINT ( 'NONE',  ( 78.77321854994620765, 47.95351654967443977, 0.000000000000000000 ) ) ;
#18549 = LINE ( 'NONE', #18204, #42445 ) ;
#18550 = EDGE_CURVE ( 'NONE', #35182, #35322, #13621, .T. ) ;
#18551 = AXIS2_PLACEMENT_3D ( 'NONE', #4152, #53294, #25004 ) ;
#18552 = VECTOR ( 'NONE', #9305, 1000.000000000000000 ) ;
#18553 = ORIENTED_EDGE ( 'NONE', *, *, #4771, .T. ) ;
#18554 = DIRECTION ( 'NONE',  ( 0.000000000000000000, 0.000000000000000000, 1.000000000000000000 ) ) ;
#18555 = DIRECTION ( 'NONE',  ( -1.000000000000000000, 2.602085213965213008E-15, 0.000000000000000000 ) ) ;
#18556 = CARTESIAN_POINT ( 'NONE',  ( -11.50000000000000000, -15.97213595500069871, 14.50000000000000000 ) ) ;
#18557 = DIRECTION ( 'NONE',  ( 1.000000000000000000, -0.000000000000000000, 1.224646799147353207E-16 ) ) ;
#18558 = DIRECTION ( 'NONE',  ( 0.000000000000000000, 1.000000000000000000, 0.000000000000000000 ) ) ;
#18559 = AXIS2_PLACEMENT_3D ( 'NONE', #48510, #6072, #65132 ) ;
#18560 = ORIENTED_EDGE ( 'NONE', *, *, #56249, .T. ) ;
#18561 = CARTESIAN_POINT ( 'NONE',  ( -15.50000000000000000, -0.2038245569916614930, -21.05662432702600029 ) ) ;
#18562 = DIRECTION ( 'NONE',  ( 0.000000000000000000, 1.000000000000000000, 0.000000000000000000 ) ) ;
#18563 = ADVANCED_FACE ( 'NONE', ( #67014 ), #8310, .F. ) ;
#18564 = PLANE ( 'NONE',  #58237 ) ;
#18565 = CARTESIAN_POINT ( 'NONE',  ( 283.0000000000000568, -26.79000000000000625, 0.000000000000000000 ) ) ;
#18566 = CARTESIAN_POINT ( 'NONE',  ( -10.03972626211722918, 9.689726262117183353, 54.00000000000000711 ) ) ;
#18567 = EDGE_LOOP ( 'NONE', ( #38086, #37911, #49770, #55962 ) ) ;
#18569 = VERTEX_POINT ( 'NONE', #56064 ) ;
#18568 = DIRECTION ( 'NONE',  ( 0.7071067811865515695, 0.7071067811865435759, 0.000000000000000000 ) ) ;
#18570 = LINE ( 'NONE', #24593, #62048 ) ;
#18571 = DIRECTION ( 'NONE',  ( 0.000000000000000000, -0.7046037717806115097, -0.7096009616626348659 ) ) ;
#18572 = VECTOR ( 'NONE', #30105, 1000.000000000000000 ) ;
#18573 = ORIENTED_EDGE ( 'NONE', *, *, #66026, .T. ) ;
#18574 = CIRCLE ( 'NONE', #2778, 0.2000000000000005107 ) ;
#18575 = DIRECTION ( 'NONE',  ( -1.000000000000000000, 7.808916176531286882E-15, 0.000000000000000000 ) ) ;
#18576 = ORIENTED_EDGE ( 'NONE', *, *, #25510, .F. ) ;
#18577 = DIRECTION ( 'NONE',  ( -1.000000000000000000, 0.000000000000000000, 0.000000000000000000 ) ) ;
#18578 = ORIENTED_EDGE ( 'NONE', *, *, #19025, .T. ) ;
#18579 = EDGE_LOOP ( 'NONE', ( #49749, #19795, #43476, #35387 ) ) ;
#18580 = DIRECTION ( 'NONE',  ( 0.000000000000000000, 0.000000000000000000, -1.000000000000000000 ) ) ;
#18581 = CARTESIAN_POINT ( 'NONE',  ( 1.090483450353420425, 11.33351654964659971, 455.0000000000000568 ) ) ;
#18582 = EDGE_CURVE ( 'NONE', #51967, #21925, #43595, .T. ) ;
#18583 = CARTESIAN_POINT ( 'NONE',  ( 49.00000000000000000, -0.1999999999911795112, 8.826273045769999343E-12 ) ) ;
#18584 = CARTESIAN_POINT ( 'NONE',  ( 7.250000000000004441, 8.750000000000001776, -30.00000000000001066 ) ) ;
#18585 = ORIENTED_EDGE ( 'NONE', *, *, #50681, .T. ) ;
#18586 = ORIENTED_EDGE ( 'NONE', *, *, #10090, .T. ) ;
#18587 = EDGE_CURVE ( 'NONE', #67830, #48298, #8546, .T. ) ;
#18588 = DIRECTION ( 'NONE',  ( 1.000000000000000000, -2.309061475090597584E-14, 1.836970198720987533E-16 ) ) ;
#18589 = FACE_OUTER_BOUND ( 'NONE', #39256, .T. ) ;
#18590 = ORIENTED_EDGE ( 'NONE', *, *, #41107, .T. ) ;
#18591 = EDGE_CURVE ( 'NONE', #68006, #5476, #67379, .T. ) ;
#18592 = VECTOR ( 'NONE', #46914, 1000.000000000000000 ) ;
#18593 = VERTEX_POINT ( 'NONE', #50413 ) ;
#18594 = VERTEX_POINT ( 'NONE', #50052 ) ;
#18595 = DIRECTION ( 'NONE',  ( 0.000000000000000000, 1.000000000000000000, 0.000000000000000000 ) ) ;
#18596 = EDGE_CURVE ( 'NONE', #37823, #26265, #22149, .T. ) ;
#18598 = ORIENTED_EDGE ( 'NONE', *, *, #26782, .F. ) ;
#18597 = CARTESIAN_POINT ( 'NONE',  ( 46.39999999999999858, 21.00000000000000000, -1.750000000000000222 ) ) ;
#18599 = FACE_OUTER_BOUND ( 'NONE', #38435, .T. ) ;
#18600 = CIRCLE ( 'NONE', #20889, 1.620999999999997332 ) ;
#18601 = CIRCLE ( 'NONE', #40040, 0.2000000000000005107 ) ;
#18602 = DIRECTION ( 'NONE',  ( 0.000000000000000000, 1.000000000000000000, 0.000000000000000000 ) ) ;
#18603 = VERTEX_POINT ( 'NONE', #29177 ) ;
#18604 = VERTEX_POINT ( 'NONE', #66669 ) ;
#18605 = CIRCLE ( 'NONE', #14071, 0.5249999999999990230 ) ;
#18606 = ADVANCED_FACE ( 'NONE', ( #66331 ), #39445, .F. ) ;
#18607 = DIRECTION ( 'NONE',  ( -0.000000000000000000, -0.000000000000000000, -1.000000000000000000 ) ) ;
#18608 = DIRECTION ( 'NONE',  ( 0.000000000000000000, 1.000000000000000000, 0.000000000000000000 ) ) ;
#18609 = CIRCLE ( 'NONE', #59261, 3.999999999999993339 ) ;
#18610 = DIRECTION ( 'NONE',  ( 0.000000000000000000, 1.000000000000000000, 0.000000000000000000 ) ) ;
#18611 = AXIS2_PLACEMENT_3D ( 'NONE', #7234, #28805, #27782 ) ;
#18612 = DIRECTION ( 'NONE',  ( 0.000000000000000000, 0.000000000000000000, 1.000000000000000000 ) ) ;
#18613 = DIRECTION ( 'NONE',  ( 0.000000000000000000, 0.000000000000000000, 1.000000000000000000 ) ) ;
#18614 = VECTOR ( 'NONE', #47850, 1000.000000000000000 ) ;
#18616 = EDGE_LOOP ( 'NONE', ( #51591, #24862, #56713, #40796 ) ) ;
#18615 = FACE_OUTER_BOUND ( 'NONE', #20131, .T. ) ;
#18617 = VERTEX_POINT ( 'NONE', #40129 ) ;
#18618 = VECTOR ( 'NONE', #64225, 1000.000000000000000 ) ;
#18619 = FACE_OUTER_BOUND ( 'NONE', #16424, .T. ) ;
#18620 = CARTESIAN_POINT ( 'NONE',  ( 6.849523737882814878, 10.49297626211720136, 26.00000000000000711 ) ) ;
#18621 = FACE_OUTER_BOUND ( 'NONE', #36093, .T. ) ;
#18622 = DIRECTION ( 'NONE',  ( 0.6414496315691485817, -0.7671651518153073113, 0.000000000000000000 ) ) ;
#18623 = FACE_OUTER_BOUND ( 'NONE', #37606, .T. ) ;
#18624 = ORIENTED_EDGE ( 'NONE', *, *, #32522, .F. ) ;
#18625 = DIRECTION ( 'NONE',  ( 0.000000000000000000, 1.000000000000000000, 3.673940397442059868E-16 ) ) ;
#18626 = CYLINDRICAL_SURFACE ( 'NONE', #34999, 0.7500000000000006661 ) ;
#18627 = EDGE_CURVE ( 'NONE', #69122, #65979, #54915, .T. ) ;
#18628 = DIRECTION ( 'NONE',  ( 1.000000000000000000, 0.000000000000000000, 0.000000000000000000 ) ) ;
#18629 = EDGE_CURVE ( 'NONE', #47019, #61785, #40490, .T. ) ;
#18630 = DIRECTION ( 'NONE',  ( 0.000000000000000000, 0.000000000000000000, 1.000000000000000000 ) ) ;
#18631 = ADVANCED_FACE ( 'NONE', ( #29533 ), #6917, .F. ) ;
#18632 = LINE ( 'NONE', #8369, #4811 ) ;
#18633 = LINE ( 'NONE', #23944, #63637 ) ;
#18634 = ORIENTED_EDGE ( 'NONE', *, *, #12999, .F. ) ;
#18635 = LINE ( 'NONE', #17602, #34289 ) ;
#18636 = DIRECTION ( 'NONE',  ( 1.836970198721029934E-16, 1.836970198721010706E-16, -1.000000000000000000 ) ) ;
#18637 = CIRCLE ( 'NONE', #23136, 0.1749999999999989342 ) ;
#18638 = ORIENTED_EDGE ( 'NONE', *, *, #68346, .F. ) ;
#18639 = CARTESIAN_POINT ( 'NONE',  ( -7.250000000000000888, 7.250000000000001776, -23.50000000000000000 ) ) ;
#18640 = CARTESIAN_POINT ( 'NONE',  ( 9.306483450353368880, 10.08346604330778362, 195.0000000000000284 ) ) ;
#18641 = DIRECTION ( 'NONE',  ( 0.000000000000000000, 0.000000000000000000, 1.000000000000000000 ) ) ;
#18642 = AXIS2_PLACEMENT_3D ( 'NONE', #32147, #4588, #20833 ) ;
#18643 = DIRECTION ( 'NONE',  ( -0.000000000000000000, -0.000000000000000000, -1.000000000000000000 ) ) ;
#18644 = ORIENTED_EDGE ( 'NONE', *, *, #63874, .T. ) ;
#18645 = LINE ( 'NONE', #8031, #30897 ) ;
#18646 = CIRCLE ( 'NONE', #28840, 0.1999999999999987899 ) ;
#18647 = VECTOR ( 'NONE', #30739, 1000.000000000000000 ) ;
#18648 = VECTOR ( 'NONE', #8783, 1000.000000000000000 ) ;
#18649 = ORIENTED_EDGE ( 'NONE', *, *, #61874, .F. ) ;
#18650 = FACE_OUTER_BOUND ( 'NONE', #26075, .T. ) ;
#18651 = ORIENTED_EDGE ( 'NONE', *, *, #53137, .T. ) ;
#18652 = FACE_OUTER_BOUND ( 'NONE', #59484, .T. ) ;
#18653 = AXIS2_PLACEMENT_3D ( 'NONE', #60417, #33557, #7016 ) ;
#18654 = AXIS2_PLACEMENT_3D ( 'NONE', #39026, #23103, #17454 ) ;
#18655 = VERTEX_POINT ( 'NONE', #1972 ) ;
#18656 = CARTESIAN_POINT ( 'NONE',  ( -10.50000000000000178, 9.690000000000001279, -5.000000000000000000 ) ) ;
#18657 = CIRCLE ( 'NONE', #5114, 3.500000000000003109 ) ;
#18658 = LINE ( 'NONE', #34570, #55965 ) ;
#18659 = ORIENTED_EDGE ( 'NONE', *, *, #54480, .T. ) ;
#18660 = ORIENTED_EDGE ( 'NONE', *, *, #13643, .F. ) ;
#18661 = CARTESIAN_POINT ( 'NONE',  ( 11.00000000000000000, -16.28999999999710369, -15.00000000000794920 ) ) ;
#18662 = VERTEX_POINT ( 'NONE', #18223 ) ;
#18663 = VERTEX_POINT ( 'NONE', #51104 ) ;
#18664 = EDGE_CURVE ( 'NONE', #17757, #30300, #48146, .T. ) ;
#18665 = DIRECTION ( 'NONE',  ( 0.000000000000000000, 0.000000000000000000, 1.000000000000000000 ) ) ;
#18666 = FACE_OUTER_BOUND ( 'NONE', #4510, .T. ) ;
#18667 =( GEOMETRIC_REPRESENTATION_CONTEXT ( 3 ) GLOBAL_UNCERTAINTY_ASSIGNED_CONTEXT ( ( #536 ) ) GLOBAL_UNIT_ASSIGNED_CONTEXT ( ( #15361, #37281, #4755 ) ) REPRESENTATION_CONTEXT ( 'NONE', 'WORKASPACE' ) );
#18668 = LINE ( 'NONE', #60763, #61456 ) ;
#18669 = ORIENTED_EDGE ( 'NONE', *, *, #54883, .T. ) ;
#18670 = MECHANICAL_DESIGN_GEOMETRIC_PRESENTATION_REPRESENTATION (  '', ( #44660 ), #57092 ) ;
#18671 = EDGE_CURVE ( 'NONE', #29287, #12416, #15385, .T. ) ;
#18672 = DIRECTION ( 'NONE',  ( 0.000000000000000000, 0.000000000000000000, -1.000000000000000000 ) ) ;
#18674 = CARTESIAN_POINT ( 'NONE',  ( -5.993516549646711766, 8.198316549646602169, 455.0000000000000568 ) ) ;
#18673 = DIRECTION ( 'NONE',  ( 0.000000000000000000, 0.000000000000000000, -1.000000000000000000 ) ) ;
#18675 = ORIENTED_EDGE ( 'NONE', *, *, #434, .F. ) ;
#18677 = EDGE_LOOP ( 'NONE', ( #67107, #51038, #34551, #51906 ) ) ;
#18676 = DIRECTION ( 'NONE',  ( 0.000000000000000000, 0.000000000000000000, 1.000000000000000000 ) ) ;
#18678 = EDGE_CURVE ( 'NONE', #11380, #65843, #44678, .T. ) ;
#18679 = VERTEX_POINT ( 'NONE', #35900 ) ;
#18680 = EDGE_CURVE ( 'NONE', #13213, #10975, #28878, .T. ) ;
#18681 = EDGE_CURVE ( 'NONE', #51393, #47121, #8674, .T. ) ;
#18682 = ADVANCED_FACE ( 'NONE', ( #19985 ), #52158, .T. ) ;
#18683 = DIRECTION ( 'NONE',  ( -0.000000000000000000, 3.673940397442059868E-16, -1.000000000000000000 ) ) ;
#18684 = ORIENTED_EDGE ( 'NONE', *, *, #61779, .F. ) ;
#18685 = CARTESIAN_POINT ( 'NONE',  ( 11.50000000000000000, -11.50000000000100009, 15.00000000000084910 ) ) ;
#18686 = EDGE_CURVE ( 'NONE', #15026, #60382, #62399, .T. ) ;
#18687 = CYLINDRICAL_SURFACE ( 'NONE', #7924, 1.000000000000000000 ) ;
#18688 = EDGE_LOOP ( 'NONE', ( #3855, #45195 ) ) ;
#18689 = MECHANICAL_DESIGN_GEOMETRIC_PRESENTATION_REPRESENTATION (  '', ( #52752 ), #22250 ) ;
#18690 = ORIENTED_EDGE ( 'NONE', *, *, #40272, .F. ) ;
#18691 = CARTESIAN_POINT ( 'NONE',  ( -8.821682069070780230, 2.530476262117183683, 54.00000000000000711 ) ) ;
#18692 = LINE ( 'NONE', #7378, #27806 ) ;
#18693 = VECTOR ( 'NONE', #11271, 1000.000000000000000 ) ;
#18694 = VERTEX_POINT ( 'NONE', #19281 ) ;
#18695 = FACE_OUTER_BOUND ( 'NONE', #16086, .T. ) ;
#18696 = CARTESIAN_POINT ( 'NONE',  ( 9.690000000000001279, -9.690000000000001279, -4.250000000000000000 ) ) ;
#18697 = VECTOR ( 'NONE', #56396, 1000.000000000000114 ) ;
#18698 = CARTESIAN_POINT ( 'NONE',  ( -3.663616288757055806, 4.135079735113128763, 54.00000000000000711 ) ) ;
#18699 = ORIENTED_EDGE ( 'NONE', *, *, #26840, .T. ) ;
#18700 = VECTOR ( 'NONE', #21680, 1000.000000000000000 ) ;
#18701 = CIRCLE ( 'NONE', #37915, 0.3499999999999597877 ) ;
#18702 = FACE_OUTER_BOUND ( 'NONE', #46839, .T. ) ;
#18703 = DIRECTION ( 'NONE',  ( 0.000000000000000000, 1.000000000000000000, 0.000000000000000000 ) ) ;
#18705 = ORIENTED_EDGE ( 'NONE', *, *, #67934, .T. ) ;
#18704 = SURFACE_STYLE_USAGE ( .BOTH. , #28276 ) ;
#18707 = ORIENTED_EDGE ( 'NONE', *, *, #54203, .T. ) ;
#18706 = DIRECTION ( 'NONE',  ( 0.000000000000000000, 0.000000000000000000, -1.000000000000000000 ) ) ;
#18708 = CARTESIAN_POINT ( 'NONE',  ( 10.50000000000000178, 9.690000000000001279, -4.250000000000000000 ) ) ;
#18709 = VECTOR ( 'NONE', #14296, 1000.000000000000000 ) ;
#18710 = AXIS2_PLACEMENT_3D ( 'NONE', #31399, #14767, #46935 ) ;
#18711 = AXIS2_PLACEMENT_3D ( 'NONE', #15224, #15916, #47389 ) ;
#18712 = CARTESIAN_POINT ( 'NONE',  ( 7.900000000000000355, 18.00000000000000355, -21.00000000000000000 ) ) ;
#18713 = LINE ( 'NONE', #50193, #25672 ) ;
#18714 = DIRECTION ( 'NONE',  ( -1.000000000000000000, 7.808916176531286882E-15, 0.000000000000000000 ) ) ;
#18715 = VECTOR ( 'NONE', #58631, 1000.000000000000000 ) ;
#18716 = LINE ( 'NONE', #55515, #40927 ) ;
#18717 = VERTEX_POINT ( 'NONE', #57805 ) ;
#18718 = CYLINDRICAL_SURFACE ( 'NONE', #44775, 0.1999999999999987899 ) ;
#18719 = CYLINDRICAL_SURFACE ( 'NONE', #49651, 24.99999999998784972 ) ;
#18720 = DIRECTION ( 'NONE',  ( 0.000000000000000000, 0.000000000000000000, 1.000000000000000000 ) ) ;
#18722 = VERTEX_POINT ( 'NONE', #51808 ) ;
#18721 = CARTESIAN_POINT ( 'NONE',  ( -30.00000000000000000, -9.487228132326899654, 12.50000000000000000 ) ) ;
#18723 = EDGE_CURVE ( 'NONE', #11916, #23956, #35529, .T. ) ;
#18724 = AXIS2_PLACEMENT_3D ( 'NONE', #9182, #52320, #56653 ) ;
#18725 = CARTESIAN_POINT ( 'NONE',  ( -4.173516549646666185, 11.99351654964658920, 195.0000000000000284 ) ) ;
#18726 = EDGE_CURVE ( 'NONE', #67203, #8462, #14338, .T. ) ;
#18727 = CARTESIAN_POINT ( 'NONE',  ( 275.0000000000000000, -23.50007830495750127, 12.28007262201345995 ) ) ;
#18728 = EDGE_CURVE ( 'NONE', #57404, #42826, #66198, .T. ) ;
#18729 = ORIENTED_EDGE ( 'NONE', *, *, #374, .T. ) ;
#18730 = VERTEX_POINT ( 'NONE', #24934 ) ;
#18731 = CARTESIAN_POINT ( 'NONE',  ( -8.250000000000000000, 7.250000000000001776, -9.000000000000001776 ) ) ;
#18732 = DIRECTION ( 'NONE',  ( -0.000000000000000000, -0.000000000000000000, -1.000000000000000000 ) ) ;
#18734 = ORIENTED_EDGE ( 'NONE', *, *, #18406, .F. ) ;
#18733 = EDGE_CURVE ( 'NONE', #35825, #66963, #9730, .T. ) ;
#18735 = DIRECTION ( 'NONE',  ( 1.000000000000000000, -0.000000000000000000, -0.000000000000000000 ) ) ;
#18736 =( NAMED_UNIT ( * ) SI_UNIT ( $, .STERADIAN. ) SOLID_ANGLE_UNIT ( ) );
#18737 =( REPRESENTATION_RELATIONSHIP ('NONE','NONE', #33057, #53035 ) REPRESENTATION_RELATIONSHIP_WITH_TRANSFORMATION ( #5577 )SHAPE_REPRESENTATION_RELATIONSHIP( ) );
#18738 = CARTESIAN_POINT ( 'NONE',  ( -7.250000000000000888, 7.250000000000001776, -8.000000000000000000 ) ) ;
#18739 = DIRECTION ( 'NONE',  ( -1.000000000000000000, 0.000000000000000000, 0.000000000000000000 ) ) ;
#18740 = ORIENTED_EDGE ( 'NONE', *, *, #45807, .F. ) ;
#18741 = CARTESIAN_POINT ( 'NONE',  ( 283.0000000000000568, -27.13000000000000611, -15.49999999999930012 ) ) ;
#18742 = VERTEX_POINT ( 'NONE', #47896 ) ;
#18743 = AXIS2_PLACEMENT_3D ( 'NONE', #5171, #48302, #42985 ) ;
#18744 = ORIENTED_EDGE ( 'NONE', *, *, #66823, .F. ) ;
#18745 = CARTESIAN_POINT ( 'NONE',  ( 7.186223737882818874, -5.257023737882815517, 26.00000000000000711 ) ) ;
#18746 = VECTOR ( 'NONE', #32761, 1000.000000000000000 ) ;
#18747 = SURFACE_SIDE_STYLE ('',( #40666 ) ) ;
#18748 = CIRCLE ( 'NONE', #58292, 4.000000000000000000 ) ;
#18750 = LINE ( 'NONE', #56922, #32138 ) ;
#18749 = DIRECTION ( 'NONE',  ( -1.000000000000000000, 0.000000000000000000, 0.000000000000000000 ) ) ;
#18751 = ORIENTED_EDGE ( 'NONE', *, *, #38413, .T. ) ;
#18752 = VERTEX_POINT ( 'NONE', #13969 ) ;
#18753 = CARTESIAN_POINT ( 'NONE',  ( 30.00000000000000000, -13.79999999999979998, 17.30000000000000071 ) ) ;
#18754 = VERTEX_POINT ( 'NONE', #20332 ) ;
#18755 = AXIS2_PLACEMENT_3D ( 'NONE', #22721, #58829, #37609 ) ;
#18756 = VECTOR ( 'NONE', #38581, 1000.000000000000000 ) ;
#18757 = ADVANCED_FACE ( 'NONE', ( #52513 ), #46843, .T. ) ;
#18758 = CIRCLE ( 'NONE', #65068, 1.449999999999996403 ) ;
#18759 = CYLINDRICAL_SURFACE ( 'NONE', #45040, 0.2000000000000005107 ) ;
#18760 = LINE ( 'NONE', #35010, #1959 ) ;
#18761 = DIRECTION ( 'NONE',  ( 0.7142857142857395036, 0.000000000000000000, 0.6998542122237394469 ) ) ;
#18762 = CYLINDRICAL_SURFACE ( 'NONE', #409, 24.99999999998784972 ) ;
#18763 = VERTEX_POINT ( 'NONE', #57106 ) ;
#18764 = CARTESIAN_POINT ( 'NONE',  ( -8.000000000000000000, 7.281754163448145079, -1.000000000000000000 ) ) ;
#18765 = CIRCLE ( 'NONE', #60559, 0.1749999999999989342 ) ;
#18766 = AXIS2_PLACEMENT_3D ( 'NONE', #7098, #28677, #50244 ) ;
#18768 = DIRECTION ( 'NONE',  ( 1.000000000000000000, -0.000000000000000000, -0.000000000000000000 ) ) ;
#18767 = DIRECTION ( 'NONE',  ( -1.000000000000000000, 0.000000000000000000, 0.000000000000000000 ) ) ;
#18769 = EDGE_LOOP ( 'NONE', ( #14749, #24628, #69929, #4783 ) ) ;
#18771 = ORIENTED_EDGE ( 'NONE', *, *, #16847, .T. ) ;
#18770 = DIRECTION ( 'NONE',  ( -0.7071067811865475727, 0.000000000000000000, -0.7071067811865475727 ) ) ;
#18772 = ORIENTED_EDGE ( 'NONE', *, *, #22436, .T. ) ;
#18773 = ORIENTED_EDGE ( 'NONE', *, *, #67881, .T. ) ;
#18774 = AXIS2_PLACEMENT_3D ( 'NONE', #36273, #26028, #47582 ) ;
#18775 = ADVANCED_FACE ( 'NONE', ( #3722 ), #53230, .F. ) ;
#18776 = CARTESIAN_POINT ( 'NONE',  ( 290.0000000000000000, 4.428935149116382035E-16, -3.232999999999965901 ) ) ;
#18777 = AXIS2_PLACEMENT_3D ( 'NONE', #39397, #45044, #35133 ) ;
#18778 = CARTESIAN_POINT ( 'NONE',  ( 47.00000000000000000, 0.7500000000000000000, 3.418698582794335028 ) ) ;
#18779 = EDGE_CURVE ( 'NONE', #60848, #12404, #68776, .T. ) ;
#18780 = VERTEX_POINT ( 'NONE', #36588 ) ;
#18781 = ORIENTED_EDGE ( 'NONE', *, *, #24183, .T. ) ;
#18782 = DIRECTION ( 'NONE',  ( 1.000000000000000000, 0.000000000000000000, 0.000000000000000000 ) ) ;
#18783 = DIRECTION ( 'NONE',  ( -1.000000000000000000, 0.000000000000000000, 0.000000000000000000 ) ) ;
#18784 = VERTEX_POINT ( 'NONE', #31317 ) ;
#18785 = VERTEX_POINT ( 'NONE', #69120 ) ;
#18786 = LINE ( 'NONE', #57318, #16118 ) ;
#18787 = CARTESIAN_POINT ( 'NONE',  ( 55.00000000000000000, 21.00000000000000000, -16.96999999999999886 ) ) ;
#18788 = ORIENTED_EDGE ( 'NONE', *, *, #43183, .T. ) ;
#18789 = CARTESIAN_POINT ( 'NONE',  ( 9.404523737882817258, -1.480523737882815549, 26.00000000000000711 ) ) ;
#18790 = LINE ( 'NONE', #35390, #37345 ) ;
#18791 = AXIS2_PLACEMENT_3D ( 'NONE', #41515, #41861, #4405 ) ;
#18793 = EDGE_LOOP ( 'NONE', ( #15701, #65307, #38834, #24144 ) ) ;
#18792 = LINE ( 'NONE', #20544, #47583 ) ;
#18794 = EDGE_LOOP ( 'NONE', ( #6553, #49629, #3196, #4659 ) ) ;
#18795 = DIRECTION ( 'NONE',  ( 0.000000000000000000, 0.000000000000000000, -1.000000000000000000 ) ) ;
#18796 = DIRECTION ( 'NONE',  ( -1.000000000000000000, 0.000000000000000000, 0.000000000000000000 ) ) ;
#18797 = DIRECTION ( 'NONE',  ( -0.6414496315691473605, -0.7671651518153083105, -2.309356642089130002E-17 ) ) ;
#18798 = DIRECTION ( 'NONE',  ( 0.000000000000000000, 0.000000000000000000, -1.000000000000000000 ) ) ;
#18799 = CARTESIAN_POINT ( 'NONE',  ( -5.242976262117259978, 5.242976262117182706, 26.00000000000000711 ) ) ;
#18800 = DIRECTION ( 'NONE',  ( 0.6414496315691575745, 0.7671651518152998728, 2.587583378555112027E-16 ) ) ;
#18801 = VECTOR ( 'NONE', #1761, 1000.000000000000000 ) ;
#18802 = VECTOR ( 'NONE', #59071, 1000.000000000000000 ) ;
#18803 = CARTESIAN_POINT ( 'NONE',  ( -30.00000000000000000, -17.00000000000000000, 15.70499999999969809 ) ) ;
#18804 = ORIENTED_EDGE ( 'NONE', *, *, #48389, .F. ) ;
#18805 = DIRECTION ( 'NONE',  ( -1.000000000000000000, 5.120954910632640039E-15, 1.881408311965255020E-30 ) ) ;
#18807 = EDGE_LOOP ( 'NONE', ( #15554, #5294, #26016, #46208 ) ) ;
#18806 = CARTESIAN_POINT ( 'NONE',  ( -5.242976262117259978, 5.242976262117182706, 26.00000000000000711 ) ) ;
#18808 = AXIS2_PLACEMENT_3D ( 'NONE', #28811, #45076, #39767 ) ;
#18810 = DIRECTION ( 'NONE',  ( 0.000000000000000000, 1.000000000000000000, 0.000000000000000000 ) ) ;
#18809 = AXIS2_PLACEMENT_3D ( 'NONE', #49835, #22624, #66441 ) ;
#18811 = CARTESIAN_POINT ( 'NONE',  ( 30.00000000000000000, -5.000000000000000000, 27.00000000000000000 ) ) ;
#18812 = DIRECTION ( 'NONE',  ( -1.000000000000000000, 1.047444401652939849E-14, -1.836970198721010706E-16 ) ) ;
#18813 = EDGE_CURVE ( 'NONE', #42028, #13533, #4439, .T. ) ;
#18814 = CARTESIAN_POINT ( 'NONE',  ( 275.0000000000000000, -23.65000000000000568, -12.40000000000000213 ) ) ;
#18815 = CIRCLE ( 'NONE', #21099, 1.224999999999999423 ) ;
#18816 = AXIS2_PLACEMENT_3D ( 'NONE', #57473, #4453, #9752 ) ;
#18817 = CARTESIAN_POINT ( 'NONE',  ( 7.250000000000005329, 8.250000000000001776, -7.500000000000000000 ) ) ;
#18818 = ORIENTED_EDGE ( 'NONE', *, *, #51938, .T. ) ;
#18819 = LINE ( 'NONE', #8903, #27948 ) ;
#18821 = ORIENTED_EDGE ( 'NONE', *, *, #50061, .T. ) ;
#18820 = EDGE_CURVE ( 'NONE', #42686, #31923, #26000, .T. ) ;
#18822 = VECTOR ( 'NONE', #6023, 1000.000000000000000 ) ;
#18823 = CYLINDRICAL_SURFACE ( 'NONE', #37043, 0.2000000000000005107 ) ;
#18824 = CARTESIAN_POINT ( 'NONE',  ( 176.4833316329832940, -10.00000000000000178, 324.6739988703752715 ) ) ;
#18825 = VECTOR ( 'NONE', #56283, 1000.000000000000000 ) ;
#18826 = CARTESIAN_POINT ( 'NONE',  ( 0.000000000000000000, 0.000000000000000000, -22.00000000000000000 ) ) ;
#18827 = ORIENTED_EDGE ( 'NONE', *, *, #55895, .F. ) ;
#18828 = CARTESIAN_POINT ( 'NONE',  ( -9.234937905884020637, 9.942044687070460185, 195.0000000000000284 ) ) ;
#18829 = EDGE_LOOP ( 'NONE', ( #9908, #20327, #45437, #64449 ) ) ;
#18830 = VERTEX_POINT ( 'NONE', #32342 ) ;
#18831 = LINE ( 'NONE', #40399, #59560 ) ;
#18832 = CARTESIAN_POINT ( 'NONE',  ( 10.74648345035338082, -1.090483450353395334, 195.0000000000000284 ) ) ;
#18833 = ORIENTED_EDGE ( 'NONE', *, *, #16396, .T. ) ;
#18834 = DIRECTION ( 'NONE',  ( 0.000000000000000000, 0.000000000000000000, 1.000000000000000000 ) ) ;
#18835 = CARTESIAN_POINT ( 'NONE',  ( -11.07551654964667520, 11.47551654964660450, 195.0000000000000284 ) ) ;
#18836 = ADVANCED_FACE ( 'NONE', ( #6157 ), #27384, .T. ) ;
#18837 = CARTESIAN_POINT ( 'NONE',  ( 30.00000000000000000, -8.959999999999999076, 12.95475478405700009 ) ) ;
#18838 = ORIENTED_EDGE ( 'NONE', *, *, #63495, .F. ) ;
#18839 = EDGE_LOOP ( 'NONE', ( #17817, #11936, #18114, #59907 ) ) ;
#18841 = VERTEX_POINT ( 'NONE', #22429 ) ;
#18840 = LINE ( 'NONE', #56669, #54316 ) ;
#18842 = VERTEX_POINT ( 'NONE', #49307 ) ;
#18843 = DIRECTION ( 'NONE',  ( -1.000000000000000000, 0.000000000000000000, 0.000000000000000000 ) ) ;
#18844 = CARTESIAN_POINT ( 'NONE',  ( 25.50000000000000355, -15.12100000000000044, -24.12099999999999511 ) ) ;
#18845 = CARTESIAN_POINT ( 'NONE',  ( 11.12648345035338160, 4.193516549646526315, 455.0000000000000568 ) ) ;
#18846 = DIRECTION ( 'NONE',  ( -1.000000000000000000, 0.000000000000000000, 0.000000000000000000 ) ) ;
#18847 = AXIS2_PLACEMENT_3D ( 'NONE', #18020, #34978, #45950 ) ;
#18848 = CARTESIAN_POINT ( 'NONE',  ( 11.00000000000000000, -11.70000000000000284, -12.50000000000000000 ) ) ;
#18849 = CARTESIAN_POINT ( 'NONE',  ( -1.677516549646768551, -9.841277389592764990, 195.0000000000000284 ) ) ;
#18850 = COLOUR_RGB ( '', 0.66274510, 0.83137255, 0.94901961) ;
#18851 = ORIENTED_EDGE ( 'NONE', *, *, #67678, .F. ) ;
#18852 = ORIENTED_EDGE ( 'NONE', *, *, #37991, .F. ) ;
#18853 = ORIENTED_EDGE ( 'NONE', *, *, #31995, .F. ) ;
#18854 = VECTOR ( 'NONE', #14824, 1000.000000000000000 ) ;
#18855 = VECTOR ( 'NONE', #54383, 1000.000000000000000 ) ;
#18856 = ORIENTED_EDGE ( 'NONE', *, *, #8216, .T. ) ;
#18857 = DIRECTION ( 'NONE',  ( 0.000000000000000000, -1.000000000000000000, 0.000000000000000000 ) ) ;
#18858 = CARTESIAN_POINT ( 'NONE',  ( 7.450000000000006395, 7.250000000000000888, -23.50000000000000000 ) ) ;
#18859 = ADVANCED_FACE ( 'NONE', ( #5481 ), #173, .F. ) ;
#18860 = AXIS2_PLACEMENT_3D ( 'NONE', #55963, #7521, #2918 ) ;
#18861 = AXIS2_PLACEMENT_3D ( 'NONE', #47585, #63856, #32031 ) ;
#18862 = DIRECTION ( 'NONE',  ( 1.000000000000000000, -0.000000000000000000, -0.000000000000000000 ) ) ;
#18863 = AXIS2_PLACEMENT_3D ( 'NONE', #26618, #30872, #53162 ) ;
#18864 = EDGE_CURVE ( 'NONE', #27405, #24080, #11115, .T. ) ;
#18865 = ORIENTED_EDGE ( 'NONE', *, *, #36967, .T. ) ;
#18866 = ORIENTED_EDGE ( 'NONE', *, *, #62841, .F. ) ;
#18867 = EDGE_CURVE ( 'NONE', #8437, #35406, #5123, .T. ) ;
#18868 = ORIENTED_EDGE ( 'NONE', *, *, #45240, .T. ) ;
#18869 = CARTESIAN_POINT ( 'NONE',  ( 7.450000000000003730, -7.249999999999997335, -14.50000000000000000 ) ) ;
#18870 = VECTOR ( 'NONE', #47951, 1000.000000000000000 ) ;
#18871 = AXIS2_PLACEMENT_3D ( 'NONE', #19369, #7707, #56844 ) ;
#18872 = ORIENTED_EDGE ( 'NONE', *, *, #16320, .F. ) ;
#18873 = EDGE_CURVE ( 'NONE', #16636, #67323, #43644, .T. ) ;
#18874 = ORIENTED_EDGE ( 'NONE', *, *, #9513, .F. ) ;
#18875 = CARTESIAN_POINT ( 'NONE',  ( 3.157023737882797665, 4.031976262117209053, 54.00000000000000711 ) ) ;
#18877 = ORIENTED_EDGE ( 'NONE', *, *, #59440, .T. ) ;
#18876 = PRODUCT_DEFINITION ( 'UNKNOWN', '', #1908, #19027 ) ;
#18878 = ORIENTED_EDGE ( 'NONE', *, *, #38889, .F. ) ;
#18879 = AXIS2_PLACEMENT_3D ( 'NONE', #14370, #46881, #23922 ) ;
#18880 = LINE ( 'NONE', #36181, #11299 ) ;
#18881 = ADVANCED_FACE ( 'NONE', ( #43290 ), #59898, .F. ) ;
#18883 = ORIENTED_EDGE ( 'NONE', *, *, #7106, .F. ) ;
#18882 = DIRECTION ( 'NONE',  ( 1.000000000000000000, 1.671920889371702854E-15, 6.142537696789956391E-31 ) ) ;
#18885 = ORIENTED_EDGE ( 'NONE', *, *, #41589, .T. ) ;
#18884 = EDGE_CURVE ( 'NONE', #10983, #62987, #48249, .T. ) ;
#18886 = CARTESIAN_POINT ( 'NONE',  ( -9.690000000000001279, -9.690000000000001279, -5.000000000000000000 ) ) ;
#18887 = CIRCLE ( 'NONE', #65192, 0.1999999999999992339 ) ;
#18888 = CARTESIAN_POINT ( 'NONE',  ( 36.90000000000000568, 13.66939075806899240, -20.79999999999999361 ) ) ;
#18889 = DIRECTION ( 'NONE',  ( -1.836970198721029934E-16, 1.836970198721036344E-16, -1.000000000000000000 ) ) ;
#18891 = EDGE_LOOP ( 'NONE', ( #42436, #49175, #33244, #41658 ) ) ;
#18890 = DIRECTION ( 'NONE',  ( 1.062171939662867618E-14, 1.000000000000000000, 0.000000000000000000 ) ) ;
#18892 = ORIENTED_EDGE ( 'NONE', *, *, #43939, .T. ) ;
#18893 = CARTESIAN_POINT ( 'NONE',  ( 7.357023737882784964, 3.834182069070697807, 54.00000000000000711 ) ) ;
#18894 = FACE_OUTER_BOUND ( 'NONE', #55929, .T. ) ;
#18895 = DIRECTION ( 'NONE',  ( 0.000000000000000000, 0.7066873191085843997, 0.7075259945833241026 ) ) ;
#18896 = VERTEX_POINT ( 'NONE', #42599 ) ;
#18897 = LINE ( 'NONE', #35490, #3225 ) ;
#18898 = FACE_OUTER_BOUND ( 'NONE', #45844, .T. ) ;
#18899 = CARTESIAN_POINT ( 'NONE',  ( 78.77321854994620765, 47.95351654967443977, 20.00000000000000000 ) ) ;
#18900 = ADVANCED_FACE ( 'NONE', ( #32001 ), #33377, .F. ) ;
#18901 = VECTOR ( 'NONE', #42742, 1000.000000000000000 ) ;
#18902 = ORIENTED_EDGE ( 'NONE', *, *, #7251, .T. ) ;
#18903 = CARTESIAN_POINT ( 'NONE',  ( -30.00000000000000000, -14.33999999999999986, 14.50000000000000000 ) ) ;
#18904 = CARTESIAN_POINT ( 'NONE',  ( -7.250000000000000888, 8.250000000000001776, -12.00000000000000000 ) ) ;
#18905 = DIRECTION ( 'NONE',  ( -1.000000000000000000, 1.280238727658158432E-15, 0.000000000000000000 ) ) ;
#18906 = ORIENTED_EDGE ( 'NONE', *, *, #50945, .T. ) ;
#18907 = AXIS2_PLACEMENT_3D ( 'NONE', #13029, #56188, #23999 ) ;
#18908 = AXIS2_PLACEMENT_3D ( 'NONE', #19670, #20387, #36298 ) ;
#18909 = AXIS2_PLACEMENT_3D ( 'NONE', #48303, #27426, #69515 ) ;
#18910 = LINE ( 'NONE', #51434, #9887 ) ;
#18911 = CARTESIAN_POINT ( 'NONE',  ( -15.50000000000000000, -0.2000000000000000111, 22.50000000000000000 ) ) ;
#18912 = AXIS2_PLACEMENT_3D ( 'NONE', #60142, #11696, #6415 ) ;
#18913 = AXIS2_PLACEMENT_3D ( 'NONE', #28355, #16034, #466 ) ;
#18914 = PRODUCT_DEFINITION_FORMATION_WITH_SPECIFIED_SOURCE ( 'ANY', '', #6975, .NOT_KNOWN. ) ;
#18915 = ORIENTED_EDGE ( 'NONE', *, *, #991, .F. ) ;
#18916 = DIRECTION ( 'NONE',  ( -0.4999999999999695244, 0.8660254037844562491, 0.000000000000000000 ) ) ;
#18917 = CARTESIAN_POINT ( 'NONE',  ( 37.90000000000000568, 20.60000000000000142, -13.86939075806900057 ) ) ;
#18918 = DIRECTION ( 'NONE',  ( 0.000000000000000000, 1.000000000000000000, 0.000000000000000000 ) ) ;
#18919 = CIRCLE ( 'NONE', #66364, 1.224999999999999423 ) ;
#18920 = DIRECTION ( 'NONE',  ( -0.000000000000000000, -0.000000000000000000, -1.000000000000000000 ) ) ;
#18921 = AXIS2_PLACEMENT_3D ( 'NONE', #58616, #20080, #63209 ) ;
#18922 = DIRECTION ( 'NONE',  ( 0.000000000000000000, 0.000000000000000000, 1.000000000000000000 ) ) ;
#18923 = ORIENTED_EDGE ( 'NONE', *, *, #26534, .F. ) ;
#18924 = CARTESIAN_POINT ( 'NONE',  ( -2.893516549646673930, 11.11351654964657598, 195.0000000000000284 ) ) ;
#18925 = FACE_OUTER_BOUND ( 'NONE', #24329, .T. ) ;
#18926 = CARTESIAN_POINT ( 'NONE',  ( 12.90000000000000213, -0.1999999999911430404, -8.864436962241481021E-12 ) ) ;
#18927 = CARTESIAN_POINT ( 'NONE',  ( -14.25000000000000000, -2.500000000000000000, 21.77831216351300014 ) ) ;
#18928 = ADVANCED_FACE ( 'NONE', ( #27035 ), #69826, .T. ) ;
#18929 = CARTESIAN_POINT ( 'NONE',  ( -8.697938382363135545, 8.079219948824830411, 26.00000000000000711 ) ) ;
#18930 = ORIENTED_EDGE ( 'NONE', *, *, #47319, .F. ) ;
#18932 = ORIENTED_EDGE ( 'NONE', *, *, #786, .T. ) ;
#18931 = CARTESIAN_POINT ( 'NONE',  ( 29.89999999999999858, 0.000000000000000000, 0.000000000000000000 ) ) ;
#18933 = VECTOR ( 'NONE', #62815, 1000.000000000000000 ) ;
#18934 = CARTESIAN_POINT ( 'NONE',  ( 10.50702373788277910, 3.650476262117147375, 26.00000000000000711 ) ) ;
#18935 = CARTESIAN_POINT ( 'NONE',  ( 6.884529946162100345, -21.00000000000000000, 0.000000000000000000 ) ) ;
#18937 = ORIENTED_EDGE ( 'NONE', *, *, #22222, .T. ) ;
#18936 = EDGE_CURVE ( 'NONE', #40026, #10730, #42942, .T. ) ;
#18938 = CARTESIAN_POINT ( 'NONE',  ( 38.90000000000000568, -21.00000000000000000, 13.86939075806900057 ) ) ;
#18939 = EDGE_CURVE ( 'NONE', #44299, #67897, #11791, .T. ) ;
#18940 = EDGE_LOOP ( 'NONE', ( #67020, #3108, #5674, #20386 ) ) ;
#18941 = EDGE_CURVE ( 'NONE', #54968, #56561, #43650, .T. ) ;
#18942 = CYLINDRICAL_SURFACE ( 'NONE', #60560, 2.458500000000000796 ) ;
#18943 = ORIENTED_EDGE ( 'NONE', *, *, #7618, .F. ) ;
#18944 = VERTEX_POINT ( 'NONE', #48952 ) ;
#18945 = CARTESIAN_POINT ( 'NONE',  ( -9.547976262117254365, 8.130476262117182884, 26.00000000000000711 ) ) ;
#18946 = FACE_OUTER_BOUND ( 'NONE', #44125, .T. ) ;
#18947 = FACE_OUTER_BOUND ( 'NONE', #19424, .T. ) ;
#18948 = DIRECTION ( 'NONE',  ( 0.000000000000000000, 0.000000000000000000, 1.000000000000000000 ) ) ;
#18949 = ADVANCED_FACE ( 'NONE', ( #33028 ), #48260, .F. ) ;
#18950 = AXIS2_PLACEMENT_3D ( 'NONE', #17087, #48581, #5798 ) ;
#18951 = ORIENTED_EDGE ( 'NONE', *, *, #42927, .T. ) ;
#18952 = ORIENTED_EDGE ( 'NONE', *, *, #185, .F. ) ;
#18953 = DIRECTION ( 'NONE',  ( 0.000000000000000000, 0.000000000000000000, -1.000000000000000000 ) ) ;
#18954 = DIRECTION ( 'NONE',  ( -1.000000000000000000, 0.000000000000000000, 0.000000000000000000 ) ) ;
#18955 = VERTEX_POINT ( 'NONE', #59213 ) ;
#18956 = ORIENTED_EDGE ( 'NONE', *, *, #6122, .F. ) ;
#18957 = ORIENTED_EDGE ( 'NONE', *, *, #45027, .T. ) ;
#18958 = CARTESIAN_POINT ( 'NONE',  ( 7.806483450353379538, -11.32648345035348925, 455.0000000000000568 ) ) ;
#18959 = ADVANCED_FACE ( 'NONE', ( #10762 ), #16080, .F. ) ;
#18961 = EDGE_LOOP ( 'NONE', ( #20530, #3894, #59569, #16509, #18205, #37124 ) ) ;
#18960 = LINE ( 'NONE', #34508, #16840 ) ;
#18962 = ADVANCED_FACE ( 'NONE', ( #66243 ), #45706, .F. ) ;
#18963 = AXIS2_PLACEMENT_3D ( 'NONE', #49111, #5301, #22587 ) ;
#18964 = DIRECTION ( 'NONE',  ( 1.000000000000000000, 0.000000000000000000, 0.000000000000000000 ) ) ;
#18965 = PLANE ( 'NONE',  #39670 ) ;
#18966 = EDGE_LOOP ( 'NONE', ( #53589, #16179, #55117, #23798 ) ) ;
#18967 = ORIENTED_EDGE ( 'NONE', *, *, #39286, .F. ) ;
#18968 = VECTOR ( 'NONE', #51927, 1000.000000000000000 ) ;
#18969 = AXIS2_PLACEMENT_3D ( 'NONE', #45107, #61725, #30261 ) ;
#18970 = CARTESIAN_POINT ( 'NONE',  ( 106.4257688009193430, 0.000000000000000000, 327.4830310981789694 ) ) ;
#18971 = PLANE ( 'NONE',  #18879 ) ;
#18972 = DIRECTION ( 'NONE',  ( -1.000000000000000000, 0.000000000000000000, 0.000000000000000000 ) ) ;
#18973 = AXIS2_PLACEMENT_3D ( 'NONE', #21428, #5869, #561 ) ;
#18974 = FACE_OUTER_BOUND ( 'NONE', #62317, .T. ) ;
#18975 = LINE ( 'NONE', #52198, #50498 ) ;
#18976 = EDGE_LOOP ( 'NONE', ( #23454, #67288, #66419, #69226, #28833, #37233 ) ) ;
#18977 = ORIENTED_EDGE ( 'NONE', *, *, #13541, .F. ) ;
#18978 = CARTESIAN_POINT ( 'NONE',  ( 10.50702373788281996, -6.849523737882823760, 54.00000000000000711 ) ) ;
#18979 = LINE ( 'NONE', #3078, #44790 ) ;
#18980 = CYLINDRICAL_SURFACE ( 'NONE', #10477, 25.39999999999999858 ) ;
#18981 = CYLINDRICAL_SURFACE ( 'NONE', #12160, 0.2000000000000005107 ) ;
#18982 = EDGE_CURVE ( 'NONE', #20667, #26162, #49313, .T. ) ;
#18983 = DIRECTION ( 'NONE',  ( 0.000000000000000000, 0.000000000000000000, -1.000000000000000000 ) ) ;
#18984 = VERTEX_POINT ( 'NONE', #65888 ) ;
#18985 = CARTESIAN_POINT ( 'NONE',  ( 275.0000000000000000, -38.10000000000000142, 8.400000000000000355 ) ) ;
#18986 = CARTESIAN_POINT ( 'NONE',  ( 7.450000000000003730, -7.249999999999997335, -23.50000000000000000 ) ) ;
#18987 = DIRECTION ( 'NONE',  ( 0.000000000000000000, 0.000000000000000000, 1.000000000000000000 ) ) ;
#18988 = EDGE_CURVE ( 'NONE', #35354, #62970, #13538, .T. ) ;
#18989 = LINE ( 'NONE', #56126, #59406 ) ;
#18990 = CIRCLE ( 'NONE', #58544, 3.300000002979700753 ) ;
#18991 = CARTESIAN_POINT ( 'NONE',  ( 11.18999999999999950, -11.18999999999999950, -4.250000000000000000 ) ) ;
#18992 = LINE ( 'NONE', #2722, #51072 ) ;
#18993 = ADVANCED_FACE ( 'NONE', ( #39366 ), #49971, .F. ) ;
#18994 = LINE ( 'NONE', #3437, #63478 ) ;
#18995 = VERTEX_POINT ( 'NONE', #66929 ) ;
#18996 = FACE_OUTER_BOUND ( 'NONE', #41795, .T. ) ;
#18997 = ADVANCED_FACE ( 'NONE', ( #23803 ), #17449, .F. ) ;
#18998 = FACE_OUTER_BOUND ( 'NONE', #16231, .T. ) ;
#18999 = VERTEX_POINT ( 'NONE', #35095 ) ;
#19000 = CARTESIAN_POINT ( 'NONE',  ( -29.25000000000000000, -5.200000000000001066, 26.25000000000000000 ) ) ;
#19001 = CYLINDRICAL_SURFACE ( 'NONE', #52540, 24.99999999998794920 ) ;
#19002 = LINE ( 'NONE', #1687, #1583 ) ;
#19003 = ADVANCED_FACE ( 'NONE', ( #33715 ), #40043, .F. ) ;
#19004 = DIRECTION ( 'NONE',  ( -1.836970198721029934E-16, 1.836970198721036344E-16, -1.000000000000000000 ) ) ;
#19005 = EDGE_LOOP ( 'NONE', ( #31958, #51655, #2221, #36114, #30356, #34769, #16979, #62050 ) ) ;
#19006 = AXIS2_PLACEMENT_3D ( 'NONE', #20414, #35977, #41980 ) ;
#19007 = LINE ( 'NONE', #46568, #8158 ) ;
#19008 = EDGE_LOOP ( 'NONE', ( #62854, #51867, #31363, #63193 ) ) ;
#19009 = DIRECTION ( 'NONE',  ( 1.060575238724893480E-16, 0.5000000000000189848, -0.8660254037844277164 ) ) ;
#19010 = CARTESIAN_POINT ( 'NONE',  ( 17.00000000000000000, -15.50000000000000000, -19.33772233983200195 ) ) ;
#19012 = ORIENTED_EDGE ( 'NONE', *, *, #39519, .T. ) ;
#19011 = EDGE_CURVE ( 'NONE', #61131, #50332, #44656, .T. ) ;
#19013 = LINE ( 'NONE', #17619, #32609 ) ;
#19014 = EDGE_CURVE ( 'NONE', #61781, #992, #7534, .T. ) ;
#19015 = AXIS2_PLACEMENT_3D ( 'NONE', #3144, #8066, #2431 ) ;
#19016 = ORIENTED_EDGE ( 'NONE', *, *, #26809, .T. ) ;
#19017 = ADVANCED_FACE ( 'NONE', ( #29108 ), #50670, .T. ) ;
#19018 = ADVANCED_FACE ( 'NONE', ( #6832 ), #23459, .T. ) ;
#19019 = DIRECTION ( 'NONE',  ( 0.000000000000000000, 0.000000000000000000, 1.000000000000000000 ) ) ;
#19020 = ORIENTED_EDGE ( 'NONE', *, *, #28975, .F. ) ;
#19021 = ORIENTED_EDGE ( 'NONE', *, *, #17407, .T. ) ;
#19022 = PLANE ( 'NONE',  #54311 ) ;
#19023 = ORIENTED_EDGE ( 'NONE', *, *, #57002, .T. ) ;
#19024 = ORIENTED_EDGE ( 'NONE', *, *, #6772, .T. ) ;
#19025 = EDGE_CURVE ( 'NONE', #61277, #26426, #59447, .T. ) ;
#19026 = CIRCLE ( 'NONE', #3233, 5.200000000000009948 ) ;
#19027 = PRODUCT_DEFINITION_CONTEXT ( 'detailed design', #9255, 'design' ) ;
#19028 = DIRECTION ( 'NONE',  ( 0.000000000000000000, 1.000000000000000000, 0.000000000000000000 ) ) ;
#19029 = CARTESIAN_POINT ( 'NONE',  ( -7.250000000000000888, 7.250000000000001776, -26.00000000000001066 ) ) ;
#19030 = DIRECTION ( 'NONE',  ( 0.000000000000000000, -3.673940397442059868E-16, 1.000000000000000000 ) ) ;
#19031 = VERTEX_POINT ( 'NONE', #8228 ) ;
#19032 = CARTESIAN_POINT ( 'NONE',  ( -10.49297626211729551, -6.849523737882748264, 54.00000000000000711 ) ) ;
#19034 = DIRECTION ( 'NONE',  ( -1.000000000000000000, 0.000000000000000000, 0.000000000000000000 ) ) ;
#19033 = CARTESIAN_POINT ( 'NONE',  ( 7.450000000000003730, -7.249999999999997335, -17.50000000000000000 ) ) ;
#19035 = VERTEX_POINT ( 'NONE', #45011 ) ;
#19037 = ORIENTED_EDGE ( 'NONE', *, *, #47050, .T. ) ;
#19036 = FACE_OUTER_BOUND ( 'NONE', #63739, .T. ) ;
#19038 = VERTEX_POINT ( 'NONE', #49633 ) ;
#19039 = SHAPE_DEFINITION_REPRESENTATION ( #29445, #1995 ) ;
#19040 = CARTESIAN_POINT ( 'NONE',  ( -7.744988412222944874, -8.465062094116097668, 455.0000000000000568 ) ) ;
#19041 = EDGE_CURVE ( 'NONE', #65847, #45123, #17805, .T. ) ;
#19042 = EDGE_LOOP ( 'NONE', ( #4878, #10901, #29927, #50408, #12287, #15410, #29089, #25849 ) ) ;
#19043 = ADVANCED_FACE ( 'NONE', ( #61262 ), #60925, .F. ) ;
#19044 = CARTESIAN_POINT ( 'NONE',  ( 7.000000000000000000, -26.42999999999999972, 5.874955318979029784 ) ) ;
#19045 = PLANE ( 'NONE',  #68924 ) ;
#19046 = ORIENTED_EDGE ( 'NONE', *, *, #38153, .F. ) ;
#19047 = ORIENTED_EDGE ( 'NONE', *, *, #49810, .T. ) ;
#19048 = CARTESIAN_POINT ( 'NONE',  ( 7.000000000000000000, -28.95000000000155183, 14.49999999999845990 ) ) ;
#19049 = LINE ( 'NONE', #52278, #4098 ) ;
#19050 = EDGE_LOOP ( 'NONE', ( #26505, #730, #16965, #60515 ) ) ;
#19051 = CIRCLE ( 'NONE', #42786, 0.06000000000000102474 ) ;
#19052 = DIRECTION ( 'NONE',  ( 1.000000000000000000, 0.000000000000000000, 0.000000000000000000 ) ) ;
#19053 = CARTESIAN_POINT ( 'NONE',  ( 8.900000000000005684, -21.00000000000000355, 14.57806571531352269 ) ) ;
#19054 = CARTESIAN_POINT ( 'NONE',  ( -3.842976262117332453, -10.31452373788281740, 54.00000000000000711 ) ) ;
#19055 = ORIENTED_EDGE ( 'NONE', *, *, #22780, .F. ) ;
#19056 = CIRCLE ( 'NONE', #62004, 1.000000000000000888 ) ;
#19057 = CARTESIAN_POINT ( 'NONE',  ( 275.0000000000000000, -38.65000000000095781, 13.20000000000094253 ) ) ;
#19058 = DIRECTION ( 'NONE',  ( -1.901462112903060228E-14, -1.000000000000000000, 0.000000000000000000 ) ) ;
#19060 = VERTEX_POINT ( 'NONE', #55632 ) ;
#19059 = DIRECTION ( 'NONE',  ( 1.836970198721029934E-16, 1.836970198721010706E-16, -1.000000000000000000 ) ) ;
#19062 = VERTEX_POINT ( 'NONE', #7175 ) ;
#19061 = DIRECTION ( 'NONE',  ( 0.000000000000000000, -1.000000000000000000, 0.000000000000000000 ) ) ;
#19063 = DIRECTION ( 'NONE',  ( -1.000000000000000000, 0.000000000000000000, 0.000000000000000000 ) ) ;
#19064 = VECTOR ( 'NONE', #62366, 1000.000000000000114 ) ;
#19065 = CYLINDRICAL_SURFACE ( 'NONE', #9321, 0.1999999999999987899 ) ;
#19066 = CYLINDRICAL_SURFACE ( 'NONE', #57291, 4.000000000000000000 ) ;
#19067 = PLANE ( 'NONE',  #67781 ) ;
#19068 = AXIS2_PLACEMENT_3D ( 'NONE', #54512, #15639, #10324 ) ;
#19069 = CARTESIAN_POINT ( 'NONE',  ( 3.677663764522603795, 6.350872789121277506, 26.00000000000000711 ) ) ;
#19070 = EDGE_LOOP ( 'NONE', ( #39448, #47236, #28120, #23043, #5066, #11272, #63297, #46383 ) ) ;
#19071 = CARTESIAN_POINT ( 'NONE',  ( 11.00000000000000000, -13.79999999999979998, 17.30000000000000071 ) ) ;
#19072 = FACE_OUTER_BOUND ( 'NONE', #20600, .T. ) ;
#19073 = DIRECTION ( 'NONE',  ( 2.990116172375847553E-15, 1.000000000000000000, 0.000000000000000000 ) ) ;
#19074 = CIRCLE ( 'NONE', #12288, 0.1749999999999998224 ) ;
#19075 = ADVANCED_FACE ( 'NONE', ( #66586 ), #12823, .F. ) ;
#19077 = VERTEX_POINT ( 'NONE', #3993 ) ;
#19076 = DIRECTION ( 'NONE',  ( 1.000000000000000000, -0.000000000000000000, -0.000000000000000000 ) ) ;
#19078 = DIRECTION ( 'NONE',  ( -0.000000000000000000, 3.673940397442059868E-16, -1.000000000000000000 ) ) ;
#19079 = CARTESIAN_POINT ( 'NONE',  ( 283.0000000000000568, -32.45000000000000995, -15.00000000000000000 ) ) ;
#19080 = EDGE_CURVE ( 'NONE', #17399, #35347, #6395, .T. ) ;
#19081 = VECTOR ( 'NONE', #50195, 1000.000000000000000 ) ;
#19082 = ORIENTED_EDGE ( 'NONE', *, *, #57067, .T. ) ;
#19083 = ORIENTED_EDGE ( 'NONE', *, *, #40375, .F. ) ;
#19084 = LINE ( 'NONE', #40647, #61384 ) ;
#19085 = EDGE_CURVE ( 'NONE', #1911, #54119, #25206, .T. ) ;
#19086 = LINE ( 'NONE', #24743, #65602 ) ;
#19087 = EDGE_CURVE ( 'NONE', #3375, #56472, #1838, .T. ) ;
#19088 = ORIENTED_EDGE ( 'NONE', *, *, #16391, .F. ) ;
#19089 = CARTESIAN_POINT ( 'NONE',  ( 49.00000000000000000, 20.60000000000000142, -13.86939075806900057 ) ) ;
#19090 = CARTESIAN_POINT ( 'NONE',  ( 1.480523737882788238, -9.404523737882783507, 26.00000000000000000 ) ) ;
#19091 = EDGE_CURVE ( 'NONE', #1819, #48505, #57021, .T. ) ;
#19092 = EDGE_CURVE ( 'NONE', #33736, #21660, #16545, .T. ) ;
#19093 = DIRECTION ( 'NONE',  ( 2.135044278125299371E-15, 1.000000000000000000, 0.000000000000000000 ) ) ;
#19094 = DIRECTION ( 'NONE',  ( 0.000000000000000000, 0.000000000000000000, -1.000000000000000000 ) ) ;
#19095 = ORIENTED_EDGE ( 'NONE', *, *, #39943, .F. ) ;
#19096 = CARTESIAN_POINT ( 'NONE',  ( 30.00000000000000000, -11.70000000000000284, -11.00000000000000000 ) ) ;
#19097 = ORIENTED_EDGE ( 'NONE', *, *, #4359, .F. ) ;
#19098 = ORIENTED_EDGE ( 'NONE', *, *, #69128, .F. ) ;
#19099 = DIRECTION ( 'NONE',  ( -1.000000000000000000, 0.000000000000000000, 0.000000000000000000 ) ) ;
#19100 = VECTOR ( 'NONE', #44211, 1000.000000000000000 ) ;
#19101 = PLANE ( 'NONE',  #20847 ) ;
#19102 = DIRECTION ( 'NONE',  ( 1.000000000000000000, 0.000000000000000000, 0.000000000000000000 ) ) ;
#19103 = ORIENTED_EDGE ( 'NONE', *, *, #39358, .T. ) ;
#19104 = ORIENTED_EDGE ( 'NONE', *, *, #38579, .F. ) ;
#19105 = CARTESIAN_POINT ( 'NONE',  ( -11.07551654964667520, 11.47551654964660450, 455.0000000000000568 ) ) ;
#19106 = VERTEX_POINT ( 'NONE', #30156 ) ;
#19107 = CONICAL_SURFACE ( 'NONE', #36018, 1.621000000000000885, 0.7853981633974518317 ) ;
#19108 = EDGE_LOOP ( 'NONE', ( #22196, #5483, #3379, #24518 ) ) ;
#19109 = DIRECTION ( 'NONE',  ( -0.7071067811865474617, 0.7071067811865474617, 2.597868168706479611E-16 ) ) ;
#19110 = CARTESIAN_POINT ( 'NONE',  ( -7.250000000000000888, 8.250000000000001776, -24.50000000000000000 ) ) ;
#19111 = DIRECTION ( 'NONE',  ( 1.000000000000000000, -7.665540703601094997E-15, -2.816273965919649962E-30 ) ) ;
#19112 = DIRECTION ( 'NONE',  ( 0.000000000000000000, 0.000000000000000000, -1.000000000000000000 ) ) ;
#19113 = VERTEX_POINT ( 'NONE', #51731 ) ;
#19114 = CIRCLE ( 'NONE', #11190, 0.5000000000001386669 ) ;
#19115 = DIRECTION ( 'NONE',  ( -1.000000000000000000, 0.000000000000000000, 0.000000000000000000 ) ) ;
#19117 = DIRECTION ( 'NONE',  ( -1.000000000000000000, 1.047444401652940007E-14, -1.836970198721010706E-16 ) ) ;
#19116 = CYLINDRICAL_SURFACE ( 'NONE', #29838, 0.2000000000000005107 ) ;
#19118 = ORIENTED_EDGE ( 'NONE', *, *, #6556, .F. ) ;
#19120 = ORIENTED_EDGE ( 'NONE', *, *, #4014, .F. ) ;
#19119 = CYLINDRICAL_SURFACE ( 'NONE', #35232, 1.000000000000000000 ) ;
#19121 = EDGE_LOOP ( 'NONE', ( #56648, #4108, #50102, #35789, #58111 ) ) ;
#19122 = VERTEX_POINT ( 'NONE', #51369 ) ;
#19123 = AXIS2_PLACEMENT_3D ( 'NONE', #66542, #42980, #39327 ) ;
#19124 = PLANE ( 'NONE',  #43443 ) ;
#19125 = CIRCLE ( 'NONE', #7804, 0.5000000000001357803 ) ;
#19126 = EDGE_CURVE ( 'NONE', #22770, #18604, #68338, .T. ) ;
#19127 = DIRECTION ( 'NONE',  ( -1.000000000000000000, 0.000000000000000000, 0.000000000000000000 ) ) ;
#19128 = EDGE_LOOP ( 'NONE', ( #24157, #62609, #41163, #33609, #54901, #19443 ) ) ;
#19129 = ORIENTED_EDGE ( 'NONE', *, *, #25845, .F. ) ;
#19130 = EDGE_CURVE ( 'NONE', #5311, #50275, #3285, .T. ) ;
#19131 = CIRCLE ( 'NONE', #11253, 0.1999999999999987899 ) ;
#19132 = FACE_OUTER_BOUND ( 'NONE', #41040, .T. ) ;
#19133 = CARTESIAN_POINT ( 'NONE',  ( 15.50000000000000000, -2.500000000000000000, 23.94337567297399971 ) ) ;
#19134 = EDGE_LOOP ( 'NONE', ( #62746, #52941, #983, #61208 ) ) ;
#19135 = ORIENTED_EDGE ( 'NONE', *, *, #21743, .F. ) ;
#19136 = DIRECTION ( 'NONE',  ( 0.000000000000000000, 1.000000000000000000, 0.000000000000000000 ) ) ;
#19137 = DIRECTION ( 'NONE',  ( -1.000000000000000000, 0.000000000000000000, 0.000000000000000000 ) ) ;
#19138 = ORIENTED_EDGE ( 'NONE', *, *, #34493, .T. ) ;
#19139 = CARTESIAN_POINT ( 'NONE',  ( 9.804883450353456098, 11.07551654964653132, 455.0000000000000568 ) ) ;
#19140 = VECTOR ( 'NONE', #57307, 1000.000000000000000 ) ;
#19141 = LINE ( 'NONE', #51315, #49747 ) ;
#19143 = EDGE_LOOP ( 'NONE', ( #55731, #63420, #1396, #62329 ) ) ;
#19142 = DIRECTION ( 'NONE',  ( 0.7071067811865527908, 0.7071067811865422437, 2.597868168706460875E-16 ) ) ;
#19144 = ORIENTED_EDGE ( 'NONE', *, *, #48799, .T. ) ;
#19145 = CARTESIAN_POINT ( 'NONE',  ( -11.11351654964671098, 4.193516549646605363, 455.0000000000000568 ) ) ;
#19146 = CYLINDRICAL_SURFACE ( 'NONE', #49356, 0.2000000000000005107 ) ;
#19147 = LINE ( 'NONE', #57679, #50995 ) ;
#19148 = CARTESIAN_POINT ( 'NONE',  ( 5.257023737882819070, -7.186223737882813545, 26.00000000000000000 ) ) ;
#19149 = DIRECTION ( 'NONE',  ( 0.000000000000000000, 1.000000000000000000, 0.000000000000000000 ) ) ;
#19150 = CARTESIAN_POINT ( 'NONE',  ( 33.89999999999999858, -14.06939075806902117, -20.80000000000000426 ) ) ;
#19151 = CARTESIAN_POINT ( 'NONE',  ( -6.642976262117334940, -10.31452373788278898, 54.00000000000000711 ) ) ;
#19152 = ORIENTED_EDGE ( 'NONE', *, *, #48607, .T. ) ;
#19153 = DIRECTION ( 'NONE',  ( 0.000000000000000000, 0.5000000000000189848, 0.8660254037844277164 ) ) ;
#19154 = VECTOR ( 'NONE', #28314, 1000.000000000000000 ) ;
#19155 = AXIS2_PLACEMENT_3D ( 'NONE', #42077, #31135, #9921 ) ;
#19156 = ADVANCED_BREP_SHAPE_REPRESENTATION ( '', ( #66174, #44181, #66857, #43035, #19195, #65828, #19540, #21524, #43959, #42462, #43380, #42921, #19898, #44638, #20709, #43848, #43151, #67216, #42807, #67800, #42691, #67577, #44406, #66294, #20943, #43268, #44878, #45918 ), #55023 ) ;
#19158 = VERTEX_POINT ( 'NONE', #46413 ) ;
#19157 = CYLINDRICAL_SURFACE ( 'NONE', #38974, 0.1999999999999996503 ) ;
#19159 = EDGE_CURVE ( 'NONE', #19378, #22473, #3014, .T. ) ;
#19160 = DIRECTION ( 'NONE',  ( -1.000000000000000000, 0.000000000000000000, 0.000000000000000000 ) ) ;
#19161 = FACE_OUTER_BOUND ( 'NONE', #13617, .T. ) ;
#19162 = CARTESIAN_POINT ( 'NONE',  ( -11.77351654964674665, -7.826483450353317828, 195.0000000000000284 ) ) ;
#19163 = DIRECTION ( 'NONE',  ( -1.000000000000000000, 2.602085213965213008E-15, 0.000000000000000000 ) ) ;
#19164 = CIRCLE ( 'NONE', #58706, 2.250000000000001776 ) ;
#19165 = CARTESIAN_POINT ( 'NONE',  ( 1.690483450353367889, 9.828310488885986018, 195.0000000000000284 ) ) ;
#19166 = VERTEX_POINT ( 'NONE', #24854 ) ;
#19167 = DIRECTION ( 'NONE',  ( 0.000000000000000000, -3.673940397442059868E-16, 1.000000000000000000 ) ) ;
#19168 = CARTESIAN_POINT ( 'NONE',  ( -3.593516549646790015, -7.428221114745077180, 455.0000000000000568 ) ) ;
#19169 = ORIENTED_EDGE ( 'NONE', *, *, #66090, .F. ) ;
#19170 = VECTOR ( 'NONE', #60822, 1000.000000000000000 ) ;
#19171 = LINE ( 'NONE', #35070, #38151 ) ;
#19172 = EDGE_CURVE ( 'NONE', #7800, #67429, #12020, .T. ) ;
#19173 = EDGE_CURVE ( 'NONE', #41194, #56308, #21081, .T. ) ;
#19174 = VECTOR ( 'NONE', #29778, 1000.000000000000000 ) ;
#19175 = FACE_OUTER_BOUND ( 'NONE', #29721, .T. ) ;
#19176 = EDGE_CURVE ( 'NONE', #3811, #49314, #9294, .T. ) ;
#19177 = EDGE_LOOP ( 'NONE', ( #20159, #58074, #33055, #23288 ) ) ;
#19178 = DIRECTION ( 'NONE',  ( -0.8660254037850523279, 0.000000000000000000, -0.4999999999989371835 ) ) ;
#19179 = ORIENTED_EDGE ( 'NONE', *, *, #27978, .T. ) ;
#19180 = VERTEX_POINT ( 'NONE', #35805 ) ;
#19181 = CARTESIAN_POINT ( 'NONE',  ( 69.92576880110368620, 10.00000000000000000, 281.4830310981151911 ) ) ;
#19182 = AXIS2_PLACEMENT_3D ( 'NONE', #36925, #15697, #58495 ) ;
#19183 = LINE ( 'NONE', #35431, #2635 ) ;
#19184 = CARTESIAN_POINT ( 'NONE',  ( 146.5599459900709860, 0.000000000000000000, 276.7801873289890295 ) ) ;
#19185 = CARTESIAN_POINT ( 'NONE',  ( 7.250000000000005329, -7.249999999999998224, -26.00000000000001066 ) ) ;
#19186 = CARTESIAN_POINT ( 'NONE',  ( -30.00000000000000000, -16.64230188589299786, -14.64519951917100116 ) ) ;
#19187 = ORIENTED_EDGE ( 'NONE', *, *, #48811, .F. ) ;
#19188 = ORIENTED_EDGE ( 'NONE', *, *, #38889, .T. ) ;
#19190 = EDGE_LOOP ( 'NONE', ( #55050, #52740, #41487, #42977 ) ) ;
#19189 = DIRECTION ( 'NONE',  ( -0.000000000000000000, -0.000000000000000000, -1.000000000000000000 ) ) ;
#19191 = ORIENTED_EDGE ( 'NONE', *, *, #56623, .T. ) ;
#19192 = CARTESIAN_POINT ( 'NONE',  ( 19.90000000000000213, -21.00000000000001421, -13.86939075806900945 ) ) ;
#19193 = CARTESIAN_POINT ( 'NONE',  ( 10.92648345035340895, 9.293516549646565039, 455.0000000000000568 ) ) ;
#19194 = DIRECTION ( 'NONE',  ( -1.000000000000000000, 0.000000000000000000, 0.000000000000000000 ) ) ;
#19195 = MANIFOLD_SOLID_BREP ( 'LPattern1[5]', #12582 ) ;
#19196 = CIRCLE ( 'NONE', #66633, 0.2000000000000005107 ) ;
#19197 = LINE ( 'NONE', #47469, #16151 ) ;
#19198 = FILL_AREA_STYLE ('',( #13543 ) ) ;
#19199 = CARTESIAN_POINT ( 'NONE',  ( 0.000000000000000000, 8.250000000000001776, -21.50000000000000000 ) ) ;
#19200 = ORIENTED_EDGE ( 'NONE', *, *, #17125, .F. ) ;
#19201 = ORIENTED_EDGE ( 'NONE', *, *, #36521, .T. ) ;
#19202 = ORIENTED_EDGE ( 'NONE', *, *, #56149, .T. ) ;
#19203 = ORIENTED_EDGE ( 'NONE', *, *, #56623, .F. ) ;
#19204 = LINE ( 'NONE', #7883, #31051 ) ;
#19205 = CARTESIAN_POINT ( 'NONE',  ( 6.344579767990823349, -8.406483450353491094, 455.0000000000000568 ) ) ;
#19206 = AXIS2_PLACEMENT_3D ( 'NONE', #37649, #1205, #17448 ) ;
#19207 = SHAPE_REPRESENTATION_RELATIONSHIP ( 'NONE' , 'NONE' ,  #15926, #52879 ) ;
#19208 = CARTESIAN_POINT ( 'NONE',  ( 9.404523737882819034, -0.9555237378828257411, 54.00000000000000711 ) ) ;
#19209 = VECTOR ( 'NONE', #52147, 1000.000000000000114 ) ;
#19210 = ORIENTED_EDGE ( 'NONE', *, *, #41391, .F. ) ;
#19211 = ORIENTED_EDGE ( 'NONE', *, *, #50785, .F. ) ;
#19212 = VERTEX_POINT ( 'NONE', #16200 ) ;
#19213 = EDGE_CURVE ( 'NONE', #67306, #48721, #26739, .T. ) ;
#19214 = AXIS2_PLACEMENT_3D ( 'NONE', #62450, #24292, #40193 ) ;
#19215 = EDGE_CURVE ( 'NONE', #49394, #48512, #61746, .T. ) ;
#19216 = ADVANCED_FACE ( 'NONE', ( #58648 ), #51687, .T. ) ;
#19217 = CARTESIAN_POINT ( 'NONE',  ( 13.00000000000000178, -16.28999999999999915, -14.50000000000000000 ) ) ;
#19218 = VERTEX_POINT ( 'NONE', #53692 ) ;
#19219 = ORIENTED_EDGE ( 'NONE', *, *, #7613, .F. ) ;
#19220 = DIRECTION ( 'NONE',  ( 1.000000000000000000, 0.000000000000000000, 0.000000000000000000 ) ) ;
#19221 = ADVANCED_FACE ( 'NONE', ( #24808 ), #4560, .F. ) ;
#19222 = ORIENTED_EDGE ( 'NONE', *, *, #41543, .F. ) ;
#19223 = CIRCLE ( 'NONE', #3422, 0.1999999999999987899 ) ;
#19224 = ORIENTED_EDGE ( 'NONE', *, *, #15122, .T. ) ;
#19225 = DIRECTION ( 'NONE',  ( 1.000000000000000000, -0.000000000000000000, 0.000000000000000000 ) ) ;
#19227 = VERTEX_POINT ( 'NONE', #3240 ) ;
#19226 = CARTESIAN_POINT ( 'NONE',  ( -5.380658396643267949, -4.747751991980631026, 195.0000000000000284 ) ) ;
#19228 = EDGE_LOOP ( 'NONE', ( #45279, #68571, #52224, #3021 ) ) ;
#19229 = VECTOR ( 'NONE', #29692, 1000.000000000000000 ) ;
#19230 = CARTESIAN_POINT ( 'NONE',  ( -7.250000000000000000, -7.449999999999998401, -17.50000000000000000 ) ) ;
#19231 = LINE ( 'NONE', #13922, #6960 ) ;
#19232 = CARTESIAN_POINT ( 'NONE',  ( 49.00000000000000000, -21.00000000000000000, 13.86939075806900057 ) ) ;
#19234 = ORIENTED_EDGE ( 'NONE', *, *, #11975, .F. ) ;
#19233 = CARTESIAN_POINT ( 'NONE',  ( 283.0000000000000568, -26.50000000000000000, 0.5000000000000000000 ) ) ;
#19235 = ORIENTED_EDGE ( 'NONE', *, *, #5398, .T. ) ;
#19236 = AXIS2_PLACEMENT_3D ( 'NONE', #35055, #36111, #24101 ) ;
#19237 = AXIS2_PLACEMENT_3D ( 'NONE', #69838, #28091, #16444 ) ;
#19238 = DIRECTION ( 'NONE',  ( 1.047444401652940007E-14, 1.000000000000000000, 1.836970198721029934E-16 ) ) ;
#19239 = CARTESIAN_POINT ( 'NONE',  ( -7.450000000000001954, 7.250000000000000000, -9.000000000000001776 ) ) ;
#19240 = DIRECTION ( 'NONE',  ( 0.000000000000000000, 1.000000000000000000, 0.000000000000000000 ) ) ;
#19241 = ORIENTED_EDGE ( 'NONE', *, *, #69634, .F. ) ;
#19242 = DIRECTION ( 'NONE',  ( -1.000000000000000000, 0.000000000000000000, 0.000000000000000000 ) ) ;
#19243 = FACE_OUTER_BOUND ( 'NONE', #13470, .T. ) ;
#19244 = FACE_OUTER_BOUND ( 'NONE', #2728, .T. ) ;
#19245 = AXIS2_PLACEMENT_3D ( 'NONE', #65159, #42877, #66773 ) ;
#19246 = ORIENTED_EDGE ( 'NONE', *, *, #35295, .T. ) ;
#19247 = CARTESIAN_POINT ( 'NONE',  ( 11.00000000000000000, -10.85999999999999943, -9.000000000000001776 ) ) ;
#19248 = CARTESIAN_POINT ( 'NONE',  ( 6.849523737882817542, -10.50702373788282529, 54.00000000000000711 ) ) ;
#19249 = FACE_OUTER_BOUND ( 'NONE', #18218, .T. ) ;
#19250 = ORIENTED_EDGE ( 'NONE', *, *, #26200, .F. ) ;
#19251 = AXIS2_PLACEMENT_3D ( 'NONE', #37865, #5357, #4990 ) ;
#19252 = CARTESIAN_POINT ( 'NONE',  ( 3.157023737882819425, -4.046023737882825877, 54.00000000000000711 ) ) ;
#19253 = CIRCLE ( 'NONE', #50836, 0.3999999999993817390 ) ;
#19254 = CARTESIAN_POINT ( 'NONE',  ( -14.25000000000000000, -2.500000000000000000, -23.22168783648699986 ) ) ;
#19255 = ADVANCED_FACE ( 'NONE', ( #62276 ), #36728, .F. ) ;
#19256 = VECTOR ( 'NONE', #42463, 1000.000000000000000 ) ;
#19257 = ADVANCED_FACE ( 'NONE', ( #37428 ), #19146, .F. ) ;
#19258 = ORIENTED_EDGE ( 'NONE', *, *, #33987, .T. ) ;
#19259 = DIRECTION ( 'NONE',  ( 0.000000000000000000, 0.000000000000000000, 1.000000000000000000 ) ) ;
#19260 = PLANE ( 'NONE',  #36571 ) ;
#19261 = EDGE_CURVE ( 'NONE', #46721, #65971, #13842, .T. ) ;
#19262 = LINE ( 'NONE', #7940, #31967 ) ;
#19263 = CARTESIAN_POINT ( 'NONE',  ( 10.31889768521803319, -25.34729925119248861, -17.15270074880751494 ) ) ;
#19264 = CARTESIAN_POINT ( 'NONE',  ( 8.250000000000005329, 0.000000000000000000, -17.50000000000000000 ) ) ;
#19265 = ORIENTED_EDGE ( 'NONE', *, *, #16709, .F. ) ;
#19266 = CARTESIAN_POINT ( 'NONE',  ( -7.342976262117282715, -5.552858015815545834, 54.00000000000000711 ) ) ;
#19267 = DIRECTION ( 'NONE',  ( -1.000000000000000000, -0.000000000000000000, -0.000000000000000000 ) ) ;
#19268 = EDGE_CURVE ( 'NONE', #34611, #46340, #19968, .T. ) ;
#19269 = DIRECTION ( 'NONE',  ( -0.000000000000000000, 0.000000000000000000, 1.000000000000000000 ) ) ;
#19270 = PRODUCT_RELATED_PRODUCT_CATEGORY ( 'part', '', ( #49892 ) ) ;
#19271 = VECTOR ( 'NONE', #30585, 1000.000000000000000 ) ;
#19272 =( NAMED_UNIT ( * ) PLANE_ANGLE_UNIT ( ) SI_UNIT ( $, .RADIAN. ) );
#19273 = EDGE_CURVE ( 'NONE', #32281, #40788, #46365, .T. ) ;
#19274 = DIRECTION ( 'NONE',  ( -1.000000000000000000, 0.000000000000000000, 0.000000000000000000 ) ) ;
#19275 = ORIENTED_EDGE ( 'NONE', *, *, #49299, .F. ) ;
#19277 = ORIENTED_EDGE ( 'NONE', *, *, #51890, .F. ) ;
#19276 = DIRECTION ( 'NONE',  ( 1.000000000000000000, -0.000000000000000000, 0.000000000000000000 ) ) ;
#19278 = ADVANCED_FACE ( 'NONE', ( #54044 ), #43533, .T. ) ;
#19279 = VECTOR ( 'NONE', #7171, 1000.000000000000000 ) ;
#19280 = DIRECTION ( 'NONE',  ( 0.000000000000000000, -1.000000000000000000, 0.000000000000000000 ) ) ;
#19281 = CARTESIAN_POINT ( 'NONE',  ( 40.90000000000000568, 20.60000000000000142, 13.86939075806900057 ) ) ;
#19282 = CARTESIAN_POINT ( 'NONE',  ( 25.50000000000000355, -15.12100000000000044, 22.50000000000000000 ) ) ;
#19283 = ORIENTED_EDGE ( 'NONE', *, *, #42574, .T. ) ;
#19284 = LINE ( 'NONE', #61350, #29555 ) ;
#19285 = ORIENTED_EDGE ( 'NONE', *, *, #61633, .T. ) ;
#19286 = EDGE_LOOP ( 'NONE', ( #9639, #56450, #67583, #20009 ) ) ;
#19287 = ORIENTED_EDGE ( 'NONE', *, *, #53113, .T. ) ;
#19288 = DIRECTION ( 'NONE',  ( -1.836970198721029934E-16, -1.836970198721010706E-16, 1.000000000000000000 ) ) ;
#19289 = DIRECTION ( 'NONE',  ( 1.000000000000000000, -0.000000000000000000, 0.000000000000000000 ) ) ;
#19290 = CARTESIAN_POINT ( 'NONE',  ( -5.242976262117259978, 7.172176262117182510, 26.00000000000000711 ) ) ;
#19291 = DIRECTION ( 'NONE',  ( 0.000000000000000000, 0.000000000000000000, 1.000000000000000000 ) ) ;
#19292 = ORIENTED_EDGE ( 'NONE', *, *, #31772, .T. ) ;
#19293 = ORIENTED_EDGE ( 'NONE', *, *, #21032, .F. ) ;
#19294 = CARTESIAN_POINT ( 'NONE',  ( 15.91434062215687284, -0.3156604612129197962, 21.29584399676445727 ) ) ;
#19295 = CYLINDRICAL_SURFACE ( 'NONE', #54236, 24.99999999998784972 ) ;
#19296 = VERTEX_POINT ( 'NONE', #26125 ) ;
#19297 = ORIENTED_EDGE ( 'NONE', *, *, #20020, .T. ) ;
#19298 = VERTEX_POINT ( 'NONE', #5595 ) ;
#19299 = CARTESIAN_POINT ( 'NONE',  ( 7.250000000000004441, 7.450000000000001954, -12.50000000000000000 ) ) ;
#19301 = ORIENTED_EDGE ( 'NONE', *, *, #56446, .T. ) ;
#19300 = CARTESIAN_POINT ( 'NONE',  ( 181.4833316329832940, 9.000000000000001776, 276.7801873289890295 ) ) ;
#19302 = CARTESIAN_POINT ( 'NONE',  ( -10.19191654964671301, 11.07551654964660415, 455.0000000000000568 ) ) ;
#19303 = DIRECTION ( 'NONE',  ( 3.016910393003147986E-15, -1.000000000000000000, 0.000000000000000000 ) ) ;
#19304 = MANIFOLD_SOLID_BREP ( 'Cut-Extrude1', #8095 ) ;
#19305 = ORIENTED_EDGE ( 'NONE', *, *, #49266, .F. ) ;
#19306 = AXIS2_PLACEMENT_3D ( 'NONE', #16584, #58676, #31467 ) ;
#19307 = VERTEX_POINT ( 'NONE', #39483 ) ;
#19308 = EDGE_CURVE ( 'NONE', #56028, #26101, #1757, .T. ) ;
#19309 = VECTOR ( 'NONE', #39015, 1000.000000000000000 ) ;
#19310 = AXIS2_PLACEMENT_3D ( 'NONE', #53315, #26786, #22172 ) ;
#19311 = PLANE ( 'NONE',  #66518 ) ;
#19312 = CYLINDRICAL_SURFACE ( 'NONE', #34660, 24.99999999998789946 ) ;
#19313 = EDGE_CURVE ( 'NONE', #14048, #5488, #62872, .T. ) ;
#19314 = CARTESIAN_POINT ( 'NONE',  ( 8.250000000000005329, -7.249999999999998224, -26.00000000000001066 ) ) ;
#19315 = AXIS2_PLACEMENT_3D ( 'NONE', #46406, #14585, #57718 ) ;
#19316 = AXIS2_PLACEMENT_3D ( 'NONE', #8440, #61853, #30019 ) ;
#19317 = CARTESIAN_POINT ( 'NONE',  ( 30.00000000000000000, -13.54524521594299991, 17.53999999999999915 ) ) ;
#19318 = DIRECTION ( 'NONE',  ( 1.073876437509453175E-14, 1.000000000000000000, 0.000000000000000000 ) ) ;
#19320 = VERTEX_POINT ( 'NONE', #38795 ) ;
#19319 = DIRECTION ( 'NONE',  ( 0.000000000000000000, 0.000000000000000000, -1.000000000000000000 ) ) ;
#19321 = ORIENTED_EDGE ( 'NONE', *, *, #58543, .F. ) ;
#19322 = LINE ( 'NONE', #8723, #24185 ) ;
#19323 = CARTESIAN_POINT ( 'NONE',  ( 46.39999999999999858, 33.00000000000000000, -2.250000000000000444 ) ) ;
#19324 = VECTOR ( 'NONE', #53893, 1000.000000000000000 ) ;
#19325 = LINE ( 'NONE', #40888, #65793 ) ;
#19326 = LINE ( 'NONE', #6966, #47165 ) ;
#19327 = EDGE_CURVE ( 'NONE', #51399, #33655, #9841, .T. ) ;
#19328 = LINE ( 'NONE', #40893, #39853 ) ;
#19329 = ORIENTED_EDGE ( 'NONE', *, *, #28658, .T. ) ;
#19330 = CARTESIAN_POINT ( 'NONE',  ( 106.4257688009193998, 10.00000000000000000, 285.9830310981789125 ) ) ;
#19331 = CARTESIAN_POINT ( 'NONE',  ( -4.173516549646669738, 11.77351654964658678, 455.0000000000000568 ) ) ;
#19332 = CARTESIAN_POINT ( 'NONE',  ( -7.750000000000001776, 7.750000000000001776, 0.000000000000000000 ) ) ;
#19333 = EDGE_CURVE ( 'NONE', #21794, #68853, #12603, .T. ) ;
#19334 = CARTESIAN_POINT ( 'NONE',  ( 9.750000000000001776, 9.690000000000001279, -5.000000000000000000 ) ) ;
#19335 = PLANE ( 'NONE',  #22906 ) ;
#19336 = DIRECTION ( 'NONE',  ( 0.000000000000000000, 0.000000000000000000, 1.000000000000000000 ) ) ;
#19337 = ORIENTED_EDGE ( 'NONE', *, *, #6841, .T. ) ;
#19338 = CARTESIAN_POINT ( 'NONE',  ( 14.25000000000000000, -0.2038245569916330158, 23.22168783648699986 ) ) ;
#19339 = PLANE ( 'NONE',  #65509 ) ;
#19340 = ORIENTED_EDGE ( 'NONE', *, *, #7197, .T. ) ;
#19341 = CARTESIAN_POINT ( 'NONE',  ( 6.364920264886884560, 6.822336235477388655, 26.00000000000000711 ) ) ;
#19342 = DIRECTION ( 'NONE',  ( 0.5773502691896257311, -0.5773502691896257311, -0.5773502691896257311 ) ) ;
#19343 = DIRECTION ( 'NONE',  ( 1.000000000000000000, -5.626525616968433909E-15, -1.836970198721040534E-16 ) ) ;
#19344 = SURFACE_STYLE_FILL_AREA ( #25013 ) ;
#19345 = EDGE_CURVE ( 'NONE', #3591, #6350, #61579, .T. ) ;
#19346 = DIRECTION ( 'NONE',  ( -1.000000000000000000, 0.000000000000000000, 0.000000000000000000 ) ) ;
#19347 = AXIS2_PLACEMENT_3D ( 'NONE', #41148, #20983, #9332 ) ;
#19348 = ORIENTED_EDGE ( 'NONE', *, *, #34222, .T. ) ;
#19349 = ADVANCED_FACE ( 'NONE', ( #60014 ), #11563, .T. ) ;
#19350 = LINE ( 'NONE', #62472, #17202 ) ;
#19351 = AXIS2_PLACEMENT_3D ( 'NONE', #43496, #37176, #42465 ) ;
#19352 = ORIENTED_EDGE ( 'NONE', *, *, #12452, .F. ) ;
#19353 = DIRECTION ( 'NONE',  ( 0.000000000000000000, 0.000000000000000000, -1.000000000000000000 ) ) ;
#19354 = CARTESIAN_POINT ( 'NONE',  ( 6.849523737882817542, -10.31452373788282095, 54.00000000000000711 ) ) ;
#19355 = ORIENTED_EDGE ( 'NONE', *, *, #59192, .T. ) ;
#19356 = CARTESIAN_POINT ( 'NONE',  ( -11.00000000000000000, -12.00000000000000000, -10.20500000000000007 ) ) ;
#19357 = ADVANCED_FACE ( 'NONE', ( #17916 ), #48725, .F. ) ;
#19358 = VERTEX_POINT ( 'NONE', #54382 ) ;
#19359 = AXIS2_PLACEMENT_3D ( 'NONE', #41802, #36872, #63379 ) ;
#19360 = VECTOR ( 'NONE', #32154, 1000.000000000000000 ) ;
#19361 = CARTESIAN_POINT ( 'NONE',  ( 41.09999999999999432, -0.2000000000000000111, 0.000000000000000000 ) ) ;
#19362 = ORIENTED_EDGE ( 'NONE', *, *, #67721, .F. ) ;
#19363 = ORIENTED_EDGE ( 'NONE', *, *, #2364, .T. ) ;
#19364 = CARTESIAN_POINT ( 'NONE',  ( -3.834182069070763976, 7.517976262117170627, 26.00000000000000711 ) ) ;
#19365 = EDGE_LOOP ( 'NONE', ( #29343, #5789, #42875, #9276, #23476, #40914, #15294, #15569, #29198, #27690, #67492, #20700, #11029, #10105, #66456 ) ) ;
#19366 = VECTOR ( 'NONE', #21296, 1000.000000000000114 ) ;
#19367 = ORIENTED_EDGE ( 'NONE', *, *, #13986, .T. ) ;
#19368 = DIRECTION ( 'NONE',  ( -1.000000000000000000, 0.000000000000000000, 0.000000000000000000 ) ) ;
#19369 = CARTESIAN_POINT ( 'NONE',  ( -10.30047626211729472, -6.849523737882750929, 54.00000000000000711 ) ) ;
#19370 = CYLINDRICAL_SURFACE ( 'NONE', #37818, 0.1749999999999998224 ) ;
#19371 = ORIENTED_EDGE ( 'NONE', *, *, #60277, .T. ) ;
#19372 = CARTESIAN_POINT ( 'NONE',  ( 7.000000000000000000, -23.70411739045900390, -12.50000000000000000 ) ) ;
#19373 = VECTOR ( 'NONE', #62291, 1000.000000000000000 ) ;
#19375 = LINE ( 'NONE', #13723, #22065 ) ;
#19374 = PLANE ( 'NONE',  #13472 ) ;
#19376 = ORIENTED_EDGE ( 'NONE', *, *, #42005, .T. ) ;
#19378 = VERTEX_POINT ( 'NONE', #65677 ) ;
#19377 = DIRECTION ( 'NONE',  ( 1.000000000000000000, -0.000000000000000000, 0.000000000000000000 ) ) ;
#19379 = ORIENTED_EDGE ( 'NONE', *, *, #4674, .F. ) ;
#19380 = ADVANCED_FACE ( 'NONE', ( #55756 ), #7301, .T. ) ;
#19381 = APPLICATION_PROTOCOL_DEFINITION ( 'draft international standard', 'automotive_design', 1998, #40428 ) ;
#19382 = CARTESIAN_POINT ( 'NONE',  ( -4.609516549646703432, -3.606483450353393572, 195.0000000000000284 ) ) ;
#19384 = ORIENTED_EDGE ( 'NONE', *, *, #631, .F. ) ;
#19383 = DIRECTION ( 'NONE',  ( -1.000000000000000000, 0.000000000000000000, -0.000000000000000000 ) ) ;
#19385 = EDGE_CURVE ( 'NONE', #8573, #24168, #60352, .T. ) ;
#19386 = DIRECTION ( 'NONE',  ( -1.000000000000000000, 0.000000000000000000, 0.000000000000000000 ) ) ;
#19387 = LINE ( 'NONE', #25055, #47468 ) ;
#19388 = VERTEX_POINT ( 'NONE', #33498 ) ;
#19389 = VERTEX_POINT ( 'NONE', #55084 ) ;
#19390 = EDGE_CURVE ( 'NONE', #68564, #56334, #28193, .T. ) ;
#19391 = EDGE_CURVE ( 'NONE', #25525, #61414, #28528, .T. ) ;
#19392 = CARTESIAN_POINT ( 'NONE',  ( 3.664523737882814824, 10.30047626211720768, 26.00000000000000711 ) ) ;
#19393 = VERTEX_POINT ( 'NONE', #45130 ) ;
#19394 = DIRECTION ( 'NONE',  ( 0.000000000000000000, 0.000000000000000000, 1.000000000000000000 ) ) ;
#19395 = CARTESIAN_POINT ( 'NONE',  ( 8.900000000000005684, -21.00000000000000000, -14.57806571531351914 ) ) ;
#19396 = ADVANCED_FACE ( 'NONE', ( #18974 ), #46533, .T. ) ;
#19397 = DIRECTION ( 'NONE',  ( 0.9375000000000006661, 0.000000000000000000, 0.3479852726768744020 ) ) ;
#19398 = CIRCLE ( 'NONE', #66784, 1.449999999999999956 ) ;
#19399 = ORIENTED_EDGE ( 'NONE', *, *, #65792, .T. ) ;
#19400 = CARTESIAN_POINT ( 'NONE',  ( 15.50000000000000000, -0.2038245569916604938, -21.05662432702600029 ) ) ;
#19401 = DIRECTION ( 'NONE',  ( 1.000000000000000000, -0.000000000000000000, 0.000000000000000000 ) ) ;
#19402 = EDGE_CURVE ( 'NONE', #37065, #22759, #27896, .T. ) ;
#19404 = ORIENTED_EDGE ( 'NONE', *, *, #66701, .T. ) ;
#19403 = CARTESIAN_POINT ( 'NONE',  ( 41.09999999999999432, -14.06939075806901940, -20.80000000000000426 ) ) ;
#19406 = EDGE_LOOP ( 'NONE', ( #55967, #41903, #56883, #34430 ) ) ;
#19405 = DIRECTION ( 'NONE',  ( -1.000000000000000000, -1.671920889371702854E-15, -0.000000000000000000 ) ) ;
#19407 = EDGE_CURVE ( 'NONE', #44232, #46800, #56792, .T. ) ;
#19408 = DIRECTION ( 'NONE',  ( 0.000000000000000000, 1.000000000000000000, 0.000000000000000000 ) ) ;
#19409 = CARTESIAN_POINT ( 'NONE',  ( 8.930623737882818602, -8.580623737882856261, 54.00000000000000711 ) ) ;
#19410 = ADVANCED_FACE ( 'NONE', ( #2014 ), #30290, .F. ) ;
#19411 = FACE_OUTER_BOUND ( 'NONE', #15421, .T. ) ;
#19413 = EDGE_CURVE ( 'NONE', #20669, #42591, #67416, .T. ) ;
#19412 = VECTOR ( 'NONE', #33794, 1000.000000000000000 ) ;
#19414 = ADVANCED_FACE ( 'NONE', ( #67758 ), #61386, .F. ) ;
#19415 = AXIS2_PLACEMENT_3D ( 'NONE', #18931, #19276, #45087 ) ;
#19416 = CARTESIAN_POINT ( 'NONE',  ( 41.09999999999999432, -14.06939075806901940, -20.80000000000000426 ) ) ;
#19417 = CYLINDRICAL_SURFACE ( 'NONE', #45465, 0.1999999999999996503 ) ;
#19418 = ORIENTED_EDGE ( 'NONE', *, *, #12218, .F. ) ;
#19419 = DIRECTION ( 'NONE',  ( -0.000000000000000000, -0.000000000000000000, -1.000000000000000000 ) ) ;
#19420 = CARTESIAN_POINT ( 'NONE',  ( 7.000000000000000000, -37.15000000000001279, -7.700000000000000178 ) ) ;
#19421 = EDGE_CURVE ( 'NONE', #43665, #18078, #12951, .T. ) ;
#19422 = DIRECTION ( 'NONE',  ( 0.000000000000000000, 0.000000000000000000, -1.000000000000000000 ) ) ;
#19424 = EDGE_LOOP ( 'NONE', ( #18690, #63538, #59304, #11682 ) ) ;
#19423 = DIRECTION ( 'NONE',  ( 0.000000000000000000, -1.000000000000000000, -8.396061623720747815E-13 ) ) ;
#19425 = CARTESIAN_POINT ( 'NONE',  ( 4.155633711806658859, -5.793274621760842180, 54.00000000000000711 ) ) ;
#19426 = EDGE_CURVE ( 'NONE', #56509, #32175, #8349, .T. ) ;
#19427 = DIRECTION ( 'NONE',  ( -1.000000000000000000, 0.000000000000000000, 0.000000000000000000 ) ) ;
#19428 = AXIS2_PLACEMENT_3D ( 'NONE', #44906, #18022, #6394 ) ;
#19429 = EDGE_LOOP ( 'NONE', ( #15073, #14934, #45698, #48379 ) ) ;
#19430 = ORIENTED_EDGE ( 'NONE', *, *, #46098, .T. ) ;
#19431 = DIRECTION ( 'NONE',  ( -1.000000000000000000, 0.000000000000000000, 0.000000000000000000 ) ) ;
#19432 = DIRECTION ( 'NONE',  ( -0.7071067811865550112, -0.7071067811865401342, -2.597868168706466299E-16 ) ) ;
#19433 = ORIENTED_EDGE ( 'NONE', *, *, #26376, .F. ) ;
#19434 = DIRECTION ( 'NONE',  ( 1.000000000000000000, 0.000000000000000000, 0.000000000000000000 ) ) ;
#19435 = DIRECTION ( 'NONE',  ( 0.8660254037844482555, 0.000000000000000000, 0.4999999999999831801 ) ) ;
#19436 = ADVANCED_FACE ( 'NONE', ( #7656 ), #23924, .T. ) ;
#19437 = PLANE ( 'NONE',  #16907 ) ;
#19438 = ADVANCED_FACE ( 'NONE', ( #45479 ), #13663, .F. ) ;
#19439 = CARTESIAN_POINT ( 'NONE',  ( 30.00000000000000000, -11.50000000000100009, -15.00000000000084910 ) ) ;
#19440 = ORIENTED_EDGE ( 'NONE', *, *, #15449, .T. ) ;
#19441 = CARTESIAN_POINT ( 'NONE',  ( -11.00000000000000000, -14.04000000000000092, 17.04524521594300523 ) ) ;
#19442 = EDGE_LOOP ( 'NONE', ( #3173, #61125, #60514, #23026 ) ) ;
#19443 = ORIENTED_EDGE ( 'NONE', *, *, #46777, .T. ) ;
#19444 = ORIENTED_EDGE ( 'NONE', *, *, #6335, .T. ) ;
#19445 = DIRECTION ( 'NONE',  ( 0.000000000000000000, 0.000000000000000000, -1.000000000000000000 ) ) ;
#19446 = AXIS2_PLACEMENT_3D ( 'NONE', #1310, #43049, #60001 ) ;
#19447 = DIRECTION ( 'NONE',  ( 1.000000000000000000, -0.000000000000000000, -0.000000000000000000 ) ) ;
#19448 = CARTESIAN_POINT ( 'NONE',  ( 30.00000000000000000, -17.00000000000000000, -15.70499999999969809 ) ) ;
#19449 = ORIENTED_EDGE ( 'NONE', *, *, #63032, .F. ) ;
#19450 = EDGE_LOOP ( 'NONE', ( #33484, #52885, #37638, #26643 ) ) ;
#19451 = PLANE ( 'NONE',  #40869 ) ;
#19452 = ORIENTED_EDGE ( 'NONE', *, *, #12447, .T. ) ;
#19453 = ORIENTED_EDGE ( 'NONE', *, *, #47117, .F. ) ;
#19454 = DIRECTION ( 'NONE',  ( -0.000000000000000000, 3.673940397442059868E-16, -1.000000000000000000 ) ) ;
#19455 = LINE ( 'NONE', #51285, #9857 ) ;
#19456 = CYLINDRICAL_SURFACE ( 'NONE', #9553, 3.500000000000000000 ) ;
#19457 = DIRECTION ( 'NONE',  ( 0.000000000000000000, 0.000000000000000000, 1.000000000000000000 ) ) ;
#19458 = ORIENTED_EDGE ( 'NONE', *, *, #5937, .F. ) ;
#19459 = VECTOR ( 'NONE', #59829, 1000.000000000000000 ) ;
#19460 = DIRECTION ( 'NONE',  ( 1.000000000000000000, 0.000000000000000000, 0.000000000000000000 ) ) ;
#19462 = CYLINDRICAL_SURFACE ( 'NONE', #40096, 0.4999999999979551912 ) ;
#19461 = CARTESIAN_POINT ( 'NONE',  ( 3.157023737882796333, 5.242976262117212016, 26.00000000000000711 ) ) ;
#19463 = EDGE_LOOP ( 'NONE', ( #21635, #9873 ) ) ;
#19465 = EDGE_LOOP ( 'NONE', ( #13209, #25824, #32360, #16322 ) ) ;
#19464 = CARTESIAN_POINT ( 'NONE',  ( 10.31452373788280497, 6.642976262117183062, 54.00000000000000711 ) ) ;
#19466 = EDGE_LOOP ( 'NONE', ( #68746, #261, #26356, #33632, #31933, #54209, #58385, #10131 ) ) ;
#19467 = ORIENTED_EDGE ( 'NONE', *, *, #66513, .T. ) ;
#19468 = FACE_OUTER_BOUND ( 'NONE', #9167, .T. ) ;
#19469 = EDGE_CURVE ( 'NONE', #51221, #27077, #19659, .T. ) ;
#19470 = DIRECTION ( 'NONE',  ( 1.000000000000000000, 0.000000000000000000, 0.000000000000000000 ) ) ;
#19471 = CIRCLE ( 'NONE', #57883, 8.000000000000000000 ) ;
#19472 = ORIENTED_EDGE ( 'NONE', *, *, #63154, .F. ) ;
#19473 = ORIENTED_EDGE ( 'NONE', *, *, #29456, .F. ) ;
#19474 = EDGE_CURVE ( 'NONE', #48682, #51892, #40178, .T. ) ;
#19476 = CARTESIAN_POINT ( 'NONE',  ( -7.450000000000001954, -7.249999999999998224, -12.50000000000000000 ) ) ;
#19475 = AXIS2_PLACEMENT_3D ( 'NONE', #40393, #45685, #34030 ) ;
#19477 = EDGE_CURVE ( 'NONE', #61414, #41558, #61755, .T. ) ;
#19478 = CARTESIAN_POINT ( 'NONE',  ( 4.149127210878720717, 6.822336235477395761, 26.00000000000000711 ) ) ;
#19479 = ORIENTED_EDGE ( 'NONE', *, *, #55984, .F. ) ;
#19480 = ORIENTED_EDGE ( 'NONE', *, *, #17224, .F. ) ;
#19481 = DIRECTION ( 'NONE',  ( 1.000000000000000000, 0.000000000000000000, 0.000000000000000000 ) ) ;
#19482 = AXIS2_PLACEMENT_3D ( 'NONE', #42733, #65352, #17238 ) ;
#19483 = EDGE_CURVE ( 'NONE', #59231, #20701, #56444, .T. ) ;
#19484 = CARTESIAN_POINT ( 'NONE',  ( 283.0000000000000568, -38.15000000000000568, 14.50000000000000000 ) ) ;
#19485 = ORIENTED_EDGE ( 'NONE', *, *, #14059, .T. ) ;
#19486 = CARTESIAN_POINT ( 'NONE',  ( 25.50000000000000355, 0.000000000000000000, 20.87899999999999778 ) ) ;
#19487 = DIRECTION ( 'NONE',  ( 0.000000000000000000, 0.000000000000000000, 1.000000000000000000 ) ) ;
#19489 = VERTEX_POINT ( 'NONE', #62438 ) ;
#19488 = DIRECTION ( 'NONE',  ( 0.6414496315691617934, -0.7671651518152962090, -2.818519042763987834E-16 ) ) ;
#19490 = ORIENTED_EDGE ( 'NONE', *, *, #41195, .T. ) ;
#19491 = DIRECTION ( 'NONE',  ( 0.000000000000000000, 0.000000000000000000, 1.000000000000000000 ) ) ;
#19492 = DIRECTION ( 'NONE',  ( 0.000000000000000000, 1.000000000000000000, 0.000000000000000000 ) ) ;
#19493 = FACE_OUTER_BOUND ( 'NONE', #45813, .T. ) ;
#19494 = AXIS2_PLACEMENT_3D ( 'NONE', #15099, #62832, #53292 ) ;
#19495 = CARTESIAN_POINT ( 'NONE',  ( 25.90000000000000213, -21.00000000000000000, 13.86939075806900057 ) ) ;
#19496 = LINE ( 'NONE', #15618, #48217 ) ;
#19497 = EDGE_CURVE ( 'NONE', #278, #36973, #36793, .T. ) ;
#19498 = DIRECTION ( 'NONE',  ( 0.000000000000000000, 0.000000000000000000, -1.000000000000000000 ) ) ;
#19499 = LINE ( 'NONE', #24814, #21204 ) ;
#19500 = VECTOR ( 'NONE', #9074, 1000.000000000000000 ) ;
#19501 = ORIENTED_EDGE ( 'NONE', *, *, #21079, .F. ) ;
#19502 = CARTESIAN_POINT ( 'NONE',  ( 176.0064834503533575, -29.83962462487173894, 5.000000000000000000 ) ) ;
#19504 = ORIENTED_EDGE ( 'NONE', *, *, #12596, .F. ) ;
#19503 = CARTESIAN_POINT ( 'NONE',  ( -8.250000000000001776, 7.250000000000000888, -26.00000000000001066 ) ) ;
#19505 = CARTESIAN_POINT ( 'NONE',  ( 30.00000000000000000, -5.200000000000001066, -26.25000000000000000 ) ) ;
#19506 = CARTESIAN_POINT ( 'NONE',  ( 0.5000000000000000000, 0.000000000000000000, -26.50000000000000000 ) ) ;
#19507 = AXIS2_PLACEMENT_3D ( 'NONE', #36080, #9931, #25129 ) ;
#19508 = CARTESIAN_POINT ( 'NONE',  ( -17.24945551514599984, -15.50000000000000000, -25.53140320652400064 ) ) ;
#19509 = DIRECTION ( 'NONE',  ( 0.000000000000000000, -1.901256929667043247E-12, 1.000000000000000000 ) ) ;
#19510 = VERTEX_POINT ( 'NONE', #51856 ) ;
#19511 = CARTESIAN_POINT ( 'NONE',  ( 8.144523737882817471, -9.562023737882809016, 26.00000000000000000 ) ) ;
#19512 = CARTESIAN_POINT ( 'NONE',  ( -7.250000000000000888, -8.249999999999998224, -11.50000000000000000 ) ) ;
#19513 = ORIENTED_EDGE ( 'NONE', *, *, #38959, .T. ) ;
#19514 = CARTESIAN_POINT ( 'NONE',  ( 11.00000000000000000, -5.200000000000001066, -9.400000000000005684 ) ) ;
#19515 = ADVANCED_FACE ( 'NONE', ( #3412 ), #24980, .T. ) ;
#19516 = EDGE_CURVE ( 'NONE', #44316, #40017, #19857, .T. ) ;
#19517 = DIRECTION ( 'NONE',  ( -0.000000000000000000, 3.673940397442059868E-16, -1.000000000000000000 ) ) ;
#19518 = AXIS2_PLACEMENT_3D ( 'NONE', #53839, #21304, #69384 ) ;
#19519 = EDGE_LOOP ( 'NONE', ( #32042, #25225, #68147, #25589 ) ) ;
#19520 = PLANE ( 'NONE',  #28209 ) ;
#19521 = EDGE_LOOP ( 'NONE', ( #35765, #13354, #18469, #42523 ) ) ;
#19522 = ADVANCED_FACE ( 'NONE', ( #3758 ), #14724, .F. ) ;
#19523 = ORIENTED_EDGE ( 'NONE', *, *, #6677, .F. ) ;
#19524 = VECTOR ( 'NONE', #28133, 1000.000000000000000 ) ;
#19525 = LINE ( 'NONE', #24839, #29050 ) ;
#19526 = CARTESIAN_POINT ( 'NONE',  ( 10.00000000000000000, -18.00000000000000355, -21.00000000000000000 ) ) ;
#19527 = LINE ( 'NONE', #58068, #55903 ) ;
#19528 = CARTESIAN_POINT ( 'NONE',  ( -3.142976262117274988, -5.257023737882822623, 26.00000000000000711 ) ) ;
#19529 = VECTOR ( 'NONE', #56121, 1000.000000000000000 ) ;
#19530 = DIRECTION ( 'NONE',  ( 0.000000000000000000, -1.000000000000000000, 0.000000000000000000 ) ) ;
#19531 = VERTEX_POINT ( 'NONE', #15770 ) ;
#19532 = ORIENTED_EDGE ( 'NONE', *, *, #30133, .T. ) ;
#19534 = VERTEX_POINT ( 'NONE', #46887 ) ;
#19533 = CARTESIAN_POINT ( 'NONE',  ( -5.242976262117299946, -7.186223737882804663, 54.00000000000000711 ) ) ;
#19535 = ORIENTED_EDGE ( 'NONE', *, *, #52380, .F. ) ;
#19536 = DIRECTION ( 'NONE',  ( 0.000000000000000000, -1.000000000000000000, 0.000000000000000000 ) ) ;
#19537 = AXIS2_PLACEMENT_3D ( 'NONE', #38545, #6368, #27931 ) ;
#19538 = FACE_OUTER_BOUND ( 'NONE', #35454, .T. ) ;
#19539 = DIRECTION ( 'NONE',  ( -0.000000000000000000, -1.000000000000000000, -0.000000000000000000 ) ) ;
#19540 = MANIFOLD_SOLID_BREP ( 'LPattern1[7]', #27317 ) ;
#19541 = FACE_BOUND ( 'NONE', #38328, .T. ) ;
#19542 = CARTESIAN_POINT ( 'NONE',  ( -3.593516549646762481, -4.622483450353452206, 455.0000000000000568 ) ) ;
#19543 = CARTESIAN_POINT ( 'NONE',  ( 6.006483450353379716, -6.006483450353490738, 455.0000000000000568 ) ) ;
#19544 = AXIS2_PLACEMENT_3D ( 'NONE', #58519, #57445, #8998 ) ;
#19545 = VERTEX_POINT ( 'NONE', #4818 ) ;
#19546 = ORIENTED_EDGE ( 'NONE', *, *, #35026, .F. ) ;
#19547 = EDGE_LOOP ( 'NONE', ( #6325, #21469, #38271, #3237 ) ) ;
#19548 = ORIENTED_EDGE ( 'NONE', *, *, #10013, .T. ) ;
#19549 = CARTESIAN_POINT ( 'NONE',  ( -29.50000000000000355, -12.00000000000000000, -11.00000000000000000 ) ) ;
#19550 = VECTOR ( 'NONE', #25399, 1000.000000000000000 ) ;
#19551 = CARTESIAN_POINT ( 'NONE',  ( -17.51999999999999957, -17.50000000000000000, -26.00000000000000355 ) ) ;
#19552 = EDGE_CURVE ( 'NONE', #53664, #34294, #35643, .T. ) ;
#19553 = CARTESIAN_POINT ( 'NONE',  ( 14.25000000000000000, -0.2038245569916330158, -21.77831216351300014 ) ) ;
#19554 = VERTEX_POINT ( 'NONE', #52561 ) ;
#19555 = VERTEX_POINT ( 'NONE', #30635 ) ;
#19556 = ORIENTED_EDGE ( 'NONE', *, *, #59173, .F. ) ;
#19557 = ADVANCED_FACE ( 'NONE', ( #53612 ), #58911, .F. ) ;
#19558 = CARTESIAN_POINT ( 'NONE',  ( 8.900000000000005684, -0.2000000000000000111, 0.000000000000000000 ) ) ;
#19559 = ORIENTED_EDGE ( 'NONE', *, *, #69854, .T. ) ;
#19560 = ORIENTED_EDGE ( 'NONE', *, *, #56287, .F. ) ;
#19561 = EDGE_CURVE ( 'NONE', #49979, #62970, #39037, .T. ) ;
#19562 = CARTESIAN_POINT ( 'NONE',  ( 8.250000000000005329, 7.250000000000000888, -15.00000000000000000 ) ) ;
#19563 = EDGE_CURVE ( 'NONE', #6549, #5855, #25696, .T. ) ;
#19564 = ORIENTED_EDGE ( 'NONE', *, *, #8208, .F. ) ;
#19565 = ORIENTED_EDGE ( 'NONE', *, *, #44226, .F. ) ;
#19566 = CARTESIAN_POINT ( 'NONE',  ( 29.25000000000000000, -5.000000000000000000, 60.00000000000000000 ) ) ;
#19567 = ADVANCED_FACE ( 'NONE', ( #69861 ), #53268, .F. ) ;
#19568 = EDGE_CURVE ( 'NONE', #39415, #19811, #4475, .T. ) ;
#19570 = ORIENTED_EDGE ( 'NONE', *, *, #16149, .T. ) ;
#19569 = CARTESIAN_POINT ( 'NONE',  ( -8.250000000000001776, 7.250000000000000888, -26.00000000000001066 ) ) ;
#19571 = ORIENTED_EDGE ( 'NONE', *, *, #63115, .F. ) ;
#19572 = DIRECTION ( 'NONE',  ( 0.000000000000000000, -1.000000000000000000, 0.000000000000000000 ) ) ;
#19573 = VECTOR ( 'NONE', #757, 1000.000000000000000 ) ;
#19575 = CARTESIAN_POINT ( 'NONE',  ( -7.250000000000000888, -8.249999999999998224, -18.00000000000000000 ) ) ;
#19574 = VECTOR ( 'NONE', #6599, 1000.000000000000000 ) ;
#19576 = ADVANCED_FACE ( 'NONE', ( #63522 ), #36634, .T. ) ;
#19577 = CARTESIAN_POINT ( 'NONE',  ( 3.677663764522620227, 4.135079735113113664, 54.00000000000000711 ) ) ;
#19579 = ORIENTED_EDGE ( 'NONE', *, *, #50977, .T. ) ;
#19578 = DIRECTION ( 'NONE',  ( 0.000000000000000000, -1.000000000000000000, 0.000000000000000000 ) ) ;
#19581 = VERTEX_POINT ( 'NONE', #42639 ) ;
#19580 = AXIS2_PLACEMENT_3D ( 'NONE', #19961, #4420, #47539 ) ;
#19582 = LINE ( 'NONE', #3678, #67325 ) ;
#19583 = VECTOR ( 'NONE', #33098, 1000.000000000000000 ) ;
#19584 = VECTOR ( 'NONE', #20259, 1000.000000000000000 ) ;
#19585 = DIRECTION ( 'NONE',  ( 0.000000000000000000, -1.000000000000000000, 0.000000000000000000 ) ) ;
#19586 = LINE ( 'NONE', #18179, #40154 ) ;
#19587 = CARTESIAN_POINT ( 'NONE',  ( 9.804883450353379715, -10.20488345035343336, 195.0000000000000284 ) ) ;
#19588 = VECTOR ( 'NONE', #61388, 1000.000000000000114 ) ;
#19589 = VECTOR ( 'NONE', #28538, 1000.000000000000114 ) ;
#19590 = VERTEX_POINT ( 'NONE', #69165 ) ;
#19591 = DIRECTION ( 'NONE',  ( 0.000000000000000000, -0.9938079899998859545, 0.1111111111112941946 ) ) ;
#19592 = DIRECTION ( 'NONE',  ( 0.000000000000000000, 0.000000000000000000, 1.000000000000000000 ) ) ;
#19593 = CARTESIAN_POINT ( 'NONE',  ( 16.75000000000000000, -0.2038245569916320166, 23.22168783648699986 ) ) ;
#19594 = EDGE_LOOP ( 'NONE', ( #26955, #13428, #19283, #23591 ) ) ;
#19595 = DIRECTION ( 'NONE',  ( 1.062075597536821205E-14, 1.000000000000000000, 0.000000000000000000 ) ) ;
#19596 = DIRECTION ( 'NONE',  ( -1.000000000000000000, 0.000000000000000000, 0.000000000000000000 ) ) ;
#19597 = ORIENTED_EDGE ( 'NONE', *, *, #63152, .F. ) ;
#19598 = CARTESIAN_POINT ( 'NONE',  ( 11.50000000000000000, -11.50000000000100009, 10.50000000000065903 ) ) ;
#19599 = FACE_OUTER_BOUND ( 'NONE', #65757, .T. ) ;
#19600 = VERTEX_POINT ( 'NONE', #42285 ) ;
#19601 = DIRECTION ( 'NONE',  ( 0.7071067811865401342, -0.7071067811865550112, 0.000000000000000000 ) ) ;
#19602 = CARTESIAN_POINT ( 'NONE',  ( 283.0000000000000568, -42.50000000000000000, 10.20000000000000107 ) ) ;
#19603 = DIRECTION ( 'NONE',  ( 0.000000000000000000, 0.000000000000000000, -1.000000000000000000 ) ) ;
#19604 = EDGE_CURVE ( 'NONE', #15802, #28927, #33397, .T. ) ;
#19605 = EDGE_CURVE ( 'NONE', #13851, #35406, #59940, .T. ) ;
#19606 = CARTESIAN_POINT ( 'NONE',  ( 275.0000000000000000, -39.80000000000000426, 12.69999999999999929 ) ) ;
#19607 = CYLINDRICAL_SURFACE ( 'NONE', #8232, 4.000000000000000000 ) ;
#19608 = EDGE_LOOP ( 'NONE', ( #32850, #20967, #21119, #52821 ) ) ;
#19609 = DIRECTION ( 'NONE',  ( -1.084202172485504434E-16, 1.000000000000000000, 0.000000000000000000 ) ) ;
#19610 = DIRECTION ( 'NONE',  ( -1.000000000000000000, 0.000000000000000000, 0.000000000000000000 ) ) ;
#19611 = FACE_OUTER_BOUND ( 'NONE', #9871, .T. ) ;
#19612 = ADVANCED_FACE ( 'NONE', ( #48996 ), #27074, .T. ) ;
#19613 = FACE_OUTER_BOUND ( 'NONE', #6438, .T. ) ;
#19614 = ORIENTED_EDGE ( 'NONE', *, *, #19868, .T. ) ;
#19616 = ORIENTED_EDGE ( 'NONE', *, *, #39239, .T. ) ;
#19615 = FACE_OUTER_BOUND ( 'NONE', #15738, .T. ) ;
#19617 = CIRCLE ( 'NONE', #47841, 1.000000000000002665 ) ;
#19618 = AXIS2_PLACEMENT_3D ( 'NONE', #48274, #54620, #16785 ) ;
#19619 = DIRECTION ( 'NONE',  ( 0.000000000000000000, 0.000000000000000000, 1.000000000000000000 ) ) ;
#19620 = CARTESIAN_POINT ( 'NONE',  ( -9.722976262117258628, 6.817976262117182884, 54.00000000000000711 ) ) ;
#19621 = DIRECTION ( 'NONE',  ( 1.000000000000000000, 0.000000000000000000, 0.000000000000000000 ) ) ;
#19622 = ORIENTED_EDGE ( 'NONE', *, *, #42789, .T. ) ;
#19623 = CIRCLE ( 'NONE', #32057, 3.499999999999850342 ) ;
#19624 = CARTESIAN_POINT ( 'NONE',  ( 49.00000000000000000, 13.66939075806899950, 20.80000000000000426 ) ) ;
#19625 = VECTOR ( 'NONE', #56031, 1000.000000000000000 ) ;
#19626 = ORIENTED_EDGE ( 'NONE', *, *, #66183, .F. ) ;
#19628 = VERTEX_POINT ( 'NONE', #33071 ) ;
#19627 = VECTOR ( 'NONE', #45986, 1000.000000000000000 ) ;
#19629 = ORIENTED_EDGE ( 'NONE', *, *, #22845, .F. ) ;
#19630 = DIRECTION ( 'NONE',  ( 1.000000000000000000, -0.000000000000000000, 0.000000000000000000 ) ) ;
#19631 = DIRECTION ( 'NONE',  ( -0.000000000000000000, 3.673940397442059868E-16, -1.000000000000000000 ) ) ;
#19632 = DIRECTION ( 'NONE',  ( -1.000000000000000000, 0.000000000000000000, 0.000000000000000000 ) ) ;
#19633 = CYLINDRICAL_SURFACE ( 'NONE', #30284, 0.1999999999999987899 ) ;
#19634 = ORIENTED_EDGE ( 'NONE', *, *, #66081, .F. ) ;
#19635 = ORIENTED_EDGE ( 'NONE', *, *, #4171, .T. ) ;
#19636 = DIRECTION ( 'NONE',  ( -1.000000000000000000, 0.000000000000000000, 0.000000000000000000 ) ) ;
#19637 = AXIS2_PLACEMENT_3D ( 'NONE', #43901, #32616, #59131 ) ;
#19638 = CARTESIAN_POINT ( 'NONE',  ( 13.00000000000000178, -17.50000000000000000, 15.70499999999969809 ) ) ;
#19639 = VERTEX_POINT ( 'NONE', #17496 ) ;
#19640 = ORIENTED_EDGE ( 'NONE', *, *, #4600, .T. ) ;
#19641 = ORIENTED_EDGE ( 'NONE', *, *, #17570, .F. ) ;
#19642 = ORIENTED_EDGE ( 'NONE', *, *, #34273, .T. ) ;
#19643 = CARTESIAN_POINT ( 'NONE',  ( -7.394232575409605879, -3.724485858128642413, 54.00000000000000711 ) ) ;
#19644 = UNCERTAINTY_MEASURE_WITH_UNIT (LENGTH_MEASURE( 1.000000000000000082E-05 ), #53350, 'distance_accuracy_value', 'NONE');
#19645 = ADVANCED_FACE ( 'NONE', ( #28119 ), #22809, .T. ) ;
#19647 = VERTEX_POINT ( 'NONE', #54651 ) ;
#19646 = LINE ( 'NONE', #63848, #42390 ) ;
#19648 = PLANE ( 'NONE',  #68400 ) ;
#19649 = DIRECTION ( 'NONE',  ( 0.000000000000000000, 0.000000000000000000, -1.000000000000000000 ) ) ;
#19650 = EDGE_CURVE ( 'NONE', #19510, #19647, #60279, .T. ) ;
#19651 = ADVANCED_FACE ( 'NONE', ( #49681 ), #5517, .T. ) ;
#19652 = ORIENTED_EDGE ( 'NONE', *, *, #22333, .F. ) ;
#19653 = EDGE_LOOP ( 'NONE', ( #37744, #61852, #4802, #3575, #54648, #64193, #51632, #46445, #68950, #61640, #43036, #25027, #23109, #21412, #44512, #15875, #4676, #67447, #1438, #11002 ) ) ;
#19654 = CARTESIAN_POINT ( 'NONE',  ( -7.250000000000000000, -8.749999999999998224, -30.00000000000001066 ) ) ;
#19655 = FACE_OUTER_BOUND ( 'NONE', #13363, .T. ) ;
#19656 = EDGE_CURVE ( 'NONE', #29192, #53417, #62764, .T. ) ;
#19657 = VECTOR ( 'NONE', #50124, 1000.000000000000000 ) ;
#19658 = CIRCLE ( 'NONE', #2754, 0.2000000000000000944 ) ;
#19659 = LINE ( 'NONE', #29568, #59499 ) ;
#19660 = DIRECTION ( 'NONE',  ( -1.000000000000000000, 0.000000000000000000, 0.000000000000000000 ) ) ;
#19661 = CARTESIAN_POINT ( 'NONE',  ( -25.50000000000000355, 0.000000000000000000, 22.50000000000000000 ) ) ;
#19662 = ORIENTED_EDGE ( 'NONE', *, *, #42968, .T. ) ;
#19663 = CARTESIAN_POINT ( 'NONE',  ( 8.250000000000005329, 7.250000000000000888, -8.000000000000000000 ) ) ;
#19664 = DIRECTION ( 'NONE',  ( 1.000000000000000000, -0.000000000000000000, 0.000000000000000000 ) ) ;
#19665 = LINE ( 'NONE', #51151, #68064 ) ;
#19666 = FACE_OUTER_BOUND ( 'NONE', #24953, .T. ) ;
#19667 = VECTOR ( 'NONE', #41726, 1000.000000000000000 ) ;
#19668 = CARTESIAN_POINT ( 'NONE',  ( 4.747751991980615038, 5.380658396643156038, 195.0000000000000284 ) ) ;
#19669 = ORIENTED_EDGE ( 'NONE', *, *, #64147, .F. ) ;
#19670 = CARTESIAN_POINT ( 'NONE',  ( 7.000000000000000000, -25.69999999999924967, -14.52500000000000213 ) ) ;
#19671 = CARTESIAN_POINT ( 'NONE',  ( -11.50000000000000000, -12.00000000000000000, 11.00000000000000000 ) ) ;
#19672 = DIRECTION ( 'NONE',  ( 0.7071067811865486830, 0.7071067811865464625, 0.000000000000000000 ) ) ;
#19673 = PLANE ( 'NONE',  #45811 ) ;
#19674 = CARTESIAN_POINT ( 'NONE',  ( -11.11351654964670743, 2.893516549646604208, 195.0000000000000284 ) ) ;
#19675 = DIRECTION ( 'NONE',  ( 0.6414496315691494699, 0.7671651518153064231, 0.000000000000000000 ) ) ;
#19676 = VECTOR ( 'NONE', #20517, 1000.000000000000000 ) ;
#19677 = CARTESIAN_POINT ( 'NONE',  ( -2.893516549646675706, 10.91351654964657669, 455.0000000000000568 ) ) ;
#19678 = FACE_OUTER_BOUND ( 'NONE', #21376, .T. ) ;
#19679 = ORIENTED_EDGE ( 'NONE', *, *, #48709, .T. ) ;
#19680 = CARTESIAN_POINT ( 'NONE',  ( 14.45313394609757296, -0.2715358723599912150, 23.33896727494797929 ) ) ;
#19681 = CYLINDRICAL_SURFACE ( 'NONE', #23692, 0.5000000000009459100 ) ;
#19682 = EDGE_LOOP ( 'NONE', ( #23066, #67827, #65326, #20843 ) ) ;
#19683 = LINE ( 'NONE', #56821, #9767 ) ;
#19684 = DIRECTION ( 'NONE',  ( 0.5773502691896257311, -0.5773502691896257311, 0.5773502691896257311 ) ) ;
#19685 = EDGE_CURVE ( 'NONE', #49539, #12955, #17154, .T. ) ;
#19686 = DIRECTION ( 'NONE',  ( -0.000000000000000000, -0.000000000000000000, 1.000000000000000000 ) ) ;
#19687 = CARTESIAN_POINT ( 'NONE',  ( -7.172176262117259782, 5.242976262117182706, 26.00000000000000711 ) ) ;
#19688 = DIRECTION ( 'NONE',  ( 1.000000000000000000, 0.000000000000000000, 0.000000000000000000 ) ) ;
#19689 = VERTEX_POINT ( 'NONE', #53961 ) ;
#19690 = FACE_OUTER_BOUND ( 'NONE', #26815, .T. ) ;
#19691 = VERTEX_POINT ( 'NONE', #213 ) ;
#19692 = CARTESIAN_POINT ( 'NONE',  ( 11.00000000000000000, -9.199999999999999289, -12.69999999999986073 ) ) ;
#19693 = DIRECTION ( 'NONE',  ( 0.000000000000000000, 1.000000000000000000, 0.000000000000000000 ) ) ;
#19694 = ORIENTED_EDGE ( 'NONE', *, *, #34944, .T. ) ;
#19695 = AXIS2_PLACEMENT_3D ( 'NONE', #68606, #64010, #53739 ) ;
#19696 = DIRECTION ( 'NONE',  ( 0.000000000000000000, 0.000000000000000000, -1.000000000000000000 ) ) ;
#19697 = ADVANCED_FACE ( 'NONE', ( #1577 ), #554, .F. ) ;
#19698 = VECTOR ( 'NONE', #27105, 1000.000000000000000 ) ;
#19699 = VERTEX_POINT ( 'NONE', #22123 ) ;
#19700 = EDGE_CURVE ( 'NONE', #69920, #9064, #42431, .T. ) ;
#19701 = CARTESIAN_POINT ( 'NONE',  ( 39.90000000000000568, -0.1999999999911795112, 8.826273045769999343E-12 ) ) ;
#19702 = ORIENTED_EDGE ( 'NONE', *, *, #49073, .T. ) ;
#19703 = EDGE_LOOP ( 'NONE', ( #25318, #20962, #15527, #18751 ) ) ;
#19704 = CARTESIAN_POINT ( 'NONE',  ( 30.90000000000000213, 20.60000000000000142, 13.86939075806900057 ) ) ;
#19705 = EDGE_LOOP ( 'NONE', ( #28321, #12544, #29805, #26820 ) ) ;
#19706 = EDGE_LOOP ( 'NONE', ( #25263, #35504, #35188, #13003, #46589, #59041, #62212, #53928 ) ) ;
#19707 = DIRECTION ( 'NONE',  ( 0.000000000000000000, 0.000000000000000000, 1.000000000000000000 ) ) ;
#19708 = DIRECTION ( 'NONE',  ( 0.7071067811865411334, -0.7071067811865539010, -2.597868168706484541E-16 ) ) ;
#19709 = CIRCLE ( 'NONE', #5050, 0.3500000000009988455 ) ;
#19710 = VECTOR ( 'NONE', #30085, 1000.000000000000000 ) ;
#19711 = DIRECTION ( 'NONE',  ( 0.000000000000000000, 0.000000000000000000, 1.000000000000000000 ) ) ;
#19712 = ORIENTED_EDGE ( 'NONE', *, *, #66355, .T. ) ;
#19713 = CARTESIAN_POINT ( 'NONE',  ( 9.900000000000000355, -18.00000000000000355, -21.00000000000000000 ) ) ;
#19715 = DIRECTION ( 'NONE',  ( 0.000000000000000000, 0.000000000000000000, 1.000000000000000000 ) ) ;
#19714 = CARTESIAN_POINT ( 'NONE',  ( 15.00000000000000000, -23.65000000000000568, -12.40000000000000213 ) ) ;
#19716 = VERTEX_POINT ( 'NONE', #43329 ) ;
#19718 = ORIENTED_EDGE ( 'NONE', *, *, #59780, .F. ) ;
#19717 = CARTESIAN_POINT ( 'NONE',  ( 0.000000000000000000, 0.000000000000000000, -24.00000000000000000 ) ) ;
#19719 = ORIENTED_EDGE ( 'NONE', *, *, #61767, .T. ) ;
#19720 =( NAMED_UNIT ( * ) PLANE_ANGLE_UNIT ( ) SI_UNIT ( $, .RADIAN. ) );
#19721 = VECTOR ( 'NONE', #33724, 1000.000000000000000 ) ;
#19722 = DIRECTION ( 'NONE',  ( -0.7071067811865514585, -0.7071067811865435759, -2.597868168706465806E-16 ) ) ;
#19724 = ORIENTED_EDGE ( 'NONE', *, *, #48642, .T. ) ;
#19723 = CARTESIAN_POINT ( 'NONE',  ( 181.4833316329832940, 9.000000000000001776, 328.5239988703752942 ) ) ;
#19725 = ADVANCED_FACE ( 'NONE', ( #11153 ), #924, .F. ) ;
#19726 = DIRECTION ( 'NONE',  ( 0.000000000000000000, 0.000000000000000000, -1.000000000000000000 ) ) ;
#19727 = VECTOR ( 'NONE', #32050, 1000.000000000000000 ) ;
#19728 = DIRECTION ( 'NONE',  ( -1.000000000000000000, 1.254221251785257731E-14, 1.836970198721053107E-16 ) ) ;
#19729 = EDGE_CURVE ( 'NONE', #46020, #32262, #38050, .T. ) ;
#19730 = ORIENTED_EDGE ( 'NONE', *, *, #40892, .T. ) ;
#19731 = EDGE_CURVE ( 'NONE', #20521, #10069, #66293, .T. ) ;
#19732 = ORIENTED_EDGE ( 'NONE', *, *, #584, .T. ) ;
#19733 = CIRCLE ( 'NONE', #59228, 0.1749999999999998224 ) ;
#19734 = CYLINDRICAL_SURFACE ( 'NONE', #44736, 1.929199999999998028 ) ;
#19735 = EDGE_CURVE ( 'NONE', #1819, #13915, #20975, .T. ) ;
#19736 = ORIENTED_EDGE ( 'NONE', *, *, #2611, .F. ) ;
#19737 = EDGE_CURVE ( 'NONE', #2756, #18679, #65929, .T. ) ;
#19738 = DIRECTION ( 'NONE',  ( 1.000000000000000000, -3.491481338843133355E-15, -1.836970198721036590E-16 ) ) ;
#19739 = CARTESIAN_POINT ( 'NONE',  ( 11.00000000000000000, -12.00000000000000000, 11.03137303340310282 ) ) ;
#19740 = EDGE_CURVE ( 'NONE', #4484, #8573, #55007, .T. ) ;
#19741 = DIRECTION ( 'NONE',  ( -1.000000000000000000, 0.000000000000000000, 0.000000000000000000 ) ) ;
#19742 = ORIENTED_EDGE ( 'NONE', *, *, #48799, .F. ) ;
#19743 = EDGE_CURVE ( 'NONE', #36865, #29168, #12188, .T. ) ;
#19744 = CARTESIAN_POINT ( 'NONE',  ( 283.0000000000000568, -25.50000000000000355, 17.00000000000000000 ) ) ;
#19745 = DIRECTION ( 'NONE',  ( -4.956352788505217896E-15, -1.000000000000000000, 0.000000000000000000 ) ) ;
#19747 = ORIENTED_EDGE ( 'NONE', *, *, #46543, .F. ) ;
#19746 = CARTESIAN_POINT ( 'NONE',  ( 40.90000000000000568, 0.000000000000000000, 0.000000000000000000 ) ) ;
#19749 = ORIENTED_EDGE ( 'NONE', *, *, #44894, .T. ) ;
#19748 = CARTESIAN_POINT ( 'NONE',  ( 289.5000000000000000, -0.5000000000000000000, -27.00000000000000000 ) ) ;
#19750 = DIRECTION ( 'NONE',  ( 0.000000000000000000, 0.000000000000000000, 1.000000000000000000 ) ) ;
#19751 = LINE ( 'NONE', #47338, #18275 ) ;
#19752 = VECTOR ( 'NONE', #54251, 1000.000000000000000 ) ;
#19753 = CARTESIAN_POINT ( 'NONE',  ( 11.48848345035337104, 10.19191654964660820, 195.0000000000000284 ) ) ;
#19754 = CARTESIAN_POINT ( 'NONE',  ( 23.75054448485400016, -15.50000000000000000, -25.53140320652400064 ) ) ;
#19755 = DIRECTION ( 'NONE',  ( 1.836970198721029934E-16, -1.836970198721036344E-16, 1.000000000000000000 ) ) ;
#19756 = EDGE_LOOP ( 'NONE', ( #45955, #24161, #32848, #25170 ) ) ;
#19757 = CARTESIAN_POINT ( 'NONE',  ( -18.85410196625000268, -15.50000000000000000, -21.50000000000000000 ) ) ;
#19758 = CARTESIAN_POINT ( 'NONE',  ( -25.50000000000000355, 0.000000000000000000, 22.50000000000000000 ) ) ;
#19759 = CYLINDRICAL_SURFACE ( 'NONE', #52621, 2.458500000000000796 ) ;
#19761 = ORIENTED_EDGE ( 'NONE', *, *, #7020, .F. ) ;
#19760 = CARTESIAN_POINT ( 'NONE',  ( 24.00000000000000000, -15.50000000000000000, 14.50000000000000000 ) ) ;
#19762 = CIRCLE ( 'NONE', #551, 24.99999999998789946 ) ;
#19763 = VECTOR ( 'NONE', #26109, 1000.000000000000000 ) ;
#19764 = CARTESIAN_POINT ( 'NONE',  ( 30.00000000000000000, -10.85999999999999943, 9.000000000000001776 ) ) ;
#19765 = EDGE_CURVE ( 'NONE', #10975, #10944, #13590, .T. ) ;
#19766 = DIRECTION ( 'NONE',  ( 0.000000000000000000, 1.000000000000000000, 0.000000000000000000 ) ) ;
#19767 = AXIS2_PLACEMENT_3D ( 'NONE', #11970, #38854, #28248 ) ;
#19768 = AXIS2_PLACEMENT_3D ( 'NONE', #46072, #62325, #13892 ) ;
#19769 = VERTEX_POINT ( 'NONE', #67346 ) ;
#19770 = CARTESIAN_POINT ( 'NONE',  ( 9.912023737882815766, -6.832023737882823688, 54.00000000000000711 ) ) ;
#19771 = CARTESIAN_POINT ( 'NONE',  ( 7.806483450353379538, -11.12648345035339226, 195.0000000000000284 ) ) ;
#19772 = ORIENTED_EDGE ( 'NONE', *, *, #64922, .T. ) ;
#19773 = EDGE_CURVE ( 'NONE', #18160, #32104, #52639, .T. ) ;
#19774 = DIRECTION ( 'NONE',  ( -1.000000000000000000, 0.000000000000000000, 0.000000000000000000 ) ) ;
#19775 = CIRCLE ( 'NONE', #36709, 4.500000000000191847 ) ;
#19776 = DIRECTION ( 'NONE',  ( 0.4998444328988824181, 0.000000000000000000, -0.8661152018640445593 ) ) ;
#19777 = DIRECTION ( 'NONE',  ( 0.000000000000000000, 0.000000000000000000, 1.000000000000000000 ) ) ;
#19778 = EDGE_CURVE ( 'NONE', #56472, #39966, #46117, .T. ) ;
#19779 = DIRECTION ( 'NONE',  ( 0.000000000000000000, 0.000000000000000000, -1.000000000000000000 ) ) ;
#19780 = VECTOR ( 'NONE', #30566, 1000.000000000000114 ) ;
#19781 = ORIENTED_EDGE ( 'NONE', *, *, #8154, .T. ) ;
#19782 = LINE ( 'NONE', #41354, #13413 ) ;
#19783 = ORIENTED_EDGE ( 'NONE', *, *, #58473, .F. ) ;
#19784 = CYLINDRICAL_SURFACE ( 'NONE', #32960, 0.2000000000000005107 ) ;
#19785 = VERTEX_POINT ( 'NONE', #51069 ) ;
#19786 = AXIS2_PLACEMENT_3D ( 'NONE', #30637, #52199, #3760 ) ;
#19787 = CARTESIAN_POINT ( 'NONE',  ( 6.619341603356837744, -4.747751991980647901, 195.0000000000000284 ) ) ;
#19788 = DIRECTION ( 'NONE',  ( 0.000000000000000000, 1.000000000000000000, 0.000000000000000000 ) ) ;
#19789 = EDGE_CURVE ( 'NONE', #31070, #21380, #24558, .T. ) ;
#19790 = LINE ( 'NONE', #40322, #46810 ) ;
#19791 = ORIENTED_EDGE ( 'NONE', *, *, #69592, .T. ) ;
#19792 = ORIENTED_EDGE ( 'NONE', *, *, #43218, .F. ) ;
#19793 = CARTESIAN_POINT ( 'NONE',  ( -7.250000000000001776, -7.249999999999998224, -12.50000000000000000 ) ) ;
#19794 = VERTEX_POINT ( 'NONE', #35492 ) ;
#19795 = ORIENTED_EDGE ( 'NONE', *, *, #5604, .F. ) ;
#19796 = DIRECTION ( 'NONE',  ( 1.000000000000000000, -0.000000000000000000, 0.000000000000000000 ) ) ;
#19797 = CARTESIAN_POINT ( 'NONE',  ( 9.795823737882802362, 10.49297626211719070, 26.00000000000000711 ) ) ;
#19798 = CARTESIAN_POINT ( 'NONE',  ( -8.250000000000001776, -7.249999999999998224, -21.50000000000000000 ) ) ;
#19799 = FACE_OUTER_BOUND ( 'NONE', #20260, .T. ) ;
#19800 = EDGE_CURVE ( 'NONE', #61959, #39543, #2284, .T. ) ;
#19801 = ORIENTED_EDGE ( 'NONE', *, *, #23397, .T. ) ;
#19802 = EDGE_CURVE ( 'NONE', #69031, #63520, #16055, .T. ) ;
#19803 = FACE_OUTER_BOUND ( 'NONE', #40484, .T. ) ;
#19805 = CARTESIAN_POINT ( 'NONE',  ( -4.031976262117257903, -3.157023737882818981, 54.00000000000000711 ) ) ;
#19804 = CARTESIAN_POINT ( 'NONE',  ( 7.250000000000005329, 7.250000000000000888, -22.50000000000000000 ) ) ;
#19806 = ORIENTED_EDGE ( 'NONE', *, *, #38289, .F. ) ;
#19809 = EDGE_CURVE ( 'NONE', #23827, #45446, #32291, .T. ) ;
#19808 = VERTEX_POINT ( 'NONE', #18536 ) ;
#19807 = DIRECTION ( 'NONE',  ( 8.673617379884013384E-15, 1.000000000000000000, 0.000000000000000000 ) ) ;
#19810 = VECTOR ( 'NONE', #57712, 1000.000000000000000 ) ;
#19811 = VERTEX_POINT ( 'NONE', #61673 ) ;
#19812 = ADVANCED_FACE ( 'NONE', ( #19244 ), #61314, .F. ) ;
#19813 = EDGE_CURVE ( 'NONE', #20791, #48776, #60968, .T. ) ;
#19814 = VECTOR ( 'NONE', #57184, 1000.000000000000000 ) ;
#19815 = LINE ( 'NONE', #25488, #12939 ) ;
#19816 = EDGE_CURVE ( 'NONE', #58955, #13881, #55680, .T. ) ;
#19817 = CIRCLE ( 'NONE', #3988, 0.5249999999999994671 ) ;
#19818 = VECTOR ( 'NONE', #9522, 1000.000000000000000 ) ;
#19820 = LINE ( 'NONE', #64037, #43977 ) ;
#19819 = VECTOR ( 'NONE', #30883, 1000.000000000000000 ) ;
#19821 = EDGE_CURVE ( 'NONE', #52778, #27235, #1783, .T. ) ;
#19822 = VERTEX_POINT ( 'NONE', #3337 ) ;
#19823 = ORIENTED_EDGE ( 'NONE', *, *, #61813, .T. ) ;
#19824 = ADVANCED_FACE ( 'NONE', ( #46462 ), #45406, .F. ) ;
#19825 = AXIS2_PLACEMENT_3D ( 'NONE', #69207, #41633, #58256 ) ;
#19826 = AXIS2_PLACEMENT_3D ( 'NONE', #36430, #30429, #21233 ) ;
#19827 = FACE_OUTER_BOUND ( 'NONE', #32069, .T. ) ;
#19828 = CARTESIAN_POINT ( 'NONE',  ( -8.250000000000001776, 7.250000000000000888, -26.00000000000001066 ) ) ;
#19829 = ORIENTED_EDGE ( 'NONE', *, *, #43002, .F. ) ;
#19830 = VERTEX_POINT ( 'NONE', #28793 ) ;
#19831 = FACE_OUTER_BOUND ( 'NONE', #9050, .T. ) ;
#19832 = VECTOR ( 'NONE', #17909, 1000.000000000000000 ) ;
#19833 = ADVANCED_FACE ( 'NONE', ( #35144 ), #7582, .F. ) ;
#19834 = CARTESIAN_POINT ( 'NONE',  ( 7.000000000000000000, -26.06132420600899735, 10.13999572156699891 ) ) ;
#19835 = EDGE_LOOP ( 'NONE', ( #37667, #25575, #59364, #62595 ) ) ;
#19836 = EDGE_CURVE ( 'NONE', #27192, #16314, #65104, .T. ) ;
#19837 = VECTOR ( 'NONE', #26495, 1000.000000000000000 ) ;
#19838 = DIRECTION ( 'NONE',  ( -1.000000000000000000, 0.000000000000000000, 0.000000000000000000 ) ) ;
#19839 = PLANE ( 'NONE',  #39585 ) ;
#19841 = ORIENTED_EDGE ( 'NONE', *, *, #3359, .F. ) ;
#19840 = PLANE ( 'NONE',  #36274 ) ;
#19842 = CIRCLE ( 'NONE', #68408, 0.1749999999999989342 ) ;
#19843 = ORIENTED_EDGE ( 'NONE', *, *, #27585, .T. ) ;
#19844 = DIRECTION ( 'NONE',  ( 1.000000000000000000, -0.000000000000000000, 0.000000000000000000 ) ) ;
#19845 = DIRECTION ( 'NONE',  ( 0.000000000000000000, 0.000000000000000000, 1.000000000000000000 ) ) ;
#19846 = EDGE_CURVE ( 'NONE', #52878, #11057, #27840, .T. ) ;
#19847 = FACE_BOUND ( 'NONE', #62365, .T. ) ;
#19848 = CARTESIAN_POINT ( 'NONE',  ( 46.39999999999999858, 33.00000000000000000, 0.2500000000000000000 ) ) ;
#19849 = LINE ( 'NONE', #14547, #5728 ) ;
#19850 = CARTESIAN_POINT ( 'NONE',  ( -8.227189898828694226, -1.634292677759810575, 26.00000000000000711 ) ) ;
#19851 = EDGE_LOOP ( 'NONE', ( #65853, #14332, #30500, #1917 ) ) ;
#19852 = DIRECTION ( 'NONE',  ( -0.000000000000000000, -0.000000000000000000, 1.000000000000000000 ) ) ;
#19854 = VERTEX_POINT ( 'NONE', #8275 ) ;
#19853 = DIRECTION ( 'NONE',  ( 0.000000000000000000, 1.000000000000000000, 0.000000000000000000 ) ) ;
#19855 = FACE_OUTER_BOUND ( 'NONE', #7914, .T. ) ;
#19856 = FACE_BOUND ( 'NONE', #34695, .T. ) ;
#19857 = CIRCLE ( 'NONE', #56000, 24.99999999998794920 ) ;
#19858 = DIRECTION ( 'NONE',  ( 1.836970198721029934E-16, 1.836970198721010706E-16, -1.000000000000000000 ) ) ;
#19859 = AXIS2_PLACEMENT_3D ( 'NONE', #11869, #29884, #7256 ) ;
#19860 = ORIENTED_EDGE ( 'NONE', *, *, #60350, .F. ) ;
#19861 = DIRECTION ( 'NONE',  ( -1.836970198721029934E-16, 1.836970198721036590E-16, -1.000000000000000000 ) ) ;
#19862 = CYLINDRICAL_SURFACE ( 'NONE', #65558, 2.000000000000001776 ) ;
#19863 = ORIENTED_EDGE ( 'NONE', *, *, #26189, .F. ) ;
#19864 = EDGE_CURVE ( 'NONE', #58158, #27192, #29847, .T. ) ;
#19865 = DIRECTION ( 'NONE',  ( 0.000000000000000000, 1.000000000000000000, 0.000000000000000000 ) ) ;
#19866 = VECTOR ( 'NONE', #64512, 1000.000000000000000 ) ;
#19867 =( NAMED_UNIT ( * ) PLANE_ANGLE_UNIT ( ) SI_UNIT ( $, .RADIAN. ) );
#19868 = EDGE_CURVE ( 'NONE', #69377, #37150, #15176, .T. ) ;
#19869 = VECTOR ( 'NONE', #67227, 1000.000000000000000 ) ;
#19870 = AXIS2_PLACEMENT_3D ( 'NONE', #51873, #62823, #52213 ) ;
#19871 = AXIS2_PLACEMENT_3D ( 'NONE', #46350, #62607, #36091 ) ;
#19872 = CARTESIAN_POINT ( 'NONE',  ( -7.603567055985545942, 8.593516549646603053, 455.0000000000000568 ) ) ;
#19873 = ORIENTED_EDGE ( 'NONE', *, *, #56847, .F. ) ;
#19874 = LINE ( 'NONE', #30486, #23711 ) ;
#19875 = EDGE_LOOP ( 'NONE', ( #45118, #49433, #18198, #55931 ) ) ;
#19876 = ADVANCED_FACE ( 'NONE', ( #36934 ), #19947, .F. ) ;
#19877 = VERTEX_POINT ( 'NONE', #25619 ) ;
#19878 = DIRECTION ( 'NONE',  ( 0.000000000000000000, -3.673940397442059868E-16, 1.000000000000000000 ) ) ;
#19880 = DIRECTION ( 'NONE',  ( 0.000000000000000000, -1.000000000000000000, 0.000000000000000000 ) ) ;
#19879 = CIRCLE ( 'NONE', #2919, 0.1749999999999998224 ) ;
#19881 = VECTOR ( 'NONE', #66848, 1000.000000000000114 ) ;
#19882 = VECTOR ( 'NONE', #13720, 1000.000000000000000 ) ;
#19883 = LINE ( 'NONE', #13875, #34426 ) ;
#19884 = ADVANCED_FACE ( 'NONE', ( #8982 ), #52125, .T. ) ;
#19885 = AXIS2_PLACEMENT_3D ( 'NONE', #62353, #13920, #50699 ) ;
#19886 = DIRECTION ( 'NONE',  ( -0.000000000000000000, -0.000000000000000000, 1.000000000000000000 ) ) ;
#19887 = ADVANCED_FACE ( 'NONE', ( #48230 ), #57425, .F. ) ;
#19888 = DIRECTION ( 'NONE',  ( 0.000000000000000000, 1.000000000000000000, 0.000000000000000000 ) ) ;
#19889 = ORIENTED_EDGE ( 'NONE', *, *, #48091, .F. ) ;
#19890 = ORIENTED_EDGE ( 'NONE', *, *, #30878, .F. ) ;
#19892 = ORIENTED_EDGE ( 'NONE', *, *, #28231, .F. ) ;
#19891 = DIRECTION ( 'NONE',  ( 1.000000000000000000, -0.000000000000000000, 0.000000000000000000 ) ) ;
#19893 = ORIENTED_EDGE ( 'NONE', *, *, #33769, .F. ) ;
#19894 = CIRCLE ( 'NONE', #22178, 3.499999999999040323 ) ;
#19895 = FACE_OUTER_BOUND ( 'NONE', #34601, .T. ) ;
#19896 = FACE_OUTER_BOUND ( 'NONE', #33246, .T. ) ;
#19897 = CARTESIAN_POINT ( 'NONE',  ( 29.50000000000000355, -11.50000000000100009, 15.00000000000084910 ) ) ;
#19898 = MANIFOLD_SOLID_BREP ( 'LPattern1[13]', #64559 ) ;
#19899 = CARTESIAN_POINT ( 'NONE',  ( 283.0000000000000568, -26.50000000000000000, 0.5000000000000000000 ) ) ;
#19900 = EDGE_CURVE ( 'NONE', #46263, #9826, #41155, .T. ) ;
#19901 = CARTESIAN_POINT ( 'NONE',  ( -8.697938382363098242, -2.420780051175094094, 26.00000000000000711 ) ) ;
#19902 = DIRECTION ( 'NONE',  ( -0.000000000000000000, -0.000000000000000000, 1.000000000000000000 ) ) ;
#19903 = ORIENTED_EDGE ( 'NONE', *, *, #59136, .F. ) ;
#19904 = ORIENTED_EDGE ( 'NONE', *, *, #58982, .F. ) ;
#19905 = EDGE_LOOP ( 'NONE', ( #61733, #20619, #18838, #52099 ) ) ;
#19906 = EDGE_CURVE ( 'NONE', #21685, #53820, #62724, .T. ) ;
#19907 = EDGE_LOOP ( 'NONE', ( #51135, #7700, #66689, #13446 ) ) ;
#19908 = CYLINDRICAL_SURFACE ( 'NONE', #10755, 1.621000000000000885 ) ;
#19909 = LINE ( 'NONE', #41481, #18552 ) ;
#19910 = CARTESIAN_POINT ( 'NONE',  ( 6.006483450353379716, -4.606483450353397124, 195.0000000000000284 ) ) ;
#19911 = ORIENTED_EDGE ( 'NONE', *, *, #18453, .T. ) ;
#19912 = VERTEX_POINT ( 'NONE', #46808 ) ;
#19913 = AXIS2_PLACEMENT_3D ( 'NONE', #38313, #43255, #12113 ) ;
#19914 = ORIENTED_EDGE ( 'NONE', *, *, #21388, .T. ) ;
#19915 = DIRECTION ( 'NONE',  ( 1.836970198721029934E-16, 1.836970198721010706E-16, -1.000000000000000000 ) ) ;
#19916 = ORIENTED_EDGE ( 'NONE', *, *, #11091, .F. ) ;
#19917 = VERTEX_POINT ( 'NONE', #68390 ) ;
#19918 = CARTESIAN_POINT ( 'NONE',  ( 40.90000000000000568, 6.429395695523604153E-16, -5.250000000000000000 ) ) ;
#19919 = ORIENTED_EDGE ( 'NONE', *, *, #16592, .T. ) ;
#19920 = VERTEX_POINT ( 'NONE', #36204 ) ;
#19921 = VECTOR ( 'NONE', #36383, 1000.000000000000000 ) ;
#19923 = DIRECTION ( 'NONE',  ( -1.836970198721029934E-16, 1.836970198721036344E-16, -1.000000000000000000 ) ) ;
#19922 = AXIS2_PLACEMENT_3D ( 'NONE', #52375, #3234, #47071 ) ;
#19924 = EDGE_CURVE ( 'NONE', #59933, #41191, #26658, .T. ) ;
#19926 = VERTEX_POINT ( 'NONE', #20995 ) ;
#19925 = CARTESIAN_POINT ( 'NONE',  ( 6.872275254348378937, 2.989207322240125198, 26.00000000000000711 ) ) ;
#19927 = ORIENTED_EDGE ( 'NONE', *, *, #67861, .F. ) ;
#19928 = ADVANCED_FACE ( 'NONE', ( #47178 ), #14999, .F. ) ;
#19929 = AXIS2_PLACEMENT_3D ( 'NONE', #66540, #55587, #39657 ) ;
#19930 = VECTOR ( 'NONE', #59101, 1000.000000000000000 ) ;
#19931 = CIRCLE ( 'NONE', #33455, 2.204799999999997429 ) ;
#19932 = DIRECTION ( 'NONE',  ( 1.000000000000000000, 1.671920889371702854E-15, 6.142537696789956391E-31 ) ) ;
#19933 = LINE ( 'NONE', #62708, #27956 ) ;
#19935 = ORIENTED_EDGE ( 'NONE', *, *, #52518, .T. ) ;
#19934 = CARTESIAN_POINT ( 'NONE',  ( -9.547976262117256141, 7.955476262117183062, 26.00000000000000711 ) ) ;
#19936 = ORIENTED_EDGE ( 'NONE', *, *, #63468, .F. ) ;
#19937 = AXIS2_PLACEMENT_3D ( 'NONE', #34710, #7487, #44973 ) ;
#19938 = FACE_OUTER_BOUND ( 'NONE', #6178, .T. ) ;
#19939 = LINE ( 'NONE', #30902, #32890 ) ;
#19940 = DIRECTION ( 'NONE',  ( 0.000000000000000000, 0.7071067811865474617, 0.7071067811865474617 ) ) ;
#19941 = LINE ( 'NONE', #19587, #15810 ) ;
#19942 = CIRCLE ( 'NONE', #5270, 0.1999999999999996503 ) ;
#19943 = VERTEX_POINT ( 'NONE', #31283 ) ;
#19944 = CARTESIAN_POINT ( 'NONE',  ( 0.000000000000000000, -2.500000000000000000, 0.000000000000000000 ) ) ;
#19945 = AXIS2_PLACEMENT_3D ( 'NONE', #54136, #60113, #44190 ) ;
#19946 = CARTESIAN_POINT ( 'NONE',  ( 7.450000000000003730, -7.249999999999997335, -8.000000000000000000 ) ) ;
#19947 = PLANE ( 'NONE',  #58347 ) ;
#19948 = ORIENTED_EDGE ( 'NONE', *, *, #57347, .T. ) ;
#19949 = FACE_OUTER_BOUND ( 'NONE', #15641, .T. ) ;
#19950 = CARTESIAN_POINT ( 'NONE',  ( 7.616533956692213003, -8.406483450353396947, 195.0000000000000284 ) ) ;
#19951 = DIRECTION ( 'NONE',  ( 0.000000000000000000, 0.000000000000000000, 1.000000000000000000 ) ) ;
#19952 = ORIENTED_EDGE ( 'NONE', *, *, #61263, .T. ) ;
#19953 =( NAMED_UNIT ( * ) PLANE_ANGLE_UNIT ( ) SI_UNIT ( $, .RADIAN. ) );
#19954 = CARTESIAN_POINT ( 'NONE',  ( -4.727349090213463612, 4.188533722949258298, 455.0000000000000568 ) ) ;
#19955 = EDGE_CURVE ( 'NONE', #65565, #54361, #52850, .T. ) ;
#19956 = FACE_OUTER_BOUND ( 'NONE', #59096, .T. ) ;
#19957 = EDGE_LOOP ( 'NONE', ( #62497, #56180, #29003, #51532 ) ) ;
#19958 = FACE_OUTER_BOUND ( 'NONE', #34748, .T. ) ;
#19959 = DIRECTION ( 'NONE',  ( 0.000000000000000000, -1.000000000000000000, 0.000000000000000000 ) ) ;
#19960 = AXIS2_PLACEMENT_3D ( 'NONE', #752, #22652, #22318 ) ;
#19961 = CARTESIAN_POINT ( 'NONE',  ( 9.690000000000001279, -9.690000000000001279, -5.000000000000000000 ) ) ;
#19962 = ADVANCED_FACE ( 'NONE', ( #20641 ), #42212, .F. ) ;
#19963 = CARTESIAN_POINT ( 'NONE',  ( 275.0000000000000000, -23.50007830495750127, 12.28007262201345995 ) ) ;
#19964 = DIRECTION ( 'NONE',  ( 1.000000000000000000, 0.000000000000000000, 0.000000000000000000 ) ) ;
#19965 = ORIENTED_EDGE ( 'NONE', *, *, #15914, .F. ) ;
#19966 = CARTESIAN_POINT ( 'NONE',  ( 290.0000000000000000, 0.000000000000000000, 0.000000000000000000 ) ) ;
#19967 = DIRECTION ( 'NONE',  ( 0.000000000000000000, 1.000000000000000000, 0.000000000000000000 ) ) ;
#19968 = CIRCLE ( 'NONE', #34473, 0.1749999999999989342 ) ;
#19969 = ADVANCED_FACE ( 'NONE', ( #6129 ), #37620, .F. ) ;
#19970 = EDGE_CURVE ( 'NONE', #4070, #24615, #64491, .T. ) ;
#19971 = DIRECTION ( 'NONE',  ( 0.000000000000000000, 0.000000000000000000, 1.000000000000000000 ) ) ;
#19972 = CIRCLE ( 'NONE', #59503, 1.399999999999998579 ) ;
#19973 = VECTOR ( 'NONE', #68197, 1000.000000000000000 ) ;
#19974 = FACE_OUTER_BOUND ( 'NONE', #60105, .T. ) ;
#19975 = EDGE_CURVE ( 'NONE', #32135, #18841, #59178, .T. ) ;
#19976 = LINE ( 'NONE', #42590, #58862 ) ;
#19977 = EDGE_CURVE ( 'NONE', #53470, #21801, #6482, .T. ) ;
#19978 = ORIENTED_EDGE ( 'NONE', *, *, #7728, .F. ) ;
#19980 = ORIENTED_EDGE ( 'NONE', *, *, #17259, .T. ) ;
#19979 = CARTESIAN_POINT ( 'NONE',  ( -7.250000000000000888, 7.250000000000001776, -22.50000000000000000 ) ) ;
#19981 = CIRCLE ( 'NONE', #29001, 1.000000000000000000 ) ;
#19982 = CIRCLE ( 'NONE', #26750, 4.000000000000000888 ) ;
#19983 = EDGE_CURVE ( 'NONE', #13174, #54503, #33345, .T. ) ;
#19984 = CARTESIAN_POINT ( 'NONE',  ( 6.006483450353379716, -6.006483450353490738, 455.0000000000000568 ) ) ;
#19985 = FACE_OUTER_BOUND ( 'NONE', #53067, .T. ) ;
#19986 = CARTESIAN_POINT ( 'NONE',  ( 10.90000000000000036, 13.66939075806899240, 20.79999999999999361 ) ) ;
#19987 = ORIENTED_EDGE ( 'NONE', *, *, #6529, .T. ) ;
#19988 = AXIS2_PLACEMENT_3D ( 'NONE', #3419, #67764, #61762 ) ;
#19990 = CARTESIAN_POINT ( 'NONE',  ( 9.703773737882816164, 9.689726262117153155, 54.00000000000000711 ) ) ;
#19989 = CIRCLE ( 'NONE', #43711, 0.1749999999999998224 ) ;
#19991 = FACE_OUTER_BOUND ( 'NONE', #39648, .T. ) ;
#19992 = VERTEX_POINT ( 'NONE', #65526 ) ;
#19993 = ORIENTED_EDGE ( 'NONE', *, *, #69575, .T. ) ;
#19994 = AXIS2_PLACEMENT_3D ( 'NONE', #55751, #635, #5933 ) ;
#19995 = ORIENTED_EDGE ( 'NONE', *, *, #61997, .T. ) ;
#19996 = LINE ( 'NONE', #24945, #44143 ) ;
#19997 = CARTESIAN_POINT ( 'NONE',  ( -3.650476262117329007, -10.31452373788281385, 26.00000000000000000 ) ) ;
#19998 = DIRECTION ( 'NONE',  ( 0.000000000000000000, 0.000000000000000000, 1.000000000000000000 ) ) ;
#19999 =( LENGTH_UNIT ( ) NAMED_UNIT ( * ) SI_UNIT ( .MILLI., .METRE. ) );
#20000 = CIRCLE ( 'NONE', #59532, 3.499999999999999556 ) ;
#20001 = EDGE_LOOP ( 'NONE', ( #38947, #41176, #56253, #56684 ) ) ;
#20002 = ORIENTED_EDGE ( 'NONE', *, *, #5588, .F. ) ;
#20003 = DIRECTION ( 'NONE',  ( 0.000000000000000000, -0.7096009616570518874, 0.7046037717862339012 ) ) ;
#20004 = B_SPLINE_CURVE_WITH_KNOTS ( 'NONE', 3,
 ( #22245, #38505, #2654, #65380, #62396, #56058 ),
 .UNSPECIFIED., .F., .F.,
 ( 4, 2, 4 ),
 ( 0.0002380763768114607659, 0.7291065797294573603, 1.457975083082103218 ),
 .UNSPECIFIED. ) ;
#20005 = CARTESIAN_POINT ( 'NONE',  ( 7.000000000000000000, -38.10000000000000142, 8.400000000000000355 ) ) ;
#20006 = ORIENTED_EDGE ( 'NONE', *, *, #21976, .T. ) ;
#20007 = EDGE_LOOP ( 'NONE', ( #44571, #67579 ) ) ;
#20008 = ORIENTED_EDGE ( 'NONE', *, *, #35435, .F. ) ;
#20009 = ORIENTED_EDGE ( 'NONE', *, *, #17825, .T. ) ;
#20010 = DIRECTION ( 'NONE',  ( -1.794541526872559352E-16, -1.000000000000000000, 0.000000000000000000 ) ) ;
#20012 = ORIENTED_EDGE ( 'NONE', *, *, #41454, .F. ) ;
#20011 = DIRECTION ( 'NONE',  ( 0.000000000000000000, -3.673940397442059868E-16, 1.000000000000000000 ) ) ;
#20013 = LINE ( 'NONE', #53597, #59420 ) ;
#20014 = EDGE_CURVE ( 'NONE', #122, #63027, #33681, .T. ) ;
#20015 = DIRECTION ( 'NONE',  ( 0.000000000000000000, 1.000000000000000000, 0.000000000000000000 ) ) ;
#20016 = VECTOR ( 'NONE', #54745, 1000.000000000000000 ) ;
#20017 = ORIENTED_EDGE ( 'NONE', *, *, #31999, .F. ) ;
#20018 = ADVANCED_FACE ( 'NONE', ( #482 ), #59869, .F. ) ;
#20019 = ORIENTED_EDGE ( 'NONE', *, *, #30195, .F. ) ;
#20020 = EDGE_CURVE ( 'NONE', #23208, #30476, #49273, .T. ) ;
#20021 = ADVANCED_FACE ( 'NONE', ( #11761 ), #49602, .F. ) ;
#20022 = DIRECTION ( 'NONE',  ( -1.000000000000000000, 0.000000000000000000, 0.000000000000000000 ) ) ;
#20023 = VECTOR ( 'NONE', #45213, 1000.000000000000000 ) ;
#20024 = AXIS2_PLACEMENT_3D ( 'NONE', #52562, #9776, #16120 ) ;
#20025 = CARTESIAN_POINT ( 'NONE',  ( 283.0000000000000568, -42.00000000000000000, 15.00000000000000000 ) ) ;
#20026 = ORIENTED_EDGE ( 'NONE', *, *, #6932, .F. ) ;
#20027 = VECTOR ( 'NONE', #13873, 1000.000000000000000 ) ;
#20028 = AXIS2_PLACEMENT_3D ( 'NONE', #51403, #66960, #51055 ) ;
#20029 = LINE ( 'NONE', #25697, #53956 ) ;
#20030 = ORIENTED_EDGE ( 'NONE', *, *, #633, .T. ) ;
#20031 = DIRECTION ( 'NONE',  ( 0.000000000000000000, 0.7071067811865875408, 0.7071067811865076047 ) ) ;
#20032 = DIRECTION ( 'NONE',  ( -0.000000000000000000, -1.000000000000000000, 0.000000000000000000 ) ) ;
#20033 = CIRCLE ( 'NONE', #36970, 0.06000000000000102474 ) ;
#20034 = AXIS2_PLACEMENT_3D ( 'NONE', #52345, #35349, #62957 ) ;
#20035 = DIRECTION ( 'NONE',  ( 1.000000000000000000, -0.000000000000000000, -0.000000000000000000 ) ) ;
#20036 = DIRECTION ( 'NONE',  ( 1.836970198721029934E-16, 1.836970198721010706E-16, -1.000000000000000000 ) ) ;
#20037 = DIRECTION ( 'NONE',  ( -1.000000000000000000, 0.000000000000000000, 0.000000000000000000 ) ) ;
#20038 = ORIENTED_EDGE ( 'NONE', *, *, #31685, .T. ) ;
#20039 = CARTESIAN_POINT ( 'NONE',  ( 9.899999999999998579, -0.2000000000000000111, 0.000000000000000000 ) ) ;
#20040 = DIRECTION ( 'NONE',  ( 0.000000000000000000, 1.000000000000000000, 0.000000000000000000 ) ) ;
#20041 = DIRECTION ( 'NONE',  ( 0.000000000000000000, 0.000000000000000000, 1.000000000000000000 ) ) ;
#20042 = DIRECTION ( 'NONE',  ( -1.000000000000000000, 0.000000000000000000, 0.000000000000000000 ) ) ;
#20043 = AXIS2_PLACEMENT_3D ( 'NONE', #34176, #34875, #39831 ) ;
#20044 = EDGE_CURVE ( 'NONE', #33426, #64234, #11086, .T. ) ;
#20045 = DIRECTION ( 'NONE',  ( 1.000000000000000000, 0.000000000000000000, 0.000000000000000000 ) ) ;
#20046 = DIRECTION ( 'NONE',  ( 0.000000000000000000, -1.000000000000000000, 0.000000000000000000 ) ) ;
#20047 = CARTESIAN_POINT ( 'NONE',  ( 0.5000000000000000000, -18.00000000000000355, 21.00000000000000000 ) ) ;
#20048 = CARTESIAN_POINT ( 'NONE',  ( 4.456444791733522252E-16, 7.450000000000002842, -18.50000000000000000 ) ) ;
#20049 = ORIENTED_EDGE ( 'NONE', *, *, #17983, .F. ) ;
#20050 = DIRECTION ( 'NONE',  ( -1.000000000000000000, 0.000000000000000000, 0.000000000000000000 ) ) ;
#20051 = CARTESIAN_POINT ( 'NONE',  ( -7.744988412222854279, 8.452095193409293827, 195.0000000000000284 ) ) ;
#20052 = ORIENTED_EDGE ( 'NONE', *, *, #26825, .F. ) ;
#20053 = CARTESIAN_POINT ( 'NONE',  ( -7.250000000000000888, 7.250000000000001776, -15.50000000000000000 ) ) ;
#20054 = CARTESIAN_POINT ( 'NONE',  ( 23.90000000000000213, -14.06939075806900874, 20.80000000000001137 ) ) ;
#20055 = FACE_OUTER_BOUND ( 'NONE', #48739, .T. ) ;
#20056 = DIRECTION ( 'NONE',  ( 0.7671651518152985405, 0.6414496315691592399, -2.309356642088639737E-17 ) ) ;
#20057 = EDGE_CURVE ( 'NONE', #39293, #23736, #1831, .T. ) ;
#20058 = CARTESIAN_POINT ( 'NONE',  ( -3.650476262117223314, 10.30047626211716683, 54.00000000000000711 ) ) ;
#20059 = EDGE_CURVE ( 'NONE', #6346, #62186, #21352, .T. ) ;
#20060 = VERTEX_POINT ( 'NONE', #60204 ) ;
#20061 = ORIENTED_EDGE ( 'NONE', *, *, #34084, .T. ) ;
#20062 = ADVANCED_FACE ( 'NONE', ( #54928 ), #27356, .T. ) ;
#20063 = CARTESIAN_POINT ( 'NONE',  ( 39.00000000000000000, 4.286263797015736595E-16, -3.500000000000000000 ) ) ;
#20064 = PLANE ( 'NONE',  #31194 ) ;
#20065 = VECTOR ( 'NONE', #59539, 1000.000000000000000 ) ;
#20066 = ORIENTED_EDGE ( 'NONE', *, *, #48999, .F. ) ;
#20067 = CARTESIAN_POINT ( 'NONE',  ( 41.09999999999999432, -14.06939075806901940, -20.80000000000000426 ) ) ;
#20068 = LINE ( 'NONE', #41631, #28440 ) ;
#20069 = ORIENTED_EDGE ( 'NONE', *, *, #52806, .F. ) ;
#20070 = AXIS2_PLACEMENT_3D ( 'NONE', #44427, #59329, #5932 ) ;
#20071 = DIRECTION ( 'NONE',  ( -1.000000000000000000, -0.000000000000000000, -0.000000000000000000 ) ) ;
#20072 = ORIENTED_EDGE ( 'NONE', *, *, #980, .F. ) ;
#20073 = VERTEX_POINT ( 'NONE', #1177 ) ;
#20074 = LINE ( 'NONE', #40584, #37512 ) ;
#20075 = ORIENTED_EDGE ( 'NONE', *, *, #29369, .F. ) ;
#20076 = ORIENTED_EDGE ( 'NONE', *, *, #37080, .T. ) ;
#20077 = VECTOR ( 'NONE', #45607, 1000.000000000000000 ) ;
#20078 = VECTOR ( 'NONE', #67589, 1000.000000000000000 ) ;
#20079 = DIRECTION ( 'NONE',  ( 0.000000000000000000, 0.000000000000000000, 1.000000000000000000 ) ) ;
#20080 = DIRECTION ( 'NONE',  ( -0.000000000000000000, -0.000000000000000000, 1.000000000000000000 ) ) ;
#20081 = DIRECTION ( 'NONE',  ( 0.000000000000000000, 0.7071067811865076047, 0.7071067811865875408 ) ) ;
#20082 = VECTOR ( 'NONE', #6035, 1000.000000000000000 ) ;
#20083 = ORIENTED_EDGE ( 'NONE', *, *, #16466, .T. ) ;
#20084 = DIRECTION ( 'NONE',  ( 1.836970198721029934E-16, 1.836970198721010706E-16, -1.000000000000000000 ) ) ;
#20085 = AXIS2_PLACEMENT_3D ( 'NONE', #17082, #43608, #22045 ) ;
#20086 = AXIS2_PLACEMENT_3D ( 'NONE', #19029, #3122, #40236 ) ;
#20088 = CARTESIAN_POINT ( 'NONE',  ( 41.09999999999999432, -21.00000000000000000, -13.86939075806900057 ) ) ;
#20087 = CARTESIAN_POINT ( 'NONE',  ( 87.07321854994620480, 47.95351654967443977, 39.00000000000000000 ) ) ;
#20089 = ORIENTED_EDGE ( 'NONE', *, *, #9965, .T. ) ;
#20091 = VERTEX_POINT ( 'NONE', #38987 ) ;
#20090 = CARTESIAN_POINT ( 'NONE',  ( -4.393516549646832914, -11.32648345035344128, 455.0000000000000568 ) ) ;
#20092 = ORIENTED_EDGE ( 'NONE', *, *, #55289, .F. ) ;
#20093 = SHAPE_DEFINITION_REPRESENTATION ( #29020, #26379 ) ;
#20094 = APPLICATION_CONTEXT ( 'automotive_design' ) ;
#20095 = FACE_OUTER_BOUND ( 'NONE', #62651, .T. ) ;
#20097 = ORIENTED_EDGE ( 'NONE', *, *, #49363, .F. ) ;
#20096 = LINE ( 'NONE', #52989, #63588 ) ;
#20098 = VECTOR ( 'NONE', #29854, 1000.000000000000000 ) ;
#20099 = LINE ( 'NONE', #20787, #39013 ) ;
#20100 = DIRECTION ( 'NONE',  ( 0.000000000000000000, -1.000000000000000000, -3.673940397442059868E-16 ) ) ;
#20101 = ORIENTED_EDGE ( 'NONE', *, *, #17177, .F. ) ;
#20102 = VERTEX_POINT ( 'NONE', #42910 ) ;
#20103 = EDGE_CURVE ( 'NONE', #57937, #42164, #60556, .T. ) ;
#20104 = EDGE_CURVE ( 'NONE', #68268, #14910, #50389, .T. ) ;
#20105 = EDGE_CURVE ( 'NONE', #25597, #6930, #38002, .T. ) ;
#20106 = DIRECTION ( 'NONE',  ( -1.000000000000000000, 0.000000000000000000, 0.000000000000000000 ) ) ;
#20107 = ORIENTED_EDGE ( 'NONE', *, *, #52894, .F. ) ;
#20108 = ADVANCED_FACE ( 'NONE', ( #7143 ), #34355, .F. ) ;
#20109 = CARTESIAN_POINT ( 'NONE',  ( 7.750000000000001776, 7.750000000000000000, 0.000000000000000000 ) ) ;
#20110 = DIRECTION ( 'NONE',  ( 0.000000000000000000, 0.000000000000000000, -1.000000000000000000 ) ) ;
#20111 = DIRECTION ( 'NONE',  ( 0.6414496315691592399, 0.7671651518152985405, 2.309356642088728176E-17 ) ) ;
#20112 = ORIENTED_EDGE ( 'NONE', *, *, #6603, .T. ) ;
#20113 = B_SPLINE_CURVE_WITH_KNOTS ( 'NONE', 3,
 ( #58641, #48377, #62893, #46970, #31434, #4554 ),
 .UNSPECIFIED., .F., .F.,
 ( 4, 2, 4 ),
 ( 0.0002380763768115301549, 0.7291065797294569162, 1.457975083082102330 ),
 .UNSPECIFIED. ) ;
#20114 = DIRECTION ( 'NONE',  ( 0.000000000000000000, -1.000000000000000000, 0.000000000000000000 ) ) ;
#20115 = LINE ( 'NONE', #48641, #20183 ) ;
#20116 = VECTOR ( 'NONE', #31201, 1000.000000000000000 ) ;
#20118 = ORIENTED_EDGE ( 'NONE', *, *, #53945, .T. ) ;
#20117 = DIRECTION ( 'NONE',  ( -1.836970198721029934E-16, 1.836970198721036344E-16, -1.000000000000000000 ) ) ;
#20120 = ORIENTED_EDGE ( 'NONE', *, *, #53981, .T. ) ;
#20119 = LINE ( 'NONE', #42029, #53526 ) ;
#20121 = CARTESIAN_POINT ( 'NONE',  ( -29.50000000000000355, -15.97213595500069871, 14.50000000000000000 ) ) ;
#20122 = LINE ( 'NONE', #14819, #9271 ) ;
#20123 = DIRECTION ( 'NONE',  ( 0.000000000000000000, 0.000000000000000000, -1.000000000000000000 ) ) ;
#20124 = FACE_OUTER_BOUND ( 'NONE', #4010, .T. ) ;
#20125 = DIRECTION ( 'NONE',  ( -1.000000000000000000, 0.000000000000000000, 0.000000000000000000 ) ) ;
#20126 = ORIENTED_EDGE ( 'NONE', *, *, #13033, .T. ) ;
#20127 = DIRECTION ( 'NONE',  ( -1.836970198721029934E-16, 1.836970198721036344E-16, -1.000000000000000000 ) ) ;
#20128 = CARTESIAN_POINT ( 'NONE',  ( 11.00000000000000000, -11.50000000000000000, -11.00000000000000000 ) ) ;
#20129 = AXIS2_PLACEMENT_3D ( 'NONE', #17271, #38836, #37815 ) ;
#20131 = EDGE_LOOP ( 'NONE', ( #19571, #9105, #41400, #57114, #16517, #25774, #54774, #5851 ) ) ;
#20130 = DIRECTION ( 'NONE',  ( 0.000000000000000000, 0.000000000000000000, -1.000000000000000000 ) ) ;
#20132 = CARTESIAN_POINT ( 'NONE',  ( 6.006483450353401921, 5.993516549646582092, 455.0000000000000568 ) ) ;
#20133 = CYLINDRICAL_SURFACE ( 'NONE', #55524, 0.5999999999999989786 ) ;
#20134 = CARTESIAN_POINT ( 'NONE',  ( 3.606483450353369147, -7.428221114745003462, 195.0000000000000284 ) ) ;
#20135 = ORIENTED_EDGE ( 'NONE', *, *, #46614, .T. ) ;
#20136 = DIRECTION ( 'NONE',  ( -0.000000000000000000, -0.000000000000000000, -1.000000000000000000 ) ) ;
#20137 = LINE ( 'NONE', #47007, #64506 ) ;
#20138 = EDGE_LOOP ( 'NONE', ( #20291, #4540, #29372, #30163 ) ) ;
#20139 = CARTESIAN_POINT ( 'NONE',  ( 24.90000000000000213, -14.06939075806900163, -20.80000000000000426 ) ) ;
#20140 = LINE ( 'NONE', #51968, #9800 ) ;
#20141 = DIRECTION ( 'NONE',  ( -1.000000000000000000, 0.000000000000000000, 0.000000000000000000 ) ) ;
#20142 = CARTESIAN_POINT ( 'NONE',  ( -25.50000000000000355, -17.50000000000000000, 22.50000000000000000 ) ) ;
#20143 = EDGE_CURVE ( 'NONE', #43590, #10241, #28720, .T. ) ;
#20144 = AXIS2_PLACEMENT_3D ( 'NONE', #58670, #2900, #42394 ) ;
#20145 = DIRECTION ( 'NONE',  ( -1.000000000000000000, 0.000000000000000000, 0.000000000000000000 ) ) ;
#20146 = ORIENTED_EDGE ( 'NONE', *, *, #22440, .F. ) ;
#20147 = ADVANCED_FACE ( 'NONE', ( #19161 ), #55946, .F. ) ;
#20148 = CARTESIAN_POINT ( 'NONE',  ( 275.0000000000000000, -20.50000000000000000, -13.00000000000000178 ) ) ;
#20149 = VERTEX_POINT ( 'NONE', #7501 ) ;
#20150 = VERTEX_POINT ( 'NONE', #56982 ) ;
#20151 = ORIENTED_EDGE ( 'NONE', *, *, #39373, .F. ) ;
#20152 = EDGE_CURVE ( 'NONE', #59443, #50308, #13857, .T. ) ;
#20153 = ORIENTED_EDGE ( 'NONE', *, *, #5169, .T. ) ;
#20154 = CARTESIAN_POINT ( 'NONE',  ( 39.90000000000000568, -14.48845687959340012, 21.00000000000000000 ) ) ;
#20155 = ADVANCED_FACE ( 'NONE', ( #17775 ), #34017, .T. ) ;
#20156 = EDGE_CURVE ( 'NONE', #22480, #51618, #44623, .T. ) ;
#20157 = CARTESIAN_POINT ( 'NONE',  ( -3.593516549646701197, 7.415254214038210279, 195.0000000000000284 ) ) ;
#20158 = CYLINDRICAL_SURFACE ( 'NONE', #3926, 2.250000000000001776 ) ;
#20159 = ORIENTED_EDGE ( 'NONE', *, *, #30517, .F. ) ;
#20160 = ADVANCED_FACE ( 'NONE', ( #1858 ), #49940, .F. ) ;
#20161 = ORIENTED_EDGE ( 'NONE', *, *, #45546, .F. ) ;
#20162 = CYLINDRICAL_SURFACE ( 'NONE', #18248, 0.1749999999999998224 ) ;
#20164 = VERTEX_POINT ( 'NONE', #18105 ) ;
#20163 = EDGE_CURVE ( 'NONE', #11939, #31382, #66192, .T. ) ;
#20165 = ORIENTED_EDGE ( 'NONE', *, *, #60643, .T. ) ;
#20166 = DIRECTION ( 'NONE',  ( -1.836970198721029934E-16, -1.836970198721010706E-16, 1.000000000000000000 ) ) ;
#20167 = DIRECTION ( 'NONE',  ( 0.000000000000000000, 0.000000000000000000, 1.000000000000000000 ) ) ;
#20168 = CARTESIAN_POINT ( 'NONE',  ( 11.08848345035341687, 9.791916549646563439, 455.0000000000000568 ) ) ;
#20169 = ORIENTED_EDGE ( 'NONE', *, *, #40054, .T. ) ;
#20170 = DIRECTION ( 'NONE',  ( 0.000000000000000000, 0.000000000000000000, -1.000000000000000000 ) ) ;
#20172 = DIRECTION ( 'NONE',  ( 0.4999999999999695799, -0.8660254037844563602, -6.723777587269172655E-17 ) ) ;
#20171 = DIRECTION ( 'NONE',  ( 0.000000000000000000, 0.000000000000000000, -1.000000000000000000 ) ) ;
#20173 = ORIENTED_EDGE ( 'NONE', *, *, #5480, .F. ) ;
#20175 = ORIENTED_EDGE ( 'NONE', *, *, #815, .T. ) ;
#20174 = LINE ( 'NONE', #64031, #69186 ) ;
#20176 = ORIENTED_EDGE ( 'NONE', *, *, #24471, .F. ) ;
#20177 = CIRCLE ( 'NONE', #59693, 1.000000000000000000 ) ;
#20178 = DIRECTION ( 'NONE',  ( 0.000000000000000000, 0.000000000000000000, 1.000000000000000000 ) ) ;
#20179 = AXIS2_PLACEMENT_3D ( 'NONE', #9107, #68512, #20760 ) ;
#20180 = CARTESIAN_POINT ( 'NONE',  ( -11.18999999999999950, -11.25000000000000000, -5.000000000000000000 ) ) ;
#20181 = ORIENTED_EDGE ( 'NONE', *, *, #43320, .T. ) ;
#20182 = VERTEX_POINT ( 'NONE', #61578 ) ;
#20183 = VECTOR ( 'NONE', #11489, 1000.000000000000000 ) ;
#20184 = CARTESIAN_POINT ( 'NONE',  ( 9.690000000000001279, 9.750000000000001776, -7.000000000000000000 ) ) ;
#20185 = LINE ( 'NONE', #53081, #22110 ) ;
#20186 = ORIENTED_EDGE ( 'NONE', *, *, #68874, .T. ) ;
#20187 = VERTEX_POINT ( 'NONE', #55603 ) ;
#20188 = DIRECTION ( 'NONE',  ( 1.000000000000000000, -1.047444401652939849E-14, 1.836970198721010706E-16 ) ) ;
#20189 = LINE ( 'NONE', #14535, #30516 ) ;
#20190 = VERTEX_POINT ( 'NONE', #13154 ) ;
#20191 = VECTOR ( 'NONE', #13860, 1000.000000000000000 ) ;
#20192 = DIRECTION ( 'NONE',  ( 0.000000000000000000, -3.673940397442059868E-16, 1.000000000000000000 ) ) ;
#20193 = CYLINDRICAL_SURFACE ( 'NONE', #11390, 1.224999999999998757 ) ;
#20195 = VERTEX_POINT ( 'NONE', #56295 ) ;
#20194 = CARTESIAN_POINT ( 'NONE',  ( -7.252248008019485326, -6.619341603356823533, 195.0000000000000284 ) ) ;
#20196 = VERTEX_POINT ( 'NONE', #1501 ) ;
#20197 = CARTESIAN_POINT ( 'NONE',  ( -8.250000000000001776, -7.249999999999998224, -26.00000000000001066 ) ) ;
#20198 = ADVANCED_FACE ( 'NONE', ( #50640 ), #2203, .F. ) ;
#20199 = CYLINDRICAL_SURFACE ( 'NONE', #27301, 4.000000000000000000 ) ;
#20200 = DIRECTION ( 'NONE',  ( -0.000000000000000000, 1.000000000000000000, 3.673940397442059868E-16 ) ) ;
#20201 = CARTESIAN_POINT ( 'NONE',  ( 5.257023737882795977, 5.242976262117205799, 26.00000000000000711 ) ) ;
#20202 = FACE_OUTER_BOUND ( 'NONE', #37454, .T. ) ;
#20203 = ADVANCED_FACE ( 'NONE', ( #39669 ), #40238, .T. ) ;
#20204 = CARTESIAN_POINT ( 'NONE',  ( -12.00000000000000000, 11.18999999999999950, 0.000000000000000000 ) ) ;
#20205 = ORIENTED_EDGE ( 'NONE', *, *, #8892, .T. ) ;
#20206 = DIRECTION ( 'NONE',  ( 0.000000000000000000, 1.000000000000000000, -0.000000000000000000 ) ) ;
#20208 = ORIENTED_EDGE ( 'NONE', *, *, #66271, .F. ) ;
#20207 = PLANE ( 'NONE',  #31125 ) ;
#20209 = CARTESIAN_POINT ( 'NONE',  ( 39.00000000000000000, 16.96999999999999886, -21.00000000000000000 ) ) ;
#20210 = CARTESIAN_POINT ( 'NONE',  ( 4.747751991980625696, -5.393625297350043368, 455.0000000000000568 ) ) ;
#20211 = DIRECTION ( 'NONE',  ( -1.000000000000000000, 0.000000000000000000, -0.000000000000000000 ) ) ;
#20212 = EDGE_CURVE ( 'NONE', #54442, #53865, #67256, .T. ) ;
#20213 = CARTESIAN_POINT ( 'NONE',  ( -8.250000000000001776, -7.249999999999998224, -26.00000000000001066 ) ) ;
#20214 = VERTEX_POINT ( 'NONE', #23769 ) ;
#20215 = DIRECTION ( 'NONE',  ( 0.000000000000000000, 0.000000000000000000, 1.000000000000000000 ) ) ;
#20216 = PLANE ( 'NONE',  #20380 ) ;
#20217 = ADVANCED_FACE ( 'NONE', ( #34720 ), #45320, .T. ) ;
#20218 = ORIENTED_EDGE ( 'NONE', *, *, #37103, .T. ) ;
#20219 = AXIS2_PLACEMENT_3D ( 'NONE', #32011, #54274, #60249 ) ;
#20220 = DIRECTION ( 'NONE',  ( 1.000000000000000000, 0.000000000000000000, 0.000000000000000000 ) ) ;
#20221 = DIRECTION ( 'NONE',  ( -0.000000000000000000, 3.673940397442059868E-16, -1.000000000000000000 ) ) ;
#20222 = CIRCLE ( 'NONE', #56357, 0.2999999999998732569 ) ;
#20223 = DIRECTION ( 'NONE',  ( 0.7671651518152998728, -0.6414496315691575745, 2.309356642088859447E-17 ) ) ;
#20224 = ORIENTED_EDGE ( 'NONE', *, *, #26624, .F. ) ;
#20225 = EDGE_CURVE ( 'NONE', #35907, #38480, #13506, .T. ) ;
#20226 = DIRECTION ( 'NONE',  ( -0.000000000000000000, -0.000000000000000000, -1.000000000000000000 ) ) ;
#20227 = ORIENTED_EDGE ( 'NONE', *, *, #14647, .F. ) ;
#20228 = ORIENTED_EDGE ( 'NONE', *, *, #69159, .T. ) ;
#20229 = CIRCLE ( 'NONE', #60844, 0.1999999999999987899 ) ;
#20230 = DIRECTION ( 'NONE',  ( 0.000000000000000000, 1.000000000000000000, 0.000000000000000000 ) ) ;
#20231 = CYLINDRICAL_SURFACE ( 'NONE', #30864, 0.5999999999999998668 ) ;
#20232 = CARTESIAN_POINT ( 'NONE',  ( 8.250000000000005329, -7.249999999999998224, -16.50000000000000000 ) ) ;
#20233 = AXIS2_PLACEMENT_3D ( 'NONE', #52195, #26035, #57148 ) ;
#20234 = CARTESIAN_POINT ( 'NONE',  ( -7.250000000000001776, -7.249999999999998224, -18.50000000000000000 ) ) ;
#20235 = LINE ( 'NONE', #52792, #49853 ) ;
#20236 = EDGE_LOOP ( 'NONE', ( #30334, #37928, #18297, #63634 ) ) ;
#20237 = EDGE_CURVE ( 'NONE', #27218, #17399, #56643, .T. ) ;
#20238 = ORIENTED_EDGE ( 'NONE', *, *, #48788, .F. ) ;
#20240 = VERTEX_POINT ( 'NONE', #36475 ) ;
#20239 = DIRECTION ( 'NONE',  ( 0.000000000000000000, 1.000000000000000000, 0.000000000000000000 ) ) ;
#20242 = ORIENTED_EDGE ( 'NONE', *, *, #53090, .F. ) ;
#20241 = EDGE_CURVE ( 'NONE', #7082, #46721, #4661, .T. ) ;
#20244 = AXIS2_PLACEMENT_3D ( 'NONE', #15692, #59517, #38302 ) ;
#20243 = VECTOR ( 'NONE', #38817, 1000.000000000000000 ) ;
#20245 = DIRECTION ( 'NONE',  ( 0.7142857142857395036, 0.000000000000000000, 0.6998542122237394469 ) ) ;
#20246 = LINE ( 'NONE', #30858, #29772 ) ;
#20247 = DIRECTION ( 'NONE',  ( -1.000000000000000000, 2.602085213965213008E-15, 0.000000000000000000 ) ) ;
#20248 = CARTESIAN_POINT ( 'NONE',  ( 7.250000000000004441, 8.750000000000001776, -30.00000000000001066 ) ) ;
#20249 = AXIS2_PLACEMENT_3D ( 'NONE', #38898, #10998, #28285 ) ;
#20251 = LINE ( 'NONE', #41815, #31216 ) ;
#20250 = CYLINDRICAL_SURFACE ( 'NONE', #39962, 2.215251240775983899 ) ;
#20252 = VERTEX_POINT ( 'NONE', #19506 ) ;
#20253 = EDGE_CURVE ( 'NONE', #1592, #34851, #3251, .T. ) ;
#20254 = ORIENTED_EDGE ( 'NONE', *, *, #8666, .T. ) ;
#20255 = ORIENTED_EDGE ( 'NONE', *, *, #47918, .T. ) ;
#20256 = EDGE_LOOP ( 'NONE', ( #22021, #6771, #17920, #29701 ) ) ;
#20257 = CARTESIAN_POINT ( 'NONE',  ( -0.9414762621172296786, 9.390476262117148920, 54.00000000000000711 ) ) ;
#20258 = LINE ( 'NONE', #41822, #45648 ) ;
#20259 = DIRECTION ( 'NONE',  ( -1.836970198721029934E-16, 1.836970198721036590E-16, -1.000000000000000000 ) ) ;
#20260 = EDGE_LOOP ( 'NONE', ( #61680, #50745, #56449, #17768 ) ) ;
#20261 = ORIENTED_EDGE ( 'NONE', *, *, #13677, .T. ) ;
#20262 = ORIENTED_EDGE ( 'NONE', *, *, #56325, .T. ) ;
#20263 = FACE_OUTER_BOUND ( 'NONE', #1550, .T. ) ;
#20264 = VERTEX_POINT ( 'NONE', #63005 ) ;
#20265 = ORIENTED_EDGE ( 'NONE', *, *, #28835, .T. ) ;
#20266 = CARTESIAN_POINT ( 'NONE',  ( 0.000000000000000000, -7.449999999999998401, -16.50000000000000000 ) ) ;
#20267 = VERTEX_POINT ( 'NONE', #9615 ) ;
#20268 = EDGE_CURVE ( 'NONE', #5139, #45732, #8653, .T. ) ;
#20269 = ORIENTED_EDGE ( 'NONE', *, *, #2553, .F. ) ;
#20270 = DIRECTION ( 'NONE',  ( 1.000000000000000000, 0.000000000000000000, 0.000000000000000000 ) ) ;
#20272 = ORIENTED_EDGE ( 'NONE', *, *, #12868, .T. ) ;
#20271 = DIRECTION ( 'NONE',  ( -0.000000000000000000, -0.000000000000000000, -1.000000000000000000 ) ) ;
#20273 = AXIS2_PLACEMENT_3D ( 'NONE', #61706, #35528, #19619 ) ;
#20274 = ORIENTED_EDGE ( 'NONE', *, *, #14844, .T. ) ;
#20275 = VECTOR ( 'NONE', #57292, 1000.000000000000000 ) ;
#20276 = EDGE_CURVE ( 'NONE', #26452, #52164, #3606, .T. ) ;
#20277 = PLANE ( 'NONE',  #13733 ) ;
#20278 = DIRECTION ( 'NONE',  ( 0.000000000000000000, 0.000000000000000000, 1.000000000000000000 ) ) ;
#20279 = EDGE_CURVE ( 'NONE', #18478, #68006, #52769, .T. ) ;
#20281 = ORIENTED_EDGE ( 'NONE', *, *, #29057, .T. ) ;
#20280 = DIRECTION ( 'NONE',  ( 0.000000000000000000, 0.000000000000000000, -1.000000000000000000 ) ) ;
#20282 = EDGE_LOOP ( 'NONE', ( #55830, #11529, #9630, #27605 ) ) ;
#20283 = VECTOR ( 'NONE', #39246, 1000.000000000000000 ) ;
#20284 = LINE ( 'NONE', #26645, #47034 ) ;
#20285 = ADVANCED_FACE ( 'NONE', ( #37194 ), #42530, .T. ) ;
#20286 = DIRECTION ( 'NONE',  ( -1.000000000000000000, 0.000000000000000000, 0.000000000000000000 ) ) ;
#20287 = CARTESIAN_POINT ( 'NONE',  ( -17.00000000000000000, -16.28999999999999915, -14.50000000000000000 ) ) ;
#20288 = AXIS2_PLACEMENT_3D ( 'NONE', #34286, #61881, #46657 ) ;
#20289 = DIRECTION ( 'NONE',  ( 0.000000000000000000, 0.000000000000000000, 1.000000000000000000 ) ) ;
#20290 = EDGE_CURVE ( 'NONE', #6502, #69903, #69351, .T. ) ;
#20291 = ORIENTED_EDGE ( 'NONE', *, *, #20865, .F. ) ;
#20292 = DIRECTION ( 'NONE',  ( -1.000000000000000000, 0.000000000000000000, 0.000000000000000000 ) ) ;
#20293 = AXIS2_PLACEMENT_3D ( 'NONE', #57441, #20652, #3349 ) ;
#20294 = CARTESIAN_POINT ( 'NONE',  ( 8.250000000000005329, 0.000000000000000000, -25.00000000000000000 ) ) ;
#20295 = SURFACE_SIDE_STYLE ('',( #37273 ) ) ;
#20296 = EDGE_LOOP ( 'NONE', ( #640, #51487, #24565, #20092 ) ) ;
#20297 = ADVANCED_FACE ( 'NONE', ( #36122 ), #46379, .T. ) ;
#20298 = DIRECTION ( 'NONE',  ( 0.000000000000000000, 0.000000000000000000, 1.000000000000000000 ) ) ;
#20299 = ADVANCED_FACE ( 'NONE', ( #31190 ), #63358, .F. ) ;
#20300 = CARTESIAN_POINT ( 'NONE',  ( 7.000000000000000000, -21.00000000000000000, 4.000000000000000000 ) ) ;
#20301 = CIRCLE ( 'NONE', #56424, 0.1999999999999996503 ) ;
#20302 = CARTESIAN_POINT ( 'NONE',  ( -6.350872789121327244, 3.663616288756986084, 54.00000000000000711 ) ) ;
#20303 = ADVANCED_FACE ( 'NONE', ( #14206 ), #3959, .F. ) ;
#20304 = EDGE_CURVE ( 'NONE', #46696, #31922, #62864, .T. ) ;
#20305 = VERTEX_POINT ( 'NONE', #30824 ) ;
#20306 = FILL_AREA_STYLE_COLOUR ( '', #13288 ) ;
#20307 = DIRECTION ( 'NONE',  ( 1.000000000000000000, -0.000000000000000000, -0.000000000000000000 ) ) ;
#20308 = ADVANCED_FACE ( 'NONE', ( #25531 ), #42123, .F. ) ;
#20309 = CARTESIAN_POINT ( 'NONE',  ( -7.744988412222854279, 8.452095193409293827, 455.0000000000000568 ) ) ;
#20310 = ORIENTED_EDGE ( 'NONE', *, *, #67400, .T. ) ;
#20311 = AXIS2_PLACEMENT_3D ( 'NONE', #43134, #17905, #50770 ) ;
#20312 = LINE ( 'NONE', #31293, #64319 ) ;
#20313 = LINE ( 'NONE', #20654, #47830 ) ;
#20314 = DIRECTION ( 'NONE',  ( 6.508391731846281342E-15, 1.000000000000000000, 0.000000000000000000 ) ) ;
#20315 = CARTESIAN_POINT ( 'NONE',  ( -3.142976262117280317, -5.257023737882827952, 54.00000000000000711 ) ) ;
#20316 = CARTESIAN_POINT ( 'NONE',  ( 146.5599459900709860, 9.000000000000001776, 284.4801873289890182 ) ) ;
#20317 = ORIENTED_EDGE ( 'NONE', *, *, #45495, .T. ) ;
#20318 = DIRECTION ( 'NONE',  ( 0.000000000000000000, -5.800915303574361727E-12, -1.000000000000000000 ) ) ;
#20319 = CARTESIAN_POINT ( 'NONE',  ( 8.249999999999996447, 8.250000000000001776, 5.000000000000000000 ) ) ;
#20320 = CARTESIAN_POINT ( 'NONE',  ( 11.00000000000000000, -17.14999999999900027, -26.64999999999900027 ) ) ;
#20321 = FACE_OUTER_BOUND ( 'NONE', #46691, .T. ) ;
#20322 = DIRECTION ( 'NONE',  ( -0.6414496315691592399, -0.7671651518152985405, 0.000000000000000000 ) ) ;
#20323 = ADVANCED_FACE ( 'NONE', ( #25881, #19856, #41429, #36846, #58415 ), #47782, .T. ) ;
#20324 = VERTEX_POINT ( 'NONE', #15627 ) ;
#20325 = VECTOR ( 'NONE', #39021, 1000.000000000000000 ) ;
#20327 = ORIENTED_EDGE ( 'NONE', *, *, #51339, .T. ) ;
#20326 = CARTESIAN_POINT ( 'NONE',  ( 8.930623737882818602, -10.05377373788281581, 26.00000000000000000 ) ) ;
#20328 = VECTOR ( 'NONE', #22522, 1000.000000000000000 ) ;
#20329 = EDGE_CURVE ( 'NONE', #49395, #7815, #9833, .T. ) ;
#20330 = CIRCLE ( 'NONE', #38400, 0.1749999999999989342 ) ;
#20331 = DIRECTION ( 'NONE',  ( 0.6414496315691526895, 0.7671651518153038696, 2.587583378555111534E-16 ) ) ;
#20332 = CARTESIAN_POINT ( 'NONE',  ( 11.50000000000000000, -11.50000000000100009, 10.50000000000065903 ) ) ;
#20333 = FACE_OUTER_BOUND ( 'NONE', #67655, .T. ) ;
#20334 = ORIENTED_EDGE ( 'NONE', *, *, #35690, .T. ) ;
#20335 = VECTOR ( 'NONE', #15872, 1000.000000000000000 ) ;
#20336 = CARTESIAN_POINT ( 'NONE',  ( 6.665817930929288870, 7.342976262117195674, 54.00000000000000711 ) ) ;
#20337 = FACE_OUTER_BOUND ( 'NONE', #23297, .T. ) ;
#20338 = ORIENTED_EDGE ( 'NONE', *, *, #2151, .T. ) ;
#20339 = ORIENTED_EDGE ( 'NONE', *, *, #45193, .F. ) ;
#20340 = VECTOR ( 'NONE', #65376, 1000.000000000000000 ) ;
#20341 = ORIENTED_EDGE ( 'NONE', *, *, #3469, .F. ) ;
#20342 = CARTESIAN_POINT ( 'NONE',  ( 25.50000000000000355, -15.50000000000000000, 22.50000000000000000 ) ) ;
#20343 = CIRCLE ( 'NONE', #47398, 0.2000000000000005107 ) ;
#20344 = CARTESIAN_POINT ( 'NONE',  ( -15.50000000000000000, 0.000000000000000000, 18.50000000000000000 ) ) ;
#20345 = DIRECTION ( 'NONE',  ( 1.000000000000000000, 0.000000000000000000, 0.000000000000000000 ) ) ;
#20346 = ADVANCED_FACE ( 'NONE', ( #16305 ), #43868, .F. ) ;
#20347 = ORIENTED_EDGE ( 'NONE', *, *, #27175, .T. ) ;
#20348 = VERTEX_POINT ( 'NONE', #69718 ) ;
#20349 = DIRECTION ( 'NONE',  ( -0.6414496315691617934, 0.7671651518152962090, 0.000000000000000000 ) ) ;
#20351 = LINE ( 'NONE', #41570, #1181 ) ;
#20350 = CIRCLE ( 'NONE', #29364, 0.3499999999998879008 ) ;
#20352 = ORIENTED_EDGE ( 'NONE', *, *, #39753, .F. ) ;
#20353 = ORIENTED_EDGE ( 'NONE', *, *, #46632, .T. ) ;
#20354 = ORIENTED_EDGE ( 'NONE', *, *, #2672, .T. ) ;
#20355 = ORIENTED_EDGE ( 'NONE', *, *, #11569, .T. ) ;
#20356 = CARTESIAN_POINT ( 'NONE',  ( -7.250000000000000000, -7.449999999999998401, -9.000000000000001776 ) ) ;
#20357 = UNCERTAINTY_MEASURE_WITH_UNIT (LENGTH_MEASURE( 1.000000000000000082E-05 ), #63624, 'distance_accuracy_value', 'NONE');
#20359 = ORIENTED_EDGE ( 'NONE', *, *, #29196, .T. ) ;
#20358 = LINE ( 'NONE', #9049, #46919 ) ;
#20360 = EDGE_CURVE ( 'NONE', #38019, #11471, #59444, .T. ) ;
#20361 = DIRECTION ( 'NONE',  ( -1.000000000000000000, 0.000000000000000000, 0.000000000000000000 ) ) ;
#20362 = DIRECTION ( 'NONE',  ( 0.000000000000000000, 0.000000000000000000, 1.000000000000000000 ) ) ;
#20363 = MANIFOLD_SOLID_BREP ( 'Boss-Extrude1', #48759 ) ;
#20364 = DIRECTION ( 'NONE',  ( 0.000000000000000000, 0.000000000000000000, 1.000000000000000000 ) ) ;
#20365 = ORIENTED_EDGE ( 'NONE', *, *, #16604, .T. ) ;
#20366 = EDGE_CURVE ( 'NONE', #4872, #49395, #53800, .T. ) ;
#20367 = ORIENTED_EDGE ( 'NONE', *, *, #57253, .T. ) ;
#20368 = EDGE_CURVE ( 'NONE', #41995, #25935, #6392, .T. ) ;
#20369 = FACE_OUTER_BOUND ( 'NONE', #34003, .T. ) ;
#20370 = EDGE_CURVE ( 'NONE', #19794, #10769, #49524, .T. ) ;
#20371 = PLANE ( 'NONE',  #51884 ) ;
#20372 = VECTOR ( 'NONE', #42104, 1000.000000000000000 ) ;
#20373 = VERTEX_POINT ( 'NONE', #1092 ) ;
#20374 = AXIS2_PLACEMENT_3D ( 'NONE', #5885, #33447, #27449 ) ;
#20375 = DIRECTION ( 'NONE',  ( 1.000000000000000000, -0.000000000000000000, 0.000000000000000000 ) ) ;
#20376 = DIRECTION ( 'NONE',  ( 0.000000000000000000, 0.000000000000000000, -1.000000000000000000 ) ) ;
#20377 = SURFACE_SIDE_STYLE ('',( #31700 ) ) ;
#20378 = VERTEX_POINT ( 'NONE', #54497 ) ;
#20379 = DIRECTION ( 'NONE',  ( 0.000000000000000000, 0.000000000000000000, 1.000000000000000000 ) ) ;
#20381 = CARTESIAN_POINT ( 'NONE',  ( -8.916576262117340335, -8.580623737882760338, 26.00000000000000000 ) ) ;
#20380 = AXIS2_PLACEMENT_3D ( 'NONE', #35418, #46044, #52777 ) ;
#20382 = DIRECTION ( 'NONE',  ( 0.000000000000000000, 0.000000000000000000, 1.000000000000000000 ) ) ;
#20383 = DIRECTION ( 'NONE',  ( 1.000000000000000000, -9.050731179009442381E-15, 0.000000000000000000 ) ) ;
#20384 = AXIS2_PLACEMENT_3D ( 'NONE', #56056, #40123, #67005 ) ;
#20385 = DIRECTION ( 'NONE',  ( -0.000000000000000000, 1.000000000000000000, -0.000000000000000000 ) ) ;
#20386 = ORIENTED_EDGE ( 'NONE', *, *, #11252, .T. ) ;
#20387 = DIRECTION ( 'NONE',  ( 1.000000000000000000, -0.000000000000000000, -0.000000000000000000 ) ) ;
#20389 = VECTOR ( 'NONE', #42543, 1000.000000000000000 ) ;
#20388 = DIRECTION ( 'NONE',  ( 0.000000000000000000, 1.000000000000000000, 0.000000000000000000 ) ) ;
#20390 = FILL_AREA_STYLE ('',( #62108 ) ) ;
#20391 = DIRECTION ( 'NONE',  ( 0.000000000000000000, 0.000000000000000000, -1.000000000000000000 ) ) ;
#20392 = CARTESIAN_POINT ( 'NONE',  ( 7.000000000000000000, -21.00000000000000000, 0.000000000000000000 ) ) ;
#20393 = CARTESIAN_POINT ( 'NONE',  ( 0.5000000000000000000, 21.00000000000000000, -18.00000000000000355 ) ) ;
#20394 = AXIS2_PLACEMENT_3D ( 'NONE', #19754, #3864, #24015 ) ;
#20395 = LINE ( 'NONE', #15455, #32406 ) ;
#20396 = DIRECTION ( 'NONE',  ( 0.000000000000000000, -0.000000000000000000, 1.000000000000000000 ) ) ;
#20397 = ORIENTED_EDGE ( 'NONE', *, *, #69155, .T. ) ;
#20398 = CARTESIAN_POINT ( 'NONE',  ( 6.619341603356837744, -7.265214908726242982, 455.0000000000000568 ) ) ;
#20399 = DIRECTION ( 'NONE',  ( 9.912705577010386883E-15, 1.000000000000000000, 0.000000000000000000 ) ) ;
#20400 = CARTESIAN_POINT ( 'NONE',  ( 15.50000000000000000, -0.4000000000000000222, 22.50000000000000000 ) ) ;
#20401 = FACE_OUTER_BOUND ( 'NONE', #3365, .T. ) ;
#20402 = DIRECTION ( 'NONE',  ( 0.000000000000000000, 1.000000000000000000, 3.673940397442059868E-16 ) ) ;
#20403 = DIRECTION ( 'NONE',  ( 1.000000000000000000, 0.000000000000000000, 0.000000000000000000 ) ) ;
#20404 = DIRECTION ( 'NONE',  ( -0.7671651518152985405, -0.6414496315691592399, 0.000000000000000000 ) ) ;
#20405 = EDGE_CURVE ( 'NONE', #45925, #40436, #52747, .T. ) ;
#20406 = ORIENTED_EDGE ( 'NONE', *, *, #58322, .T. ) ;
#20407 = EDGE_CURVE ( 'NONE', #44854, #14810, #6051, .T. ) ;
#20408 = ORIENTED_EDGE ( 'NONE', *, *, #30654, .T. ) ;
#20409 = DIRECTION ( 'NONE',  ( -0.000000000000000000, 0.000000000000000000, 1.000000000000000000 ) ) ;
#20410 = VECTOR ( 'NONE', #51132, 1000.000000000000000 ) ;
#20411 = CARTESIAN_POINT ( 'NONE',  ( 29.50000000000000355, -11.50000000000100009, 15.00000000000084910 ) ) ;
#20412 = ORIENTED_EDGE ( 'NONE', *, *, #49126, .F. ) ;
#20413 = EDGE_CURVE ( 'NONE', #4203, #6649, #43171, .T. ) ;
#20414 = CARTESIAN_POINT ( 'NONE',  ( -9.690000000000001279, -9.690000000000001279, -4.250000000000000000 ) ) ;
#20415 = CARTESIAN_POINT ( 'NONE',  ( 8.406483450353379183, -4.396432944014562416, 195.0000000000000284 ) ) ;
#20416 = VERTEX_POINT ( 'NONE', #42827 ) ;
#20417 = CARTESIAN_POINT ( 'NONE',  ( -11.00000000000000000, -12.00000000000000000, 10.20500000000000007 ) ) ;
#20418 = ORIENTED_EDGE ( 'NONE', *, *, #36371, .T. ) ;
#20419 = ORIENTED_EDGE ( 'NONE', *, *, #18313, .F. ) ;
#20420 = DIRECTION ( 'NONE',  ( -1.836970198721029934E-16, 1.836970198721036590E-16, -1.000000000000000000 ) ) ;
#20421 = VECTOR ( 'NONE', #9864, 1000.000000000000000 ) ;
#20422 = VERTEX_POINT ( 'NONE', #5711 ) ;
#20423 = DIRECTION ( 'NONE',  ( 1.000000000000000000, 0.000000000000000000, 0.000000000000000000 ) ) ;
#20424 = DIRECTION ( 'NONE',  ( 1.000000000000000000, 0.000000000000000000, 0.000000000000000000 ) ) ;
#20426 = LINE ( 'NONE', #3473, #63771 ) ;
#20425 = CIRCLE ( 'NONE', #36215, 0.1749999999999993783 ) ;
#20427 = EDGE_CURVE ( 'NONE', #37433, #25346, #15488, .T. ) ;
#20428 = ORIENTED_EDGE ( 'NONE', *, *, #10820, .F. ) ;
#20429 = AXIS2_PLACEMENT_3D ( 'NONE', #11681, #18368, #1772 ) ;
#20430 = CARTESIAN_POINT ( 'NONE',  ( 4.155633711806658859, -4.720772854004808394, 54.00000000000000711 ) ) ;
#20432 = CARTESIAN_POINT ( 'NONE',  ( 8.250000000000005329, -7.249999999999998224, -26.00000000000001066 ) ) ;
#20431 = CARTESIAN_POINT ( 'NONE',  ( -3.663616288757094885, -6.364920264886888113, 54.00000000000000711 ) ) ;
#20433 = VERTEX_POINT ( 'NONE', #60124 ) ;
#20434 = VERTEX_POINT ( 'NONE', #21956 ) ;
#20435 = EDGE_LOOP ( 'NONE', ( #53799, #31350, #6923, #52690, #37607, #21877, #22576 ) ) ;
#20436 = VECTOR ( 'NONE', #54955, 1000.000000000000000 ) ;
#20437 = CIRCLE ( 'NONE', #48817, 0.5249999999999994671 ) ;
#20439 = ORIENTED_EDGE ( 'NONE', *, *, #1795, .F. ) ;
#20438 = CONTEXT_DEPENDENT_SHAPE_REPRESENTATION ( #2945, #32944 ) ;
#20440 = DIRECTION ( 'NONE',  ( 1.836970198721029934E-16, 1.836970198721010706E-16, -1.000000000000000000 ) ) ;
#20442 = ORIENTED_EDGE ( 'NONE', *, *, #29986, .T. ) ;
#20441 = CARTESIAN_POINT ( 'NONE',  ( 41.09999999999999432, -21.00000000000000000, 13.86939075806900057 ) ) ;
#20443 = VECTOR ( 'NONE', #28071, 1000.000000000000114 ) ;
#20444 = EDGE_CURVE ( 'NONE', #26978, #17145, #43518, .T. ) ;
#20445 = DIRECTION ( 'NONE',  ( 1.000000000000000000, -0.000000000000000000, 0.000000000000000000 ) ) ;
#20446 = PLANE ( 'NONE',  #54292 ) ;
#20447 = VERTEX_POINT ( 'NONE', #16669 ) ;
#20448 = VERTEX_POINT ( 'NONE', #27608 ) ;
#20449 = AXIS2_PLACEMENT_3D ( 'NONE', #5606, #55430, #28537 ) ;
#20450 = FACE_OUTER_BOUND ( 'NONE', #41281, .T. ) ;
#20451 = EDGE_CURVE ( 'NONE', #27517, #55865, #61743, .T. ) ;
#20452 = ADVANCED_FACE ( 'NONE', ( #65443 ), #33265, .T. ) ;
#20453 = ORIENTED_EDGE ( 'NONE', *, *, #21036, .F. ) ;
#20454 = CARTESIAN_POINT ( 'NONE',  ( 8.930623737882848800, 9.689726262117154931, 54.00000000000000711 ) ) ;
#20455 = DIRECTION ( 'NONE',  ( -0.000000000000000000, -0.000000000000000000, -1.000000000000000000 ) ) ;
#20456 = EDGE_CURVE ( 'NONE', #35831, #20091, #50564, .T. ) ;
#20457 = CARTESIAN_POINT ( 'NONE',  ( -11.07551654964682086, -10.20488345035337296, 455.0000000000000568 ) ) ;
#20458 = EDGE_CURVE ( 'NONE', #12841, #2217, #17689, .T. ) ;
#20459 = VERTEX_POINT ( 'NONE', #33934 ) ;
#20460 = EDGE_CURVE ( 'NONE', #21898, #59501, #50205, .T. ) ;
#20461 = CYLINDRICAL_SURFACE ( 'NONE', #1901, 1.000000000000000888 ) ;
#20462 = VECTOR ( 'NONE', #8702, 1000.000000000000000 ) ;
#20464 = ORIENTED_EDGE ( 'NONE', *, *, #35520, .F. ) ;
#20463 = DIRECTION ( 'NONE',  ( -1.000000000000000000, 0.000000000000000000, 0.000000000000000000 ) ) ;
#20466 = ORIENTED_EDGE ( 'NONE', *, *, #55642, .F. ) ;
#20465 = CARTESIAN_POINT ( 'NONE',  ( -4.135079735113214916, -6.836383711243002814, 54.00000000000000711 ) ) ;
#20467 = CARTESIAN_POINT ( 'NONE',  ( 6.006483450353353959, 5.993516549646629166, 195.0000000000000284 ) ) ;
#20468 = CARTESIAN_POINT ( 'NONE',  ( 7.000000000000000000, -20.40000000000000213, 12.40000000000000213 ) ) ;
#20469 = LINE ( 'NONE', #46991, #47107 ) ;
#20470 = CARTESIAN_POINT ( 'NONE',  ( 21.90000000000000213, -0.000000000000000000, -20.80000000000000426 ) ) ;
#20471 = CARTESIAN_POINT ( 'NONE',  ( -7.593516549646784242, -11.32648345035336312, 195.0000000000000284 ) ) ;
#20472 = VERTEX_POINT ( 'NONE', #45586 ) ;
#20473 = LINE ( 'NONE', #68917, #19921 ) ;
#20474 = CARTESIAN_POINT ( 'NONE',  ( -9.722976262117258628, 3.667976262117184749, 54.00000000000000711 ) ) ;
#20475 = AXIS2_PLACEMENT_3D ( 'NONE', #15694, #21339, #10724 ) ;
#20477 = EDGE_LOOP ( 'NONE', ( #58618, #55124, #11532, #21087, #7879, #59035, #21868 ) ) ;
#20476 = FACE_OUTER_BOUND ( 'NONE', #68532, .T. ) ;
#20478 = VECTOR ( 'NONE', #31948, 1000.000000000000000 ) ;
#20479 = FACE_OUTER_BOUND ( 'NONE', #43234, .T. ) ;
#20480 = CARTESIAN_POINT ( 'NONE',  ( 7.250000000000005329, 7.250000000000000888, -15.50000000000000000 ) ) ;
#20481 = DIRECTION ( 'NONE',  ( -1.000000000000000000, 0.000000000000000000, 0.000000000000000000 ) ) ;
#20482 = ORIENTED_EDGE ( 'NONE', *, *, #46930, .F. ) ;
#20483 = CARTESIAN_POINT ( 'NONE',  ( 0.5000000000000000000, 21.00000000000000000, 18.00000000000000355 ) ) ;
#20484 = LINE ( 'NONE', #53031, #1252 ) ;
#20485 = ORIENTED_EDGE ( 'NONE', *, *, #23734, .F. ) ;
#20486 = LINE ( 'NONE', #58678, #41285 ) ;
#20487 = VECTOR ( 'NONE', #6422, 1000.000000000000114 ) ;
#20488 = AXIS2_PLACEMENT_3D ( 'NONE', #56761, #52169, #57815 ) ;
#20489 = LINE ( 'NONE', #31469, #27700 ) ;
#20490 = DIRECTION ( 'NONE',  ( -0.000000000000000000, 3.673940397442059868E-16, -1.000000000000000000 ) ) ;
#20491 = DIRECTION ( 'NONE',  ( 0.6414496315691494699, -0.7671651518153064231, 0.000000000000000000 ) ) ;
#20492 = AXIS2_PLACEMENT_3D ( 'NONE', #52795, #8574, #35439 ) ;
#20493 = CARTESIAN_POINT ( 'NONE',  ( -7.250000000000000888, 7.250000000000001776, -25.00000000000000000 ) ) ;
#20494 = ORIENTED_EDGE ( 'NONE', *, *, #8576, .F. ) ;
#20495 = ORIENTED_EDGE ( 'NONE', *, *, #16369, .F. ) ;
#20496 = DIRECTION ( 'NONE',  ( -1.000000000000000000, 7.665540703601094997E-15, 0.000000000000000000 ) ) ;
#20497 = ORIENTED_EDGE ( 'NONE', *, *, #34594, .F. ) ;
#20498 = ORIENTED_EDGE ( 'NONE', *, *, #13681, .F. ) ;
#20499 = EDGE_CURVE ( 'NONE', #50, #11776, #29675, .T. ) ;
#20500 = DIRECTION ( 'NONE',  ( -0.000000000000000000, -0.000000000000000000, -1.000000000000000000 ) ) ;
#20501 = ADVANCED_FACE ( 'NONE', ( #66808 ), #28293, .T. ) ;
#20502 = AXIS2_PLACEMENT_3D ( 'NONE', #66893, #13156, #34722 ) ;
#20503 = ADVANCED_FACE ( 'NONE', ( #39926 ), #33604, .F. ) ;
#20504 = CARTESIAN_POINT ( 'NONE',  ( 9.929523737882817613, -0.9555237378828257411, 54.00000000000000711 ) ) ;
#20505 = DIRECTION ( 'NONE',  ( 0.000000000000000000, 0.000000000000000000, 1.000000000000000000 ) ) ;
#20506 = VERTEX_POINT ( 'NONE', #7412 ) ;
#20507 = EDGE_LOOP ( 'NONE', ( #62245, #159, #46869, #58806 ) ) ;
#20508 = CARTESIAN_POINT ( 'NONE',  ( -6.350872789121319251, -3.677663764522589140, 54.00000000000000711 ) ) ;
#20509 = ORIENTED_EDGE ( 'NONE', *, *, #22383, .T. ) ;
#20510 = VERTEX_POINT ( 'NONE', #23674 ) ;
#20511 = CARTESIAN_POINT ( 'NONE',  ( -8.250000000000000000, 7.250000000000001776, -12.00000000000000000 ) ) ;
#20512 = CARTESIAN_POINT ( 'NONE',  ( 46.39999999999999858, 21.00000000000000000, 2.250000000000000444 ) ) ;
#20513 = CARTESIAN_POINT ( 'NONE',  ( 10.92648345035337343, -2.706483450353490916, 455.0000000000000568 ) ) ;
#20514 = VECTOR ( 'NONE', #46105, 1000.000000000000000 ) ;
#20515 = ORIENTED_EDGE ( 'NONE', *, *, #19975, .F. ) ;
#20516 = PLANE ( 'NONE',  #49226 ) ;
#20518 = CARTESIAN_POINT ( 'NONE',  ( 20.90000000000000213, -0.1999999999911795112, 8.826273045769999343E-12 ) ) ;
#20517 = DIRECTION ( 'NONE',  ( -1.000000000000000000, 1.047444401652940007E-14, -1.836970198721010706E-16 ) ) ;
#20519 = ORIENTED_EDGE ( 'NONE', *, *, #18158, .T. ) ;
#20521 = VERTEX_POINT ( 'NONE', #60811 ) ;
#20520 = CARTESIAN_POINT ( 'NONE',  ( 5.793274621760843957, -4.155633711806670405, 54.00000000000000711 ) ) ;
#20522 = ORIENTED_EDGE ( 'NONE', *, *, #66910, .T. ) ;
#20523 = CARTESIAN_POINT ( 'NONE',  ( 25.57999999999999829, 6.429395695523604153E-16, -5.250000000000000000 ) ) ;
#20524 = CIRCLE ( 'NONE', #13745, 0.3499999999998866795 ) ;
#20525 = CARTESIAN_POINT ( 'NONE',  ( 0.000000000000000000, -21.00000000000000000, 0.000000000000000000 ) ) ;
#20526 = AXIS2_PLACEMENT_3D ( 'NONE', #21600, #53784, #54476 ) ;
#20527 = ORIENTED_EDGE ( 'NONE', *, *, #45339, .T. ) ;
#20528 = CARTESIAN_POINT ( 'NONE',  ( 11.00000000000000000, -14.34000000000000163, -14.50000000000000178 ) ) ;
#20529 = CARTESIAN_POINT ( 'NONE',  ( 6.665817930929297752, -7.357023737882824044, 54.00000000000000711 ) ) ;
#20530 = ORIENTED_EDGE ( 'NONE', *, *, #44360, .T. ) ;
#20531 = AXIS2_PLACEMENT_3D ( 'NONE', #59644, #60316, #11191 ) ;
#20532 = VECTOR ( 'NONE', #26164, 1000.000000000000114 ) ;
#20533 = EDGE_LOOP ( 'NONE', ( #65549, #24042, #38762, #42650 ) ) ;
#20534 = CARTESIAN_POINT ( 'NONE',  ( 39.00000000000000000, -16.96999999999999886, -21.00000000000000000 ) ) ;
#20535 = DIRECTION ( 'NONE',  ( 0.000000000000000000, 0.000000000000000000, -1.000000000000000000 ) ) ;
#20536 = EDGE_CURVE ( 'NONE', #39955, #49881, #57207, .T. ) ;
#20537 = EDGE_LOOP ( 'NONE', ( #29260, #4854, #26693, #1091 ) ) ;
#20538 = AXIS2_PLACEMENT_3D ( 'NONE', #9557, #62951, #35711 ) ;
#20539 = EDGE_CURVE ( 'NONE', #18238, #42804, #26735, .T. ) ;
#20540 = EDGE_CURVE ( 'NONE', #36929, #52415, #49863, .T. ) ;
#20541 = DIRECTION ( 'NONE',  ( 8.673617379884051249E-15, 1.000000000000000000, 0.000000000000000000 ) ) ;
#20542 = CARTESIAN_POINT ( 'NONE',  ( -10.49297626211725110, -3.664523737882711352, 54.00000000000000711 ) ) ;
#20543 = ADVANCED_FACE ( 'NONE', ( #28634 ), #51247, .F. ) ;
#20545 = EDGE_LOOP ( 'NONE', ( #26924, #10026, #29323, #9216 ) ) ;
#20544 = CARTESIAN_POINT ( 'NONE',  ( 3.677663764522614454, -4.149127210878770455, 54.00000000000000711 ) ) ;
#20547 = ORIENTED_EDGE ( 'NONE', *, *, #45271, .F. ) ;
#20546 = CARTESIAN_POINT ( 'NONE',  ( -7.250000000000000888, 7.250000000000001776, -25.50000000000000355 ) ) ;
#20549 = CARTESIAN_POINT ( 'NONE',  ( -11.50000000000000000, -11.50000000000000000, 15.00000000000000000 ) ) ;
#20548 = AXIS2_PLACEMENT_3D ( 'NONE', #49184, #22988, #2122 ) ;
#20550 = LINE ( 'NONE', #46366, #34074 ) ;
#20551 = CARTESIAN_POINT ( 'NONE',  ( -4.188533722949335569, 7.259684009079808931, 455.0000000000000568 ) ) ;
#20552 = CARTESIAN_POINT ( 'NONE',  ( -1.677516549646825839, -10.74648345035347141, 455.0000000000000568 ) ) ;
#20553 = PRODUCT_DEFINITION ( 'UNKNOWN', '', #56169, #29620 ) ;
#20554 = DIRECTION ( 'NONE',  ( 8.951101527228104953E-17, 1.000000000000000000, -0.000000000000000000 ) ) ;
#20555 = EDGE_CURVE ( 'NONE', #66065, #26683, #2461, .T. ) ;
#20556 = LINE ( 'NONE', #14548, #69916 ) ;
#20557 = ORIENTED_EDGE ( 'NONE', *, *, #65780, .F. ) ;
#20558 = DIRECTION ( 'NONE',  ( 1.901462112903059913E-14, 1.000000000000000000, 1.836970198721045958E-16 ) ) ;
#20559 = EDGE_CURVE ( 'NONE', #35542, #49922, #2809, .T. ) ;
#20561 = VERTEX_POINT ( 'NONE', #12356 ) ;
#20560 = FILL_AREA_STYLE_COLOUR ( '', #22084 ) ;
#20562 = CARTESIAN_POINT ( 'NONE',  ( -8.452095193409439489, -7.757955312929496472, 195.0000000000000284 ) ) ;
#20563 = CARTESIAN_POINT ( 'NONE',  ( 10.50702373788281996, -6.849523737882814878, 26.00000000000000000 ) ) ;
#20564 = DIRECTION ( 'NONE',  ( 0.000000000000000000, -1.901256929667036381E-12, 1.000000000000000000 ) ) ;
#20565 = DIRECTION ( 'NONE',  ( -1.000000000000000000, -0.000000000000000000, -0.000000000000000000 ) ) ;
#20566 = VERTEX_POINT ( 'NONE', #24025 ) ;
#20567 = CARTESIAN_POINT ( 'NONE',  ( 41.09999999999999432, 13.66939075806899950, -20.80000000000000426 ) ) ;
#20568 = DIRECTION ( 'NONE',  ( -0.6414496315691565753, 0.7671651518153006499, 0.000000000000000000 ) ) ;
#20569 = AXIS2_PLACEMENT_3D ( 'NONE', #38783, #49056, #21487 ) ;
#20570 = VERTEX_POINT ( 'NONE', #61866 ) ;
#20571 = DIRECTION ( 'NONE',  ( 0.000000000000000000, 0.000000000000000000, 1.000000000000000000 ) ) ;
#20572 = FACE_OUTER_BOUND ( 'NONE', #50676, .T. ) ;
#20573 = VECTOR ( 'NONE', #59341, 1000.000000000000000 ) ;
#20574 = CYLINDRICAL_SURFACE ( 'NONE', #45461, 0.1999999999999996503 ) ;
#20575 = ORIENTED_EDGE ( 'NONE', *, *, #56460, .F. ) ;
#20576 = CARTESIAN_POINT ( 'NONE',  ( 11.00000000000000000, -15.46862696659690073, -14.50000000000000000 ) ) ;
#20577 = ORIENTED_EDGE ( 'NONE', *, *, #10345, .F. ) ;
#20578 = ORIENTED_EDGE ( 'NONE', *, *, #42258, .T. ) ;
#20579 = CARTESIAN_POINT ( 'NONE',  ( 35.89999999999999858, 0.000000000000000000, 3.016910393003143647E-15 ) ) ;
#20580 = DIRECTION ( 'NONE',  ( -0.000000000000000000, 3.673940397442059868E-16, -1.000000000000000000 ) ) ;
#20581 = CARTESIAN_POINT ( 'NONE',  ( -11.00000000000000000, -13.54524521594299991, 17.53999999999999915 ) ) ;
#20582 = VECTOR ( 'NONE', #64949, 1000.000000000000000 ) ;
#20583 = EDGE_CURVE ( 'NONE', #1459, #8910, #55522, .T. ) ;
#20584 = DIRECTION ( 'NONE',  ( -0.7671651518153006499, -0.6414496315691565753, -2.356647714346250026E-16 ) ) ;
#20585 = DIRECTION ( 'NONE',  ( 0.000000000000000000, 0.000000000000000000, 1.000000000000000000 ) ) ;
#20586 = EDGE_LOOP ( 'NONE', ( #62871, #28036, #60932, #13956 ) ) ;
#20587 = VERTEX_POINT ( 'NONE', #39586 ) ;
#20589 = VERTEX_POINT ( 'NONE', #18725 ) ;
#20588 = DIRECTION ( 'NONE',  ( -1.000000000000000000, 0.000000000000000000, 0.000000000000000000 ) ) ;
#20590 = VERTEX_POINT ( 'NONE', #13424 ) ;
#20591 = CARTESIAN_POINT ( 'NONE',  ( 11.00000000000000000, -17.35230188589299871, 15.35019951917099945 ) ) ;
#20592 = DIRECTION ( 'NONE',  ( -0.000000000000000000, -0.000000000000000000, -1.000000000000000000 ) ) ;
#20593 = LINE ( 'NONE', #27641, #10494 ) ;
#20594 = AXIS2_PLACEMENT_3D ( 'NONE', #46295, #19766, #41342 ) ;
#20595 = DIRECTION ( 'NONE',  ( 0.000000000000000000, 0.000000000000000000, -1.000000000000000000 ) ) ;
#20596 = ADVANCED_FACE ( 'NONE', ( #40292 ), #23340, .F. ) ;
#20598 = CARTESIAN_POINT ( 'NONE',  ( -7.250000000000001776, -7.249999999999998224, -26.00000000000001066 ) ) ;
#20597 = DIRECTION ( 'NONE',  ( -1.000000000000000000, 0.000000000000000000, 0.000000000000000000 ) ) ;
#20599 = EDGE_LOOP ( 'NONE', ( #50616, #57614, #29263, #20075, #55134, #19362, #50674, #44862, #2490, #64187, #62404, #20915, #33857, #18226, #16879, #8338, #17807 ) ) ;
#20600 = EDGE_LOOP ( 'NONE', ( #54018, #6169, #37682, #31484 ) ) ;
#20601 = VERTEX_POINT ( 'NONE', #19764 ) ;
#20602 = ADVANCED_FACE ( 'NONE', ( #9886, #31459 ), #14832, .F. ) ;
#20603 = FACE_OUTER_BOUND ( 'NONE', #26456, .T. ) ;
#20604 = CARTESIAN_POINT ( 'NONE',  ( 0.000000000000000000, -8.249999999999998224, -23.00000000000000000 ) ) ;
#20605 = CYLINDRICAL_SURFACE ( 'NONE', #53476, 0.4000000000000010214 ) ;
#20606 = ORIENTED_EDGE ( 'NONE', *, *, #24803, .F. ) ;
#20607 = ORIENTED_EDGE ( 'NONE', *, *, #16728, .F. ) ;
#20608 = ORIENTED_EDGE ( 'NONE', *, *, #61380, .T. ) ;
#20609 = LINE ( 'NONE', #47151, #53149 ) ;
#20610 = VERTEX_POINT ( 'NONE', #41341 ) ;
#20611 = PLANE ( 'NONE',  #44635 ) ;
#20612 = CIRCLE ( 'NONE', #28521, 3.999999999999993339 ) ;
#20613 = EDGE_CURVE ( 'NONE', #44568, #57476, #25799, .T. ) ;
#20614 = VERTEX_POINT ( 'NONE', #62917 ) ;
#20615 = VERTEX_POINT ( 'NONE', #51611 ) ;
#20616 = CARTESIAN_POINT ( 'NONE',  ( 11.12648345035337982, -7.806483450353395526, 195.0000000000000284 ) ) ;
#20617 = AXIS2_PLACEMENT_3D ( 'NONE', #17159, #27777, #12874 ) ;
#20619 = ORIENTED_EDGE ( 'NONE', *, *, #40847, .F. ) ;
#20618 = CARTESIAN_POINT ( 'NONE',  ( -11.33351654964671162, 1.077516549646603483, 455.0000000000000568 ) ) ;
#20620 = EDGE_LOOP ( 'NONE', ( #26361, #39677, #67854, #46593 ) ) ;
#20621 = LINE ( 'NONE', #64140, #67960 ) ;
#20622 = EDGE_CURVE ( 'NONE', #15345, #13221, #14483, .T. ) ;
#20623 = CARTESIAN_POINT ( 'NONE',  ( -11.50000000000000000, -12.00000000000000000, 10.69999999999999929 ) ) ;
#20624 = EDGE_CURVE ( 'NONE', #2477, #29173, #41470, .T. ) ;
#20626 = ORIENTED_EDGE ( 'NONE', *, *, #60935, .T. ) ;
#20625 = CARTESIAN_POINT ( 'NONE',  ( -24.00000000000000000, -16.28999999999710369, 15.00000000000794920 ) ) ;
#20627 = ORIENTED_EDGE ( 'NONE', *, *, #39318, .F. ) ;
#20628 = CARTESIAN_POINT ( 'NONE',  ( -7.250000000000000888, 7.450000000000003730, -20.50000000000000000 ) ) ;
#20629 = DIRECTION ( 'NONE',  ( 1.000000000000000000, -0.000000000000000000, -0.000000000000000000 ) ) ;
#20630 = ADVANCED_FACE ( 'NONE', ( #4578 ), #69270, .T. ) ;
#20631 = CARTESIAN_POINT ( 'NONE',  ( 9.690000000000001279, -9.690000000000001279, -4.250000000000000000 ) ) ;
#20632 = LINE ( 'NONE', #9333, #30073 ) ;
#20633 = FACE_OUTER_BOUND ( 'NONE', #4623, .T. ) ;
#20634 = ADVANCED_FACE ( 'NONE', ( #68922 ), #3873, .T. ) ;
#20635 = ORIENTED_EDGE ( 'NONE', *, *, #57084, .T. ) ;
#20636 = CARTESIAN_POINT ( 'NONE',  ( -11.47551654964667733, 11.07551654964660237, 455.0000000000000568 ) ) ;
#20637 = EDGE_CURVE ( 'NONE', #37879, #35090, #14118, .T. ) ;
#20638 = ORIENTED_EDGE ( 'NONE', *, *, #39692, .F. ) ;
#20639 = DIRECTION ( 'NONE',  ( -0.7071067811865474617, 0.7071067811865474617, 2.597868168706479611E-16 ) ) ;
#20640 = AXIS2_PLACEMENT_3D ( 'NONE', #515, #22082, #43645 ) ;
#20641 = FACE_OUTER_BOUND ( 'NONE', #48802, .T. ) ;
#20642 = CARTESIAN_POINT ( 'NONE',  ( 18.89999999999999858, -21.00000000000000000, 13.86939075806900057 ) ) ;
#20644 = CARTESIAN_POINT ( 'NONE',  ( 13.00000000000000178, -16.64230188589299786, -14.64519951917100116 ) ) ;
#20643 = VECTOR ( 'NONE', #46131, 1000.000000000000000 ) ;
#20645 = DIRECTION ( 'NONE',  ( 1.000000000000000000, -0.000000000000000000, 0.000000000000000000 ) ) ;
#20646 = ADVANCED_FACE ( 'NONE', ( #20479 ), #56895, .F. ) ;
#20647 = ORIENTED_EDGE ( 'NONE', *, *, #10665, .F. ) ;
#20648 = AXIS2_PLACEMENT_3D ( 'NONE', #38810, #15869, #69956 ) ;
#20649 = CIRCLE ( 'NONE', #49969, 0.5250000000000003553 ) ;
#20650 = LINE ( 'NONE', #58510, #29296 ) ;
#20651 = ORIENTED_EDGE ( 'NONE', *, *, #29465, .F. ) ;
#20652 = DIRECTION ( 'NONE',  ( 0.000000000000000000, 0.000000000000000000, 1.000000000000000000 ) ) ;
#20653 = EDGE_CURVE ( 'NONE', #34278, #53158, #17741, .T. ) ;
#20654 = CARTESIAN_POINT ( 'NONE',  ( -17.00000000000000000, -17.35230188589299871, 15.35019951917099945 ) ) ;
#20655 = CARTESIAN_POINT ( 'NONE',  ( -6.822336235477446387, -4.149127210878696737, 54.00000000000000711 ) ) ;
#20656 = DIRECTION ( 'NONE',  ( 0.000000000000000000, 0.000000000000000000, -1.000000000000000000 ) ) ;
#20657 = CARTESIAN_POINT ( 'NONE',  ( -7.517976262117260333, 3.834182069070703580, 26.00000000000000711 ) ) ;
#20658 = ORIENTED_EDGE ( 'NONE', *, *, #62083, .T. ) ;
#20659 = CARTESIAN_POINT ( 'NONE',  ( -9.093516549646826874, -10.92648345035338941, 455.0000000000000568 ) ) ;
#20660 = CARTESIAN_POINT ( 'NONE',  ( 41.09999999999999432, 13.66939075806899950, 20.80000000000000426 ) ) ;
#20661 = VECTOR ( 'NONE', #21012, 1000.000000000000000 ) ;
#20662 = LINE ( 'NONE', #4430, #28880 ) ;
#20663 = EDGE_CURVE ( 'NONE', #49486, #49797, #62918, .T. ) ;
#20664 = CARTESIAN_POINT ( 'NONE',  ( 7.357023737882797398, 4.947141984184415087, 54.00000000000000711 ) ) ;
#20665 = LINE ( 'NONE', #26330, #38464 ) ;
#20666 = VECTOR ( 'NONE', #36711, 1000.000000000000000 ) ;
#20667 = VERTEX_POINT ( 'NONE', #13770 ) ;
#20669 = VERTEX_POINT ( 'NONE', #68577 ) ;
#20668 = CYLINDRICAL_SURFACE ( 'NONE', #65610, 0.2000000000000005107 ) ;
#20670 = EDGE_CURVE ( 'NONE', #27698, #24754, #64051, .T. ) ;
#20671 = DIRECTION ( 'NONE',  ( -0.000000000000000000, -0.000000000000000000, -1.000000000000000000 ) ) ;
#20672 = CARTESIAN_POINT ( 'NONE',  ( -11.33351654964671162, 1.077516549646603483, 195.0000000000000284 ) ) ;
#20673 = DIRECTION ( 'NONE',  ( 0.000000000000000000, -1.000000000000000000, 0.000000000000000000 ) ) ;
#20674 = ORIENTED_EDGE ( 'NONE', *, *, #18941, .T. ) ;
#20675 = EDGE_CURVE ( 'NONE', #19534, #33331, #58326, .T. ) ;
#20676 = VECTOR ( 'NONE', #19377, 1000.000000000000000 ) ;
#20677 = CARTESIAN_POINT ( 'NONE',  ( -8.250000000000001776, -7.249999999999998224, -9.000000000000001776 ) ) ;
#20678 = DIRECTION ( 'NONE',  ( 1.000000000000000000, 0.000000000000000000, 0.000000000000000000 ) ) ;
#20679 = ORIENTED_EDGE ( 'NONE', *, *, #7611, .T. ) ;
#20680 = EDGE_LOOP ( 'NONE', ( #16099, #60018, #10336, #53703 ) ) ;
#20681 = VERTEX_POINT ( 'NONE', #8454 ) ;
#20682 = EDGE_CURVE ( 'NONE', #49997, #16772, #67872, .T. ) ;
#20683 = FACE_OUTER_BOUND ( 'NONE', #51183, .T. ) ;
#20684 = CARTESIAN_POINT ( 'NONE',  ( 78.77321854994620765, 47.95351654967443977, 20.00000000000000000 ) ) ;
#20685 = DIRECTION ( 'NONE',  ( 0.000000000000000000, 3.673940397442059868E-16, -1.000000000000000000 ) ) ;
#20686 = VECTOR ( 'NONE', #69748, 1000.000000000000000 ) ;
#20687 = ORIENTED_EDGE ( 'NONE', *, *, #27202, .T. ) ;
#20688 = EDGE_CURVE ( 'NONE', #17050, #36357, #3522, .T. ) ;
#20689 = VERTEX_POINT ( 'NONE', #63627 ) ;
#20690 = EDGE_CURVE ( 'NONE', #5139, #42288, #62547, .T. ) ;
#20691 = AXIS2_PLACEMENT_3D ( 'NONE', #46310, #25101, #25814 ) ;
#20692 = DIRECTION ( 'NONE',  ( 1.000000000000000000, -3.491481338843133355E-15, -1.836970198721036344E-16 ) ) ;
#20693 = ORIENTED_EDGE ( 'NONE', *, *, #8803, .T. ) ;
#20694 = VECTOR ( 'NONE', #28818, 1000.000000000000000 ) ;
#20695 = VECTOR ( 'NONE', #30519, 1000.000000000000000 ) ;
#20696 = EDGE_CURVE ( 'NONE', #53754, #42236, #65206, .T. ) ;
#20697 = ORIENTED_EDGE ( 'NONE', *, *, #32575, .T. ) ;
#20698 = ADVANCED_FACE ( 'NONE', ( #63981 ), #37449, .F. ) ;
#20699 = EDGE_CURVE ( 'NONE', #6525, #31960, #21187, .T. ) ;
#20700 = ORIENTED_EDGE ( 'NONE', *, *, #17721, .T. ) ;
#20701 = VERTEX_POINT ( 'NONE', #69965 ) ;
#20702 = FACE_OUTER_BOUND ( 'NONE', #36170, .T. ) ;
#20703 = VECTOR ( 'NONE', #53280, 1000.000000000000000 ) ;
#20705 = EDGE_LOOP ( 'NONE', ( #53460, #57926, #45303, #60477 ) ) ;
#20704 = CARTESIAN_POINT ( 'NONE',  ( 7.000000000000000000, -42.50000000000000000, 7.500000000000000000 ) ) ;
#20706 = ADVANCED_FACE ( 'NONE', ( #22229 ), #37107, .F. ) ;
#20707 = DIRECTION ( 'NONE',  ( 0.000000000000000000, 0.000000000000000000, -1.000000000000000000 ) ) ;
#20708 = LINE ( 'NONE', #15419, #11423 ) ;
#20709 = MANIFOLD_SOLID_BREP ( 'LPattern1[15]', #56617 ) ;
#20710 = EDGE_CURVE ( 'NONE', #31270, #68694, #5280, .T. ) ;
#20711 = DIRECTION ( 'NONE',  ( 0.000000000000000000, 0.000000000000000000, 1.000000000000000000 ) ) ;
#20712 = ORIENTED_EDGE ( 'NONE', *, *, #25487, .F. ) ;
#20713 = EDGE_LOOP ( 'NONE', ( #50944, #43529, #35553, #45276 ) ) ;
#20714 = EDGE_CURVE ( 'NONE', #10292, #32087, #20822, .T. ) ;
#20715 = DIRECTION ( 'NONE',  ( 0.000000000000000000, 1.000000000000000000, 0.000000000000000000 ) ) ;
#20716 = ADVANCED_FACE ( 'NONE', ( #37792 ), #33170, .F. ) ;
#20717 = CARTESIAN_POINT ( 'NONE',  ( 7.000000000000000000, -30.45000000000000639, 15.00000000000000000 ) ) ;
#20718 = ORIENTED_EDGE ( 'NONE', *, *, #2494, .F. ) ;
#20719 = ADVANCED_FACE ( 'NONE', ( #48749 ), #307, .T. ) ;
#20720 = DIRECTION ( 'NONE',  ( 0.000000000000000000, 0.000000000000000000, -1.000000000000000000 ) ) ;
#20721 = DIRECTION ( 'NONE',  ( -1.000000000000000000, 0.000000000000000000, 0.000000000000000000 ) ) ;
#20722 = VERTEX_POINT ( 'NONE', #32824 ) ;
#20723 = CIRCLE ( 'NONE', #53504, 0.3999999999999993006 ) ;
#20724 = DIRECTION ( 'NONE',  ( 1.000000000000000000, -0.000000000000000000, -0.000000000000000000 ) ) ;
#20725 = CARTESIAN_POINT ( 'NONE',  ( 39.00000000000000000, -16.96999999999999886, 21.00000000000000000 ) ) ;
#20726 = LINE ( 'NONE', #58213, #44327 ) ;
#20727 = CARTESIAN_POINT ( 'NONE',  ( -7.250000000000000888, 7.250000000000001776, -14.50000000000000000 ) ) ;
#20728 = EDGE_CURVE ( 'NONE', #14563, #63937, #54405, .T. ) ;
#20729 = DIRECTION ( 'NONE',  ( -1.836970198721029934E-16, 1.836970198721036344E-16, -1.000000000000000000 ) ) ;
#20730 = ORIENTED_EDGE ( 'NONE', *, *, #36056, .T. ) ;
#20731 = LINE ( 'NONE', #9428, #60646 ) ;
#20732 = DIRECTION ( 'NONE',  ( 1.000000000000000000, -0.000000000000000000, 0.000000000000000000 ) ) ;
#20733 = CARTESIAN_POINT ( 'NONE',  ( -0.9414762621172249046, 9.915476262117151052, 54.00000000000000711 ) ) ;
#20734 = DIRECTION ( 'NONE',  ( -1.836970198721029934E-16, 1.836970198721036590E-16, -1.000000000000000000 ) ) ;
#20735 = AXIS2_PLACEMENT_3D ( 'NONE', #3183, #2466, #7417 ) ;
#20736 = VECTOR ( 'NONE', #1981, 1000.000000000000000 ) ;
#20737 = EDGE_LOOP ( 'NONE', ( #25679, #55760, #21894, #60783 ) ) ;
#20738 = DIRECTION ( 'NONE',  ( 0.000000000000000000, 1.000000000000000000, 0.000000000000000000 ) ) ;
#20739 = CARTESIAN_POINT ( 'NONE',  ( -30.00000000000000000, -16.28999999999999915, -14.50000000000000000 ) ) ;
#20740 = CARTESIAN_POINT ( 'NONE',  ( 289.5000000000000000, 50.00000000000000000, -27.00000000000000000 ) ) ;
#20741 = DIRECTION ( 'NONE',  ( 1.000000000000000000, -0.000000000000000000, -0.000000000000000000 ) ) ;
#20742 = PRESENTATION_LAYER_ASSIGNMENT (  '', '', ( #64768 ) ) ;
#20743 = EDGE_LOOP ( 'NONE', ( #21745, #34445, #52478, #41113 ) ) ;
#20744 = CIRCLE ( 'NONE', #36595, 0.2000000000000005107 ) ;
#20745 = LINE ( 'NONE', #57180, #26500 ) ;
#20746 = DIRECTION ( 'NONE',  ( 0.7671651518153029814, 0.6414496315691537998, -2.309356642088817231E-17 ) ) ;
#20747 = DIRECTION ( 'NONE',  ( 1.000000000000000000, 0.000000000000000000, -0.000000000000000000 ) ) ;
#20748 = CARTESIAN_POINT ( 'NONE',  ( 7.408280051175172076, -3.724485858128690818, 26.00000000000000711 ) ) ;
#20749 = CIRCLE ( 'NONE', #35421, 0.1999999999999992339 ) ;
#20751 = VECTOR ( 'NONE', #12412, 1000.000000000000000 ) ;
#20750 = DIRECTION ( 'NONE',  ( 0.000000000000000000, 0.000000000000000000, 1.000000000000000000 ) ) ;
#20752 = LINE ( 'NONE', #52595, #31707 ) ;
#20753 = ORIENTED_EDGE ( 'NONE', *, *, #19773, .F. ) ;
#20754 = ADVANCED_FACE ( 'NONE', ( #65361 ), #43787, .F. ) ;
#20755 = ORIENTED_EDGE ( 'NONE', *, *, #39662, .F. ) ;
#20756 = DIRECTION ( 'NONE',  ( -1.000000000000000000, 0.000000000000000000, 0.000000000000000000 ) ) ;
#20757 = DIRECTION ( 'NONE',  ( 0.000000000000000000, 1.000000000000000000, 0.000000000000000000 ) ) ;
#20758 = ORIENTED_EDGE ( 'NONE', *, *, #52722, .F. ) ;
#20759 = EDGE_CURVE ( 'NONE', #68364, #18995, #10918, .T. ) ;
#20760 = DIRECTION ( 'NONE',  ( 1.000000000000000000, -3.491481338843132961E-15, 0.000000000000000000 ) ) ;
#20761 = LINE ( 'NONE', #64597, #50959 ) ;
#20762 = EDGE_CURVE ( 'NONE', #40491, #67569, #54061, .T. ) ;
#20763 = ORIENTED_EDGE ( 'NONE', *, *, #28049, .F. ) ;
#20764 = DIRECTION ( 'NONE',  ( 1.000000000000000000, -0.000000000000000000, 0.000000000000000000 ) ) ;
#20765 = ORIENTED_EDGE ( 'NONE', *, *, #40216, .T. ) ;
#20766 = EDGE_CURVE ( 'NONE', #69773, #55741, #7931, .T. ) ;
#20767 = ORIENTED_EDGE ( 'NONE', *, *, #34807, .F. ) ;
#20768 = LINE ( 'NONE', #42337, #43045 ) ;
#20769 = EDGE_LOOP ( 'NONE', ( #3125, #31591, #51268, #60335 ) ) ;
#20770 = DIRECTION ( 'NONE',  ( -0.7071067811865446862, 0.7071067811865503483, -0.000000000000000000 ) ) ;
#20771 = FACE_OUTER_BOUND ( 'NONE', #63021, .T. ) ;
#20772 = DIRECTION ( 'NONE',  ( -0.000000000000000000, 3.673940397442059868E-16, -1.000000000000000000 ) ) ;
#20773 = ORIENTED_EDGE ( 'NONE', *, *, #6442, .F. ) ;
#20774 = VECTOR ( 'NONE', #10746, 1000.000000000000000 ) ;
#20775 = ORIENTED_EDGE ( 'NONE', *, *, #54393, .F. ) ;
#20776 = CARTESIAN_POINT ( 'NONE',  ( -8.250000000000001776, 0.000000000000000000, -18.00000000000000000 ) ) ;
#20778 = LINE ( 'NONE', #30699, #5108 ) ;
#20777 = DIRECTION ( 'NONE',  ( 0.000000000000000000, 0.000000000000000000, 1.000000000000000000 ) ) ;
#20779 = VERTEX_POINT ( 'NONE', #19252 ) ;
#20780 = ORIENTED_EDGE ( 'NONE', *, *, #12467, .T. ) ;
#20781 = EDGE_CURVE ( 'NONE', #3816, #2345, #1011, .T. ) ;
#20783 = EDGE_LOOP ( 'NONE', ( #28915, #33917, #40637, #22002 ) ) ;
#20782 = SHAPE_DEFINITION_REPRESENTATION ( #23373, #35 ) ;
#20784 = DIRECTION ( 'NONE',  ( 0.000000000000000000, 0.000000000000000000, 1.000000000000000000 ) ) ;
#20786 = ORIENTED_EDGE ( 'NONE', *, *, #45597, .T. ) ;
#20785 = LINE ( 'NONE', #31053, #1477 ) ;
#20787 = CARTESIAN_POINT ( 'NONE',  ( -8.250000000000001776, 7.250000000000000888, -26.00000000000001066 ) ) ;
#20788 = VECTOR ( 'NONE', #13429, 1000.000000000000000 ) ;
#20789 = AXIS2_PLACEMENT_3D ( 'NONE', #45024, #12834, #34398 ) ;
#20790 = CARTESIAN_POINT ( 'NONE',  ( 181.4833316329832940, 9.000000000000001776, 324.5239988703752942 ) ) ;
#20791 = VERTEX_POINT ( 'NONE', #23857 ) ;
#20792 = ORIENTED_EDGE ( 'NONE', *, *, #65315, .F. ) ;
#20793 = VECTOR ( 'NONE', #7167, 1000.000000000000000 ) ;
#20794 = AXIS2_PLACEMENT_3D ( 'NONE', #27004, #138, #11421 ) ;
#20795 = DIRECTION ( 'NONE',  ( 0.000000000000000000, 3.673940397442059868E-16, -1.000000000000000000 ) ) ;
#20796 = EDGE_LOOP ( 'NONE', ( #48940, #61565, #39592, #7404 ) ) ;
#20797 = DIRECTION ( 'NONE',  ( 1.000000000000000000, 0.000000000000000000, 0.000000000000000000 ) ) ;
#20798 = LINE ( 'NONE', #48723, #52780 ) ;
#20799 = AXIS2_PLACEMENT_3D ( 'NONE', #31839, #33206, #10598 ) ;
#20800 = CARTESIAN_POINT ( 'NONE',  ( 6.619341603356799553, 4.734785091273873370, 195.0000000000000284 ) ) ;
#20801 = EDGE_CURVE ( 'NONE', #45585, #43786, #24569, .T. ) ;
#20802 = ORIENTED_EDGE ( 'NONE', *, *, #62909, .F. ) ;
#20803 = ADVANCED_FACE ( 'NONE', ( #17244 ), #45415, .F. ) ;
#20804 = SURFACE_SIDE_STYLE ('',( #59335 ) ) ;
#20805 = CARTESIAN_POINT ( 'NONE',  ( 11.00000000000000000, -12.00000000000000000, 11.03137303340310282 ) ) ;
#20807 = VERTEX_POINT ( 'NONE', #29511 ) ;
#20806 = DIRECTION ( 'NONE',  ( 0.000000000000000000, -1.000000000000000000, 0.000000000000000000 ) ) ;
#20809 = EDGE_LOOP ( 'NONE', ( #7891, #5056, #18170, #15468 ) ) ;
#20808 = DIRECTION ( 'NONE',  ( -1.000000000000000000, 0.000000000000000000, 0.000000000000000000 ) ) ;
#20810 = VECTOR ( 'NONE', #61530, 1000.000000000000000 ) ;
#20811 = LINE ( 'NONE', #42377, #17355 ) ;
#20812 = DIRECTION ( 'NONE',  ( -1.000000000000000000, 0.000000000000000000, 0.000000000000000000 ) ) ;
#20813 = CARTESIAN_POINT ( 'NONE',  ( 30.00000000000000000, -9.200000000000120082, 17.64999999999993108 ) ) ;
#20814 = DIRECTION ( 'NONE',  ( 0.000000000000000000, -0.000000000000000000, 1.000000000000000000 ) ) ;
#20815 = CARTESIAN_POINT ( 'NONE',  ( 6.849523737882818430, 10.30047626211719169, 54.00000000000000711 ) ) ;
#20816 = ORIENTED_EDGE ( 'NONE', *, *, #64702, .F. ) ;
#20817 = DIRECTION ( 'NONE',  ( -1.000000000000000000, 0.000000000000000000, 0.000000000000000000 ) ) ;
#20818 = DIRECTION ( 'NONE',  ( -0.000000000000000000, -0.000000000000000000, -1.000000000000000000 ) ) ;
#20819 = CARTESIAN_POINT ( 'NONE',  ( 4.456444791733522252E-16, 7.450000000000002842, -10.50000000000000000 ) ) ;
#20821 = ORIENTED_EDGE ( 'NONE', *, *, #30265, .F. ) ;
#20820 = CARTESIAN_POINT ( 'NONE',  ( -11.99351654964674729, -7.826483450353316051, 195.0000000000000284 ) ) ;
#20822 = LINE ( 'NONE', #11249, #13237 ) ;
#20823 = MANIFOLD_SOLID_BREP ( 'SAWC-0630-60S_wagen', #44193 ) ;
#20824 = CARTESIAN_POINT ( 'NONE',  ( -6.331612867284196255, -8.406483450353375630, 195.0000000000000284 ) ) ;
#20825 = AXIS2_PLACEMENT_3D ( 'NONE', #31482, #3903, #37131 ) ;
#20826 = DIRECTION ( 'NONE',  ( -7.751221965937476285E-17, -1.000000000000000000, 0.000000000000000000 ) ) ;
#20827 = DIRECTION ( 'NONE',  ( 0.000000000000000000, 0.000000000000000000, 1.000000000000000000 ) ) ;
#20828 = VERTEX_POINT ( 'NONE', #35152 ) ;
#20829 = CARTESIAN_POINT ( 'NONE',  ( 4.155633711806658859, -5.793274621760832410, 26.00000000000000711 ) ) ;
#20830 = CARTESIAN_POINT ( 'NONE',  ( 14.89999999999999680, -21.00000000000001421, -13.86939075806900945 ) ) ;
#20831 = AXIS2_PLACEMENT_3D ( 'NONE', #15693, #42556, #64146 ) ;
#20832 = VERTEX_POINT ( 'NONE', #68046 ) ;
#20833 = DIRECTION ( 'NONE',  ( 0.000000000000000000, 0.000000000000000000, 1.000000000000000000 ) ) ;
#20834 = DIRECTION ( 'NONE',  ( -1.000000000000000000, 0.000000000000000000, 0.000000000000000000 ) ) ;
#20835 = PLANE ( 'NONE',  #40665 ) ;
#20836 = ADVANCED_FACE ( 'NONE', ( #41164 ), #56382, .T. ) ;
#20837 = CARTESIAN_POINT ( 'NONE',  ( 7.450000000000006395, 7.250000000000000888, -21.50000000000000000 ) ) ;
#20838 = AXIS2_PLACEMENT_3D ( 'NONE', #17522, #28137, #66321 ) ;
#20839 = VECTOR ( 'NONE', #1137, 1000.000000000000000 ) ;
#20840 = VERTEX_POINT ( 'NONE', #45772 ) ;
#20841 = ORIENTED_EDGE ( 'NONE', *, *, #37129, .F. ) ;
#20842 = DIRECTION ( 'NONE',  ( 0.000000000000000000, 1.000000000000000000, 0.000000000000000000 ) ) ;
#20843 = ORIENTED_EDGE ( 'NONE', *, *, #65185, .T. ) ;
#20844 = ORIENTED_EDGE ( 'NONE', *, *, #26315, .F. ) ;
#20845 = ADVANCED_FACE ( 'NONE', ( #46470 ), #34804, .F. ) ;
#20846 = CARTESIAN_POINT ( 'NONE',  ( -7.798499376344067535, 7.259684009079840017, 455.0000000000000568 ) ) ;
#20847 = AXIS2_PLACEMENT_3D ( 'NONE', #56236, #35340, #39276 ) ;
#20848 = AXIS2_PLACEMENT_3D ( 'NONE', #2542, #45319, #66888 ) ;
#20849 = EDGE_CURVE ( 'NONE', #4435, #20840, #62027, .T. ) ;
#20850 = EDGE_CURVE ( 'NONE', #19388, #37742, #18910, .T. ) ;
#20851 = LINE ( 'NONE', #62571, #3899 ) ;
#20852 = VECTOR ( 'NONE', #67821, 1000.000000000000000 ) ;
#20853 = LINE ( 'NONE', #26512, #65980 ) ;
#20854 = VERTEX_POINT ( 'NONE', #40470 ) ;
#20855 = ADVANCED_FACE ( 'NONE', ( #13598 ), #34447, .F. ) ;
#20856 = ORIENTED_EDGE ( 'NONE', *, *, #56465, .F. ) ;
#20857 = EDGE_CURVE ( 'NONE', #3246, #39788, #40822, .T. ) ;
#20858 = DIRECTION ( 'NONE',  ( 0.000000000000000000, -3.673940397442059868E-16, 1.000000000000000000 ) ) ;
#20859 = VERTEX_POINT ( 'NONE', #8646 ) ;
#20860 = ORIENTED_EDGE ( 'NONE', *, *, #57890, .T. ) ;
#20861 = CARTESIAN_POINT ( 'NONE',  ( -30.00000000000000000, -12.00000000000000000, 10.52786404500095863 ) ) ;
#20862 = CARTESIAN_POINT ( 'NONE',  ( 24.00000000000000000, -16.64230188589299786, -14.64519951917100116 ) ) ;
#20863 = VECTOR ( 'NONE', #48743, 1000.000000000000000 ) ;
#20864 = DIRECTION ( 'NONE',  ( 0.000000000000000000, 0.000000000000000000, 1.000000000000000000 ) ) ;
#20865 = EDGE_CURVE ( 'NONE', #16269, #1435, #27937, .T. ) ;
#20866 = ORIENTED_EDGE ( 'NONE', *, *, #41456, .F. ) ;
#20867 = AXIS2_PLACEMENT_3D ( 'NONE', #12311, #66068, #28588 ) ;
#20868 = LINE ( 'NONE', #14514, #7398 ) ;
#20870 = DIRECTION ( 'NONE',  ( -1.836970198721029934E-16, 1.836970198721036344E-16, -1.000000000000000000 ) ) ;
#20869 = DIRECTION ( 'NONE',  ( -1.000000000000000000, 0.000000000000000000, 0.000000000000000000 ) ) ;
#20871 = EDGE_LOOP ( 'NONE', ( #641, #56667, #17930, #26253 ) ) ;
#20873 = ORIENTED_EDGE ( 'NONE', *, *, #47268, .T. ) ;
#20872 = CARTESIAN_POINT ( 'NONE',  ( -7.250000000000000888, 7.250000000000001776, -10.50000000000000000 ) ) ;
#20874 = ORIENTED_EDGE ( 'NONE', *, *, #37830, .F. ) ;
#20875 = DIRECTION ( 'NONE',  ( -0.8660254037844400399, -0.4999999999999973910, 6.723777587268495961E-17 ) ) ;
#20876 = CARTESIAN_POINT ( 'NONE',  ( 52.83090410532631864, 3.657408540445007628, 2.000000000000000000 ) ) ;
#20877 = ORIENTED_EDGE ( 'NONE', *, *, #43721, .T. ) ;
#20878 = AXIS2_PLACEMENT_3D ( 'NONE', #59728, #1705, #48775 ) ;
#20879 = DIRECTION ( 'NONE',  ( 1.000000000000000000, -0.000000000000000000, -0.000000000000000000 ) ) ;
#20880 = LINE ( 'NONE', #6017, #60554 ) ;
#20881 = AXIS2_PLACEMENT_3D ( 'NONE', #41147, #68737, #41849 ) ;
#20882 = ORIENTED_EDGE ( 'NONE', *, *, #26445, .F. ) ;
#20883 = VERTEX_POINT ( 'NONE', #41524 ) ;
#20884 = PLANE ( 'NONE',  #35318 ) ;
#20885 = CARTESIAN_POINT ( 'NONE',  ( -25.50000000000000355, 0.000000000000000000, 22.50000000000000000 ) ) ;
#20886 = DIRECTION ( 'NONE',  ( -1.000000000000000000, 0.000000000000000000, 0.000000000000000000 ) ) ;
#20887 = ORIENTED_EDGE ( 'NONE', *, *, #61955, .T. ) ;
#20888 = EDGE_CURVE ( 'NONE', #54143, #8176, #53542, .T. ) ;
#20889 = AXIS2_PLACEMENT_3D ( 'NONE', #21277, #64075, #31538 ) ;
#20890 = AXIS2_PLACEMENT_3D ( 'NONE', #64035, #26190, #21923 ) ;
#20891 = FACE_OUTER_BOUND ( 'NONE', #50294, .T. ) ;
#20892 = CARTESIAN_POINT ( 'NONE',  ( 4.046023737882794791, 3.142976262117205266, 54.00000000000000711 ) ) ;
#20894 = ORIENTED_EDGE ( 'NONE', *, *, #24591, .T. ) ;
#20893 = EDGE_CURVE ( 'NONE', #28576, #48129, #40397, .T. ) ;
#20896 = ORIENTED_EDGE ( 'NONE', *, *, #46306, .F. ) ;
#20895 = CARTESIAN_POINT ( 'NONE',  ( 11.90000000000000036, -0.000000000000000000, -20.80000000000000426 ) ) ;
#20897 = EDGE_CURVE ( 'NONE', #56261, #12819, #39232, .T. ) ;
#20898 = CARTESIAN_POINT ( 'NONE',  ( 7.250000000000004441, 7.450000000000001954, -19.00000000000000000 ) ) ;
#20899 = AXIS2_PLACEMENT_3D ( 'NONE', #56155, #55464, #23612 ) ;
#20900 = CARTESIAN_POINT ( 'NONE',  ( -30.00000000000000000, -12.00000000000000000, 12.20000000000000107 ) ) ;
#20901 = DIRECTION ( 'NONE',  ( 0.000000000000000000, 0.000000000000000000, 1.000000000000000000 ) ) ;
#20902 = DIRECTION ( 'NONE',  ( -0.7671651518152895477, 0.6414496315691698980, -2.309356642088442522E-17 ) ) ;
#20903 = EDGE_CURVE ( 'NONE', #30511, #12117, #16056, .T. ) ;
#20904 = CARTESIAN_POINT ( 'NONE',  ( -7.342976262117259623, 3.834182069070703580, 54.00000000000000711 ) ) ;
#20905 = AXIS2_PLACEMENT_3D ( 'NONE', #20257, #63753, #41821 ) ;
#20906 = LINE ( 'NONE', #9964, #5571 ) ;
#20907 = ORIENTED_EDGE ( 'NONE', *, *, #39997, .F. ) ;
#20908 = FACE_OUTER_BOUND ( 'NONE', #33812, .T. ) ;
#20910 = EDGE_LOOP ( 'NONE', ( #17622, #33708, #68235, #10370, #66608, #36637, #33260, #50258 ) ) ;
#20909 = PRESENTATION_STYLE_ASSIGNMENT (( #4658 ) ) ;
#20911 = CARTESIAN_POINT ( 'NONE',  ( 30.00000000000000000, -9.454754784057099570, -17.53999999999999915 ) ) ;
#20912 = DIRECTION ( 'NONE',  ( 1.836970198721029934E-16, 1.836970198721010706E-16, -1.000000000000000000 ) ) ;
#20913 = VECTOR ( 'NONE', #29073, 1000.000000000000000 ) ;
#20914 = DIRECTION ( 'NONE',  ( 1.000000000000000000, -0.000000000000000000, 0.000000000000000000 ) ) ;
#20915 = ORIENTED_EDGE ( 'NONE', *, *, #15181, .F. ) ;
#20916 = CARTESIAN_POINT ( 'NONE',  ( 78.77321854994620765, 47.95351654967443977, 29.00000000000000000 ) ) ;
#20917 = FACE_OUTER_BOUND ( 'NONE', #18411, .T. ) ;
#20918 = EDGE_LOOP ( 'NONE', ( #35512, #10364, #28239, #33361 ) ) ;
#20919 = CARTESIAN_POINT ( 'NONE',  ( -7.259684009079963474, -4.201500623656036382, 455.0000000000000568 ) ) ;
#20920 = EDGE_CURVE ( 'NONE', #26334, #62286, #41869, .T. ) ;
#20921 = CARTESIAN_POINT ( 'NONE',  ( -17.00000000000000000, -17.35230188589299871, -15.35019951917099945 ) ) ;
#20922 = VERTEX_POINT ( 'NONE', #52857 ) ;
#20923 = CARTESIAN_POINT ( 'NONE',  ( 3.848229544836322180, -7.532023737882811432, 54.00000000000000711 ) ) ;
#20924 = ORIENTED_EDGE ( 'NONE', *, *, #33387, .F. ) ;
#20925 = ORIENTED_EDGE ( 'NONE', *, *, #13303, .F. ) ;
#20926 = CARTESIAN_POINT ( 'NONE',  ( 9.703773737882785966, -8.930623737882855906, 54.00000000000000711 ) ) ;
#20927 = DIRECTION ( 'NONE',  ( 1.000000000000000000, -0.000000000000000000, 1.224646799147353207E-16 ) ) ;
#20928 = VECTOR ( 'NONE', #22419, 1000.000000000000000 ) ;
#20929 = DIRECTION ( 'NONE',  ( -1.000000000000000000, 0.000000000000000000, 0.000000000000000000 ) ) ;
#20930 = CARTESIAN_POINT ( 'NONE',  ( 41.09999999999999432, 20.60000000000000142, -13.86939075806900057 ) ) ;
#20931 = ORIENTED_EDGE ( 'NONE', *, *, #9528, .T. ) ;
#20932 = EDGE_LOOP ( 'NONE', ( #65346, #23880, #12639, #5985 ) ) ;
#20933 = EDGE_CURVE ( 'NONE', #13102, #50086, #52134, .T. ) ;
#20935 = ORIENTED_EDGE ( 'NONE', *, *, #14021, .F. ) ;
#20934 = CARTESIAN_POINT ( 'NONE',  ( -15.50000000000000000, -0.2000000000000000111, 22.50000000000000000 ) ) ;
#20936 = ORIENTED_EDGE ( 'NONE', *, *, #20413, .F. ) ;
#20937 = CIRCLE ( 'NONE', #62720, 0.5000000000079367624 ) ;
#20938 = VECTOR ( 'NONE', #34536, 1000.000000000000000 ) ;
#20939 = AXIS2_PLACEMENT_3D ( 'NONE', #13384, #45911, #8064 ) ;
#20940 = CARTESIAN_POINT ( 'NONE',  ( 29.50000000000000355, -11.70000000000012008, 10.70000000000011831 ) ) ;
#20941 = LINE ( 'NONE', #42159, #69314 ) ;
#20942 = EDGE_CURVE ( 'NONE', #50555, #1682, #31628, .T. ) ;
#20943 = MANIFOLD_SOLID_BREP ( 'LPattern1[26]', #25029 ) ;
#20944 = DIRECTION ( 'NONE',  ( -1.011922027653137735E-14, -1.000000000000000000, 0.000000000000000000 ) ) ;
#20945 = CARTESIAN_POINT ( 'NONE',  ( -4.383466043307969962, -8.606483450353444198, 455.0000000000000568 ) ) ;
#20946 = VECTOR ( 'NONE', #36701, 1000.000000000000000 ) ;
#20947 = VECTOR ( 'NONE', #12825, 1000.000000000000000 ) ;
#20949 = DIRECTION ( 'NONE',  ( 1.000000000000000000, 0.000000000000000000, 0.000000000000000000 ) ) ;
#20948 = DIRECTION ( 'NONE',  ( -1.000000000000000000, 0.000000000000000000, 0.000000000000000000 ) ) ;
#20950 = ORIENTED_EDGE ( 'NONE', *, *, #67366, .F. ) ;
#20951 = ORIENTED_EDGE ( 'NONE', *, *, #7372, .T. ) ;
#20952 = VERTEX_POINT ( 'NONE', #36564 ) ;
#20953 = VERTEX_POINT ( 'NONE', #47871 ) ;
#20954 = CIRCLE ( 'NONE', #60460, 0.3999999999999993006 ) ;
#20955 = DIRECTION ( 'NONE',  ( 0.4285714285711678118, 0.000000000000000000, 0.9035079029053749711 ) ) ;
#20956 = LINE ( 'NONE', #64118, #41167 ) ;
#20957 = CARTESIAN_POINT ( 'NONE',  ( 51.41996235573692786, 113.8644206549746940, 281.7837994620734889 ) ) ;
#20958 = VECTOR ( 'NONE', #3003, 1000.000000000000000 ) ;
#20959 = LINE ( 'NONE', #53500, #69258 ) ;
#20960 = ORIENTED_EDGE ( 'NONE', *, *, #48604, .F. ) ;
#20961 = ORIENTED_EDGE ( 'NONE', *, *, #39906, .T. ) ;
#20962 = ORIENTED_EDGE ( 'NONE', *, *, #57868, .F. ) ;
#20963 = VECTOR ( 'NONE', #14203, 1000.000000000000000 ) ;
#20964 = DIRECTION ( 'NONE',  ( 1.000000000000000000, -0.000000000000000000, 0.000000000000000000 ) ) ;
#20965 = VERTEX_POINT ( 'NONE', #10402 ) ;
#20966 = PLANE ( 'NONE',  #26601 ) ;
#20967 = ORIENTED_EDGE ( 'NONE', *, *, #6431, .F. ) ;
#20968 = ORIENTED_EDGE ( 'NONE', *, *, #40216, .F. ) ;
#20969 = LINE ( 'NONE', #48901, #57636 ) ;
#20971 = ORIENTED_EDGE ( 'NONE', *, *, #48349, .T. ) ;
#20970 = CARTESIAN_POINT ( 'NONE',  ( 151.5599459900709860, 0.000000000000000000, 280.6301873289890523 ) ) ;
#20972 = ORIENTED_EDGE ( 'NONE', *, *, #48263, .T. ) ;
#20973 = DIRECTION ( 'NONE',  ( 1.000000000000000000, 0.000000000000000000, 0.000000000000000000 ) ) ;
#20974 = PLANE ( 'NONE',  #31358 ) ;
#20975 = CIRCLE ( 'NONE', #30001, 0.3499999999999285905 ) ;
#20978 = ORIENTED_EDGE ( 'NONE', *, *, #56988, .F. ) ;
#20977 = ADVANCED_FACE ( 'NONE', ( #36212 ), #63799, .T. ) ;
#20976 = CARTESIAN_POINT ( 'NONE',  ( 11.08848345035342042, 11.47551654964652812, 455.0000000000000568 ) ) ;
#20979 = EDGE_LOOP ( 'NONE', ( #53671, #59541, #25739, #36487, #2905, #2616, #40499, #24922, #29490, #48119 ) ) ;
#20980 = LINE ( 'NONE', #26994, #14087 ) ;
#20981 = DIRECTION ( 'NONE',  ( 0.000000000000000000, -0.1111111111108840643, -0.9938079899999319178 ) ) ;
#20982 = AXIS2_PLACEMENT_3D ( 'NONE', #50826, #66406, #2396 ) ;
#20983 = DIRECTION ( 'NONE',  ( -1.000000000000000000, 0.000000000000000000, 0.000000000000000000 ) ) ;
#20984 = DIRECTION ( 'NONE',  ( -0.000000000000000000, 3.673940397442059868E-16, -1.000000000000000000 ) ) ;
#20985 = EDGE_CURVE ( 'NONE', #31578, #58971, #30916, .T. ) ;
#20986 = DIRECTION ( 'NONE',  ( -0.5000000000000019984, -0.8660254037844375974, -0.000000000000000000 ) ) ;
#20987 = VECTOR ( 'NONE', #62042, 1000.000000000000000 ) ;
#20988 = ORIENTED_EDGE ( 'NONE', *, *, #11008, .F. ) ;
#20989 = FACE_BOUND ( 'NONE', #5053, .T. ) ;
#20990 = ORIENTED_EDGE ( 'NONE', *, *, #34809, .F. ) ;
#20991 = CIRCLE ( 'NONE', #6299, 2.204799999999997873 ) ;
#20992 = AXIS2_PLACEMENT_3D ( 'NONE', #69013, #13249, #3967 ) ;
#20994 = LINE ( 'NONE', #43253, #6164 ) ;
#20993 = AXIS2_PLACEMENT_3D ( 'NONE', #41399, #3930, #24793 ) ;
#20995 = CARTESIAN_POINT ( 'NONE',  ( 10.50702373788280219, 6.835476262117187396, 26.00000000000000711 ) ) ;
#20996 = DIRECTION ( 'NONE',  ( -1.000000000000000000, 2.602085213965213008E-15, 0.000000000000000000 ) ) ;
#20997 = CARTESIAN_POINT ( 'NONE',  ( 7.000000000000000000, -25.93000000000544958, -9.412893218815410634 ) ) ;
#20998 = CIRCLE ( 'NONE', #60506, 0.5999999999999998668 ) ;
#20999 = DIRECTION ( 'NONE',  ( 0.000000000000000000, -0.000000000000000000, 1.000000000000000000 ) ) ;
#21000 = VERTEX_POINT ( 'NONE', #58506 ) ;
#21001 = VECTOR ( 'NONE', #30971, 1000.000000000000000 ) ;
#21002 = EDGE_CURVE ( 'NONE', #40605, #37208, #64164, .T. ) ;
#21003 = DIRECTION ( 'NONE',  ( 0.6785983445458467767, -0.2810846377148228381, -0.6785983445458462215 ) ) ;
#21004 = PLANE ( 'NONE',  #59319 ) ;
#21005 = VECTOR ( 'NONE', #22408, 1000.000000000000000 ) ;
#21006 = ORIENTED_EDGE ( 'NONE', *, *, #43195, .T. ) ;
#21007 = CARTESIAN_POINT ( 'NONE',  ( 27.90000000000000213, 0.000000000000000000, 0.000000000000000000 ) ) ;
#21008 = CARTESIAN_POINT ( 'NONE',  ( 41.09999999999999432, -21.00000000000000000, 13.86939075806900057 ) ) ;
#21009 = CARTESIAN_POINT ( 'NONE',  ( -28.00000000000000000, -15.50000000000000000, -20.05051025721700242 ) ) ;
#21010 = CIRCLE ( 'NONE', #67295, 0.2000000000000005107 ) ;
#21011 = CARTESIAN_POINT ( 'NONE',  ( -14.25000000000000000, -0.2038245569916330158, 21.77831216351300014 ) ) ;
#21012 = DIRECTION ( 'NONE',  ( 0.000000000000000000, -0.000000000000000000, 1.000000000000000000 ) ) ;
#21013 = ORIENTED_EDGE ( 'NONE', *, *, #23700, .F. ) ;
#21014 = LINE ( 'NONE', #65211, #19752 ) ;
#21015 = PLANE ( 'NONE',  #37300 ) ;
#21016 = CARTESIAN_POINT ( 'NONE',  ( 39.00000000000000000, 21.00000000000000000, 16.96999999999999886 ) ) ;
#21017 = CYLINDRICAL_SURFACE ( 'NONE', #51217, 6.000000000000005329 ) ;
#21018 = CARTESIAN_POINT ( 'NONE',  ( 10.00000000000000000, 21.00000000000000000, -18.00000000000000355 ) ) ;
#21019 = EDGE_LOOP ( 'NONE', ( #24694, #30169, #36225, #42439 ) ) ;
#21021 = EDGE_LOOP ( 'NONE', ( #32873, #58095, #27339, #36408 ) ) ;
#21020 = CARTESIAN_POINT ( 'NONE',  ( 39.00000000000000000, -14.48845687959340012, 21.00000000000000000 ) ) ;
#21022 = EDGE_CURVE ( 'NONE', #17604, #50924, #5096, .T. ) ;
#21023 = CARTESIAN_POINT ( 'NONE',  ( 6.364920264886885448, -6.836383711243011696, 26.00000000000000000 ) ) ;
#21024 = EDGE_CURVE ( 'NONE', #12238, #16445, #69802, .T. ) ;
#21025 = CARTESIAN_POINT ( 'NONE',  ( 15.08565937784311117, -0.3156604612129180754, -21.29584399676446793 ) ) ;
#21026 = CARTESIAN_POINT ( 'NONE',  ( 9.562023737882764607, 2.355476262117153663, 54.00000000000000711 ) ) ;
#21027 = ORIENTED_EDGE ( 'NONE', *, *, #27486, .T. ) ;
#21028 = EDGE_CURVE ( 'NONE', #46021, #40627, #44292, .T. ) ;
#21029 = AXIS2_PLACEMENT_3D ( 'NONE', #36557, #25967, #9701 ) ;
#21030 = LINE ( 'NONE', #38346, #24322 ) ;
#21031 = DIRECTION ( 'NONE',  ( -1.000000000000000000, 0.000000000000000000, 0.000000000000000000 ) ) ;
#21032 = EDGE_CURVE ( 'NONE', #34914, #40390, #32320, .T. ) ;
#21033 = VECTOR ( 'NONE', #53305, 1000.000000000000000 ) ;
#21034 = ORIENTED_EDGE ( 'NONE', *, *, #35281, .T. ) ;
#21035 = ORIENTED_EDGE ( 'NONE', *, *, #21919, .F. ) ;
#21036 = EDGE_CURVE ( 'NONE', #48516, #9337, #16754, .T. ) ;
#21037 = VECTOR ( 'NONE', #37178, 1000.000000000000000 ) ;
#21038 = ADVANCED_FACE ( 'NONE', ( #6490 ), #17781, .F. ) ;
#21039 = ORIENTED_EDGE ( 'NONE', *, *, #8795, .F. ) ;
#21040 = EDGE_CURVE ( 'NONE', #47795, #47021, #50541, .T. ) ;
#21041 = PLANE ( 'NONE',  #36585 ) ;
#21042 = EDGE_CURVE ( 'NONE', #40439, #42288, #24608, .T. ) ;
#21043 = DIRECTION ( 'NONE',  ( 0.000000000000000000, 0.000000000000000000, -1.000000000000000000 ) ) ;
#21044 = DIRECTION ( 'NONE',  ( 0.000000000000000000, 1.000000000000000000, 0.000000000000000000 ) ) ;
#21045 = VECTOR ( 'NONE', #38303, 1000.000000000000000 ) ;
#21046 = VECTOR ( 'NONE', #66642, 1000.000000000000000 ) ;
#21047 = VECTOR ( 'NONE', #39557, 1000.000000000000114 ) ;
#21048 = ORIENTED_EDGE ( 'NONE', *, *, #22019, .F. ) ;
#21049 = ORIENTED_EDGE ( 'NONE', *, *, #57640, .F. ) ;
#21050 = CARTESIAN_POINT ( 'NONE',  ( -7.450000000000001954, 7.250000000000000000, -8.500000000000000000 ) ) ;
#21051 = VECTOR ( 'NONE', #474, 1000.000000000000114 ) ;
#21052 = AXIS2_PLACEMENT_3D ( 'NONE', #42862, #20949, #10350 ) ;
#21053 = AXIS2_PLACEMENT_3D ( 'NONE', #27228, #44494, #38852 ) ;
#21054 = ORIENTED_EDGE ( 'NONE', *, *, #43069, .T. ) ;
#21055 = ORIENTED_EDGE ( 'NONE', *, *, #19731, .F. ) ;
#21056 = VERTEX_POINT ( 'NONE', #49947 ) ;
#21057 = ORIENTED_EDGE ( 'NONE', *, *, #22563, .F. ) ;
#21058 = AXIS2_PLACEMENT_3D ( 'NONE', #18696, #24000, #61844 ) ;
#21059 = CARTESIAN_POINT ( 'NONE',  ( 6.665817930929288870, 7.342976262117195674, 54.00000000000000711 ) ) ;
#21060 = UNCERTAINTY_MEASURE_WITH_UNIT (LENGTH_MEASURE( 1.000000000000000082E-05 ), #4006, 'distance_accuracy_value', 'NONE');
#21062 = EDGE_LOOP ( 'NONE', ( #29572, #68088, #9260, #32967, #33735, #22102, #6511, #2549 ) ) ;
#21061 = FACE_OUTER_BOUND ( 'NONE', #37126, .T. ) ;
#21063 = LINE ( 'NONE', #10449, #11942 ) ;
#21064 = CIRCLE ( 'NONE', #67344, 0.1999999999999987899 ) ;
#21065 = CARTESIAN_POINT ( 'NONE',  ( 13.90000000000000213, -14.06939075806902117, -20.80000000000000426 ) ) ;
#21066 = EDGE_CURVE ( 'NONE', #47485, #68671, #1511, .T. ) ;
#21067 = CARTESIAN_POINT ( 'NONE',  ( 7.450000000000003730, -7.249999999999997335, -9.500000000000001776 ) ) ;
#21068 = VERTEX_POINT ( 'NONE', #53897 ) ;
#21069 = VERTEX_POINT ( 'NONE', #22406 ) ;
#21070 = CARTESIAN_POINT ( 'NONE',  ( 276.8775010008008053, -25.00000000000000000, -17.50000000000000000 ) ) ;
#21071 = DIRECTION ( 'NONE',  ( -0.000000000000000000, -0.000000000000000000, -1.000000000000000000 ) ) ;
#21072 = ORIENTED_EDGE ( 'NONE', *, *, #55654, .F. ) ;
#21073 = CARTESIAN_POINT ( 'NONE',  ( 7.250000000000005329, 7.250000000000000888, -9.500000000000001776 ) ) ;
#21074 = VECTOR ( 'NONE', #5373, 1000.000000000000000 ) ;
#21075 = CARTESIAN_POINT ( 'NONE',  ( 7.250000000000005329, -7.249999999999998224, -12.00000000000000000 ) ) ;
#21076 = ORIENTED_EDGE ( 'NONE', *, *, #35500, .T. ) ;
#21077 = DIRECTION ( 'NONE',  ( -1.000000000000000000, 0.000000000000000000, 0.000000000000000000 ) ) ;
#21078 = CARTESIAN_POINT ( 'NONE',  ( -7.415254214038336400, 2.993516549646603853, 455.0000000000000568 ) ) ;
#21079 = EDGE_CURVE ( 'NONE', #2931, #11595, #38995, .T. ) ;
#21080 = CARTESIAN_POINT ( 'NONE',  ( -5.993516549646711766, 5.993516549646603409, 195.0000000000000284 ) ) ;
#21081 = CIRCLE ( 'NONE', #60593, 1.000000000000000000 ) ;
#21082 = DIRECTION ( 'NONE',  ( 1.000000000000000000, -0.000000000000000000, 0.000000000000000000 ) ) ;
#21083 = AXIS2_PLACEMENT_3D ( 'NONE', #55854, #45579, #66463 ) ;
#21084 = AXIS2_PLACEMENT_3D ( 'NONE', #25861, #31171, #20541 ) ;
#21085 = ADVANCED_FACE ( 'NONE', ( #48931 ), #32662, .F. ) ;
#21086 = PLANE ( 'NONE',  #37630 ) ;
#21087 = ORIENTED_EDGE ( 'NONE', *, *, #60881, .T. ) ;
#21088 = DIRECTION ( 'NONE',  ( 1.836970198721029934E-16, 1.836970198721010706E-16, -1.000000000000000000 ) ) ;
#21089 = CARTESIAN_POINT ( 'NONE',  ( 7.450000000000003730, -7.249999999999997335, -15.50000000000000000 ) ) ;
#21090 = CARTESIAN_POINT ( 'NONE',  ( 30.00000000000000000, -13.54524521594299991, 17.53999999999999915 ) ) ;
#21091 = CARTESIAN_POINT ( 'NONE',  ( -7.450000000000001954, 7.250000000000000000, -25.00000000000000000 ) ) ;
#21092 = AXIS2_PLACEMENT_3D ( 'NONE', #38073, #64243, #10484 ) ;
#21093 = CIRCLE ( 'NONE', #18809, 0.1999999999999987899 ) ;
#21094 = AXIS2_PLACEMENT_3D ( 'NONE', #51469, #1983, #3043 ) ;
#21095 = VERTEX_POINT ( 'NONE', #5460 ) ;
#21096 = LINE ( 'NONE', #4146, #43912 ) ;
#21097 = ADVANCED_FACE ( 'NONE', ( #33689 ), #55271, .T. ) ;
#21098 = CARTESIAN_POINT ( 'NONE',  ( 0.000000000000000000, 0.000000000000000000, -25.00000000000000000 ) ) ;
#21099 = AXIS2_PLACEMENT_3D ( 'NONE', #10994, #54485, #1083 ) ;
#21100 = CARTESIAN_POINT ( 'NONE',  ( 8.250000000000005329, 7.250000000000000888, -26.00000000000001066 ) ) ;
#21101 = VECTOR ( 'NONE', #22527, 1000.000000000000000 ) ;
#21102 = DIRECTION ( 'NONE',  ( 1.000000000000000000, -5.981805089575194965E-17, 0.000000000000000000 ) ) ;
#21103 = VERTEX_POINT ( 'NONE', #21707 ) ;
#21104 = CARTESIAN_POINT ( 'NONE',  ( 7.250000000000005329, -7.449999999999998401, -20.50000000000000000 ) ) ;
#21105 = DIRECTION ( 'NONE',  ( -1.794541526872559352E-16, -1.000000000000000000, 0.000000000000000000 ) ) ;
#21106 = ADVANCED_FACE ( 'NONE', ( #43262 ), #64846, .T. ) ;
#21107 = EDGE_CURVE ( 'NONE', #37207, #32424, #27362, .T. ) ;
#21108 = DIRECTION ( 'NONE',  ( 1.000000000000000000, 0.000000000000000000, 0.000000000000000000 ) ) ;
#21109 = AXIS2_PLACEMENT_3D ( 'NONE', #67051, #29566, #2356 ) ;
#21110 = LINE ( 'NONE', #58595, #19698 ) ;
#21111 = DIRECTION ( 'NONE',  ( 0.000000000000000000, 0.000000000000000000, 1.000000000000000000 ) ) ;
#21112 = DIRECTION ( 'NONE',  ( 0.000000000000000000, 0.000000000000000000, 1.000000000000000000 ) ) ;
#21113 = ORIENTED_EDGE ( 'NONE', *, *, #51327, .F. ) ;
#21114 = AXIS2_PLACEMENT_3D ( 'NONE', #59434, #60801, #38226 ) ;
#21115 = ORIENTED_EDGE ( 'NONE', *, *, #4683, .T. ) ;
#21116 = DIRECTION ( 'NONE',  ( -1.000000000000000000, 0.000000000000000000, 0.000000000000000000 ) ) ;
#21117 = EDGE_CURVE ( 'NONE', #58645, #29870, #43620, .T. ) ;
#21118 = LINE ( 'NONE', #42676, #21033 ) ;
#21119 = ORIENTED_EDGE ( 'NONE', *, *, #66501, .T. ) ;
#21120 = DIRECTION ( 'NONE',  ( -0.7071067811865550112, -0.7071067811865401342, -2.597868168706466299E-16 ) ) ;
#21121 = DIRECTION ( 'NONE',  ( 1.000000000000000000, -0.000000000000000000, -0.000000000000000000 ) ) ;
#21122 = ORIENTED_EDGE ( 'NONE', *, *, #68021, .F. ) ;
#21123 = CARTESIAN_POINT ( 'NONE',  ( -11.77351654964670935, 7.813516549646603693, 455.0000000000000568 ) ) ;
#21124 = EDGE_LOOP ( 'NONE', ( #60700, #61597, #50873, #55944 ) ) ;
#21125 = ORIENTED_EDGE ( 'NONE', *, *, #29506, .F. ) ;
#21127 = EDGE_CURVE ( 'NONE', #29091, #4296, #59876, .T. ) ;
#21126 = CARTESIAN_POINT ( 'NONE',  ( 30.00000000000000000, -8.959999999999999076, 17.04524521594300523 ) ) ;
#21128 = EDGE_LOOP ( 'NONE', ( #49397, #61586, #5822, #35802 ) ) ;
#21129 = CARTESIAN_POINT ( 'NONE',  ( 49.00000000000000000, -0.2000000000089119934, 8.909539772616881237E-12 ) ) ;
#21130 = ADVANCED_FACE ( 'NONE', ( #49284 ), #857, .T. ) ;
#21131 = DIRECTION ( 'NONE',  ( -1.836970198721029934E-16, 1.836970198721036344E-16, -1.000000000000000000 ) ) ;
#21132 = DIRECTION ( 'NONE',  ( -0.000000000000000000, -0.000000000000000000, 1.000000000000000000 ) ) ;
#21133 = CARTESIAN_POINT ( 'NONE',  ( 11.78648345035337819, -7.826483450353491023, 455.0000000000000568 ) ) ;
#21134 = VECTOR ( 'NONE', #36752, 1000.000000000000000 ) ;
#21135 = ORIENTED_EDGE ( 'NONE', *, *, #11722, .F. ) ;
#21136 = ORIENTED_EDGE ( 'NONE', *, *, #57659, .T. ) ;
#21137 = CARTESIAN_POINT ( 'NONE',  ( 5.552858015815581361, -7.357023737882824044, 54.00000000000000711 ) ) ;
#21139 = FACE_OUTER_BOUND ( 'NONE', #68102, .T. ) ;
#21138 = LINE ( 'NONE', #264, #8986 ) ;
#21140 = ORIENTED_EDGE ( 'NONE', *, *, #69269, .F. ) ;
#21141 = EDGE_CURVE ( 'NONE', #57577, #17297, #60215, .T. ) ;
#21142 = ORIENTED_EDGE ( 'NONE', *, *, #43626, .T. ) ;
#21144 = ORIENTED_EDGE ( 'NONE', *, *, #9526, .T. ) ;
#21143 = SHAPE_DEFINITION_REPRESENTATION ( #43085, #53035 ) ;
#21145 = VECTOR ( 'NONE', #62521, 1000.000000000000000 ) ;
#21146 = CIRCLE ( 'NONE', #50497, 0.2000000000000005107 ) ;
#21147 = VECTOR ( 'NONE', #17571, 999.9999999999998863 ) ;
#21148 = DIRECTION ( 'NONE',  ( 0.000000000000000000, -0.000000000000000000, 1.000000000000000000 ) ) ;
#21150 = ORIENTED_EDGE ( 'NONE', *, *, #69559, .F. ) ;
#21149 = DIRECTION ( 'NONE',  ( -1.000000000000000000, 0.000000000000000000, 0.000000000000000000 ) ) ;
#21151 = VECTOR ( 'NONE', #23086, 1000.000000000000000 ) ;
#21152 = VECTOR ( 'NONE', #61293, 1000.000000000000000 ) ;
#21153 = CARTESIAN_POINT ( 'NONE',  ( 8.250000000000005329, 8.250000000000001776, -26.00000000000001066 ) ) ;
#21154 = LINE ( 'NONE', #48371, #6866 ) ;
#21155 = AXIS2_PLACEMENT_3D ( 'NONE', #28254, #26971, #44503 ) ;
#21156 = EDGE_LOOP ( 'NONE', ( #27038, #8739, #62168, #23201, #16782, #63576, #18915, #32007 ) ) ;
#21157 = EDGE_LOOP ( 'NONE', ( #23524, #51907, #39912, #23212 ) ) ;
#21158 = CIRCLE ( 'NONE', #48264, 0.5999999999999989786 ) ;
#21159 = VECTOR ( 'NONE', #9922, 1000.000000000000000 ) ;
#21160 = CARTESIAN_POINT ( 'NONE',  ( -8.393516549646712122, 4.383466043307770121, 455.0000000000000568 ) ) ;
#21161 = ORIENTED_EDGE ( 'NONE', *, *, #30203, .T. ) ;
#21162 = ADVANCED_FACE ( 'NONE', ( #66900 ), #56651, .F. ) ;
#21163 = CARTESIAN_POINT ( 'NONE',  ( 152.0064834503532722, -29.01119750012554732, 5.000000000000000000 ) ) ;
#21164 = LINE ( 'NONE', #53689, #68555 ) ;
#21165 = CARTESIAN_POINT ( 'NONE',  ( 175.4206970127264356, -30.42541106249864669, 0.000000000000000000 ) ) ;
#21166 = ORIENTED_EDGE ( 'NONE', *, *, #38878, .T. ) ;
#21167 = ADVANCED_FACE ( 'NONE', ( #29773 ), #41083, .T. ) ;
#21168 = AXIS2_PLACEMENT_3D ( 'NONE', #63259, #15174, #31449 ) ;
#21169 = DIRECTION ( 'NONE',  ( -1.000000000000000000, 0.000000000000000000, 0.000000000000000000 ) ) ;
#21170 = CYLINDRICAL_SURFACE ( 'NONE', #43699, 1.000000000000000000 ) ;
#21171 = ORIENTED_EDGE ( 'NONE', *, *, #33608, .F. ) ;
#21172 = ORIENTED_EDGE ( 'NONE', *, *, #56039, .F. ) ;
#21173 = ADVANCED_FACE ( 'NONE', ( #13865 ), #18115, .T. ) ;
#21174 = CARTESIAN_POINT ( 'NONE',  ( 283.0000000000000568, -40.30000000000000426, 8.900000000000000355 ) ) ;
#21175 = DIRECTION ( 'NONE',  ( 1.836970198721029934E-16, 1.836970198721010706E-16, -1.000000000000000000 ) ) ;
#21176 = ADVANCED_FACE ( 'NONE', ( #12802 ), #18823, .T. ) ;
#21177 = LINE ( 'NONE', #4225, #844 ) ;
#21178 = CARTESIAN_POINT ( 'NONE',  ( 9.690000000000001279, 9.690000000000001279, -5.000000000000000000 ) ) ;
#21179 = ADVANCED_FACE ( 'NONE', ( #34363 ), #51711, .F. ) ;
#21180 = DIRECTION ( 'NONE',  ( 0.000000000000000000, 0.000000000000000000, 1.000000000000000000 ) ) ;
#21181 = ORIENTED_EDGE ( 'NONE', *, *, #51013, .T. ) ;
#21182 = CARTESIAN_POINT ( 'NONE',  ( 8.900000000000005684, -14.48845687959340012, 21.00000000000000000 ) ) ;
#21183 = CARTESIAN_POINT ( 'NONE',  ( -29.25000000000000000, -5.000000000000000000, -26.25000000000000000 ) ) ;
#21184 = FACE_OUTER_BOUND ( 'NONE', #57197, .T. ) ;
#21186 = ORIENTED_EDGE ( 'NONE', *, *, #42488, .T. ) ;
#21185 = CARTESIAN_POINT ( 'NONE',  ( 4.201500623656003519, -7.272650909786698037, 455.0000000000000568 ) ) ;
#21187 = LINE ( 'NONE', #60036, #20016 ) ;
#21188 = AXIS2_PLACEMENT_3D ( 'NONE', #34727, #13164, #3262 ) ;
#21189 = LINE ( 'NONE', #31461, #69860 ) ;
#21190 = ADVANCED_FACE ( 'NONE', ( #2907 ), #55954, .F. ) ;
#21191 = DIRECTION ( 'NONE',  ( -1.794541526872559352E-16, -1.000000000000000000, 0.000000000000000000 ) ) ;
#21192 = ADVANCED_FACE ( 'NONE', ( #40741 ), #67967, .F. ) ;
#21193 = DIRECTION ( 'NONE',  ( 1.000000000000000000, -0.000000000000000000, 0.000000000000000000 ) ) ;
#21194 = ORIENTED_EDGE ( 'NONE', *, *, #23037, .T. ) ;
#21195 = CYLINDRICAL_SURFACE ( 'NONE', #7187, 0.1749999999999989342 ) ;
#21196 = DIRECTION ( 'NONE',  ( 0.3479852726768751237, 0.000000000000000000, 0.9375000000000004441 ) ) ;
#21197 = ORIENTED_EDGE ( 'NONE', *, *, #49754, .T. ) ;
#21198 = LINE ( 'NONE', #27196, #49239 ) ;
#21199 = ADVANCED_FACE ( 'NONE', ( #50297 ), #29084, .T. ) ;
#21200 = EDGE_CURVE ( 'NONE', #27438, #64069, #24831, .T. ) ;
#21201 = DIRECTION ( 'NONE',  ( 1.000000000000000000, 0.000000000000000000, 0.000000000000000000 ) ) ;
#21202 = CIRCLE ( 'NONE', #60694, 1.000000000000002665 ) ;
#21203 = VECTOR ( 'NONE', #15781, 1000.000000000000000 ) ;
#21204 = VECTOR ( 'NONE', #46371, 999.9999999999998863 ) ;
#21205 = CARTESIAN_POINT ( 'NONE',  ( 12.00648345035338238, 4.173516549646515195, 455.0000000000000568 ) ) ;
#21206 = DIRECTION ( 'NONE',  ( -9.912705577010344285E-15, -1.000000000000000000, 0.000000000000000000 ) ) ;
#21207 = EDGE_CURVE ( 'NONE', #28218, #14914, #30213, .T. ) ;
#21208 = VECTOR ( 'NONE', #36492, 1000.000000000000000 ) ;
#21210 = DIRECTION ( 'NONE',  ( -1.836970198721029934E-16, -1.836970198721010706E-16, 1.000000000000000000 ) ) ;
#21209 = VECTOR ( 'NONE', #64475, 1000.000000000000000 ) ;
#21211 = ORIENTED_EDGE ( 'NONE', *, *, #2482, .F. ) ;
#21212 = ORIENTED_EDGE ( 'NONE', *, *, #17927, .F. ) ;
#21213 = CARTESIAN_POINT ( 'NONE',  ( -6.822336235477441946, -4.149127210878692296, 26.00000000000000711 ) ) ;
#21214 = ORIENTED_EDGE ( 'NONE', *, *, #47720, .T. ) ;
#21215 = ORIENTED_EDGE ( 'NONE', *, *, #38588, .T. ) ;
#21216 = CARTESIAN_POINT ( 'NONE',  ( -3.593516549646701197, 7.415254214038210279, 455.0000000000000568 ) ) ;
#21217 = AXIS2_PLACEMENT_3D ( 'NONE', #63440, #5455, #30912 ) ;
#21218 = VECTOR ( 'NONE', #8324, 1000.000000000000000 ) ;
#21219 = LINE ( 'NONE', #5305, #41175 ) ;
#21220 = CARTESIAN_POINT ( 'NONE',  ( 10.09643294401454661, -2.706483450353396325, 195.0000000000000284 ) ) ;
#21221 = ORIENTED_EDGE ( 'NONE', *, *, #22900, .T. ) ;
#21222 = ORIENTED_EDGE ( 'NONE', *, *, #33567, .T. ) ;
#21224 = ADVANCED_FACE ( 'NONE', ( #8553 ), #7510, .F. ) ;
#21223 = DIRECTION ( 'NONE',  ( 0.000000000000000000, -0.7071067811865460184, -0.7071067811865489050 ) ) ;
#21225 = ORIENTED_EDGE ( 'NONE', *, *, #67052, .T. ) ;
#21226 = ORIENTED_EDGE ( 'NONE', *, *, #586, .F. ) ;
#21227 = EDGE_CURVE ( 'NONE', #114, #4139, #67617, .T. ) ;
#21228 = AXIS2_PLACEMENT_3D ( 'NONE', #29579, #67067, #18622 ) ;
#21229 = CARTESIAN_POINT ( 'NONE',  ( 14.25000000000000000, -0.2038245569916330158, -23.22168783648699986 ) ) ;
#21230 = DIRECTION ( 'NONE',  ( 1.000000000000000000, -0.000000000000000000, -0.000000000000000000 ) ) ;
#21231 = CARTESIAN_POINT ( 'NONE',  ( 2.420780051175147829, -8.711985858128677762, 54.00000000000000711 ) ) ;
#21232 = VERTEX_POINT ( 'NONE', #2210 ) ;
#21233 = DIRECTION ( 'NONE',  ( 1.000000000000000000, 0.000000000000000000, 0.000000000000000000 ) ) ;
#21235 = DIRECTION ( 'NONE',  ( 1.000000000000000000, 0.000000000000000000, 0.000000000000000000 ) ) ;
#21234 = CARTESIAN_POINT ( 'NONE',  ( 40.90000000000000568, 16.96999999999999886, 21.00000000000000000 ) ) ;
#21236 = ORIENTED_EDGE ( 'NONE', *, *, #35527, .T. ) ;
#21238 = ORIENTED_EDGE ( 'NONE', *, *, #12091, .T. ) ;
#21237 = DIRECTION ( 'NONE',  ( 1.000000000000000000, -0.000000000000000000, -0.000000000000000000 ) ) ;
#21239 = ORIENTED_EDGE ( 'NONE', *, *, #63778, .F. ) ;
#21240 = FACE_OUTER_BOUND ( 'NONE', #35030, .T. ) ;
#21241 = CARTESIAN_POINT ( 'NONE',  ( -9.689726262117227762, 8.916576262117214213, 54.00000000000000711 ) ) ;
#21242 = COLOUR_RGB ( '', 0.31764706, 0.68627451, 0.89019608) ;
#21243 = ORIENTED_EDGE ( 'NONE', *, *, #37412, .F. ) ;
#21244 = DIRECTION ( 'NONE',  ( 0.000000000000000000, 0.6801302850037830305, 0.7330912599538155217 ) ) ;
#21245 = LINE ( 'NONE', #16638, #22158 ) ;
#21246 = EDGE_LOOP ( 'NONE', ( #24671, #44508, #396, #54342 ) ) ;
#21247 = ORIENTED_EDGE ( 'NONE', *, *, #21833, .T. ) ;
#21248 = DIRECTION ( 'NONE',  ( -0.000000000000000000, -0.000000000000000000, -1.000000000000000000 ) ) ;
#21249 = CARTESIAN_POINT ( 'NONE',  ( 30.00000000000000000, -17.00000000000000000, -15.70499999999969809 ) ) ;
#21250 = CARTESIAN_POINT ( 'NONE',  ( 16.89999999999999858, 20.60000000000000142, 13.86939075806900057 ) ) ;
#21251 = VERTEX_POINT ( 'NONE', #23777 ) ;
#21252 = CIRCLE ( 'NONE', #14480, 0.2000000000000005107 ) ;
#21253 = EDGE_CURVE ( 'NONE', #7192, #7881, #19171, .T. ) ;
#21254 = FACE_OUTER_BOUND ( 'NONE', #44003, .T. ) ;
#21255 = LINE ( 'NONE', #37860, #58804 ) ;
#21257 = EDGE_LOOP ( 'NONE', ( #13403, #50149, #22426, #37856, #27343, #47308, #17561, #47862, #67249, #27374, #10493, #31123, #62897, #38954, #41976, #2241, #66852 ) ) ;
#21256 = DIRECTION ( 'NONE',  ( -1.000000000000000000, 0.000000000000000000, 0.000000000000000000 ) ) ;
#21259 = ORIENTED_EDGE ( 'NONE', *, *, #25428, .T. ) ;
#21258 = DIRECTION ( 'NONE',  ( -1.000000000000000000, 0.000000000000000000, 0.000000000000000000 ) ) ;
#21260 = EDGE_CURVE ( 'NONE', #14532, #7744, #45329, .T. ) ;
#21261 = DIRECTION ( 'NONE',  ( -0.000000000000000000, -0.000000000000000000, -1.000000000000000000 ) ) ;
#21262 = CIRCLE ( 'NONE', #69812, 1.500000000000000444 ) ;
#21263 = VECTOR ( 'NONE', #30956, 1000.000000000000000 ) ;
#21264 = DIRECTION ( 'NONE',  ( 0.000000000000000000, -0.6857142857147903170, 0.7278708115913530285 ) ) ;
#21265 = EDGE_CURVE ( 'NONE', #28244, #14932, #24127, .T. ) ;
#21266 = DIRECTION ( 'NONE',  ( -1.836970198721029934E-16, 1.836970198721036344E-16, -1.000000000000000000 ) ) ;
#21267 = EDGE_CURVE ( 'NONE', #65495, #11767, #47444, .T. ) ;
#21268 = CARTESIAN_POINT ( 'NONE',  ( 11.75000000000000000, -5.000000000000000000, -26.25000000000000000 ) ) ;
#21269 = DIRECTION ( 'NONE',  ( -0.000000000000000000, -0.000000000000000000, -1.000000000000000000 ) ) ;
#21270 = ADVANCED_FACE ( 'NONE', ( #14929 ), #63367, .F. ) ;
#21271 = EDGE_CURVE ( 'NONE', #8645, #57546, #26235, .T. ) ;
#21272 = LINE ( 'NONE', #25874, #60863 ) ;
#21273 = ORIENTED_EDGE ( 'NONE', *, *, #25342, .F. ) ;
#21274 = CARTESIAN_POINT ( 'NONE',  ( -7.290476262117262074, 9.722976262117178692, 54.00000000000000711 ) ) ;
#21276 = ORIENTED_EDGE ( 'NONE', *, *, #8202, .T. ) ;
#21275 = DIRECTION ( 'NONE',  ( -1.000000000000000000, 0.000000000000000000, 0.000000000000000000 ) ) ;
#21277 = CARTESIAN_POINT ( 'NONE',  ( -25.50000000000000355, -15.12100000000000044, 22.50000000000000000 ) ) ;
#21278 = DIRECTION ( 'NONE',  ( 0.000000000000000000, 0.000000000000000000, 1.000000000000000000 ) ) ;
#21279 = PLANE ( 'NONE',  #14903 ) ;
#21280 = VERTEX_POINT ( 'NONE', #9625 ) ;
#21281 = DIRECTION ( 'NONE',  ( 0.000000000000000000, 0.000000000000000000, 1.000000000000000000 ) ) ;
#21282 = DIRECTION ( 'NONE',  ( 1.836970198721029934E-16, 1.836970198721010706E-16, -1.000000000000000000 ) ) ;
#21283 = ORIENTED_EDGE ( 'NONE', *, *, #68265, .T. ) ;
#21284 = PLANE ( 'NONE',  #59457 ) ;
#21285 = CYLINDRICAL_SURFACE ( 'NONE', #16749, 1.000000000000000000 ) ;
#21286 = EDGE_LOOP ( 'NONE', ( #13318, #56426, #69847, #56659 ) ) ;
#21287 = DIRECTION ( 'NONE',  ( 1.000000000000000000, 0.000000000000000000, 0.000000000000000000 ) ) ;
#21288 = ORIENTED_EDGE ( 'NONE', *, *, #12599, .T. ) ;
#21289 = EDGE_LOOP ( 'NONE', ( #66254, #33301, #13198, #69600 ) ) ;
#21290 = CARTESIAN_POINT ( 'NONE',  ( 7.450000000000006395, 7.250000000000000888, -19.00000000000000000 ) ) ;
#21291 = DIRECTION ( 'NONE',  ( 0.000000000000000000, 0.000000000000000000, 1.000000000000000000 ) ) ;
#21292 = CYLINDRICAL_SURFACE ( 'NONE', #21912, 24.99999999998794920 ) ;
#21293 = PLANE ( 'NONE',  #17100 ) ;
#21294 = ORIENTED_EDGE ( 'NONE', *, *, #12049, .T. ) ;
#21295 = EDGE_LOOP ( 'NONE', ( #53902, #29368, #52693, #52953 ) ) ;
#21297 = ORIENTED_EDGE ( 'NONE', *, *, #55328, .F. ) ;
#21296 = DIRECTION ( 'NONE',  ( -0.7071067811865474617, -0.7071067811865474617, -2.597868168706479611E-16 ) ) ;
#21298 = EDGE_LOOP ( 'NONE', ( #22293, #41816, #24798, #25380 ) ) ;
#21299 = AXIS2_PLACEMENT_3D ( 'NONE', #23098, #64948, #7173 ) ;
#21300 = ADVANCED_FACE ( 'NONE', ( #14218 ), #25541, .F. ) ;
#21301 = DIRECTION ( 'NONE',  ( 0.000000000000000000, 3.673940397442059868E-16, -1.000000000000000000 ) ) ;
#21302 = CARTESIAN_POINT ( 'NONE',  ( 7.000000000000000000, -29.94999999999999929, 14.50000000000000000 ) ) ;
#21303 = MANIFOLD_SOLID_BREP ( 'Cut-Extrude3', #43096 ) ;
#21304 = DIRECTION ( 'NONE',  ( 1.000000000000000000, -0.000000000000000000, 0.000000000000000000 ) ) ;
#21305 = EDGE_CURVE ( 'NONE', #67015, #29909, #32549, .T. ) ;
#21306 = AXIS2_PLACEMENT_3D ( 'NONE', #2101, #67850, #46275 ) ;
#21307 = DIRECTION ( 'NONE',  ( 0.000000000000000000, 0.000000000000000000, 1.000000000000000000 ) ) ;
#21309 = CARTESIAN_POINT ( 'NONE',  ( 30.00000000000000000, -11.85423089348099879, 9.852125413066602277 ) ) ;
#21308 = LINE ( 'NONE', #1128, #43369 ) ;
#21310 = ORIENTED_EDGE ( 'NONE', *, *, #32523, .F. ) ;
#21312 = ORIENTED_EDGE ( 'NONE', *, *, #53464, .T. ) ;
#21311 = LINE ( 'NONE', #32263, #45392 ) ;
#21313 = ORIENTED_EDGE ( 'NONE', *, *, #25708, .F. ) ;
#21314 = EDGE_LOOP ( 'NONE', ( #7799, #48746, #22140, #58534 ) ) ;
#21315 = FACE_BOUND ( 'NONE', #61309, .T. ) ;
#21316 = CARTESIAN_POINT ( 'NONE',  ( 9.900000000000000355, 0.000000000000000000, 2.154935995002245639E-16 ) ) ;
#21317 = AXIS2_PLACEMENT_3D ( 'NONE', #23432, #50643, #38990 ) ;
#21318 = LINE ( 'NONE', #42871, #34247 ) ;
#21319 = ORIENTED_EDGE ( 'NONE', *, *, #16142, .F. ) ;
#21320 = VERTEX_POINT ( 'NONE', #47104 ) ;
#21321 = VERTEX_POINT ( 'NONE', #37202 ) ;
#21322 = PLANE ( 'NONE',  #15877 ) ;
#21323 = ORIENTED_EDGE ( 'NONE', *, *, #44784, .F. ) ;
#21324 = CYLINDRICAL_SURFACE ( 'NONE', #12803, 0.1749999999999998224 ) ;
#21325 = CARTESIAN_POINT ( 'NONE',  ( -8.821682069070780230, 7.955476262117183062, 26.00000000000000711 ) ) ;
#21326 = ORIENTED_EDGE ( 'NONE', *, *, #62252, .T. ) ;
#21327 = ORIENTED_EDGE ( 'NONE', *, *, #19789, .T. ) ;
#21328 = FACE_OUTER_BOUND ( 'NONE', #53399, .T. ) ;
#21329 = LINE ( 'NONE', #54211, #45810 ) ;
#21330 = VERTEX_POINT ( 'NONE', #42491 ) ;
#21331 = ADVANCED_FACE ( 'NONE', ( #20572 ), #63014, .F. ) ;
#21332 = DIRECTION ( 'NONE',  ( -1.000000000000000000, 0.000000000000000000, 0.000000000000000000 ) ) ;
#21334 = VERTEX_POINT ( 'NONE', #14567 ) ;
#21333 = CARTESIAN_POINT ( 'NONE',  ( 4.740315990920131561, -7.811466277050742590, 195.0000000000000284 ) ) ;
#21335 = EDGE_LOOP ( 'NONE', ( #43431, #43473, #59507, #61828 ) ) ;
#21336 = CARTESIAN_POINT ( 'NONE',  ( -7.450000000000001954, 7.250000000000000000, -17.50000000000000000 ) ) ;
#21337 = CARTESIAN_POINT ( 'NONE',  ( 7.826483450353380000, -11.78648345035339418, 195.0000000000000284 ) ) ;
#21338 = ADVANCED_FACE ( 'NONE', ( #30482 ), #15278, .F. ) ;
#21339 = DIRECTION ( 'NONE',  ( 1.000000000000000000, -0.000000000000000000, -0.000000000000000000 ) ) ;
#21340 = EDGE_CURVE ( 'NONE', #68617, #6256, #58763, .T. ) ;
#21341 = EDGE_CURVE ( 'NONE', #7480, #11799, #31894, .T. ) ;
#21342 = FACE_OUTER_BOUND ( 'NONE', #30608, .T. ) ;
#21343 = CIRCLE ( 'NONE', #23580, 9.300000000000002487 ) ;
#21344 = PLANE ( 'NONE',  #33854 ) ;
#21345 = ADVANCED_FACE ( 'NONE', ( #69728 ), #21285, .T. ) ;
#21346 = ADVANCED_FACE ( 'NONE', ( #28303 ), #1430, .F. ) ;
#21347 = ORIENTED_EDGE ( 'NONE', *, *, #67768, .F. ) ;
#21348 = LINE ( 'NONE', #10389, #46165 ) ;
#21349 = VECTOR ( 'NONE', #27992, 1000.000000000000000 ) ;
#21350 = EDGE_LOOP ( 'NONE', ( #54533, #43940, #48891, #25928 ) ) ;
#21351 = CARTESIAN_POINT ( 'NONE',  ( 30.00000000000000000, -10.85999999999999943, -9.000000000000001776 ) ) ;
#21352 = LINE ( 'NONE', #38652, #51505 ) ;
#21353 = ADVANCED_FACE ( 'NONE', ( #65117 ), #1100, .T. ) ;
#21354 = CARTESIAN_POINT ( 'NONE',  ( -7.603567055985634759, -8.406483450353409381, 455.0000000000000568 ) ) ;
#21355 = DIRECTION ( 'NONE',  ( 1.356437060717834182E-15, 1.000000000000000000, 1.836970198721033878E-16 ) ) ;
#21356 = CIRCLE ( 'NONE', #47337, 0.4999999999979768961 ) ;
#21357 = DIRECTION ( 'NONE',  ( 0.000000000000000000, 0.000000000000000000, -1.000000000000000000 ) ) ;
#21358 = EDGE_LOOP ( 'NONE', ( #5775, #11960, #4001, #68377 ) ) ;
#21359 = CIRCLE ( 'NONE', #8919, 0.5000000000023396840 ) ;
#21360 = CARTESIAN_POINT ( 'NONE',  ( -6.344366288193441505, -5.793274621760819088, 54.00000000000000711 ) ) ;
#21361 = AXIS2_PLACEMENT_3D ( 'NONE', #14743, #52942, #69532 ) ;
#21362 = ORIENTED_EDGE ( 'NONE', *, *, #6561, .T. ) ;
#21363 = FACE_OUTER_BOUND ( 'NONE', #23303, .T. ) ;
#21364 = CARTESIAN_POINT ( 'NONE',  ( 41.09999999999999432, -21.00000000000000000, -13.86939075806900057 ) ) ;
#21365 = ORIENTED_EDGE ( 'NONE', *, *, #58233, .F. ) ;
#21366 = FACE_OUTER_BOUND ( 'NONE', #54038, .T. ) ;
#21367 = AXIS2_PLACEMENT_3D ( 'NONE', #3245, #51328, #41064 ) ;
#21368 = PLANE ( 'NONE',  #62432 ) ;
#21369 = ORIENTED_EDGE ( 'NONE', *, *, #47204, .T. ) ;
#21370 = CARTESIAN_POINT ( 'NONE',  ( -8.250000000000001776, 7.250000000000000888, -26.00000000000001066 ) ) ;
#21371 = DIRECTION ( 'NONE',  ( 1.000000000000000000, -0.000000000000000000, 0.000000000000000000 ) ) ;
#21372 = CARTESIAN_POINT ( 'NONE',  ( 8.249999999999996447, 8.250000000000001776, 0.000000000000000000 ) ) ;
#21373 = DIRECTION ( 'NONE',  ( 0.000000000000000000, -1.000000000000000000, 0.000000000000000000 ) ) ;
#21374 = ORIENTED_EDGE ( 'NONE', *, *, #11643, .T. ) ;
#21376 = EDGE_LOOP ( 'NONE', ( #66055, #56133, #44987, #42100 ) ) ;
#21375 = DIRECTION ( 'NONE',  ( 0.000000000000000000, 0.000000000000000000, 1.000000000000000000 ) ) ;
#21377 = CARTESIAN_POINT ( 'NONE',  ( 8.250000000000005329, 0.000000000000000000, -24.00000000000000000 ) ) ;
#21378 = CARTESIAN_POINT ( 'NONE',  ( 16.75000000000000000, -2.500000000000000000, -23.22168783648699986 ) ) ;
#21379 = CARTESIAN_POINT ( 'NONE',  ( 7.250000000000005329, -7.249999999999998224, -11.50000000000000000 ) ) ;
#21380 = VERTEX_POINT ( 'NONE', #33615 ) ;
#21381 = EDGE_CURVE ( 'NONE', #63246, #14509, #59103, .T. ) ;
#21382 = ADVANCED_FACE ( 'NONE', ( #27969 ), #32926, .T. ) ;
#21383 = EDGE_CURVE ( 'NONE', #23822, #68865, #10664, .T. ) ;
#21384 = DIRECTION ( 'NONE',  ( -1.000000000000000000, 0.000000000000000000, 0.000000000000000000 ) ) ;
#21385 = LINE ( 'NONE', #31323, #18288 ) ;
#21386 = VERTEX_POINT ( 'NONE', #37895 ) ;
#21387 = ORIENTED_EDGE ( 'NONE', *, *, #37069, .F. ) ;
#21388 = EDGE_CURVE ( 'NONE', #36247, #4689, #54506, .T. ) ;
#21389 = AXIS2_PLACEMENT_3D ( 'NONE', #61630, #17465, #44670 ) ;
#21390 = ORIENTED_EDGE ( 'NONE', *, *, #48435, .T. ) ;
#21391 = CARTESIAN_POINT ( 'NONE',  ( -2.693516549646820746, -10.09643294401462832, 455.0000000000000568 ) ) ;
#21392 = VECTOR ( 'NONE', #7085, 1000.000000000000000 ) ;
#21393 = AXIS2_PLACEMENT_3D ( 'NONE', #28240, #49811, #1376 ) ;
#21394 = DIRECTION ( 'NONE',  ( 0.000000000000000000, -1.000000000000000000, 0.000000000000000000 ) ) ;
#21395 = PLANE ( 'NONE',  #40420 ) ;
#21396 = ORIENTED_EDGE ( 'NONE', *, *, #51496, .T. ) ;
#21397 = VERTEX_POINT ( 'NONE', #43181 ) ;
#21398 = DIRECTION ( 'NONE',  ( -1.000000000000000000, 3.491481338843133355E-15, 1.836970198721036344E-16 ) ) ;
#21399 = ORIENTED_EDGE ( 'NONE', *, *, #18520, .T. ) ;
#21400 = ORIENTED_EDGE ( 'NONE', *, *, #66579, .F. ) ;
#21401 = EDGE_LOOP ( 'NONE', ( #24971, #31534, #18122, #53855 ) ) ;
#21402 = AXIS2_PLACEMENT_3D ( 'NONE', #45477, #18610, #15426 ) ;
#21403 = ORIENTED_EDGE ( 'NONE', *, *, #29728, .T. ) ;
#21404 = CARTESIAN_POINT ( 'NONE',  ( -5.993516549646776603, -6.006483450353426790, 455.0000000000000568 ) ) ;
#21406 = VERTEX_POINT ( 'NONE', #59797 ) ;
#21405 = DIRECTION ( 'NONE',  ( -0.000000000000000000, 3.673940397442059868E-16, -1.000000000000000000 ) ) ;
#21407 = AXIS2_PLACEMENT_3D ( 'NONE', #66995, #18554, #40111 ) ;
#21408 = DIRECTION ( 'NONE',  ( -0.000000000000000000, -0.000000000000000000, 1.000000000000000000 ) ) ;
#21409 = CARTESIAN_POINT ( 'NONE',  ( 25.50000000000000355, -15.50000000000000000, -25.99999999999985434 ) ) ;
#21410 = MANIFOLD_SOLID_BREP ( 'Scale1', #4703 ) ;
#21411 = LINE ( 'NONE', #36623, #29052 ) ;
#21412 = ORIENTED_EDGE ( 'NONE', *, *, #60633, .F. ) ;
#21413 = CIRCLE ( 'NONE', #12343, 0.8128000000000145109 ) ;
#21414 = FACE_OUTER_BOUND ( 'NONE', #28843, .T. ) ;
#21415 = CARTESIAN_POINT ( 'NONE',  ( 30.00000000000000000, -17.00000000000000000, 15.70499999999969809 ) ) ;
#21416 = EDGE_LOOP ( 'NONE', ( #3053, #41460, #11166, #20367 ) ) ;
#21417 = CARTESIAN_POINT ( 'NONE',  ( 39.90000000000000568, 6.429395695523604153E-16, -5.250000000000000000 ) ) ;
#21418 = EDGE_CURVE ( 'NONE', #37177, #51945, #765, .T. ) ;
#21419 = FILL_AREA_STYLE_COLOUR ( '', #49252 ) ;
#21420 = FACE_OUTER_BOUND ( 'NONE', #9089, .T. ) ;
#21421 = EDGE_CURVE ( 'NONE', #57899, #16799, #48499, .T. ) ;
#21422 = AXIS2_PLACEMENT_3D ( 'NONE', #35374, #35738, #18071 ) ;
#21423 = EDGE_CURVE ( 'NONE', #60071, #33734, #49875, .T. ) ;
#21424 = ORIENTED_EDGE ( 'NONE', *, *, #31581, .F. ) ;
#21425 = DIRECTION ( 'NONE',  ( 1.000000000000000000, 0.000000000000000000, 0.000000000000000000 ) ) ;
#21426 = DIRECTION ( 'NONE',  ( -1.000000000000000000, 0.000000000000000000, 0.000000000000000000 ) ) ;
#21427 = EDGE_CURVE ( 'NONE', #61212, #25535, #44936, .T. ) ;
#21428 = CARTESIAN_POINT ( 'NONE',  ( -0.9414762621173239365, -9.404523737882849233, 54.00000000000000711 ) ) ;
#21429 = APPLICATION_CONTEXT ( 'automotive_design' ) ;
#21430 = CARTESIAN_POINT ( 'NONE',  ( -8.689999999999999503, 9.750000000000001776, -7.000000000000000000 ) ) ;
#21431 = EDGE_CURVE ( 'NONE', #52778, #9070, #65454, .T. ) ;
#21432 = DIRECTION ( 'NONE',  ( 0.000000000000000000, -1.000000000000000000, 0.000000000000000000 ) ) ;
#21433 = CARTESIAN_POINT ( 'NONE',  ( -17.00000000000000000, -16.28999999999710369, -14.50000000000000000 ) ) ;
#21434 = VECTOR ( 'NONE', #48257, 1000.000000000000000 ) ;
#21436 = ADVANCED_FACE ( 'NONE', ( #33276 ), #54844, .F. ) ;
#21435 = LINE ( 'NONE', #27085, #36714 ) ;
#21437 = DIRECTION ( 'NONE',  ( -0.000000000000000000, -0.000000000000000000, 1.000000000000000000 ) ) ;
#21438 = VECTOR ( 'NONE', #50126, 1000.000000000000000 ) ;
#21439 = VERTEX_POINT ( 'NONE', #50575 ) ;
#21440 = DIRECTION ( 'NONE',  ( 1.000000000000000000, -1.047444401652940007E-14, 0.000000000000000000 ) ) ;
#21441 = DIRECTION ( 'NONE',  ( 0.000000000000000000, 0.000000000000000000, -1.000000000000000000 ) ) ;
#21442 = AXIS2_PLACEMENT_3D ( 'NONE', #56124, #56808, #24649 ) ;
#21443 = DIRECTION ( 'NONE',  ( -1.000000000000000000, 0.000000000000000000, 0.000000000000000000 ) ) ;
#21444 = DIRECTION ( 'NONE',  ( 0.000000000000000000, 0.000000000000000000, -1.000000000000000000 ) ) ;
#21445 = ORIENTED_EDGE ( 'NONE', *, *, #53804, .T. ) ;
#21446 = CARTESIAN_POINT ( 'NONE',  ( 29.89999999999999858, -21.00000000000000000, 13.86939075806900057 ) ) ;
#21447 = CARTESIAN_POINT ( 'NONE',  ( -8.821682069070751808, -2.544523737882741887, 54.00000000000000711 ) ) ;
#21448 = DIRECTION ( 'NONE',  ( -0.000000000000000000, -0.000000000000000000, 1.000000000000000000 ) ) ;
#21449 = CIRCLE ( 'NONE', #66610, 3.499999999999999556 ) ;
#21450 = DIRECTION ( 'NONE',  ( -3.491481338843133355E-15, -1.000000000000000000, -1.836970198721029934E-16 ) ) ;
#21451 = DIRECTION ( 'NONE',  ( -2.439149994343049068E-15, -1.000000000000000000, 0.000000000000000000 ) ) ;
#21452 = CARTESIAN_POINT ( 'NONE',  ( -16.75000000000000000, -2.500000000000000000, -21.77831216351300014 ) ) ;
#21453 = VERTEX_POINT ( 'NONE', #61508 ) ;
#21454 = AXIS2_PLACEMENT_3D ( 'NONE', #18121, #39689, #12807 ) ;
#21455 = ORIENTED_EDGE ( 'NONE', *, *, #61100, .F. ) ;
#21456 = FACE_OUTER_BOUND ( 'NONE', #64459, .T. ) ;
#21457 = LINE ( 'NONE', #53996, #10833 ) ;
#21458 = ORIENTED_EDGE ( 'NONE', *, *, #12768, .T. ) ;
#21459 = CARTESIAN_POINT ( 'NONE',  ( 15.50000000000000000, 0.000000000000000000, -18.50000000000000000 ) ) ;
#21460 = AXIS2_PLACEMENT_3D ( 'NONE', #37959, #59525, #475 ) ;
#21461 = VECTOR ( 'NONE', #8692, 1000.000000000000000 ) ;
#21462 = LINE ( 'NONE', #4169, #2506 ) ;
#21463 = VERTEX_POINT ( 'NONE', #13072 ) ;
#21464 = ADVANCED_FACE ( 'NONE', ( #12364, #2129, #60820, #18030, #45249, #7424, #66132, #50219, #39597, #28642 ), #30046, .F. ) ;
#21465 = FACE_OUTER_BOUND ( 'NONE', #22497, .T. ) ;
#21466 = ORIENTED_EDGE ( 'NONE', *, *, #47070, .T. ) ;
#21467 = ORIENTED_EDGE ( 'NONE', *, *, #21701, .T. ) ;
#21468 = DIRECTION ( 'NONE',  ( 0.000000000000000000, 0.000000000000000000, 1.000000000000000000 ) ) ;
#21469 = ORIENTED_EDGE ( 'NONE', *, *, #34471, .F. ) ;
#21470 = CARTESIAN_POINT ( 'NONE',  ( 11.34648345035334671, 1.077516549646521327, 455.0000000000000568 ) ) ;
#21471 = PLANE ( 'NONE',  #38255 ) ;
#21472 = LINE ( 'NONE', #54016, #49424 ) ;
#21473 = AXIS2_PLACEMENT_3D ( 'NONE', #52908, #48627, #64206 ) ;
#21474 = ORIENTED_EDGE ( 'NONE', *, *, #37486, .T. ) ;
#21475 = VERTEX_POINT ( 'NONE', #40304 ) ;
#21476 = CARTESIAN_POINT ( 'NONE',  ( -8.916576262117358098, -9.703773737882734451, 54.00000000000000711 ) ) ;
#21478 = DIRECTION ( 'NONE',  ( 0.000000000000000000, 0.000000000000000000, 1.000000000000000000 ) ) ;
#21477 = DIRECTION ( 'NONE',  ( 0.000000000000000000, 3.673940397442059868E-16, -1.000000000000000000 ) ) ;
#21479 = EDGE_CURVE ( 'NONE', #34893, #14054, #28999, .T. ) ;
#21480 = ORIENTED_EDGE ( 'NONE', *, *, #46694, .F. ) ;
#21481 = ORIENTED_EDGE ( 'NONE', *, *, #61369, .F. ) ;
#21483 = VERTEX_POINT ( 'NONE', #62218 ) ;
#21482 = ITEM_DEFINED_TRANSFORMATION ( 'NONE', 'NONE', #61756,  #45918 ) ;
#21484 = EDGE_CURVE ( 'NONE', #17477, #11057, #18990, .T. ) ;
#21485 = DIRECTION ( 'NONE',  ( 0.000000000000000000, 1.000000000000000000, 0.000000000000000000 ) ) ;
#21486 = AXIS2_PLACEMENT_3D ( 'NONE', #2872, #8170, #52022 ) ;
#21488 = VERTEX_POINT ( 'NONE', #19090 ) ;
#21487 = DIRECTION ( 'NONE',  ( 0.000000000000000000, 1.000000000000000000, 0.000000000000000000 ) ) ;
#21489 = DIRECTION ( 'NONE',  ( -1.836970198721029934E-16, 1.836970198721036344E-16, -1.000000000000000000 ) ) ;
#21490 = CIRCLE ( 'NONE', #64411, 0.5999999999999998668 ) ;
#21491 = LINE ( 'NONE', #4543, #61063 ) ;
#21492 = ORIENTED_EDGE ( 'NONE', *, *, #28082, .F. ) ;
#21493 = ORIENTED_EDGE ( 'NONE', *, *, #65910, .T. ) ;
#21494 = AXIS2_PLACEMENT_3D ( 'NONE', #5182, #36299, #42299 ) ;
#21495 = CARTESIAN_POINT ( 'NONE',  ( 275.0000000000000000, -20.40000000000000213, -12.40000000000000213 ) ) ;
#21496 = EDGE_CURVE ( 'NONE', #47032, #5159, #7075, .T. ) ;
#21497 = ORIENTED_EDGE ( 'NONE', *, *, #31630, .T. ) ;
#21498 = AXIS2_PLACEMENT_3D ( 'NONE', #67087, #18643, #13695 ) ;
#21499 = DIRECTION ( 'NONE',  ( -1.000000000000000000, 0.000000000000000000, 0.000000000000000000 ) ) ;
#21500 = DIRECTION ( 'NONE',  ( -1.000000000000000000, 0.000000000000000000, 0.000000000000000000 ) ) ;
#21501 = CIRCLE ( 'NONE', #66927, 0.2000000000000005107 ) ;
#21502 = ORIENTED_EDGE ( 'NONE', *, *, #36058, .F. ) ;
#21503 = DIRECTION ( 'NONE',  ( 0.000000000000000000, 3.673940397442059868E-16, -1.000000000000000000 ) ) ;
#21504 = CARTESIAN_POINT ( 'NONE',  ( 11.50000000000000000, -15.46862696659690073, 14.50000000000000000 ) ) ;
#21505 = EDGE_CURVE ( 'NONE', #29254, #37032, #51621, .T. ) ;
#21507 = EDGE_LOOP ( 'NONE', ( #53506, #3387, #24620, #22622, #66611, #33940, #1569, #32831 ) ) ;
#21506 = CARTESIAN_POINT ( 'NONE',  ( -8.250000000000000000, 7.250000000000001776, -16.00000000000000000 ) ) ;
#21508 = ORIENTED_EDGE ( 'NONE', *, *, #22748, .F. ) ;
#21509 = DIRECTION ( 'NONE',  ( -1.034072152899300274E-14, -1.000000000000000000, 0.000000000000000000 ) ) ;
#21510 = AXIS2_PLACEMENT_3D ( 'NONE', #32576, #53793, #43507 ) ;
#21511 = AXIS2_PLACEMENT_3D ( 'NONE', #35115, #13561, #67657 ) ;
#21512 = CARTESIAN_POINT ( 'NONE',  ( 9.404523737882753309, 1.466476262117160312, 26.00000000000000711 ) ) ;
#21513 = CARTESIAN_POINT ( 'NONE',  ( 4.201500623656003519, -4.740315990920286104, 455.0000000000000568 ) ) ;
#21514 = DIRECTION ( 'NONE',  ( -1.836970198721029934E-16, 1.836970198721036344E-16, -1.000000000000000000 ) ) ;
#21515 = LINE ( 'NONE', #16570, #8218 ) ;
#21516 = ADVANCED_FACE ( 'NONE', ( #51256 ), #34645, .T. ) ;
#21517 = VERTEX_POINT ( 'NONE', #44916 ) ;
#21518 = CARTESIAN_POINT ( 'NONE',  ( -25.50000000000000355, -5.200000000000001066, -22.50000000000000000 ) ) ;
#21519 = DIRECTION ( 'NONE',  ( 0.000000000000000000, -1.000000000000000000, -1.880440247955360336E-12 ) ) ;
#21520 = EDGE_CURVE ( 'NONE', #26683, #27626, #66479, .T. ) ;
#21522 = ORIENTED_EDGE ( 'NONE', *, *, #7463, .T. ) ;
#21521 = CARTESIAN_POINT ( 'NONE',  ( 30.00000000000000000, -11.70000000000000284, -12.50000000000000000 ) ) ;
#21523 = DIRECTION ( 'NONE',  ( 0.000000000000000000, -0.7071067811865455743, 0.7071067811865495711 ) ) ;
#21524 = MANIFOLD_SOLID_BREP ( 'LPattern1[8]', #49854 ) ;
#21525 = VECTOR ( 'NONE', #10021, 1000.000000000000000 ) ;
#21526 = PLANE ( 'NONE',  #64220 ) ;
#21527 = LINE ( 'NONE', #10225, #66861 ) ;
#21528 = CARTESIAN_POINT ( 'NONE',  ( -11.99351654964671354, 4.173516549646604901, 455.0000000000000568 ) ) ;
#21529 = ORIENTED_EDGE ( 'NONE', *, *, #45261, .T. ) ;
#21530 = CARTESIAN_POINT ( 'NONE',  ( 46.39999999999999858, 21.00000000000000000, 0.7500000000000000000 ) ) ;
#21531 = DIRECTION ( 'NONE',  ( 0.000000000000000000, 0.000000000000000000, 1.000000000000000000 ) ) ;
#21532 = EDGE_CURVE ( 'NONE', #29731, #53055, #35329, .T. ) ;
#21533 = ORIENTED_EDGE ( 'NONE', *, *, #60371, .T. ) ;
#21534 = DIRECTION ( 'NONE',  ( 0.6414496315691367023, -0.7671651518153173033, -2.309356642089295169E-17 ) ) ;
#21535 = CARTESIAN_POINT ( 'NONE',  ( 11.75000000000000000, -5.000000000000000000, -11.75000000000000000 ) ) ;
#21536 = DIRECTION ( 'NONE',  ( 1.047444401652940007E-14, 1.000000000000000000, 1.836970198721029934E-16 ) ) ;
#21537 = DIRECTION ( 'NONE',  ( -1.000000000000000000, 0.000000000000000000, 0.000000000000000000 ) ) ;
#21538 = AXIS2_PLACEMENT_3D ( 'NONE', #62527, #56876, #3153 ) ;
#21539 = LINE ( 'NONE', #48763, #11695 ) ;
#21540 = AXIS2_PLACEMENT_3D ( 'NONE', #47203, #10071, #68767 ) ;
#21541 = ORIENTED_EDGE ( 'NONE', *, *, #23563, .T. ) ;
#21542 = VERTEX_POINT ( 'NONE', #46305 ) ;
#21543 = DIRECTION ( 'NONE',  ( 0.000000000000000000, 0.000000000000000000, 1.000000000000000000 ) ) ;
#21544 = ORIENTED_EDGE ( 'NONE', *, *, #48476, .F. ) ;
#21545 = EDGE_LOOP ( 'NONE', ( #66337, #47136, #66692, #6142 ) ) ;
#21546 = VECTOR ( 'NONE', #27964, 1000.000000000000000 ) ;
#21547 = DIRECTION ( 'NONE',  ( 1.000000000000000000, 0.000000000000000000, 0.000000000000000000 ) ) ;
#21548 = VECTOR ( 'NONE', #16844, 1000.000000000000000 ) ;
#21549 = CIRCLE ( 'NONE', #68994, 0.5000000000004272138 ) ;
#21550 = EDGE_CURVE ( 'NONE', #23129, #39526, #31814, .T. ) ;
#21551 = CARTESIAN_POINT ( 'NONE',  ( 283.0000000000000568, -32.00000000000000000, -8.400000000000000355 ) ) ;
#21552 = DIRECTION ( 'NONE',  ( -1.000000000000000000, 0.000000000000000000, -0.000000000000000000 ) ) ;
#21553 = EDGE_LOOP ( 'NONE', ( #1508, #9994, #45883, #11361 ) ) ;
#21554 = EDGE_LOOP ( 'NONE', ( #68452, #65383, #34067, #920 ) ) ;
#21555 = CARTESIAN_POINT ( 'NONE',  ( 11.19368345035340973, 11.99351654964656433, 455.0000000000000568 ) ) ;
#21556 = ORIENTED_EDGE ( 'NONE', *, *, #45904, .F. ) ;
#21557 = VECTOR ( 'NONE', #53226, 1000.000000000000000 ) ;
#21558 = EDGE_CURVE ( 'NONE', #56607, #50075, #14002, .T. ) ;
#21559 = ORIENTED_EDGE ( 'NONE', *, *, #13507, .T. ) ;
#21560 = DIRECTION ( 'NONE',  ( 0.000000000000000000, -0.1249999999999996531, -0.9921567416492215186 ) ) ;
#21561 = DIRECTION ( 'NONE',  ( 0.000000000000000000, -0.9938079899998859545, 0.1111111111112941946 ) ) ;
#21562 = DIRECTION ( 'NONE',  ( 0.000000000000000000, 1.000000000000000000, 0.000000000000000000 ) ) ;
#21563 = VERTEX_POINT ( 'NONE', #31115 ) ;
#21564 = EDGE_CURVE ( 'NONE', #63213, #54079, #52440, .T. ) ;
#21565 = LINE ( 'NONE', #55135, #1862 ) ;
#21566 = AXIS2_PLACEMENT_3D ( 'NONE', #10907, #63260, #64310 ) ;
#21568 = LINE ( 'NONE', #37145, #29914 ) ;
#21567 = FACE_OUTER_BOUND ( 'NONE', #28861, .T. ) ;
#21569 = ORIENTED_EDGE ( 'NONE', *, *, #44083, .T. ) ;
#21570 = VERTEX_POINT ( 'NONE', #40996 ) ;
#21571 = ADVANCED_FACE ( 'NONE', ( #63278 ), #52687, .F. ) ;
#21573 = ORIENTED_EDGE ( 'NONE', *, *, #41787, .T. ) ;
#21572 = DIRECTION ( 'NONE',  ( -0.000000000000000000, -0.000000000000000000, -1.000000000000000000 ) ) ;
#21574 = ORIENTED_EDGE ( 'NONE', *, *, #23263, .F. ) ;
#21575 = ADVANCED_FACE ( 'NONE', ( #3188 ), #58680, .F. ) ;
#21576 = DIRECTION ( 'NONE',  ( 0.000000000000000000, 0.000000000000000000, 1.000000000000000000 ) ) ;
#21577 = CARTESIAN_POINT ( 'NONE',  ( 0.000000000000000000, -8.249999999999998224, -18.00000000000000000 ) ) ;
#21578 = VECTOR ( 'NONE', #11555, 1000.000000000000000 ) ;
#21579 = ORIENTED_EDGE ( 'NONE', *, *, #44661, .F. ) ;
#21580 = EDGE_CURVE ( 'NONE', #32122, #33533, #58338, .T. ) ;
#21581 = VERTEX_POINT ( 'NONE', #42408 ) ;
#21582 = EDGE_CURVE ( 'NONE', #29427, #18454, #14847, .T. ) ;
#21583 = LINE ( 'NONE', #11641, #769 ) ;
#21584 = LINE ( 'NONE', #54463, #17647 ) ;
#21585 = ADVANCED_FACE ( 'NONE', ( #46654 ), #62557, .F. ) ;
#21586 = ORIENTED_EDGE ( 'NONE', *, *, #3004, .F. ) ;
#21587 = EDGE_CURVE ( 'NONE', #67901, #42614, #25099, .T. ) ;
#21588 = EDGE_CURVE ( 'NONE', #50155, #41366, #9186, .T. ) ;
#21589 = ORIENTED_EDGE ( 'NONE', *, *, #68420, .F. ) ;
#21590 = DIRECTION ( 'NONE',  ( 1.000000000000000000, 0.000000000000000000, 0.000000000000000000 ) ) ;
#21591 = FACE_OUTER_BOUND ( 'NONE', #16262, .T. ) ;
#21592 = DIRECTION ( 'NONE',  ( -1.000000000000000000, 0.000000000000000000, 0.000000000000000000 ) ) ;
#21593 = AXIS2_PLACEMENT_3D ( 'NONE', #30202, #47172, #25610 ) ;
#21594 = ORIENTED_EDGE ( 'NONE', *, *, #2023, .F. ) ;
#21595 = EDGE_CURVE ( 'NONE', #62386, #54520, #15193, .T. ) ;
#21596 = VECTOR ( 'NONE', #54216, 1000.000000000000114 ) ;
#21597 = DIRECTION ( 'NONE',  ( -1.047444401652939849E-14, -1.000000000000000000, -1.836970198721029934E-16 ) ) ;
#21598 = ADVANCED_FACE ( 'NONE', ( #57968 ), #15196, .T. ) ;
#21599 = CARTESIAN_POINT ( 'NONE',  ( 7.250000000000004441, 7.450000000000001954, -25.50000000000000355 ) ) ;
#21601 = EDGE_LOOP ( 'NONE', ( #56414, #16054, #60096, #205, #14088, #51529, #44637, #68444 ) ) ;
#21600 = CARTESIAN_POINT ( 'NONE',  ( 8.835729544836338434, -2.544523737882825820, 54.00000000000000711 ) ) ;
#21603 = EDGE_LOOP ( 'NONE', ( #62576, #9582, #7709, #30427 ) ) ;
#21602 = CARTESIAN_POINT ( 'NONE',  ( -7.813516549646839948, -12.00648345035340903, 455.0000000000000568 ) ) ;
#21604 = ADVANCED_FACE ( 'NONE', ( #30755 ), #31470, .F. ) ;
#21605 = DIRECTION ( 'NONE',  ( 0.000000000000000000, 0.000000000000000000, 1.000000000000000000 ) ) ;
#21606 = LINE ( 'NONE', #21942, #48742 ) ;
#21607 = DIRECTION ( 'NONE',  ( 1.000000000000000000, 0.000000000000000000, 0.000000000000000000 ) ) ;
#21608 = DIRECTION ( 'NONE',  ( 0.000000000000000000, -3.673940397442059868E-16, 1.000000000000000000 ) ) ;
#21609 = VECTOR ( 'NONE', #50661, 1000.000000000000000 ) ;
#21610 = AXIS2_PLACEMENT_3D ( 'NONE', #64604, #53655, #69211 ) ;
#21611 = DIRECTION ( 'NONE',  ( -1.000000000000000000, 0.000000000000000000, 0.000000000000000000 ) ) ;
#21612 = LINE ( 'NONE', #11329, #50719 ) ;
#21613 = EDGE_CURVE ( 'NONE', #36374, #37725, #30403, .T. ) ;
#21614 = VERTEX_POINT ( 'NONE', #14492 ) ;
#21615 = CARTESIAN_POINT ( 'NONE',  ( 14.50000000000000000, -42.00000000000000000, 27.00000000000000000 ) ) ;
#21616 = VECTOR ( 'NONE', #38600, 1000.000000000000000 ) ;
#21619 = ORIENTED_EDGE ( 'NONE', *, *, #36019, .T. ) ;
#21618 = ADVANCED_FACE ( 'NONE', ( #4589 ), #36047, .T. ) ;
#21617 = PLANE ( 'NONE',  #15318 ) ;
#21621 = ORIENTED_EDGE ( 'NONE', *, *, #19080, .F. ) ;
#21620 = LINE ( 'NONE', #48841, #60389 ) ;
#21622 = DIRECTION ( 'NONE',  ( 0.000000000000000000, 0.8346456692913390985, -0.5507872608668546999 ) ) ;
#21623 = VECTOR ( 'NONE', #25423, 1000.000000000000000 ) ;
#21624 = PLANE ( 'NONE',  #45360 ) ;
#21625 = AXIS2_PLACEMENT_3D ( 'NONE', #65528, #58503, #26660 ) ;
#21626 = VERTEX_POINT ( 'NONE', #26158 ) ;
#21627 = CARTESIAN_POINT ( 'NONE',  ( 6.665817930929297752, -7.357023737882824044, 54.00000000000000711 ) ) ;
#21628 = CARTESIAN_POINT ( 'NONE',  ( -10.30047626211725742, 3.650476262117184234, 26.00000000000000711 ) ) ;
#21629 = VERTEX_POINT ( 'NONE', #37119 ) ;
#21630 = LINE ( 'NONE', #32590, #17646 ) ;
#21631 = DIRECTION ( 'NONE',  ( -0.6414496315691473605, -0.7671651518153083105, -2.309356642089130002E-17 ) ) ;
#21632 = ORIENTED_EDGE ( 'NONE', *, *, #35365, .T. ) ;
#21633 = DIRECTION ( 'NONE',  ( 0.000000000000000000, 1.000000000000000000, 0.000000000000000000 ) ) ;
#21634 = EDGE_LOOP ( 'NONE', ( #9751, #399, #48864, #14768 ) ) ;
#21635 = ORIENTED_EDGE ( 'NONE', *, *, #6606, .F. ) ;
#21636 = DIRECTION ( 'NONE',  ( -1.000000000000000000, 0.000000000000000000, 0.000000000000000000 ) ) ;
#21637 = DIRECTION ( 'NONE',  ( 0.000000000000000000, 0.000000000000000000, -1.000000000000000000 ) ) ;
#21638 = CARTESIAN_POINT ( 'NONE',  ( 25.57999999999999829, 0.000000000000000000, 2.458500000000000796 ) ) ;
#21639 = FACE_OUTER_BOUND ( 'NONE', #33792, .T. ) ;
#21640 = EDGE_LOOP ( 'NONE', ( #3449, #67798, #12700, #57303 ) ) ;
#21641 = VERTEX_POINT ( 'NONE', #48416 ) ;
#21642 = AXIS2_PLACEMENT_3D ( 'NONE', #44971, #1839, #28709 ) ;
#21644 = ORIENTED_EDGE ( 'NONE', *, *, #12294, .F. ) ;
#21643 = CARTESIAN_POINT ( 'NONE',  ( 4.622483450353380263, -3.606483450353491271, 455.0000000000000568 ) ) ;
#21645 = ORIENTED_EDGE ( 'NONE', *, *, #65964, .T. ) ;
#21646 = EDGE_CURVE ( 'NONE', #13697, #65251, #1023, .T. ) ;
#21647 = PRODUCT_DEFINITION_SHAPE ( 'NONE', 'NONE',  #52984 ) ;
#21648 = CIRCLE ( 'NONE', #38603, 0.3499999999999308664 ) ;
#21649 = DIRECTION ( 'NONE',  ( 0.000000000000000000, -0.7071067811865475727, 0.7071067811865475727 ) ) ;
#21650 = CARTESIAN_POINT ( 'NONE',  ( -10.08346604330788665, -2.906483450353353426, 455.0000000000000568 ) ) ;
#21651 = DIRECTION ( 'NONE',  ( 0.3479852726768748461, 0.000000000000000000, 0.9375000000000006661 ) ) ;
#21652 = ADVANCED_FACE ( 'NONE', ( #42755 ), #32505, .F. ) ;
#21653 = CARTESIAN_POINT ( 'NONE',  ( 0.000000000000000000, 0.000000000000000000, 0.000000000000000000 ) ) ;
#21655 = DIRECTION ( 'NONE',  ( -0.000000000000000000, 3.673940397442059868E-16, -1.000000000000000000 ) ) ;
#21654 = DIRECTION ( 'NONE',  ( -0.000000000000000000, -0.000000000000000000, -1.000000000000000000 ) ) ;
#21656 = VERTEX_POINT ( 'NONE', #5969 ) ;
#21657 = ADVANCED_FACE ( 'NONE', ( #32148 ), #33181, .F. ) ;
#21659 = VERTEX_POINT ( 'NONE', #10576 ) ;
#21658 = FACE_OUTER_BOUND ( 'NONE', #51657, .T. ) ;
#21660 = VERTEX_POINT ( 'NONE', #320 ) ;
#21661 = ORIENTED_EDGE ( 'NONE', *, *, #14557, .F. ) ;
#21662 = VECTOR ( 'NONE', #36144, 1000.000000000000000 ) ;
#21663 = CLOSED_SHELL ( 'NONE', ( #16815, #55988, #49612, #15746, #52033, #56946, #39277, #69776, #40513, #25017, #61315, #47320 ) ) ;
#21664 = FACE_OUTER_BOUND ( 'NONE', #28800, .T. ) ;
#21665 = ADVANCED_FACE ( 'NONE', ( #60385 ), #11598, .F. ) ;
#21666 = DIRECTION ( 'NONE',  ( 0.000000000000000000, 0.000000000000000000, 1.000000000000000000 ) ) ;
#21667 = VECTOR ( 'NONE', #24765, 1000.000000000000000 ) ;
#21668 = CARTESIAN_POINT ( 'NONE',  ( 7.250000000000005329, -7.449999999999998401, -18.50000000000000000 ) ) ;
#21669 = ORIENTED_EDGE ( 'NONE', *, *, #29875, .F. ) ;
#21670 = ORIENTED_EDGE ( 'NONE', *, *, #22133, .T. ) ;
#21671 = VERTEX_POINT ( 'NONE', #15887 ) ;
#21673 = DIRECTION ( 'NONE',  ( -1.000000000000000000, 0.000000000000000000, 0.000000000000000000 ) ) ;
#21672 = VECTOR ( 'NONE', #69719, 1000.000000000000000 ) ;
#21674 = DIRECTION ( 'NONE',  ( 4.336808689942006692E-15, 1.000000000000000000, 0.000000000000000000 ) ) ;
#21675 = CARTESIAN_POINT ( 'NONE',  ( -24.00000000000000000, -15.50000000000000000, 19.33772233983200195 ) ) ;
#21676 = VERTEX_POINT ( 'NONE', #65710 ) ;
#21677 = ADVANCED_FACE ( 'NONE', ( #11262 ), #5631, .F. ) ;
#21678 = ORIENTED_EDGE ( 'NONE', *, *, #64488, .F. ) ;
#21679 = DIRECTION ( 'NONE',  ( 1.836970198721029934E-16, 1.836970198721010706E-16, -1.000000000000000000 ) ) ;
#21680 = DIRECTION ( 'NONE',  ( 0.000000000000000000, 0.000000000000000000, -1.000000000000000000 ) ) ;
#21681 = VERTEX_POINT ( 'NONE', #37462 ) ;
#21682 = ADVANCED_BREP_SHAPE_REPRESENTATION ( '', ( #43625, #45918 ), #47199 ) ;
#21683 = PLANE ( 'NONE',  #29104 ) ;
#21685 = VERTEX_POINT ( 'NONE', #54074 ) ;
#21684 = LINE ( 'NONE', #22384, #63386 ) ;
#21686 = ORIENTED_EDGE ( 'NONE', *, *, #19836, .T. ) ;
#21687 = CYLINDRICAL_SURFACE ( 'NONE', #52970, 0.1749999999999980738 ) ;
#21688 = CARTESIAN_POINT ( 'NONE',  ( -8.250000000000001776, 0.000000000000000000, -23.00000000000000000 ) ) ;
#21689 = LINE ( 'NONE', #22722, #47578 ) ;
#21690 = CIRCLE ( 'NONE', #32987, 4.000000000000000888 ) ;
#21691 = LINE ( 'NONE', #43936, #69614 ) ;
#21692 = DIRECTION ( 'NONE',  ( 0.000000000000000000, 0.000000000000000000, -1.000000000000000000 ) ) ;
#21693 = VECTOR ( 'NONE', #53438, 1000.000000000000000 ) ;
#21694 = ADVANCED_FACE ( 'NONE', ( #26857 ), #27198, .T. ) ;
#21695 = ORIENTED_EDGE ( 'NONE', *, *, #57844, .T. ) ;
#21696 = CARTESIAN_POINT ( 'NONE',  ( 9.900000000000000355, 18.00000000000000355, 21.00000000000000000 ) ) ;
#21698 = ORIENTED_EDGE ( 'NONE', *, *, #66476, .T. ) ;
#21697 = EDGE_CURVE ( 'NONE', #61197, #48072, #48761, .T. ) ;
#21699 = CARTESIAN_POINT ( 'NONE',  ( -14.25000000000000000, -2.500000000000000000, 23.22168783648699986 ) ) ;
#21700 = DIRECTION ( 'NONE',  ( -1.000000000000000000, 0.000000000000000000, 0.000000000000000000 ) ) ;
#21701 = EDGE_CURVE ( 'NONE', #53480, #22431, #28690, .T. ) ;
#21702 = DIRECTION ( 'NONE',  ( 0.000000000000000000, 0.000000000000000000, 1.000000000000000000 ) ) ;
#21703 = LINE ( 'NONE', #48926, #9199 ) ;
#21704 = PLANE ( 'NONE',  #17865 ) ;
#21705 = VECTOR ( 'NONE', #69899, 1000.000000000000000 ) ;
#21706 = VERTEX_POINT ( 'NONE', #53381 ) ;
#21707 = CARTESIAN_POINT ( 'NONE',  ( -9.249999999999998224, -7.848062532927998269, 0.000000000000000000 ) ) ;
#21708 = CARTESIAN_POINT ( 'NONE',  ( 78.77321854994620765, 47.95351654967443977, 39.00000000000000000 ) ) ;
#21709 = VECTOR ( 'NONE', #6332, 1000.000000000000000 ) ;
#21710 = VECTOR ( 'NONE', #63281, 1000.000000000000000 ) ;
#21711 = VERTEX_POINT ( 'NONE', #4933 ) ;
#21712 = PLANE ( 'NONE',  #38417 ) ;
#21713 = CARTESIAN_POINT ( 'NONE',  ( -30.00000000000000000, -5.200000000000001066, 9.400000000000000355 ) ) ;
#21714 = ORIENTED_EDGE ( 'NONE', *, *, #29379, .F. ) ;
#21715 = AXIS2_PLACEMENT_3D ( 'NONE', #20480, #31462, #63984 ) ;
#21716 = DIRECTION ( 'NONE',  ( 1.000000000000000000, -0.000000000000000000, 0.000000000000000000 ) ) ;
#21717 = DIRECTION ( 'NONE',  ( 0.000000000000000000, 0.000000000000000000, -1.000000000000000000 ) ) ;
#21718 = VERTEX_POINT ( 'NONE', #10929 ) ;
#21719 = DIRECTION ( 'NONE',  ( 4.121462285523434951E-16, 1.000000000000000000, 3.673940397442059868E-16 ) ) ;
#21720 = DIRECTION ( 'NONE',  ( 1.000000000000000000, 0.000000000000000000, 0.000000000000000000 ) ) ;
#21721 = DIRECTION ( 'NONE',  ( -1.836970198721029934E-16, 1.836970198721036590E-16, -1.000000000000000000 ) ) ;
#21722 = ORIENTED_EDGE ( 'NONE', *, *, #8799, .T. ) ;
#21724 = EDGE_LOOP ( 'NONE', ( #17491, #53574, #11184, #40286 ) ) ;
#21723 = CARTESIAN_POINT ( 'NONE',  ( 8.900000000000005684, -0.2000000000089119934, -8.913009219568841313E-12 ) ) ;
#21725 = ADVANCED_FACE ( 'NONE', ( #64667 ), #26497, .T. ) ;
#21726 = DIRECTION ( 'NONE',  ( -0.000000000000000000, -0.000000000000000000, -1.000000000000000000 ) ) ;
#21727 = DIRECTION ( 'NONE',  ( -0.000000000000000000, -0.000000000000000000, -1.000000000000000000 ) ) ;
#21728 = DIRECTION ( 'NONE',  ( 0.000000000000000000, 0.7071067811865074937, 0.7071067811865876518 ) ) ;
#21729 = VERTEX_POINT ( 'NONE', #37805 ) ;
#21730 = EDGE_CURVE ( 'NONE', #21280, #65046, #59368, .T. ) ;
#21731 = FILL_AREA_STYLE ('',( #37654 ) ) ;
#21732 = LINE ( 'NONE', #65231, #40909 ) ;
#21733 = EDGE_CURVE ( 'NONE', #1307, #58955, #29806, .T. ) ;
#21734 = CIRCLE ( 'NONE', #61216, 24.99999999998789946 ) ;
#21735 = EDGE_LOOP ( 'NONE', ( #5487, #49185, #52276, #39558, #57276, #21048, #64340 ) ) ;
#21736 = VERTEX_POINT ( 'NONE', #49099 ) ;
#21737 = EDGE_CURVE ( 'NONE', #6284, #35692, #50141, .T. ) ;
#21738 = ORIENTED_EDGE ( 'NONE', *, *, #31529, .F. ) ;
#21739 = EDGE_CURVE ( 'NONE', #60151, #30310, #43798, .T. ) ;
#21740 = EDGE_CURVE ( 'NONE', #48173, #11798, #28556, .T. ) ;
#21741 = FACE_OUTER_BOUND ( 'NONE', #2092, .T. ) ;
#21742 = CARTESIAN_POINT ( 'NONE',  ( 280.0000000000000000, -25.50000000000000355, -16.00000000000000711 ) ) ;
#21743 = EDGE_CURVE ( 'NONE', #57686, #28197, #12630, .T. ) ;
#21744 = ORIENTED_EDGE ( 'NONE', *, *, #17258, .F. ) ;
#21745 = ORIENTED_EDGE ( 'NONE', *, *, #15924, .F. ) ;
#21746 = VERTEX_POINT ( 'NONE', #56142 ) ;
#21747 = VECTOR ( 'NONE', #43904, 1000.000000000000000 ) ;
#21748 = DIRECTION ( 'NONE',  ( 1.000000000000000000, -1.813998472013049506E-14, 0.000000000000000000 ) ) ;
#21749 = ORIENTED_EDGE ( 'NONE', *, *, #34956, .F. ) ;
#21750 = ORIENTED_EDGE ( 'NONE', *, *, #42396, .F. ) ;
#21751 = AXIS2_PLACEMENT_3D ( 'NONE', #50673, #7178, #66590 ) ;
#21752 = ORIENTED_EDGE ( 'NONE', *, *, #50852, .F. ) ;
#21753 = VERTEX_POINT ( 'NONE', #2388 ) ;
#21754 = CARTESIAN_POINT ( 'NONE',  ( -25.50000000000000355, 0.000000000000000000, -22.50000000000000000 ) ) ;
#21755 = UNCERTAINTY_MEASURE_WITH_UNIT (LENGTH_MEASURE( 1.000000000000000082E-05 ), #23818, 'distance_accuracy_value', 'NONE');
#21757 = ORIENTED_EDGE ( 'NONE', *, *, #14556, .T. ) ;
#21756 = CARTESIAN_POINT ( 'NONE',  ( 7.606483450353380249, -11.78648345035349010, 455.0000000000000568 ) ) ;
#21758 = DIRECTION ( 'NONE',  ( 0.6414496315691494699, 0.7671651518153064231, 0.000000000000000000 ) ) ;
#21760 = DIRECTION ( 'NONE',  ( 0.000000000000000000, 1.000000000000000000, 1.880440247955334083E-12 ) ) ;
#21759 = VECTOR ( 'NONE', #40842, 1000.000000000000000 ) ;
#21761 = DIRECTION ( 'NONE',  ( 0.000000000000000000, -0.5017180897718492849, 0.8650311892618014475 ) ) ;
#21762 = ORIENTED_EDGE ( 'NONE', *, *, #26637, .F. ) ;
#21763 = AXIS2_PLACEMENT_3D ( 'NONE', #22494, #44038, #44723 ) ;
#21764 = AXIS2_PLACEMENT_3D ( 'NONE', #18826, #61954, #18118 ) ;
#21765 = CARTESIAN_POINT ( 'NONE',  ( -3.593516549646712299, 4.609516549646604844, 455.0000000000000568 ) ) ;
#21766 = AXIS2_PLACEMENT_3D ( 'NONE', #51604, #44534, #12699 ) ;
#21767 = DIRECTION ( 'NONE',  ( 0.000000000000000000, 0.000000000000000000, 1.000000000000000000 ) ) ;
#21768 = EDGE_LOOP ( 'NONE', ( #43042, #25031, #19305, #13066 ) ) ;
#21769 = CARTESIAN_POINT ( 'NONE',  ( 283.0000000000000568, -25.14575131106458272, -17.35424868893542083 ) ) ;
#21770 = ADVANCED_FACE ( 'NONE', ( #6989 ), #28221, .F. ) ;
#21771 = EDGE_CURVE ( 'NONE', #46957, #56934, #19002, .T. ) ;
#21772 = DIRECTION ( 'NONE',  ( 1.000000000000000000, 0.000000000000000000, 0.000000000000000000 ) ) ;
#21773 = DIRECTION ( 'NONE',  ( 0.000000000000000000, 0.000000000000000000, -1.000000000000000000 ) ) ;
#21774 = EDGE_LOOP ( 'NONE', ( #10047, #34849, #48193, #56215 ) ) ;
#21775 = EDGE_CURVE ( 'NONE', #42524, #24992, #37751, .T. ) ;
#21776 = PLANE ( 'NONE',  #832 ) ;
#21777 = EDGE_CURVE ( 'NONE', #20922, #21542, #51173, .T. ) ;
#21778 = DIRECTION ( 'NONE',  ( -4.121462285523434951E-16, -1.000000000000000000, -0.000000000000000000 ) ) ;
#21779 = CARTESIAN_POINT ( 'NONE',  ( 46.39999999999999858, 21.00000000000000000, -0.2500000000000000000 ) ) ;
#21780 = VECTOR ( 'NONE', #54948, 1000.000000000000000 ) ;
#21781 = EDGE_CURVE ( 'NONE', #65232, #9638, #58084, .T. ) ;
#21782 = CARTESIAN_POINT ( 'NONE',  ( 32.89999999999999858, -0.2000000000089119934, 8.909539772616881237E-12 ) ) ;
#21783 = LINE ( 'NONE', #31710, #3111 ) ;
#21784 = CARTESIAN_POINT ( 'NONE',  ( -7.342976262117293373, -6.665817930929262225, 54.00000000000000711 ) ) ;
#21785 = AXIS2_PLACEMENT_3D ( 'NONE', #26389, #217, #54308 ) ;
#21786 =( NAMED_UNIT ( * ) SI_UNIT ( $, .STERADIAN. ) SOLID_ANGLE_UNIT ( ) );
#21787 = DIRECTION ( 'NONE',  ( -0.000000000000000000, -0.000000000000000000, -1.000000000000000000 ) ) ;
#21788 = ORIENTED_EDGE ( 'NONE', *, *, #9999, .T. ) ;
#21789 = CARTESIAN_POINT ( 'NONE',  ( 283.0000000000000568, -31.30000000000000071, -8.400000000000000355 ) ) ;
#21790 = LINE ( 'NONE', #54323, #16112 ) ;
#21791 = AXIS2_PLACEMENT_3D ( 'NONE', #43128, #15921, #31846 ) ;
#21792 = DIRECTION ( 'NONE',  ( 0.000000000000000000, -1.000000000000000000, 0.000000000000000000 ) ) ;
#21793 = CARTESIAN_POINT ( 'NONE',  ( 23.90000000000000213, -21.00000000000001421, -13.86939075806900945 ) ) ;
#21794 = VERTEX_POINT ( 'NONE', #28908 ) ;
#21795 = CARTESIAN_POINT ( 'NONE',  ( -7.250000000000000888, 7.450000000000003730, -25.50000000000000355 ) ) ;
#21796 = DIRECTION ( 'NONE',  ( 1.000000000000000000, 0.000000000000000000, 0.000000000000000000 ) ) ;
#21797 = DIRECTION ( 'NONE',  ( 1.000000000000000000, 0.000000000000000000, 0.000000000000000000 ) ) ;
#21798 = CARTESIAN_POINT ( 'NONE',  ( -6.486996718459908884, -3.157023737882779013, 26.00000000000000711 ) ) ;
#21799 = SURFACE_SIDE_STYLE ('',( #15465 ) ) ;
#21800 = DIRECTION ( 'NONE',  ( 1.000000000000000000, 0.000000000000000000, 0.000000000000000000 ) ) ;
#21801 = VERTEX_POINT ( 'NONE', #50482 ) ;
#21802 = AXIS2_PLACEMENT_3D ( 'NONE', #44935, #66499, #65477 ) ;
#21803 = VERTEX_POINT ( 'NONE', #7683 ) ;
#21804 = DIRECTION ( 'NONE',  ( 0.000000000000000000, 0.7071067811865474617, -0.7071067811865474617 ) ) ;
#21805 = CARTESIAN_POINT ( 'NONE',  ( -2.617976262117251540, 6.486996718459834277, 54.00000000000000711 ) ) ;
#21806 = EDGE_LOOP ( 'NONE', ( #64972, #66343 ) ) ;
#21807 = CARTESIAN_POINT ( 'NONE',  ( 7.428221114745000797, 3.593516549646565750, 455.0000000000000568 ) ) ;
#21808 = VECTOR ( 'NONE', #56143, 1000.000000000000000 ) ;
#21809 = LINE ( 'NONE', #34130, #19412 ) ;
#21810 = ORIENTED_EDGE ( 'NONE', *, *, #53413, .T. ) ;
#21811 = DIRECTION ( 'NONE',  ( 0.000000000000000000, 0.000000000000000000, -1.000000000000000000 ) ) ;
#21812 = ORIENTED_EDGE ( 'NONE', *, *, #67041, .F. ) ;
#21813 = CIRCLE ( 'NONE', #22965, 0.2000000000000005107 ) ;
#21814 = ORIENTED_EDGE ( 'NONE', *, *, #33705, .T. ) ;
#21815 = LINE ( 'NONE', #31743, #164 ) ;
#21816 = EDGE_CURVE ( 'NONE', #31048, #5249, #36627, .T. ) ;
#21817 = VERTEX_POINT ( 'NONE', #62123 ) ;
#21818 = DIRECTION ( 'NONE',  ( 0.7671651518152963201, -0.6414496315691619044, -2.356647714346269747E-16 ) ) ;
#21819 = LINE ( 'NONE', #6249, #63224 ) ;
#21820 = DIRECTION ( 'NONE',  ( 1.000000000000000000, -0.000000000000000000, 0.000000000000000000 ) ) ;
#21821 = EDGE_CURVE ( 'NONE', #18330, #28426, #23090, .T. ) ;
#21822 = ORIENTED_EDGE ( 'NONE', *, *, #6637, .T. ) ;
#21823 = ORIENTED_EDGE ( 'NONE', *, *, #56146, .T. ) ;
#21824 = CARTESIAN_POINT ( 'NONE',  ( 7.450000000000006395, 7.250000000000000888, -15.00000000000000000 ) ) ;
#21826 = CARTESIAN_POINT ( 'NONE',  ( 283.0000000000000568, -20.40000000000000213, 17.35424868893542438 ) ) ;
#21825 = DIRECTION ( 'NONE',  ( -1.836970198721029934E-16, -1.836970198721010706E-16, 1.000000000000000000 ) ) ;
#21827 = VERTEX_POINT ( 'NONE', #12283 ) ;
#21828 = AXIS2_PLACEMENT_3D ( 'NONE', #30491, #14578, #14232 ) ;
#21829 = ORIENTED_EDGE ( 'NONE', *, *, #57887, .T. ) ;
#21830 = ORIENTED_EDGE ( 'NONE', *, *, #5079, .T. ) ;
#21831 = CARTESIAN_POINT ( 'NONE',  ( 8.900000000000005684, 14.08845687959340331, -21.00000000000000000 ) ) ;
#21832 = AXIS2_PLACEMENT_3D ( 'NONE', #8417, #57222, #49241 ) ;
#21833 = EDGE_CURVE ( 'NONE', #27500, #27698, #18290, .T. ) ;
#21835 = ORIENTED_EDGE ( 'NONE', *, *, #62952, .F. ) ;
#21834 = CARTESIAN_POINT ( 'NONE',  ( 7.250000000000005329, -7.249999999999998224, -25.50000000000000355 ) ) ;
#21836 = CARTESIAN_POINT ( 'NONE',  ( 29.25000000000000000, -5.000000000000000000, 26.25000000000000000 ) ) ;
#21837 = CARTESIAN_POINT ( 'NONE',  ( 9.404523737882747980, 0.9414762621171599566, 26.00000000000000711 ) ) ;
#21838 = VERTEX_POINT ( 'NONE', #55108 ) ;
#21839 = ORIENTED_EDGE ( 'NONE', *, *, #30224, .T. ) ;
#21840 = VECTOR ( 'NONE', #7365, 1000.000000000000114 ) ;
#21841 = PLANE ( 'NONE',  #56061 ) ;
#21842 = ORIENTED_EDGE ( 'NONE', *, *, #2409, .T. ) ;
#21843 = DIRECTION ( 'NONE',  ( -0.000000000000000000, -0.000000000000000000, -1.000000000000000000 ) ) ;
#21844 = CARTESIAN_POINT ( 'NONE',  ( -2.993516549646701108, 7.415254214038204061, 455.0000000000000568 ) ) ;
#21845 = VERTEX_POINT ( 'NONE', #61417 ) ;
#21846 = VECTOR ( 'NONE', #45592, 1000.000000000000000 ) ;
#21847 =( NAMED_UNIT ( * ) PLANE_ANGLE_UNIT ( ) SI_UNIT ( $, .RADIAN. ) );
#21848 = DIRECTION ( 'NONE',  ( 0.000000000000000000, 0.000000000000000000, 1.000000000000000000 ) ) ;
#21850 = ORIENTED_EDGE ( 'NONE', *, *, #8941, .T. ) ;
#21849 = DIRECTION ( 'NONE',  ( 0.000000000000000000, 0.000000000000000000, -1.000000000000000000 ) ) ;
#21851 = ORIENTED_EDGE ( 'NONE', *, *, #10600, .T. ) ;
#21853 = CARTESIAN_POINT ( 'NONE',  ( 0.000000000000000000, 20.50000000000002487, 17.79289321881347163 ) ) ;
#21852 = VECTOR ( 'NONE', #44133, 1000.000000000000000 ) ;
#21854 = VECTOR ( 'NONE', #11517, 1000.000000000000000 ) ;
#21856 = CIRCLE ( 'NONE', #60211, 1.929199999999998916 ) ;
#21855 = DIRECTION ( 'NONE',  ( -1.000000000000000000, 0.000000000000000000, 0.000000000000000000 ) ) ;
#21857 = CARTESIAN_POINT ( 'NONE',  ( -30.00000000000000000, -11.10796162543699950, 9.102987789146602893 ) ) ;
#21858 = DIRECTION ( 'NONE',  ( 1.000000000000000000, -0.000000000000000000, -0.000000000000000000 ) ) ;
#21859 = EDGE_CURVE ( 'NONE', #4446, #1910, #51306, .T. ) ;
#21860 = VECTOR ( 'NONE', #14009, 1000.000000000000000 ) ;
#21861 = VECTOR ( 'NONE', #18414, 1000.000000000000000 ) ;
#21862 = DIRECTION ( 'NONE',  ( 0.000000000000000000, 0.000000000000000000, -1.000000000000000000 ) ) ;
#21863 = EDGE_LOOP ( 'NONE', ( #15051, #2096, #16717, #23764 ) ) ;
#21864 = DIRECTION ( 'NONE',  ( 2.135044278125299371E-15, 1.000000000000000000, 0.000000000000000000 ) ) ;
#21865 = DIRECTION ( 'NONE',  ( -1.000000000000000000, 0.000000000000000000, 0.000000000000000000 ) ) ;
#21866 = CARTESIAN_POINT ( 'NONE',  ( -15.50000000000000000, -5.000000000000000000, 26.00000000000000000 ) ) ;
#21868 = ORIENTED_EDGE ( 'NONE', *, *, #28042, .F. ) ;
#21867 = CARTESIAN_POINT ( 'NONE',  ( -11.00000000000000000, -11.50000000000100009, 15.00000000000084910 ) ) ;
#21869 = DIRECTION ( 'NONE',  ( 0.000000000000000000, 0.7071067811865495711, 0.7071067811865455743 ) ) ;
#21870 = CARTESIAN_POINT ( 'NONE',  ( -30.00000000000000000, -11.50000000000000000, 19.00000000000000000 ) ) ;
#21871 = CARTESIAN_POINT ( 'NONE',  ( -9.897976262117243351, -3.682023737882718972, 26.00000000000000000 ) ) ;
#21872 = EDGE_CURVE ( 'NONE', #24588, #11628, #28739, .T. ) ;
#21873 = DIRECTION ( 'NONE',  ( 0.7071067811865446862, -0.7071067811865503483, 0.000000000000000000 ) ) ;
#21874 = VERTEX_POINT ( 'NONE', #29245 ) ;
#21875 = DIRECTION ( 'NONE',  ( -1.000000000000000000, 0.000000000000000000, 0.000000000000000000 ) ) ;
#21876 = FACE_OUTER_BOUND ( 'NONE', #30532, .T. ) ;
#21877 = ORIENTED_EDGE ( 'NONE', *, *, #48311, .F. ) ;
#21878 = LINE ( 'NONE', #43436, #22121 ) ;
#21879 = CARTESIAN_POINT ( 'NONE',  ( -7.450000000000001954, 7.250000000000000000, -13.00000000000000178 ) ) ;
#21880 = CARTESIAN_POINT ( 'NONE',  ( 49.00000000000000000, -0.2000000000089119934, 8.909539772616881237E-12 ) ) ;
#21881 = EDGE_CURVE ( 'NONE', #7012, #4376, #44469, .T. ) ;
#21882 = DIRECTION ( 'NONE',  ( -1.000000000000000000, 0.000000000000000000, 0.000000000000000000 ) ) ;
#21883 = DIRECTION ( 'NONE',  ( -1.000000000000000000, 0.000000000000000000, 0.000000000000000000 ) ) ;
#21884 = ORIENTED_EDGE ( 'NONE', *, *, #51754, .F. ) ;
#21885 = ORIENTED_EDGE ( 'NONE', *, *, #7324, .F. ) ;
#21886 = DIRECTION ( 'NONE',  ( 0.7671651518153106419, 0.6414496315691445849, 0.000000000000000000 ) ) ;
#21887 = ORIENTED_EDGE ( 'NONE', *, *, #42492, .T. ) ;
#21888 = LINE ( 'NONE', #36870, #34477 ) ;
#21889 = ORIENTED_EDGE ( 'NONE', *, *, #65503, .F. ) ;
#21890 = CIRCLE ( 'NONE', #44423, 0.1999999999999996503 ) ;
#21891 = DIRECTION ( 'NONE',  ( -1.000000000000000000, 0.000000000000000000, 0.000000000000000000 ) ) ;
#21892 = PLANE ( 'NONE',  #54767 ) ;
#21893 = CARTESIAN_POINT ( 'NONE',  ( 40.90000000000000568, 0.000000000000000000, 3.447897592003593022E-15 ) ) ;
#21894 = ORIENTED_EDGE ( 'NONE', *, *, #63531, .F. ) ;
#21895 = EDGE_LOOP ( 'NONE', ( #26932, #42095, #53999, #3113 ) ) ;
#21896 = CARTESIAN_POINT ( 'NONE',  ( 7.250000000000005329, -7.249999999999998224, -10.00000000000000000 ) ) ;
#21897 = ORIENTED_EDGE ( 'NONE', *, *, #43067, .F. ) ;
#21898 = VERTEX_POINT ( 'NONE', #45512 ) ;
#21899 = ADVANCED_FACE ( 'NONE', ( #67085 ), #66038, .F. ) ;
#21900 = CARTESIAN_POINT ( 'NONE',  ( -9.750000000000001776, 9.690000000000001279, -5.000000000000000000 ) ) ;
#21901 = LINE ( 'NONE', #26177, #15513 ) ;
#21902 = VECTOR ( 'NONE', #49453, 1000.000000000000000 ) ;
#21903 = VECTOR ( 'NONE', #9745, 1000.000000000000114 ) ;
#21904 = FACE_OUTER_BOUND ( 'NONE', #17204, .T. ) ;
#21905 = ADVANCED_FACE ( 'NONE', ( #40212 ), #13347, .F. ) ;
#21906 = EDGE_CURVE ( 'NONE', #33844, #63336, #29600, .T. ) ;
#21907 = ORIENTED_EDGE ( 'NONE', *, *, #51281, .T. ) ;
#21908 = CARTESIAN_POINT ( 'NONE',  ( 7.532023737882783898, 3.834182069070696031, 54.00000000000000711 ) ) ;
#21910 = DIRECTION ( 'NONE',  ( -1.000000000000000000, 0.000000000000000000, 0.000000000000000000 ) ) ;
#21909 = LINE ( 'NONE', #11290, #9567 ) ;
#21911 = ORIENTED_EDGE ( 'NONE', *, *, #55276, .F. ) ;
#21912 = AXIS2_PLACEMENT_3D ( 'NONE', #47118, #25194, #47802 ) ;
#21914 = VERTEX_POINT ( 'NONE', #24661 ) ;
#21913 = AXIS2_PLACEMENT_3D ( 'NONE', #47518, #30210, #52480 ) ;
#21917 = ORIENTED_EDGE ( 'NONE', *, *, #47464, .T. ) ;
#21916 = ADVANCED_FACE ( 'NONE', ( #20055 ), #63187, .F. ) ;
#21915 = CARTESIAN_POINT ( 'NONE',  ( 11.50000000000000000, -11.70000000000012008, 10.70000000000011831 ) ) ;
#21918 = ORIENTED_EDGE ( 'NONE', *, *, #58097, .F. ) ;
#21919 = EDGE_CURVE ( 'NONE', #68564, #32818, #8745, .T. ) ;
#21920 = VECTOR ( 'NONE', #14950, 1000.000000000000000 ) ;
#21921 = CIRCLE ( 'NONE', #5962, 24.99999999998789946 ) ;
#21922 = EDGE_CURVE ( 'NONE', #17131, #67314, #38892, .T. ) ;
#21923 = DIRECTION ( 'NONE',  ( -1.000000000000000000, 0.000000000000000000, -0.000000000000000000 ) ) ;
#21924 = EDGE_CURVE ( 'NONE', #15298, #33692, #68275, .T. ) ;
#21925 = VERTEX_POINT ( 'NONE', #52950 ) ;
#21926 = EDGE_LOOP ( 'NONE', ( #50635, #64852, #38694, #2315 ) ) ;
#21927 = CARTESIAN_POINT ( 'NONE',  ( 31.89999999999999858, -21.00000000000000000, 13.86939075806900057 ) ) ;
#21928 = LINE ( 'NONE', #27578, #32357 ) ;
#21929 = ORIENTED_EDGE ( 'NONE', *, *, #16466, .F. ) ;
#21930 = CARTESIAN_POINT ( 'NONE',  ( 11.00000000000000000, -12.00000000000000000, -12.20000000000000107 ) ) ;
#21931 = CARTESIAN_POINT ( 'NONE',  ( 7.250000000000004441, 7.450000000000001954, -21.00000000000000000 ) ) ;
#21932 = DIRECTION ( 'NONE',  ( 3.491481338843133355E-15, 1.000000000000000000, 1.836970198721029934E-16 ) ) ;
#21933 = ORIENTED_EDGE ( 'NONE', *, *, #47067, .T. ) ;
#21934 = DIRECTION ( 'NONE',  ( -0.000000000000000000, -0.000000000000000000, 1.000000000000000000 ) ) ;
#21935 = EDGE_CURVE ( 'NONE', #35258, #42826, #51885, .T. ) ;
#21936 = CARTESIAN_POINT ( 'NONE',  ( 9.955011587777223170, 2.752095193409229257, 455.0000000000000568 ) ) ;
#21937 = CIRCLE ( 'NONE', #15185, 1.000000000000001776 ) ;
#21938 = EDGE_LOOP ( 'NONE', ( #44122, #34810, #4121, #38843 ) ) ;
#21940 = ORIENTED_EDGE ( 'NONE', *, *, #54954, .T. ) ;
#21939 = FACE_OUTER_BOUND ( 'NONE', #64257, .T. ) ;
#21941 = CARTESIAN_POINT ( 'NONE',  ( 0.000000000000000000, 0.000000000000000000, 0.000000000000000000 ) ) ;
#21942 = CARTESIAN_POINT ( 'NONE',  ( 24.00000000000000000, -15.50000000000000000, -19.33772233983200195 ) ) ;
#21943 = LINE ( 'NONE', #65767, #60624 ) ;
#21944 = CARTESIAN_POINT ( 'NONE',  ( 3.857023737882783188, -9.912023737882810437, 54.00000000000000711 ) ) ;
#21945 = EDGE_CURVE ( 'NONE', #16520, #4997, #3445, .T. ) ;
#21946 = DIRECTION ( 'NONE',  ( -1.000000000000000000, 0.000000000000000000, 0.000000000000000000 ) ) ;
#21947 = CARTESIAN_POINT ( 'NONE',  ( -3.842976262117332453, -10.31452373788281740, 54.00000000000000711 ) ) ;
#21948 = ORIENTED_EDGE ( 'NONE', *, *, #28420, .F. ) ;
#21949 = CARTESIAN_POINT ( 'NONE',  ( -11.00000000000000000, -9.487228132326899654, -12.50000000000000000 ) ) ;
#21951 = VERTEX_POINT ( 'NONE', #14755 ) ;
#21950 = CARTESIAN_POINT ( 'NONE',  ( 7.250000000000005329, 8.250000000000001776, -26.00000000000001066 ) ) ;
#21953 = ORIENTED_EDGE ( 'NONE', *, *, #64928, .F. ) ;
#21952 = PLANE ( 'NONE',  #9588 ) ;
#21954 = CIRCLE ( 'NONE', #11788, 0.5000000000001392220 ) ;
#21955 = VECTOR ( 'NONE', #38949, 1000.000000000000114 ) ;
#21956 = CARTESIAN_POINT ( 'NONE',  ( 7.000000000000000000, -25.60000000000000142, -16.03137303340311348 ) ) ;
#21957 = LINE ( 'NONE', #26574, #21672 ) ;
#21958 = AXIS2_PLACEMENT_3D ( 'NONE', #1442, #59810, #11366 ) ;
#21959 = VECTOR ( 'NONE', #29076, 1000.000000000000000 ) ;
#21960 = VERTEX_POINT ( 'NONE', #20748 ) ;
#21961 = CARTESIAN_POINT ( 'NONE',  ( -4.173516549646666185, 11.99351654964658920, 455.0000000000000568 ) ) ;
#21962 = CARTESIAN_POINT ( 'NONE',  ( 16.90000000000000213, 0.000000000000000000, 8.619743980008982554E-16 ) ) ;
#21963 = ORIENTED_EDGE ( 'NONE', *, *, #36177, .T. ) ;
#21964 = CARTESIAN_POINT ( 'NONE',  ( 11.50000000000000000, -11.50000000000100009, 10.50000000000065903 ) ) ;
#21965 = DIRECTION ( 'NONE',  ( -1.000000000000000000, 0.000000000000000000, 0.000000000000000000 ) ) ;
#21966 = CIRCLE ( 'NONE', #62572, 0.1999999999999987899 ) ;
#21967 = DIRECTION ( 'NONE',  ( 1.000000000000000000, -0.000000000000000000, -0.000000000000000000 ) ) ;
#21968 = EDGE_CURVE ( 'NONE', #25188, #3392, #15240, .T. ) ;
#21969 = CARTESIAN_POINT ( 'NONE',  ( 176.0064834503533575, 2.160375375128253950, 5.000000000000000000 ) ) ;
#21970 = ORIENTED_EDGE ( 'NONE', *, *, #37172, .F. ) ;
#21971 = CARTESIAN_POINT ( 'NONE',  ( 275.5000000000000000, -42.50000000000000000, 15.10000000000000142 ) ) ;
#21972 = ORIENTED_EDGE ( 'NONE', *, *, #59467, .F. ) ;
#21973 = EDGE_CURVE ( 'NONE', #39038, #15670, #3789, .T. ) ;
#21974 = ORIENTED_EDGE ( 'NONE', *, *, #34809, .T. ) ;
#21976 = EDGE_CURVE ( 'NONE', #33844, #11146, #47623, .T. ) ;
#21975 = AXIS2_PLACEMENT_3D ( 'NONE', #15586, #3915, #26183 ) ;
#21977 = PLANE ( 'NONE',  #53959 ) ;
#21978 = CARTESIAN_POINT ( 'NONE',  ( -7.813516549646836395, -11.78648345035340661, 455.0000000000000568 ) ) ;
#21979 = EDGE_CURVE ( 'NONE', #14406, #12509, #57878, .T. ) ;
#21980 = EDGE_CURVE ( 'NONE', #38683, #40165, #26493, .T. ) ;
#21981 = EDGE_CURVE ( 'NONE', #45407, #19689, #41260, .T. ) ;
#21982 = DIRECTION ( 'NONE',  ( 0.000000000000000000, 0.000000000000000000, -1.000000000000000000 ) ) ;
#21983 = CARTESIAN_POINT ( 'NONE',  ( 9.737023737882815055, -2.544523737882825820, 54.00000000000000711 ) ) ;
#21984 = VERTEX_POINT ( 'NONE', #40911 ) ;
#21985 = VERTEX_POINT ( 'NONE', #35242 ) ;
#21987 = ORIENTED_EDGE ( 'NONE', *, *, #59894, .T. ) ;
#21986 = DIRECTION ( 'NONE',  ( 0.7071067811865451302, -0.7071067811865500152, -2.597868168706484048E-16 ) ) ;
#21988 = EDGE_CURVE ( 'NONE', #29287, #43823, #46814, .T. ) ;
#21989 = ORIENTED_EDGE ( 'NONE', *, *, #6013, .F. ) ;
#21990 = FACE_OUTER_BOUND ( 'NONE', #36440, .T. ) ;
#21991 = DIRECTION ( 'NONE',  ( 0.000000000000000000, -0.1249999999999996531, -0.9921567416492215186 ) ) ;
#21992 = EDGE_CURVE ( 'NONE', #7898, #68617, #41970, .T. ) ;
#21993 = CARTESIAN_POINT ( 'NONE',  ( 7.250000000000005329, -8.249999999999998224, -15.50000000000000000 ) ) ;
#21994 = EDGE_CURVE ( 'NONE', #68084, #25376, #63549, .T. ) ;
#21995 = LINE ( 'NONE', #11377, #24373 ) ;
#21997 = DIRECTION ( 'NONE',  ( 1.000000000000000000, 0.000000000000000000, 0.000000000000000000 ) ) ;
#21996 = CARTESIAN_POINT ( 'NONE',  ( -9.093516549646711411, 11.11351654964659730, 455.0000000000000568 ) ) ;
#21998 = ORIENTED_EDGE ( 'NONE', *, *, #49654, .F. ) ;
#22000 = VERTEX_POINT ( 'NONE', #25725 ) ;
#21999 = PLANE ( 'NONE',  #64640 ) ;
#22001 = VECTOR ( 'NONE', #16842, 1000.000000000000000 ) ;
#22002 = ORIENTED_EDGE ( 'NONE', *, *, #50911, .F. ) ;
#22003 = VERTEX_POINT ( 'NONE', #68850 ) ;
#22004 = CARTESIAN_POINT ( 'NONE',  ( -11.11351654964675539, -9.106483450353326958, 195.0000000000000284 ) ) ;
#22005 = EDGE_CURVE ( 'NONE', #31165, #11267, #8390, .T. ) ;
#22006 = DIRECTION ( 'NONE',  ( -1.000000000000000000, 0.000000000000000000, 0.000000000000000000 ) ) ;
#22007 = EDGE_CURVE ( 'NONE', #33692, #43764, #35598, .T. ) ;
#22008 = AXIS2_PLACEMENT_3D ( 'NONE', #47092, #35407, #3605 ) ;
#22010 = LINE ( 'NONE', #43570, #30901 ) ;
#22009 = VECTOR ( 'NONE', #54107, 1000.000000000000000 ) ;
#22011 = ORIENTED_EDGE ( 'NONE', *, *, #14012, .F. ) ;
#22012 = VERTEX_POINT ( 'NONE', #56823 ) ;
#22013 = ORIENTED_EDGE ( 'NONE', *, *, #34321, .T. ) ;
#22014 = FACE_OUTER_BOUND ( 'NONE', #2168, .T. ) ;
#22015 = CIRCLE ( 'NONE', #69408, 1.000000000000000000 ) ;
#22016 = AXIS2_PLACEMENT_3D ( 'NONE', #32524, #54087, #10586 ) ;
#22017 = LINE ( 'NONE', #48198, #9451 ) ;
#22018 = LINE ( 'NONE', #54206, #24362 ) ;
#22019 = EDGE_CURVE ( 'NONE', #58904, #48024, #8378, .T. ) ;
#22020 = ORIENTED_EDGE ( 'NONE', *, *, #65253, .F. ) ;
#22021 = ORIENTED_EDGE ( 'NONE', *, *, #55564, .F. ) ;
#22022 = CARTESIAN_POINT ( 'NONE',  ( 3.682023737882814007, 9.722976262117208890, 26.00000000000000711 ) ) ;
#22023 = VECTOR ( 'NONE', #68002, 1000.000000000000000 ) ;
#22024 = LINE ( 'NONE', #43583, #24361 ) ;
#22025 = ORIENTED_EDGE ( 'NONE', *, *, #38797, .T. ) ;
#22026 = AXIS2_PLACEMENT_3D ( 'NONE', #55690, #29159, #1261 ) ;
#22027 = DIRECTION ( 'NONE',  ( 0.000000000000000000, -1.000000000000000000, 0.000000000000000000 ) ) ;
#22028 = CIRCLE ( 'NONE', #11851, 1.000000000000000000 ) ;
#22030 = VERTEX_POINT ( 'NONE', #37036 ) ;
#22029 = LINE ( 'NONE', #38299, #45286 ) ;
#22031 = CIRCLE ( 'NONE', #19786, 4.500000000000190958 ) ;
#22032 = VERTEX_POINT ( 'NONE', #10835 ) ;
#22033 = DIRECTION ( 'NONE',  ( -0.000000000000000000, 3.673940397442059868E-16, -1.000000000000000000 ) ) ;
#22034 = CARTESIAN_POINT ( 'NONE',  ( -9.828310488886000229, -2.290483450353309358, 195.0000000000000284 ) ) ;
#22035 = CARTESIAN_POINT ( 'NONE',  ( 26.90000000000000213, -21.00000000000000000, 13.86939075806900057 ) ) ;
#22036 = PLANE ( 'NONE',  #65128 ) ;
#22037 = EDGE_CURVE ( 'NONE', #67299, #16582, #64903, .T. ) ;
#22038 = CARTESIAN_POINT ( 'NONE',  ( 41.09999999999999432, -0.1999999999911795112, 8.826273045769999343E-12 ) ) ;
#22039 = ORIENTED_EDGE ( 'NONE', *, *, #26931, .F. ) ;
#22040 = FACE_BOUND ( 'NONE', #49911, .T. ) ;
#22041 = EDGE_CURVE ( 'NONE', #51945, #20060, #21110, .T. ) ;
#22042 = ORIENTED_EDGE ( 'NONE', *, *, #69213, .T. ) ;
#22043 = DIRECTION ( 'NONE',  ( 1.000000000000000000, 0.000000000000000000, 0.000000000000000000 ) ) ;
#22044 = DIRECTION ( 'NONE',  ( 0.7071067811865537900, 0.7071067811865412445, -1.896300252935124802E-30 ) ) ;
#22046 = EDGE_CURVE ( 'NONE', #11939, #66346, #49024, .T. ) ;
#22045 = DIRECTION ( 'NONE',  ( 0.000000000000000000, -0.7046037717859445770, 0.7096009616573392131 ) ) ;
#22047 = CARTESIAN_POINT ( 'NONE',  ( 11.75000000000000000, -5.000000000000000000, 26.25000000000000000 ) ) ;
#22048 = LINE ( 'NONE', #15707, #12199 ) ;
#22049 = EDGE_CURVE ( 'NONE', #9283, #22404, #5197, .T. ) ;
#22050 = VECTOR ( 'NONE', #40402, 1000.000000000000000 ) ;
#22051 = EDGE_LOOP ( 'NONE', ( #5684, #20126, #48253, #18103 ) ) ;
#22052 = AXIS2_PLACEMENT_3D ( 'NONE', #52229, #68141, #67791 ) ;
#22053 = DIRECTION ( 'NONE',  ( 0.8660254037844510311, 0.4999999999999785727, 1.836970198720951294E-16 ) ) ;
#22054 = EDGE_CURVE ( 'NONE', #13915, #14923, #41162, .T. ) ;
#22055 = VECTOR ( 'NONE', #47929, 1000.000000000000000 ) ;
#22056 = VECTOR ( 'NONE', #17243, 1000.000000000000000 ) ;
#22057 = AXIS2_PLACEMENT_3D ( 'NONE', #41656, #30705, #56859 ) ;
#22058 = ORIENTED_EDGE ( 'NONE', *, *, #60831, .F. ) ;
#22059 = CARTESIAN_POINT ( 'NONE',  ( 0.7669999999999959073, 4.898587196589385219E-16, 3.999999999999977351 ) ) ;
#22060 = DIRECTION ( 'NONE',  ( 0.000000000000000000, 0.000000000000000000, 1.000000000000000000 ) ) ;
#22061 = VERTEX_POINT ( 'NONE', #238 ) ;
#22062 = EDGE_CURVE ( 'NONE', #32555, #13545, #582, .T. ) ;
#22063 = FACE_OUTER_BOUND ( 'NONE', #29251, .T. ) ;
#22064 = DIRECTION ( 'NONE',  ( 0.000000000000000000, 0.000000000000000000, 1.000000000000000000 ) ) ;
#22065 = VECTOR ( 'NONE', #46592, 1000.000000000000000 ) ;
#22066 = VECTOR ( 'NONE', #53153, 1000.000000000000000 ) ;
#22067 = ORIENTED_EDGE ( 'NONE', *, *, #14208, .F. ) ;
#22068 = DIRECTION ( 'NONE',  ( -1.000000000000000000, 0.000000000000000000, 0.000000000000000000 ) ) ;
#22069 = CARTESIAN_POINT ( 'NONE',  ( -10.49297626211726175, 6.835476262117182955, 26.00000000000000711 ) ) ;
#22070 = EDGE_CURVE ( 'NONE', #26452, #9904, #37718, .T. ) ;
#22071 = EDGE_CURVE ( 'NONE', #43831, #46841, #15464, .T. ) ;
#22072 = AXIS2_PLACEMENT_3D ( 'NONE', #16349, #65487, #11046 ) ;
#22073 = CARTESIAN_POINT ( 'NONE',  ( -11.00000000000000000, -12.00000000000000000, -10.20500000000000007 ) ) ;
#22074 = DIRECTION ( 'NONE',  ( 0.000000000000000000, 1.000000000000000000, 0.000000000000000000 ) ) ;
#22075 = ORIENTED_EDGE ( 'NONE', *, *, #19172, .F. ) ;
#22077 = VERTEX_POINT ( 'NONE', #59278 ) ;
#22076 = CARTESIAN_POINT ( 'NONE',  ( 15.50000000000000000, -1.037157890325000054, -22.50000000000000000 ) ) ;
#22078 = ADVANCED_FACE ( 'NONE', ( #4845, #64249 ), #10147, .T. ) ;
#22079 = AXIS2_PLACEMENT_3D ( 'NONE', #68756, #13947, #35153 ) ;
#22080 = CARTESIAN_POINT ( 'NONE',  ( 37.90000000000000568, -21.00000000000000000, 13.86939075806900057 ) ) ;
#22081 = DIRECTION ( 'NONE',  ( 0.4999999999999827360, 0.000000000000000000, -0.8660254037844485886 ) ) ;
#22082 = DIRECTION ( 'NONE',  ( -0.000000000000000000, -0.000000000000000000, -1.000000000000000000 ) ) ;
#22083 = ORIENTED_EDGE ( 'NONE', *, *, #20329, .T. ) ;
#22084 = COLOUR_RGB ( '', 0.66274510, 0.83137255, 0.94901961) ;
#22085 = PLANE ( 'NONE',  #26607 ) ;
#22086 = CARTESIAN_POINT ( 'NONE',  ( 283.0000000000000568, -21.00000000000000000, 12.50000000000000000 ) ) ;
#22087 = ORIENTED_EDGE ( 'NONE', *, *, #40503, .F. ) ;
#22088 = ORIENTED_EDGE ( 'NONE', *, *, #33550, .T. ) ;
#22089 = ORIENTED_EDGE ( 'NONE', *, *, #48320, .F. ) ;
#22090 = EDGE_CURVE ( 'NONE', #28902, #9955, #15799, .T. ) ;
#22091 = DIRECTION ( 'NONE',  ( 0.000000000000000000, 0.000000000000000000, 1.000000000000000000 ) ) ;
#22092 = FACE_OUTER_BOUND ( 'NONE', #56566, .T. ) ;
#22093 = EDGE_CURVE ( 'NONE', #66591, #39463, #43355, .T. ) ;
#22094 = EDGE_LOOP ( 'NONE', ( #47148, #18380, #51574, #49565 ) ) ;
#22095 = ORIENTED_EDGE ( 'NONE', *, *, #7206, .T. ) ;
#22096 = VERTEX_POINT ( 'NONE', #43011 ) ;
#22097 = CARTESIAN_POINT ( 'NONE',  ( 11.00000000000000000, -15.97213595500069871, 14.50000000000000000 ) ) ;
#22098 = ORIENTED_EDGE ( 'NONE', *, *, #58524, .F. ) ;
#22099 = VECTOR ( 'NONE', #6659, 1000.000000000000000 ) ;
#22100 = VERTEX_POINT ( 'NONE', #59633 ) ;
#22101 = ORIENTED_EDGE ( 'NONE', *, *, #36219, .T. ) ;
#22102 = ORIENTED_EDGE ( 'NONE', *, *, #34772, .T. ) ;
#22103 = VECTOR ( 'NONE', #22832, 1000.000000000000000 ) ;
#22104 = CARTESIAN_POINT ( 'NONE',  ( 7.450000000000003730, -7.249999999999997335, -15.00000000000000000 ) ) ;
#22106 = ORIENTED_EDGE ( 'NONE', *, *, #42387, .F. ) ;
#22105 = DIRECTION ( 'NONE',  ( -0.7071067811865474617, -0.7071067811865474617, 0.000000000000000000 ) ) ;
#22107 = DIRECTION ( 'NONE',  ( 0.000000000000000000, 0.000000000000000000, -1.000000000000000000 ) ) ;
#22108 = CIRCLE ( 'NONE', #66153, 0.1749999999999998224 ) ;
#22109 = CIRCLE ( 'NONE', #6300, 3.499999999999999556 ) ;
#22110 = VECTOR ( 'NONE', #14177, 1000.000000000000000 ) ;
#22111 = DIRECTION ( 'NONE',  ( 1.000000000000000000, 0.000000000000000000, -0.000000000000000000 ) ) ;
#22112 = CARTESIAN_POINT ( 'NONE',  ( 283.0000000000000568, -38.10000000000000142, 8.400000000000000355 ) ) ;
#22113 = ORIENTED_EDGE ( 'NONE', *, *, #61452, .T. ) ;
#22114 = VECTOR ( 'NONE', #208, 1000.000000000000000 ) ;
#22115 = VECTOR ( 'NONE', #54007, 1000.000000000000000 ) ;
#22116 = CYLINDRICAL_SURFACE ( 'NONE', #14231, 1.621000000000000885 ) ;
#22117 = AXIS2_PLACEMENT_3D ( 'NONE', #44091, #34158, #6269 ) ;
#22118 = ORIENTED_EDGE ( 'NONE', *, *, #45013, .T. ) ;
#22119 = DIRECTION ( 'NONE',  ( -1.000000000000000000, 0.000000000000000000, -0.000000000000000000 ) ) ;
#22120 = EDGE_CURVE ( 'NONE', #31022, #33386, #22151, .T. ) ;
#22121 = VECTOR ( 'NONE', #65026, 1000.000000000000000 ) ;
#22122 = CARTESIAN_POINT ( 'NONE',  ( 1.090483450353338268, -11.34648345035345329, 455.0000000000000568 ) ) ;
#22123 = CARTESIAN_POINT ( 'NONE',  ( 7.250000000000005329, -8.249999999999998224, -8.500000000000000000 ) ) ;
#22124 = LINE ( 'NONE', #10119, #64116 ) ;
#22125 = VERTEX_POINT ( 'NONE', #16145 ) ;
#22127 = EDGE_CURVE ( 'NONE', #35485, #61156, #51355, .T. ) ;
#22126 = CARTESIAN_POINT ( 'NONE',  ( 25.90000000000000213, -21.00000000000001421, -13.86939075806900945 ) ) ;
#22128 = LINE ( 'NONE', #560, #38690 ) ;
#22129 = LINE ( 'NONE', #32045, #59622 ) ;
#22130 = EDGE_CURVE ( 'NONE', #37742, #39718, #67152, .T. ) ;
#22131 = ADVANCED_FACE ( 'NONE', ( #4731 ), #52115, .T. ) ;
#22132 = DIRECTION ( 'NONE',  ( 1.000000000000000000, 0.000000000000000000, 0.000000000000000000 ) ) ;
#22133 = EDGE_CURVE ( 'NONE', #44422, #40712, #26293, .T. ) ;
#22134 = FACE_OUTER_BOUND ( 'NONE', #43059, .T. ) ;
#22135 = EDGE_CURVE ( 'NONE', #46851, #29966, #24255, .T. ) ;
#22136 = CARTESIAN_POINT ( 'NONE',  ( -11.11351654964668789, 8.333516549646644123, 195.0000000000000284 ) ) ;
#22137 = DIRECTION ( 'NONE',  ( -1.000000000000000000, 0.000000000000000000, 0.000000000000000000 ) ) ;
#22138 = CARTESIAN_POINT ( 'NONE',  ( -4.188533722949335569, 4.727349090213398775, 455.0000000000000568 ) ) ;
#22139 = EDGE_CURVE ( 'NONE', #38571, #56028, #15804, .T. ) ;
#22140 = ORIENTED_EDGE ( 'NONE', *, *, #11103, .T. ) ;
#22141 = CARTESIAN_POINT ( 'NONE',  ( -7.250000000000000888, 7.250000000000001776, -17.50000000000000000 ) ) ;
#22142 = VECTOR ( 'NONE', #44357, 1000.000000000000000 ) ;
#22143 = LINE ( 'NONE', #39084, #11589 ) ;
#22144 = CARTESIAN_POINT ( 'NONE',  ( -9.722976262117294155, -6.832023737882757963, 54.00000000000000711 ) ) ;
#22145 = PLANE ( 'NONE',  #2530 ) ;
#22146 = ORIENTED_EDGE ( 'NONE', *, *, #61016, .F. ) ;
#22147 = CARTESIAN_POINT ( 'NONE',  ( -15.50000000000000000, -15.50000000000000000, -22.50000000000000000 ) ) ;
#22148 = FACE_OUTER_BOUND ( 'NONE', #4765, .T. ) ;
#22149 = CIRCLE ( 'NONE', #15391, 1.000000000000000000 ) ;
#22150 = DIRECTION ( 'NONE',  ( 1.000000000000000000, 0.000000000000000000, 0.000000000000000000 ) ) ;
#22151 = LINE ( 'NONE', #32063, #49095 ) ;
#22152 = AXIS2_PLACEMENT_3D ( 'NONE', #14667, #4073, #25640 ) ;
#22153 = CYLINDRICAL_SURFACE ( 'NONE', #26357, 0.2000000000000005107 ) ;
#22154 = CARTESIAN_POINT ( 'NONE',  ( 10.14575131106465378, -25.50000000000000355, 17.00000000000000000 ) ) ;
#22155 = ORIENTED_EDGE ( 'NONE', *, *, #18123, .F. ) ;
#22156 = VECTOR ( 'NONE', #53881, 1000.000000000000000 ) ;
#22157 = CIRCLE ( 'NONE', #68489, 0.1750000000000002387 ) ;
#22158 = VECTOR ( 'NONE', #5340, 1000.000000000000000 ) ;
#22159 = EDGE_LOOP ( 'NONE', ( #8755, #33402, #63586, #19712 ) ) ;
#22160 = DIRECTION ( 'NONE',  ( -0.000000000000000000, 3.673940397442059868E-16, -1.000000000000000000 ) ) ;
#22161 = DIRECTION ( 'NONE',  ( -1.794541526872559352E-16, -1.000000000000000000, 0.000000000000000000 ) ) ;
#22162 = ORIENTED_EDGE ( 'NONE', *, *, #64785, .F. ) ;
#22163 = VECTOR ( 'NONE', #5447, 1000.000000000000000 ) ;
#22164 = VECTOR ( 'NONE', #27647, 1000.000000000000114 ) ;
#22165 = AXIS2_PLACEMENT_3D ( 'NONE', #26526, #41380, #26884 ) ;
#22166 = DIRECTION ( 'NONE',  ( -0.000000000000000000, 1.000000000000000000, -0.000000000000000000 ) ) ;
#22167 = ORIENTED_EDGE ( 'NONE', *, *, #40222, .T. ) ;
#22168 = AXIS2_PLACEMENT_3D ( 'NONE', #58898, #30621, #20707 ) ;
#22169 = DIRECTION ( 'NONE',  ( 0.000000000000000000, 0.000000000000000000, -1.000000000000000000 ) ) ;
#22170 = ORIENTED_EDGE ( 'NONE', *, *, #50611, .T. ) ;
#22171 = ORIENTED_EDGE ( 'NONE', *, *, #44959, .T. ) ;
#22172 = DIRECTION ( 'NONE',  ( 1.000000000000000000, 0.000000000000000000, 0.000000000000000000 ) ) ;
#22173 = EDGE_LOOP ( 'NONE', ( #23536, #34837, #42400, #49013, #32554, #58611, #31131, #15153 ) ) ;
#22174 = FACE_OUTER_BOUND ( 'NONE', #42890, .T. ) ;
#22175 = DIRECTION ( 'NONE',  ( -0.000000000000000000, 0.000000000000000000, -1.000000000000000000 ) ) ;
#22177 = EDGE_CURVE ( 'NONE', #30033, #24504, #60333, .T. ) ;
#22176 = LINE ( 'NONE', #43739, #24579 ) ;
#22178 = AXIS2_PLACEMENT_3D ( 'NONE', #28781, #6869, #50359 ) ;
#22179 = ORIENTED_EDGE ( 'NONE', *, *, #36202, .T. ) ;
#22181 = ADVANCED_FACE ( 'NONE', ( #57414 ), #62712, .T. ) ;
#22180 = ORIENTED_EDGE ( 'NONE', *, *, #13986, .F. ) ;
#22182 = DIRECTION ( 'NONE',  ( -1.000000000000000000, 0.000000000000000000, 0.000000000000000000 ) ) ;
#22183 = CARTESIAN_POINT ( 'NONE',  ( -10.30047626211725742, 6.642976262117184838, 26.00000000000000711 ) ) ;
#22184 = ORIENTED_EDGE ( 'NONE', *, *, #59182, .F. ) ;
#22185 = ORIENTED_EDGE ( 'NONE', *, *, #19773, .T. ) ;
#22186 = EDGE_CURVE ( 'NONE', #62668, #48333, #57059, .T. ) ;
#22187 = EDGE_CURVE ( 'NONE', #63906, #30476, #8971, .T. ) ;
#22188 = VERTEX_POINT ( 'NONE', #68378 ) ;
#22189 = CARTESIAN_POINT ( 'NONE',  ( 8.900000000000002132, -18.00000000000000355, 21.00000000000000000 ) ) ;
#22191 = VERTEX_POINT ( 'NONE', #31612 ) ;
#22190 = PLANE ( 'NONE',  #58980 ) ;
#22192 = CARTESIAN_POINT ( 'NONE',  ( -7.250000000000001776, -7.249999999999998224, -9.500000000000001776 ) ) ;
#22193 = CARTESIAN_POINT ( 'NONE',  ( 7.000000000000000000, -31.30000000000000071, 8.400000000000000355 ) ) ;
#22194 = ORIENTED_EDGE ( 'NONE', *, *, #59905, .T. ) ;
#22195 = AXIS2_PLACEMENT_3D ( 'NONE', #48573, #28041, #17418 ) ;
#22196 = ORIENTED_EDGE ( 'NONE', *, *, #56272, .T. ) ;
#22197 = ORIENTED_EDGE ( 'NONE', *, *, #8127, .F. ) ;
#22198 = FACE_OUTER_BOUND ( 'NONE', #52808, .T. ) ;
#22199 = CARTESIAN_POINT ( 'NONE',  ( 7.281754163448140638, 8.000000000000001776, 5.000000000000000000 ) ) ;
#22200 = VECTOR ( 'NONE', #16286, 1000.000000000000000 ) ;
#22201 = CIRCLE ( 'NONE', #34590, 0.1749999999999980738 ) ;
#22202 = ORIENTED_EDGE ( 'NONE', *, *, #8341, .T. ) ;
#22203 = CIRCLE ( 'NONE', #767, 1.000000000000000000 ) ;
#22204 = AXIS2_PLACEMENT_3D ( 'NONE', #44127, #1686, #66037 ) ;
#22205 = ADVANCED_FACE ( 'NONE', ( #58492 ), #35849, .T. ) ;
#22206 = VECTOR ( 'NONE', #48111, 1000.000000000000000 ) ;
#22207 =( NAMED_UNIT ( * ) SI_UNIT ( $, .STERADIAN. ) SOLID_ANGLE_UNIT ( ) );
#22208 = CARTESIAN_POINT ( 'NONE',  ( 2.420780051175169145, 8.697938382363084031, 54.00000000000000711 ) ) ;
#22210 = ORIENTED_EDGE ( 'NONE', *, *, #51481, .T. ) ;
#22209 = DIRECTION ( 'NONE',  ( 1.836970198721029934E-16, 1.836970198721010706E-16, -1.000000000000000000 ) ) ;
#22211 = ORIENTED_EDGE ( 'NONE', *, *, #40588, .T. ) ;
#22212 = DIRECTION ( 'NONE',  ( 0.000000000000000000, 1.000000000000000000, 0.000000000000000000 ) ) ;
#22213 = CIRCLE ( 'NONE', #58368, 0.2000000000000005107 ) ;
#22214 = AXIS2_PLACEMENT_3D ( 'NONE', #44409, #45457, #17899 ) ;
#22215 = DIRECTION ( 'NONE',  ( 0.000000000000000000, 0.000000000000000000, -1.000000000000000000 ) ) ;
#22216 = FACE_OUTER_BOUND ( 'NONE', #22380, .T. ) ;
#22217 = CARTESIAN_POINT ( 'NONE',  ( -15.91242688423473517, -0.3152598339554900653, 21.29473909965994594 ) ) ;
#22218 = CARTESIAN_POINT ( 'NONE',  ( -7.250000000000000888, 7.250000000000001776, -19.00000000000000000 ) ) ;
#22220 = VERTEX_POINT ( 'NONE', #31273 ) ;
#22219 = EDGE_CURVE ( 'NONE', #7598, #67007, #53187, .T. ) ;
#22221 = LINE ( 'NONE', #54741, #16606 ) ;
#22222 = EDGE_CURVE ( 'NONE', #9656, #3514, #19582, .T. ) ;
#22223 = DIRECTION ( 'NONE',  ( -0.000000000000000000, -0.000000000000000000, -1.000000000000000000 ) ) ;
#22224 = LINE ( 'NONE', #43423, #17618 ) ;
#22226 = EDGE_LOOP ( 'NONE', ( #45518, #19433, #61473, #69757 ) ) ;
#22225 = LINE ( 'NONE', #49775, #54811 ) ;
#22227 = PRODUCT_DEFINITION_SHAPE ( 'NONE', 'NONE',  #69995 ) ;
#22228 = AXIS2_PLACEMENT_3D ( 'NONE', #59777, #27264, #17323 ) ;
#22229 = FACE_OUTER_BOUND ( 'NONE', #42832, .T. ) ;
#22230 = EDGE_CURVE ( 'NONE', #3052, #16796, #56060, .T. ) ;
#22231 = FACE_OUTER_BOUND ( 'NONE', #20537, .T. ) ;
#22232 = DIRECTION ( 'NONE',  ( 0.4999999999989410693, 0.000000000000000000, -0.8660254037850499964 ) ) ;
#22233 = LINE ( 'NONE', #27191, #22831 ) ;
#22234 = EDGE_LOOP ( 'NONE', ( #47409, #66785, #16644, #64833 ) ) ;
#22235 = FACE_OUTER_BOUND ( 'NONE', #48635, .T. ) ;
#22236 = LINE ( 'NONE', #49785, #60941 ) ;
#22237 = ORIENTED_EDGE ( 'NONE', *, *, #6047, .F. ) ;
#22238 = DIRECTION ( 'NONE',  ( 0.000000000000000000, 0.000000000000000000, 1.000000000000000000 ) ) ;
#22239 = LINE ( 'NONE', #65372, #9636 ) ;
#22240 = DIRECTION ( 'NONE',  ( 0.000000000000000000, 0.000000000000000000, -1.000000000000000000 ) ) ;
#22241 = LINE ( 'NONE', #65375, #52296 ) ;
#22242 = DIRECTION ( 'NONE',  ( 1.000000000000000000, 0.000000000000000000, 0.000000000000000000 ) ) ;
#22243 = FACE_OUTER_BOUND ( 'NONE', #32293, .T. ) ;
#22244 = ORIENTED_EDGE ( 'NONE', *, *, #37164, .T. ) ;
#22245 = CARTESIAN_POINT ( 'NONE',  ( 16.75000000000000000, -0.2038245569916320166, -23.22168783648699986 ) ) ;
#22246 = DIRECTION ( 'NONE',  ( 0.000000000000000000, 0.000000000000000000, 1.000000000000000000 ) ) ;
#22247 = VECTOR ( 'NONE', #65101, 1000.000000000000000 ) ;
#22248 = ORIENTED_EDGE ( 'NONE', *, *, #5858, .F. ) ;
#22249 = LINE ( 'NONE', #46016, #28007 ) ;
#22250 =( GEOMETRIC_REPRESENTATION_CONTEXT ( 3 ) GLOBAL_UNCERTAINTY_ASSIGNED_CONTEXT ( ( #27407 ) ) GLOBAL_UNIT_ASSIGNED_CONTEXT ( ( #64992, #21847, #22207 ) ) REPRESENTATION_CONTEXT ( 'NONE', 'WORKASPACE' ) );
#22251 = DIRECTION ( 'NONE',  ( -1.000000000000000000, 0.000000000000000000, 0.000000000000000000 ) ) ;
#22252 = CIRCLE ( 'NONE', #31306, 3.500000000000003109 ) ;
#22253 = CIRCLE ( 'NONE', #31307, 0.7112000000000124889 ) ;
#22254 = FACE_OUTER_BOUND ( 'NONE', #49563, .T. ) ;
#22255 = VERTEX_POINT ( 'NONE', #30899 ) ;
#22256 = ORIENTED_EDGE ( 'NONE', *, *, #41195, .F. ) ;
#22257 = CARTESIAN_POINT ( 'NONE',  ( 10.20488345035340494, 9.791916549646614953, 195.0000000000000284 ) ) ;
#22258 = ORIENTED_EDGE ( 'NONE', *, *, #69942, .T. ) ;
#22259 = VERTEX_POINT ( 'NONE', #69074 ) ;
#22260 = AXIS2_PLACEMENT_3D ( 'NONE', #33362, #23445, #65540 ) ;
#22261 = VECTOR ( 'NONE', #37338, 1000.000000000000000 ) ;
#22262 = CARTESIAN_POINT ( 'NONE',  ( 8.250000000000005329, 0.000000000000000000, -19.50000000000000000 ) ) ;
#22263 = CARTESIAN_POINT ( 'NONE',  ( 5.257023737882819070, -7.186223737882822427, 54.00000000000000711 ) ) ;
#22264 = FACE_OUTER_BOUND ( 'NONE', #10086, .T. ) ;
#22265 = AXIS2_PLACEMENT_3D ( 'NONE', #56178, #11976, #60422 ) ;
#22266 = ORIENTED_EDGE ( 'NONE', *, *, #68882, .T. ) ;
#22267 = ADVANCED_FACE ( 'NONE', ( #19938 ), #3328, .F. ) ;
#22268 = EDGE_CURVE ( 'NONE', #58579, #27218, #63953, .T. ) ;
#22269 = LINE ( 'NONE', #22604, #31217 ) ;
#22270 = ADVANCED_FACE ( 'NONE', ( #10037 ), #14632, .T. ) ;
#22271 = VECTOR ( 'NONE', #24643, 1000.000000000000000 ) ;
#22272 = VECTOR ( 'NONE', #37139, 1000.000000000000000 ) ;
#22274 = CARTESIAN_POINT ( 'NONE',  ( -7.250000000000001776, -7.249999999999998224, -11.00000000000000000 ) ) ;
#22273 = CARTESIAN_POINT ( 'NONE',  ( -2.406732575409589625, 8.697938382363036069, 54.00000000000000711 ) ) ;
#22275 = ORIENTED_EDGE ( 'NONE', *, *, #13369, .T. ) ;
#22276 = ORIENTED_EDGE ( 'NONE', *, *, #23913, .T. ) ;
#22278 = ORIENTED_EDGE ( 'NONE', *, *, #55539, .T. ) ;
#22277 = LINE ( 'NONE', #69677, #41005 ) ;
#22279 = ORIENTED_EDGE ( 'NONE', *, *, #9200, .F. ) ;
#22280 = EDGE_CURVE ( 'NONE', #1298, #26074, #20284, .T. ) ;
#22281 = AXIS2_PLACEMENT_3D ( 'NONE', #58642, #63948, #42369 ) ;
#22282 = FACE_BOUND ( 'NONE', #53238, .T. ) ;
#22283 = AXIS2_PLACEMENT_3D ( 'NONE', #56203, #34621, #7749 ) ;
#22284 = LINE ( 'NONE', #2081, #34801 ) ;
#22285 = ORIENTED_EDGE ( 'NONE', *, *, #50921, .F. ) ;
#22286 = ORIENTED_EDGE ( 'NONE', *, *, #3176, .T. ) ;
#22287 = DIRECTION ( 'NONE',  ( 0.000000000000000000, 1.000000000000000000, 0.000000000000000000 ) ) ;
#22288 = DIRECTION ( 'NONE',  ( 1.836970198721029934E-16, -1.836970198721036344E-16, 1.000000000000000000 ) ) ;
#22289 = VERTEX_POINT ( 'NONE', #38640 ) ;
#22290 = DIRECTION ( 'NONE',  ( -0.000000000000000000, -0.000000000000000000, -1.000000000000000000 ) ) ;
#22291 = CARTESIAN_POINT ( 'NONE',  ( 25.49999999999869971, -15.50000000000000000, -22.50000000000000000 ) ) ;
#22292 = CARTESIAN_POINT ( 'NONE',  ( 29.89999999999999858, 0.000000000000000000, 2.370429594502469981E-15 ) ) ;
#22293 = ORIENTED_EDGE ( 'NONE', *, *, #44266, .T. ) ;
#22294 = DIRECTION ( 'NONE',  ( -0.000000000000000000, -0.000000000000000000, -1.000000000000000000 ) ) ;
#22295 = DIRECTION ( 'NONE',  ( 0.8660254037844322683, -0.5000000000000111022, 6.723777587268230953E-17 ) ) ;
#22296 = VECTOR ( 'NONE', #32494, 1000.000000000000000 ) ;
#22298 = ORIENTED_EDGE ( 'NONE', *, *, #30666, .T. ) ;
#22297 = CARTESIAN_POINT ( 'NONE',  ( 9.955011587777235604, -2.765062094116182312, 455.0000000000000568 ) ) ;
#22300 = VERTEX_POINT ( 'NONE', #471 ) ;
#22299 = CARTESIAN_POINT ( 'NONE',  ( 4.456444791733522252E-16, 7.450000000000002842, -7.000000000000000000 ) ) ;
#22301 = LINE ( 'NONE', #27942, #47194 ) ;
#22302 = CARTESIAN_POINT ( 'NONE',  ( -15.50000000000000000, -0.1999999999999999556, 22.50000000000000000 ) ) ;
#22303 = FACE_OUTER_BOUND ( 'NONE', #35654, .T. ) ;
#22304 = DIRECTION ( 'NONE',  ( 0.000000000000000000, 0.000000000000000000, -1.000000000000000000 ) ) ;
#22305 = CARTESIAN_POINT ( 'NONE',  ( 30.00000000000000000, -16.28999999999999915, 14.50000000000000000 ) ) ;
#22306 = AXIS2_PLACEMENT_3D ( 'NONE', #40738, #45679, #62294 ) ;
#22307 = AXIS2_PLACEMENT_3D ( 'NONE', #52925, #58571, #4819 ) ;
#22308 = DIRECTION ( 'NONE',  ( -1.000000000000000000, -5.013651664672856055E-16, -1.841985738954423698E-31 ) ) ;
#22309 = ORIENTED_EDGE ( 'NONE', *, *, #24193, .T. ) ;
#22310 = FACE_OUTER_BOUND ( 'NONE', #42438, .T. ) ;
#22311 = EDGE_CURVE ( 'NONE', #47920, #19060, #16556, .T. ) ;
#22313 = ORIENTED_EDGE ( 'NONE', *, *, #22849, .F. ) ;
#22312 = DIRECTION ( 'NONE',  ( 1.000000000000000000, 0.000000000000000000, 0.000000000000000000 ) ) ;
#22314 = VECTOR ( 'NONE', #27628, 1000.000000000000000 ) ;
#22317 = VERTEX_POINT ( 'NONE', #22388 ) ;
#22316 = FACE_OUTER_BOUND ( 'NONE', #54025, .T. ) ;
#22315 = AXIS2_PLACEMENT_3D ( 'NONE', #15331, #30894, #57408 ) ;
#22318 = DIRECTION ( 'NONE',  ( -1.000000000000000000, 0.000000000000000000, 0.000000000000000000 ) ) ;
#22319 = EDGE_CURVE ( 'NONE', #8790, #57591, #43246, .T. ) ;
#22320 = EDGE_CURVE ( 'NONE', #28515, #27839, #36858, .T. ) ;
#22321 = CARTESIAN_POINT ( 'NONE',  ( 30.00000000000000000, -11.50000000000000000, -19.00000000000000000 ) ) ;
#22322 = VECTOR ( 'NONE', #62371, 1000.000000000000000 ) ;
#22323 = VECTOR ( 'NONE', #24332, 1000.000000000000000 ) ;
#22324 = EDGE_CURVE ( 'NONE', #23509, #51833, #11078, .T. ) ;
#22325 = ORIENTED_EDGE ( 'NONE', *, *, #1537, .T. ) ;
#22326 = LINE ( 'NONE', #65109, #54623 ) ;
#22327 = CARTESIAN_POINT ( 'NONE',  ( 2.369523737882815784, 8.821682069070730492, 54.00000000000000711 ) ) ;
#22328 = ORIENTED_EDGE ( 'NONE', *, *, #49695, .T. ) ;
#22329 = PRODUCT_RELATED_PRODUCT_CATEGORY ( 'part', '', ( #38037 ) ) ;
#22330 = DIRECTION ( 'NONE',  ( 0.000000000000000000, -0.9938079899998859545, 0.1111111111112941946 ) ) ;
#22331 = DIRECTION ( 'NONE',  ( -0.7071067811865475727, 0.000000000000000000, 0.7071067811865475727 ) ) ;
#22332 = CARTESIAN_POINT ( 'NONE',  ( 7.265214908726155052, 6.606374702650035680, 455.0000000000000568 ) ) ;
#22333 = EDGE_CURVE ( 'NONE', #61486, #36045, #49257, .T. ) ;
#22334 = DIRECTION ( 'NONE',  ( 0.000000000000000000, 0.000000000000000000, -1.000000000000000000 ) ) ;
#22335 = EDGE_CURVE ( 'NONE', #40341, #9194, #35715, .T. ) ;
#22336 = AXIS2_PLACEMENT_3D ( 'NONE', #38477, #65001, #43077 ) ;
#22337 = DIRECTION ( 'NONE',  ( 0.000000000000000000, 0.000000000000000000, 1.000000000000000000 ) ) ;
#22338 = VERTEX_POINT ( 'NONE', #833 ) ;
#22339 = LINE ( 'NONE', #27292, #67628 ) ;
#22340 = ORIENTED_EDGE ( 'NONE', *, *, #10641, .T. ) ;
#22341 = ORIENTED_EDGE ( 'NONE', *, *, #63499, .F. ) ;
#22342 = DIRECTION ( 'NONE',  ( 0.000000000000000000, -1.000000000000000000, 0.000000000000000000 ) ) ;
#22343 = CARTESIAN_POINT ( 'NONE',  ( 8.406483450353348985, 5.655420232009159776, 195.0000000000000284 ) ) ;
#22344 = DIRECTION ( 'NONE',  ( -1.920885163218982051E-15, -1.000000000000000000, 0.000000000000000000 ) ) ;
#22345 = DIRECTION ( 'NONE',  ( -0.000000000000000000, 3.673940397442059868E-16, -1.000000000000000000 ) ) ;
#22346 = ORIENTED_EDGE ( 'NONE', *, *, #10003, .F. ) ;
#22347 = ORIENTED_EDGE ( 'NONE', *, *, #53856, .F. ) ;
#22349 = EDGE_LOOP ( 'NONE', ( #16594, #60782, #16576, #5986 ) ) ;
#22348 = PLANE ( 'NONE',  #33998 ) ;
#22350 = ORIENTED_EDGE ( 'NONE', *, *, #53056, .F. ) ;
#22351 = FACE_OUTER_BOUND ( 'NONE', #25914, .T. ) ;
#22352 = CARTESIAN_POINT ( 'NONE',  ( -4.141586236041129077, -4.720772854004773755, 54.00000000000000711 ) ) ;
#22353 = FACE_OUTER_BOUND ( 'NONE', #28970, .T. ) ;
#22354 = AXIS2_PLACEMENT_3D ( 'NONE', #57783, #69444, #9711 ) ;
#22355 = FILL_AREA_STYLE_COLOUR ( '', #41274 ) ;
#22357 = CARTESIAN_POINT ( 'NONE',  ( -30.00000000000000000, -9.200000000000120082, 17.64999999999993108 ) ) ;
#22356 = CARTESIAN_POINT ( 'NONE',  ( -7.250000000000000888, 7.250000000000001776, -19.50000000000000000 ) ) ;
#22358 = ORIENTED_EDGE ( 'NONE', *, *, #38033, .F. ) ;
#22360 = ORIENTED_EDGE ( 'NONE', *, *, #16379, .T. ) ;
#22359 = LINE ( 'NONE', #37578, #21747 ) ;
#22361 = EDGE_LOOP ( 'NONE', ( #5770, #33603, #1967, #7621 ) ) ;
#22362 = ORIENTED_EDGE ( 'NONE', *, *, #59422, .T. ) ;
#22363 = CARTESIAN_POINT ( 'NONE',  ( 7.450000000000003730, -7.249999999999997335, -7.500000000000000000 ) ) ;
#22364 = DIRECTION ( 'NONE',  ( -1.836970198721029934E-16, 1.836970198721036590E-16, -1.000000000000000000 ) ) ;
#22365 = CIRCLE ( 'NONE', #57322, 0.4999999999945534124 ) ;
#22366 = CARTESIAN_POINT ( 'NONE',  ( 9.899999999999998579, -0.2000000000089119934, 8.909539772616881237E-12 ) ) ;
#22367 = LINE ( 'NONE', #17049, #38729 ) ;
#22368 = VERTEX_POINT ( 'NONE', #32645 ) ;
#22369 = ORIENTED_EDGE ( 'NONE', *, *, #57483, .T. ) ;
#22370 = VECTOR ( 'NONE', #21702, 1000.000000000000000 ) ;
#22371 = EDGE_CURVE ( 'NONE', #67986, #27724, #6469, .T. ) ;
#22372 = LINE ( 'NONE', #43918, #59118 ) ;
#22373 = LINE ( 'NONE', #31935, #52599 ) ;
#22374 = VERTEX_POINT ( 'NONE', #69789 ) ;
#22375 = ORIENTED_EDGE ( 'NONE', *, *, #56446, .F. ) ;
#22376 = DIRECTION ( 'NONE',  ( -0.8660254037844347108, 0.5000000000000069944, 2.509347957447884214E-16 ) ) ;
#22377 = ADVANCED_FACE ( 'NONE', ( #64481 ), #5445, .F. ) ;
#22378 =( REPRESENTATION_RELATIONSHIP ('NONE','NONE', #33057, #62481 ) REPRESENTATION_RELATIONSHIP_WITH_TRANSFORMATION ( #21482 )SHAPE_REPRESENTATION_RELATIONSHIP( ) );
#22379 = CARTESIAN_POINT ( 'NONE',  ( 275.2500000000001137, -0.2500000000000497935, 26.75000000000004263 ) ) ;
#22380 = EDGE_LOOP ( 'NONE', ( #12090, #44486, #24389, #38914 ) ) ;
#22381 = VECTOR ( 'NONE', #62025, 1000.000000000000000 ) ;
#22382 = DIRECTION ( 'NONE',  ( 1.836970198721029934E-16, -1.836970198721036344E-16, 1.000000000000000000 ) ) ;
#22383 = EDGE_CURVE ( 'NONE', #47820, #57771, #54221, .T. ) ;
#22385 = ORIENTED_EDGE ( 'NONE', *, *, #54891, .F. ) ;
#22384 = CARTESIAN_POINT ( 'NONE',  ( -10.03972626211722918, 8.916576262117214213, 54.00000000000000711 ) ) ;
#22386 = ORIENTED_EDGE ( 'NONE', *, *, #39087, .F. ) ;
#22387 = CARTESIAN_POINT ( 'NONE',  ( -10.30047626211724321, -3.664523737882710464, 26.00000000000000000 ) ) ;
#22388 = CARTESIAN_POINT ( 'NONE',  ( -11.99351654964671354, 7.813516549646603693, 455.0000000000000568 ) ) ;
#22389 = CARTESIAN_POINT ( 'NONE',  ( -8.598420958951683346, 1.991476262117183316, 54.00000000000000711 ) ) ;
#22390 = EDGE_CURVE ( 'NONE', #64346, #1690, #17071, .T. ) ;
#22391 = LINE ( 'NONE', #33337, #21051 ) ;
#22392 = DIRECTION ( 'NONE',  ( 0.000000000000000000, 0.000000000000000000, -1.000000000000000000 ) ) ;
#22393 = EDGE_LOOP ( 'NONE', ( #50015, #42939, #64686, #1461 ) ) ;
#22394 = PLANE ( 'NONE',  #62011 ) ;
#22396 = VERTEX_POINT ( 'NONE', #33335 ) ;
#22395 = CYLINDRICAL_SURFACE ( 'NONE', #67183, 24.99999999998789946 ) ;
#22397 = CARTESIAN_POINT ( 'NONE',  ( -10.49297626211726175, 3.650476262117184234, 26.00000000000000711 ) ) ;
#22398 = DIRECTION ( 'NONE',  ( 1.000000000000000000, 0.000000000000000000, 0.000000000000000000 ) ) ;
#22399 = EDGE_CURVE ( 'NONE', #53770, #18339, #48911, .T. ) ;
#22400 = VECTOR ( 'NONE', #33947, 1000.000000000000000 ) ;
#22401 = DIRECTION ( 'NONE',  ( 9.050731179009442381E-15, 1.000000000000000000, 3.673940397442060361E-16 ) ) ;
#22402 = CARTESIAN_POINT ( 'NONE',  ( 152.0064834503532722, -16.00648345035295250, 0.000000000000000000 ) ) ;
#22403 = CARTESIAN_POINT ( 'NONE',  ( 7.450000000000003730, -7.249999999999997335, -12.50000000000000000 ) ) ;
#22404 = VERTEX_POINT ( 'NONE', #59858 ) ;
#22405 = ORIENTED_EDGE ( 'NONE', *, *, #45368, .T. ) ;
#22406 = CARTESIAN_POINT ( 'NONE',  ( 7.500000000000000000, -25.60000000000000142, -16.00000000000000000 ) ) ;
#22407 = ADVANCED_FACE ( 'NONE', ( #16039 ), #60192, .F. ) ;
#22408 = DIRECTION ( 'NONE',  ( -1.836970198721029934E-16, 1.836970198721036590E-16, -1.000000000000000000 ) ) ;
#22409 = ADVANCED_FACE ( 'NONE', ( #1162 ), #54567, .F. ) ;
#22410 = VECTOR ( 'NONE', #68237, 1000.000000000000000 ) ;
#22411 = ORIENTED_EDGE ( 'NONE', *, *, #57919, .F. ) ;
#22412 = DIRECTION ( 'NONE',  ( 1.000000000000000000, -0.000000000000000000, -0.000000000000000000 ) ) ;
#22413 = LINE ( 'NONE', #21364, #3875 ) ;
#22414 = VERTEX_POINT ( 'NONE', #59163 ) ;
#22415 = VECTOR ( 'NONE', #44506, 1000.000000000000000 ) ;
#22416 = PLANE ( 'NONE',  #30173 ) ;
#22417 = CARTESIAN_POINT ( 'NONE',  ( 3.682023737882786918, -9.737023737882799068, 26.00000000000000000 ) ) ;
#22418 = EDGE_LOOP ( 'NONE', ( #52525, #23116, #36211, #24850, #7847, #23044, #47643, #13925 ) ) ;
#22419 = DIRECTION ( 'NONE',  ( 0.000000000000000000, 0.000000000000000000, -1.000000000000000000 ) ) ;
#22420 = EDGE_CURVE ( 'NONE', #65971, #41893, #31952, .T. ) ;
#22421 = FACE_OUTER_BOUND ( 'NONE', #25213, .T. ) ;
#22422 = FACE_OUTER_BOUND ( 'NONE', #32003, .T. ) ;
#22423 = DIRECTION ( 'NONE',  ( 1.000000000000000000, 0.000000000000000000, -0.000000000000000000 ) ) ;
#22424 = ORIENTED_EDGE ( 'NONE', *, *, #64835, .F. ) ;
#22426 = ORIENTED_EDGE ( 'NONE', *, *, #25510, .T. ) ;
#22425 = LINE ( 'NONE', #60232, #11407 ) ;
#22427 = AXIS2_PLACEMENT_3D ( 'NONE', #28378, #7844, #7148 ) ;
#22428 = FACE_OUTER_BOUND ( 'NONE', #18466, .T. ) ;
#22429 = CARTESIAN_POINT ( 'NONE',  ( -30.00000000000000000, -9.454754784057099570, -17.53999999999999915 ) ) ;
#22430 = CARTESIAN_POINT ( 'NONE',  ( 4.396432944014576627, 8.393516549646587777, 455.0000000000000568 ) ) ;
#22431 = VERTEX_POINT ( 'NONE', #10723 ) ;
#22432 = DIRECTION ( 'NONE',  ( 0.000000000000000000, 1.000000000000000000, 0.000000000000000000 ) ) ;
#22433 = DIRECTION ( 'NONE',  ( -1.000000000000000000, 0.000000000000000000, 0.000000000000000000 ) ) ;
#22434 = ORIENTED_EDGE ( 'NONE', *, *, #45448, .F. ) ;
#22435 = VERTEX_POINT ( 'NONE', #32296 ) ;
#22436 = EDGE_CURVE ( 'NONE', #11224, #49372, #26995, .T. ) ;
#22437 = VERTEX_POINT ( 'NONE', #67240 ) ;
#22438 = LINE ( 'NONE', #17818, #56973 ) ;
#22439 = CARTESIAN_POINT ( 'NONE',  ( 15.50000000000000000, 0.000000000000000000, -26.50000000000000000 ) ) ;
#22440 = EDGE_CURVE ( 'NONE', #34368, #51768, #40370, .T. ) ;
#22441 = CARTESIAN_POINT ( 'NONE',  ( 25.50000000000000355, -15.50000000000000000, 22.50000000000000000 ) ) ;
#22442 =( NAMED_UNIT ( * ) PLANE_ANGLE_UNIT ( ) SI_UNIT ( $, .RADIAN. ) );
#22443 = ORIENTED_EDGE ( 'NONE', *, *, #3839, .T. ) ;
#22444 = ORIENTED_EDGE ( 'NONE', *, *, #50032, .T. ) ;
#22445 = EDGE_LOOP ( 'NONE', ( #30700, #24340, #68558, #32602 ) ) ;
#22446 = EDGE_CURVE ( 'NONE', #69428, #28943, #46024, .T. ) ;
#22447 = DIRECTION ( 'NONE',  ( 1.000000000000000000, -1.047444401652939849E-14, 1.836970198721010706E-16 ) ) ;
#22448 = ORIENTED_EDGE ( 'NONE', *, *, #50456, .T. ) ;
#22449 = EDGE_CURVE ( 'NONE', #56239, #45920, #24459, .T. ) ;
#22450 = ORIENTED_EDGE ( 'NONE', *, *, #54969, .F. ) ;
#22451 = VERTEX_POINT ( 'NONE', #23055 ) ;
#22452 = VECTOR ( 'NONE', #26348, 1000.000000000000000 ) ;
#22453 = ORIENTED_EDGE ( 'NONE', *, *, #42707, .T. ) ;
#22454 = CYLINDRICAL_SURFACE ( 'NONE', #67773, 4.000000000000000000 ) ;
#22455 = UNCERTAINTY_MEASURE_WITH_UNIT (LENGTH_MEASURE( 1.000000000000000082E-05 ), #1482, 'distance_accuracy_value', 'NONE');
#22456 = EDGE_CURVE ( 'NONE', #32779, #10509, #45307, .T. ) ;
#22458 = ORIENTED_EDGE ( 'NONE', *, *, #63972, .F. ) ;
#22457 = CARTESIAN_POINT ( 'NONE',  ( 11.00000000000000000, -9.200000000000120082, 17.30000000000000071 ) ) ;
#22459 = AXIS2_PLACEMENT_3D ( 'NONE', #13705, #23272, #44827 ) ;
#22460 = FACE_OUTER_BOUND ( 'NONE', #45278, .T. ) ;
#22461 = LINE ( 'NONE', #49665, #5877 ) ;
#22462 = CARTESIAN_POINT ( 'NONE',  ( 146.5599459900709860, 9.000000000000001776, 276.7801873289890295 ) ) ;
#22463 = ADVANCED_FACE ( 'NONE', ( #66875 ), #12430, .F. ) ;
#22464 = ORIENTED_EDGE ( 'NONE', *, *, #8236, .F. ) ;
#22465 = EDGE_CURVE ( 'NONE', #44295, #13178, #61655, .T. ) ;
#22466 = AXIS2_PLACEMENT_3D ( 'NONE', #36021, #38048, #212 ) ;
#22467 = EDGE_CURVE ( 'NONE', #13174, #68300, #2189, .T. ) ;
#22468 = DIRECTION ( 'NONE',  ( -0.000000000000000000, 1.000000000000000000, -0.000000000000000000 ) ) ;
#22469 = EDGE_CURVE ( 'NONE', #25374, #58001, #28706, .T. ) ;
#22470 = EDGE_CURVE ( 'NONE', #26653, #5963, #2882, .T. ) ;
#22471 = CARTESIAN_POINT ( 'NONE',  ( -7.517976262117260333, 6.651770455163663165, 54.00000000000000711 ) ) ;
#22472 = AXIS2_PLACEMENT_3D ( 'NONE', #19096, #50451, #18972 ) ;
#22473 = VERTEX_POINT ( 'NONE', #1489 ) ;
#22474 = LINE ( 'NONE', #54300, #29194 ) ;
#22475 = ADVANCED_FACE ( 'NONE', ( #29060 ), #6789, .F. ) ;
#22477 = VECTOR ( 'NONE', #43245, 1000.000000000000000 ) ;
#22476 = VECTOR ( 'NONE', #32495, 1000.000000000000000 ) ;
#22478 = DIRECTION ( 'NONE',  ( 0.000000000000000000, 1.000000000000000000, 0.000000000000000000 ) ) ;
#22479 = CARTESIAN_POINT ( 'NONE',  ( -30.00000000000000000, -12.00000000000000000, -11.03137303340310282 ) ) ;
#22480 = VERTEX_POINT ( 'NONE', #44970 ) ;
#22481 = DIRECTION ( 'NONE',  ( -1.000000000000000000, 0.000000000000000000, 0.000000000000000000 ) ) ;
#22482 = CIRCLE ( 'NONE', #21367, 0.3500000000002722600 ) ;
#22483 = CARTESIAN_POINT ( 'NONE',  ( -30.00000000000000000, 0.000000000000000000, -27.00000000000000000 ) ) ;
#22484 = LINE ( 'NONE', #44025, #54034 ) ;
#22485 = CARTESIAN_POINT ( 'NONE',  ( 11.00000000000000000, -16.64230188589300141, 14.64519951917099583 ) ) ;
#22486 = CARTESIAN_POINT ( 'NONE',  ( 0.000000000000000000, 9.000000000000001776, 0.000000000000000000 ) ) ;
#22487 = DIRECTION ( 'NONE',  ( -1.000000000000000000, 3.491481338843133355E-15, 1.836970198721036344E-16 ) ) ;
#22488 = EDGE_CURVE ( 'NONE', #5502, #28088, #26702, .T. ) ;
#22489 = DIRECTION ( 'NONE',  ( -1.836970198721029934E-16, 1.836970198721036344E-16, -1.000000000000000000 ) ) ;
#22490 = DIRECTION ( 'NONE',  ( 1.000000000000000000, 0.000000000000000000, 0.000000000000000000 ) ) ;
#22491 = EDGE_CURVE ( 'NONE', #7579, #28918, #7827, .T. ) ;
#22492 = ORIENTED_EDGE ( 'NONE', *, *, #24942, .T. ) ;
#22493 = DIRECTION ( 'NONE',  ( -0.000000000000000000, -0.000000000000000000, 1.000000000000000000 ) ) ;
#22494 = CARTESIAN_POINT ( 'NONE',  ( 7.750000000000001776, 7.750000000000000000, -5.000000000000000000 ) ) ;
#22495 = DIRECTION ( 'NONE',  ( 0.000000000000000000, 1.000000000000000000, -0.000000000000000000 ) ) ;
#22496 = LINE ( 'NONE', #53983, #26277 ) ;
#22497 = EDGE_LOOP ( 'NONE', ( #56786, #31418, #50348, #45613 ) ) ;
#22498 = CARTESIAN_POINT ( 'NONE',  ( -7.750000000000001776, -7.348062532927999158, 5.000000000000000000 ) ) ;
#22499 = CARTESIAN_POINT ( 'NONE',  ( 4.201500623656003519, -7.272650909786602114, 195.0000000000000284 ) ) ;
#22500 = LINE ( 'NONE', #7249, #26650 ) ;
#22501 = AXIS2_PLACEMENT_3D ( 'NONE', #64420, #1099, #27287 ) ;
#22502 = CARTESIAN_POINT ( 'NONE',  ( -10.30047626211724321, -3.664523737882710464, 26.00000000000000000 ) ) ;
#22503 = DIRECTION ( 'NONE',  ( 0.000000000000000000, 0.000000000000000000, -1.000000000000000000 ) ) ;
#22504 = EDGE_LOOP ( 'NONE', ( #43828, #66240, #47307, #1990 ) ) ;
#22505 = AXIS2_PLACEMENT_3D ( 'NONE', #23712, #39959, #51996 ) ;
#22506 = EDGE_LOOP ( 'NONE', ( #14033, #47552, #52543, #22679 ) ) ;
#22507 = DIRECTION ( 'NONE',  ( 0.000000000000000000, 0.000000000000000000, 1.000000000000000000 ) ) ;
#22508 = FACE_OUTER_BOUND ( 'NONE', #38659, .T. ) ;
#22509 = EDGE_LOOP ( 'NONE', ( #17872, #19911, #55853, #66538 ) ) ;
#22510 = AXIS2_PLACEMENT_3D ( 'NONE', #35766, #25171, #3247 ) ;
#22511 = DIRECTION ( 'NONE',  ( 0.000000000000000000, 0.000000000000000000, 1.000000000000000000 ) ) ;
#22512 = ORIENTED_EDGE ( 'NONE', *, *, #17265, .T. ) ;
#22513 = CIRCLE ( 'NONE', #30437, 0.5999999999999998668 ) ;
#22514 = DIRECTION ( 'NONE',  ( 1.000000000000000000, 1.671920889371702657E-15, 0.000000000000000000 ) ) ;
#22515 = EDGE_LOOP ( 'NONE', ( #65305, #7699, #67205, #23741 ) ) ;
#22516 = ORIENTED_EDGE ( 'NONE', *, *, #42974, .T. ) ;
#22517 = DIRECTION ( 'NONE',  ( -0.000000000000000000, -0.000000000000000000, -1.000000000000000000 ) ) ;
#22518 = VERTEX_POINT ( 'NONE', #39325 ) ;
#22519 = CARTESIAN_POINT ( 'NONE',  ( -29.50000000000000355, -12.00000000000000000, 11.03137303340310282 ) ) ;
#22520 = CIRCLE ( 'NONE', #65474, 1.399999999999999245 ) ;
#22521 = EDGE_CURVE ( 'NONE', #30867, #36429, #18431, .T. ) ;
#22522 = DIRECTION ( 'NONE',  ( 1.000000000000000000, -1.088659024508174415E-14, 1.836970198721009966E-16 ) ) ;
#22523 = DIRECTION ( 'NONE',  ( 7.457533623526253657E-15, 1.000000000000000000, 0.000000000000000000 ) ) ;
#22524 = ORIENTED_EDGE ( 'NONE', *, *, #25167, .T. ) ;
#22525 = VERTEX_POINT ( 'NONE', #34706 ) ;
#22526 = EDGE_CURVE ( 'NONE', #14272, #40017, #56630, .T. ) ;
#22527 = DIRECTION ( 'NONE',  ( -1.000000000000000000, 0.000000000000000000, 0.000000000000000000 ) ) ;
#22529 = CARTESIAN_POINT ( 'NONE',  ( -30.00000000000000000, -8.959999999999999076, -12.95475478405700009 ) ) ;
#22528 = AXIS2_PLACEMENT_3D ( 'NONE', #1243, #60630, #49676 ) ;
#22530 = ORIENTED_EDGE ( 'NONE', *, *, #41299, .F. ) ;
#22531 = EDGE_CURVE ( 'NONE', #41506, #57189, #8179, .T. ) ;
#22532 = ORIENTED_EDGE ( 'NONE', *, *, #26635, .F. ) ;
#22533 = ORIENTED_EDGE ( 'NONE', *, *, #21066, .T. ) ;
#22534 = EDGE_CURVE ( 'NONE', #30734, #47809, #13489, .T. ) ;
#22535 = DIRECTION ( 'NONE',  ( 0.7071067811865500152, 0.7071067811865451302, -4.429638872090642462E-31 ) ) ;
#22537 = ORIENTED_EDGE ( 'NONE', *, *, #23998, .T. ) ;
#22536 = DIRECTION ( 'NONE',  ( 0.000000000000000000, 0.000000000000000000, 1.000000000000000000 ) ) ;
#22538 = CARTESIAN_POINT ( 'NONE',  ( 8.711985858128693749, -2.420780051175170478, 26.00000000000000711 ) ) ;
#22539 = LINE ( 'NONE', #33486, #32825 ) ;
#22540 = VECTOR ( 'NONE', #52730, 1000.000000000000000 ) ;
#22541 = ORIENTED_EDGE ( 'NONE', *, *, #63414, .F. ) ;
#22542 = ORIENTED_EDGE ( 'NONE', *, *, #3536, .F. ) ;
#22543 = EDGE_CURVE ( 'NONE', #3117, #51826, #50975, .T. ) ;
#22544 = LINE ( 'NONE', #33491, #63144 ) ;
#22545 = CARTESIAN_POINT ( 'NONE',  ( -0.9414762621173239365, -9.404523737882849233, 54.00000000000000711 ) ) ;
#22546 = VERTEX_POINT ( 'NONE', #66197 ) ;
#22547 = CIRCLE ( 'NONE', #28191, 1.224999999999998757 ) ;
#22548 = DIRECTION ( 'NONE',  ( 0.000000000000000000, -1.000000000000000000, 0.000000000000000000 ) ) ;
#22549 = DIRECTION ( 'NONE',  ( 1.000000000000000000, 0.000000000000000000, 0.000000000000000000 ) ) ;
#22551 = ORIENTED_EDGE ( 'NONE', *, *, #50121, .F. ) ;
#22550 = CARTESIAN_POINT ( 'NONE',  ( 38.90000000000000568, 20.60000000000000142, -13.86939075806900057 ) ) ;
#22552 = ORIENTED_EDGE ( 'NONE', *, *, #9055, .T. ) ;
#22553 = PLANE ( 'NONE',  #29834 ) ;
#22554 = VECTOR ( 'NONE', #60806, 1000.000000000000000 ) ;
#22555 = FACE_OUTER_BOUND ( 'NONE', #49061, .T. ) ;
#22556 = CARTESIAN_POINT ( 'NONE',  ( 7.000000000000000000, -25.56180396883900130, -14.25872597390799967 ) ) ;
#22557 = CARTESIAN_POINT ( 'NONE',  ( 30.00000000000000000, -16.64230188589299786, -14.64519951917100116 ) ) ;
#22558 = VECTOR ( 'NONE', #44917, 1000.000000000000000 ) ;
#22559 = LINE ( 'NONE', #54052, #18351 ) ;
#22560 = VERTEX_POINT ( 'NONE', #35049 ) ;
#22561 = FACE_OUTER_BOUND ( 'NONE', #54880, .T. ) ;
#22562 = FACE_OUTER_BOUND ( 'NONE', #60705, .T. ) ;
#22563 = EDGE_CURVE ( 'NONE', #37419, #59900, #17761, .T. ) ;
#22564 = DIRECTION ( 'NONE',  ( 0.000000000000000000, 0.000000000000000000, -1.000000000000000000 ) ) ;
#22565 = VECTOR ( 'NONE', #26585, 1000.000000000000000 ) ;
#22566 = LINE ( 'NONE', #45150, #11884 ) ;
#22567 = ADVANCED_FACE ( 'NONE', ( #12363 ), #9086, .T. ) ;
#22568 = CARTESIAN_POINT ( 'NONE',  ( 1.634292677759874746, 8.227189898828697778, 54.00000000000000711 ) ) ;
#22569 = EDGE_CURVE ( 'NONE', #27390, #26801, #18029, .T. ) ;
#22570 = CYLINDRICAL_SURFACE ( 'NONE', #18301, 0.1999999999999996503 ) ;
#22571 = VECTOR ( 'NONE', #30814, 1000.000000000000000 ) ;
#22572 = DIRECTION ( 'NONE',  ( 0.000000000000000000, 0.000000000000000000, 1.000000000000000000 ) ) ;
#22573 = EDGE_LOOP ( 'NONE', ( #61536, #12927, #6706, #63031, #63621 ) ) ;
#22574 = DIRECTION ( 'NONE',  ( 0.000000000000000000, 0.000000000000000000, -1.000000000000000000 ) ) ;
#22575 = CYLINDRICAL_SURFACE ( 'NONE', #12370, 3.999999999999993339 ) ;
#22576 = ORIENTED_EDGE ( 'NONE', *, *, #9587, .F. ) ;
#22577 = LINE ( 'NONE', #32835, #65031 ) ;
#22578 = PLANE ( 'NONE',  #22204 ) ;
#22579 = DIRECTION ( 'NONE',  ( 1.836970198721029934E-16, 1.836970198721010706E-16, -1.000000000000000000 ) ) ;
#22580 = FACE_OUTER_BOUND ( 'NONE', #68220, .T. ) ;
#22581 = CYLINDRICAL_SURFACE ( 'NONE', #12434, 0.6000000000000005329 ) ;
#22582 = CARTESIAN_POINT ( 'NONE',  ( 275.2500000000000000, -0.2500000000000000000, 26.75000000000000000 ) ) ;
#22583 = ORIENTED_EDGE ( 'NONE', *, *, #2579, .F. ) ;
#22584 = VECTOR ( 'NONE', #42267, 1000.000000000000000 ) ;
#22585 = CARTESIAN_POINT ( 'NONE',  ( -6.350872789121327244, 6.822336235477381550, 54.00000000000000711 ) ) ;
#22586 = ORIENTED_EDGE ( 'NONE', *, *, #47629, .F. ) ;
#22587 = DIRECTION ( 'NONE',  ( -1.000000000000000000, 0.000000000000000000, 0.000000000000000000 ) ) ;
#22588 = DIRECTION ( 'NONE',  ( -1.000000000000000000, 0.000000000000000000, 0.000000000000000000 ) ) ;
#22589 = CARTESIAN_POINT ( 'NONE',  ( -11.99351654964671354, 4.173516549646604901, 455.0000000000000568 ) ) ;
#22590 = ORIENTED_EDGE ( 'NONE', *, *, #42701, .T. ) ;
#22591 = ORIENTED_EDGE ( 'NONE', *, *, #62083, .F. ) ;
#22592 = CARTESIAN_POINT ( 'NONE',  ( 151.5599459900709860, 9.000000000000001776, 278.4149360882130395 ) ) ;
#22593 = VECTOR ( 'NONE', #68421, 1000.000000000000000 ) ;
#22594 = VERTEX_POINT ( 'NONE', #66131 ) ;
#22595 = VECTOR ( 'NONE', #44841, 1000.000000000000000 ) ;
#22596 = ORIENTED_EDGE ( 'NONE', *, *, #45597, .F. ) ;
#22597 = EDGE_CURVE ( 'NONE', #66031, #36357, #33946, .T. ) ;
#22598 = DIRECTION ( 'NONE',  ( 0.4999999999989410693, 0.000000000000000000, 0.8660254037850499964 ) ) ;
#22599 = LINE ( 'NONE', #61096, #38074 ) ;
#22601 = PLANE ( 'NONE',  #23062 ) ;
#22600 = VECTOR ( 'NONE', #16494, 1000.000000000000000 ) ;
#22602 = ORIENTED_EDGE ( 'NONE', *, *, #17247, .F. ) ;
#22603 = AXIS2_PLACEMENT_3D ( 'NONE', #51518, #34881, #51156 ) ;
#22604 = CARTESIAN_POINT ( 'NONE',  ( 2.420780051175148273, -8.711985858128677762, 54.00000000000000711 ) ) ;
#22606 = CARTESIAN_POINT ( 'NONE',  ( 283.0000000000000568, -38.10000000000000142, 8.400000000000000355 ) ) ;
#22605 = CARTESIAN_POINT ( 'NONE',  ( 10.62249899919920004, -25.00000000000000000, 17.50000000000000000 ) ) ;
#22607 = VERTEX_POINT ( 'NONE', #50217 ) ;
#22609 = ORIENTED_EDGE ( 'NONE', *, *, #42532, .F. ) ;
#22608 = CARTESIAN_POINT ( 'NONE',  ( -28.00000000000000000, -16.64230188589299786, -14.64519951917100116 ) ) ;
#22610 = EDGE_CURVE ( 'NONE', #11813, #66424, #55870, .T. ) ;
#22611 = ORIENTED_EDGE ( 'NONE', *, *, #33177, .F. ) ;
#22612 = ADVANCED_FACE ( 'NONE', ( #14746 ), #57870, .F. ) ;
#22613 = AXIS2_PLACEMENT_3D ( 'NONE', #12632, #33183, #11602 ) ;
#22614 = ADVANCED_FACE ( 'NONE', ( #7074 ), #28641, .F. ) ;
#22615 = EDGE_CURVE ( 'NONE', #30686, #10280, #39262, .T. ) ;
#22617 = CIRCLE ( 'NONE', #50804, 0.5999999999999998668 ) ;
#22616 = DIRECTION ( 'NONE',  ( 0.000000000000000000, 0.000000000000000000, 1.000000000000000000 ) ) ;
#22618 = AXIS2_PLACEMENT_3D ( 'NONE', #37547, #48503, #53821 ) ;
#22619 = CARTESIAN_POINT ( 'NONE',  ( 22.90000000000000213, -0.2000000000089119934, 8.909539772616881237E-12 ) ) ;
#22620 = ADVANCED_FACE ( 'NONE', ( #23684 ), #66816, .F. ) ;
#22621 = VERTEX_POINT ( 'NONE', #7423 ) ;
#22622 = ORIENTED_EDGE ( 'NONE', *, *, #68959, .T. ) ;
#22623 = VECTOR ( 'NONE', #46112, 1000.000000000000000 ) ;
#22624 = DIRECTION ( 'NONE',  ( 0.000000000000000000, 3.673940397442059868E-16, -1.000000000000000000 ) ) ;
#22625 = LINE ( 'NONE', #17303, #40198 ) ;
#22626 = ORIENTED_EDGE ( 'NONE', *, *, #64540, .F. ) ;
#22627 = CARTESIAN_POINT ( 'NONE',  ( -9.722976262117294155, -6.832023737882757963, 54.00000000000000711 ) ) ;
#22628 = CARTESIAN_POINT ( 'NONE',  ( 49.00000000000000000, -0.1999999999911430404, -8.864436962241481021E-12 ) ) ;
#22629 = CARTESIAN_POINT ( 'NONE',  ( 7.250000000000005329, 7.250000000000000888, -8.500000000000000000 ) ) ;
#22630 = ORIENTED_EDGE ( 'NONE', *, *, #62587, .T. ) ;
#22631 = DIRECTION ( 'NONE',  ( 1.000000000000000000, -0.000000000000000000, 0.000000000000000000 ) ) ;
#22632 = CARTESIAN_POINT ( 'NONE',  ( 9.737023737882816832, -3.682023737882817116, 26.00000000000000711 ) ) ;
#22634 = ORIENTED_EDGE ( 'NONE', *, *, #8576, .T. ) ;
#22633 = DIRECTION ( 'NONE',  ( 0.000000000000000000, 1.000000000000000000, 0.000000000000000000 ) ) ;
#22636 = VERTEX_POINT ( 'NONE', #56226 ) ;
#22635 = CARTESIAN_POINT ( 'NONE',  ( 283.0000000000000568, -42.50000000000000000, 7.500000000000000000 ) ) ;
#22637 = CARTESIAN_POINT ( 'NONE',  ( -8.697938382363135545, 8.079219948824830411, 54.00000000000000711 ) ) ;
#22638 = CYLINDRICAL_SURFACE ( 'NONE', #22790, 0.3499999999999996447 ) ;
#22639 = CARTESIAN_POINT ( 'NONE',  ( 7.357023737882802727, 5.538810540049955655, 54.00000000000000711 ) ) ;
#22640 = CYLINDRICAL_SURFACE ( 'NONE', #31272, 0.5000000000004236611 ) ;
#22641 = DIRECTION ( 'NONE',  ( 0.000000000000000000, 0.000000000000000000, -1.000000000000000000 ) ) ;
#22642 = VECTOR ( 'NONE', #42813, 1000.000000000000000 ) ;
#22643 = DIRECTION ( 'NONE',  ( 0.000000000000000000, 0.000000000000000000, 1.000000000000000000 ) ) ;
#22644 = ORIENTED_EDGE ( 'NONE', *, *, #48130, .F. ) ;
#22645 = CARTESIAN_POINT ( 'NONE',  ( 30.00000000000000000, -10.85999999999999943, 9.000000000000001776 ) ) ;
#22646 = VECTOR ( 'NONE', #28613, 1000.000000000000000 ) ;
#22648 = ORIENTED_EDGE ( 'NONE', *, *, #5216, .F. ) ;
#22647 =( NAMED_UNIT ( * ) SI_UNIT ( $, .STERADIAN. ) SOLID_ANGLE_UNIT ( ) );
#22650 = ORIENTED_EDGE ( 'NONE', *, *, #6572, .F. ) ;
#22649 = FACE_OUTER_BOUND ( 'NONE', #14519, .T. ) ;
#22651 = VECTOR ( 'NONE', #19267, 1000.000000000000000 ) ;
#22652 = DIRECTION ( 'NONE',  ( 0.000000000000000000, 0.000000000000000000, -1.000000000000000000 ) ) ;
#22653 = EDGE_CURVE ( 'NONE', #35273, #48543, #52708, .T. ) ;
#22654 = CARTESIAN_POINT ( 'NONE',  ( 7.450000000000003730, -7.249999999999997335, -19.50000000000000000 ) ) ;
#22655 = AXIS2_PLACEMENT_3D ( 'NONE', #58921, #26057, #15087 ) ;
#22656 = EDGE_CURVE ( 'NONE', #55322, #34914, #22203, .T. ) ;
#22657 = ORIENTED_EDGE ( 'NONE', *, *, #56336, .T. ) ;
#22658 = CARTESIAN_POINT ( 'NONE',  ( 7.616533956692213003, -8.406483450353491094, 455.0000000000000568 ) ) ;
#22659 = DIRECTION ( 'NONE',  ( -1.000000000000000000, 0.000000000000000000, 0.000000000000000000 ) ) ;
#22661 = EDGE_LOOP ( 'NONE', ( #44011, #28078, #46162, #67333 ) ) ;
#22660 = EDGE_CURVE ( 'NONE', #34914, #2392, #28996, .T. ) ;
#22662 = AXIS2_PLACEMENT_3D ( 'NONE', #69195, #64250, #42318 ) ;
#22663 = DIRECTION ( 'NONE',  ( 1.000000000000000000, -0.000000000000000000, 0.000000000000000000 ) ) ;
#22664 = FACE_OUTER_BOUND ( 'NONE', #58395, .T. ) ;
#22665 = CARTESIAN_POINT ( 'NONE',  ( 9.737023737882815055, -2.544523737882816050, 26.00000000000000711 ) ) ;
#22666 = CARTESIAN_POINT ( 'NONE',  ( 3.606483450353380249, -4.622483450353491286, 455.0000000000000568 ) ) ;
#22667 = ORIENTED_EDGE ( 'NONE', *, *, #69729, .F. ) ;
#22668 = FACE_OUTER_BOUND ( 'NONE', #45376, .T. ) ;
#22669 = ORIENTED_EDGE ( 'NONE', *, *, #57556, .T. ) ;
#22670 = VERTEX_POINT ( 'NONE', #61506 ) ;
#22671 = DIRECTION ( 'NONE',  ( 0.000000000000000000, 0.000000000000000000, 1.000000000000000000 ) ) ;
#22672 = CIRCLE ( 'NONE', #19236, 0.1750000000000002387 ) ;
#22673 = CARTESIAN_POINT ( 'NONE',  ( -4.242044687070659847, -8.465062094116134972, 455.0000000000000568 ) ) ;
#22674 = CARTESIAN_POINT ( 'NONE',  ( 7.250000000000005329, -7.449999999999998401, -10.50000000000000000 ) ) ;
#22675 = CARTESIAN_POINT ( 'NONE',  ( 7.250000000000005329, -7.449999999999998401, -14.50000000000000000 ) ) ;
#22676 = ORIENTED_EDGE ( 'NONE', *, *, #25989, .F. ) ;
#22677 = VERTEX_POINT ( 'NONE', #22997 ) ;
#22679 = ORIENTED_EDGE ( 'NONE', *, *, #35885, .T. ) ;
#22678 = DIRECTION ( 'NONE',  ( -1.836970198721029934E-16, -1.836970198721010706E-16, 1.000000000000000000 ) ) ;
#22680 = ORIENTED_EDGE ( 'NONE', *, *, #33886, .F. ) ;
#22681 = PLANE ( 'NONE',  #23586 ) ;
#22682 = DIRECTION ( 'NONE',  ( 1.000000000000000000, -0.000000000000000000, -0.000000000000000000 ) ) ;
#22683 = VECTOR ( 'NONE', #10883, 1000.000000000000000 ) ;
#22684 = DIRECTION ( 'NONE',  ( 0.000000000000000000, 0.000000000000000000, -1.000000000000000000 ) ) ;
#22685 = CARTESIAN_POINT ( 'NONE',  ( 106.4257688009193998, 0.000000000000000000, 285.9830310981789125 ) ) ;
#22687 = CARTESIAN_POINT ( 'NONE',  ( 10.50702373788281641, 9.781776262117171328, 54.00000000000000711 ) ) ;
#22686 = LINE ( 'NONE', #12064, #52417 ) ;
#22688 = ORIENTED_EDGE ( 'NONE', *, *, #21739, .T. ) ;
#22690 = EDGE_LOOP ( 'NONE', ( #40668, #34411, #17617, #63479 ) ) ;
#22689 = LINE ( 'NONE', #27649, #51057 ) ;
#22691 = ORIENTED_EDGE ( 'NONE', *, *, #23913, .F. ) ;
#22692 = ORIENTED_EDGE ( 'NONE', *, *, #54510, .F. ) ;
#22693 = LINE ( 'NONE', #38617, #8464 ) ;
#22694 = ADVANCED_FACE ( 'NONE', ( #7770 ), #68132, .F. ) ;
#22695 = LINE ( 'NONE', #39971, #47946 ) ;
#22696 = CIRCLE ( 'NONE', #35088, 1.224999999999998757 ) ;
#22697 = ADVANCED_FACE ( 'NONE', ( #14401 ), #35957, .F. ) ;
#22698 = CARTESIAN_POINT ( 'NONE',  ( 33.89999999999999858, 0.000000000000000000, 0.000000000000000000 ) ) ;
#22699 = VECTOR ( 'NONE', #33581, 1000.000000000000000 ) ;
#22700 = ADVANCED_FACE ( 'NONE', ( #3780 ), #25354, .F. ) ;
#22701 = CARTESIAN_POINT ( 'NONE',  ( 4.740315990920129785, -4.201500623656146516, 455.0000000000000568 ) ) ;
#22702 = EDGE_LOOP ( 'NONE', ( #55266, #38754, #50459, #17416 ) ) ;
#22703 = EDGE_CURVE ( 'NONE', #1953, #1721, #58587, .T. ) ;
#22704 = ORIENTED_EDGE ( 'NONE', *, *, #47130, .F. ) ;
#22705 = DIRECTION ( 'NONE',  ( 1.000000000000000000, -0.000000000000000000, 0.000000000000000000 ) ) ;
#22706 = DIRECTION ( 'NONE',  ( -0.000000000000000000, -0.000000000000000000, -1.000000000000000000 ) ) ;
#22707 = VERTEX_POINT ( 'NONE', #9805 ) ;
#22708 = VECTOR ( 'NONE', #29097, 1000.000000000000000 ) ;
#22709 = VECTOR ( 'NONE', #46237, 1000.000000000000000 ) ;
#22710 = ORIENTED_EDGE ( 'NONE', *, *, #67549, .F. ) ;
#22711 = PLANE ( 'NONE',  #38467 ) ;
#22712 = CARTESIAN_POINT ( 'NONE',  ( 19.90000000000000213, 13.66939075806899240, -20.79999999999999361 ) ) ;
#22714 = VERTEX_POINT ( 'NONE', #4839 ) ;
#22713 = EDGE_CURVE ( 'NONE', #8058, #31208, #43660, .T. ) ;
#22715 = DIRECTION ( 'NONE',  ( 0.000000000000000000, 0.000000000000000000, -1.000000000000000000 ) ) ;
#22717 = ORIENTED_EDGE ( 'NONE', *, *, #35755, .T. ) ;
#22716 = CARTESIAN_POINT ( 'NONE',  ( -11.75000000000000000, -5.200000000000001066, 11.75000000000000000 ) ) ;
#22718 = ORIENTED_EDGE ( 'NONE', *, *, #35241, .T. ) ;
#22720 = CARTESIAN_POINT ( 'NONE',  ( 7.408280051175172076, -6.789561617636949542, 54.00000000000000711 ) ) ;
#22719 = CIRCLE ( 'NONE', #3495, 3.499999999999999556 ) ;
#22721 = CARTESIAN_POINT ( 'NONE',  ( 15.00000000000000000, -42.50000000000000000, -26.50000000000000000 ) ) ;
#22722 = CARTESIAN_POINT ( 'NONE',  ( 41.09999999999999432, 13.66939075806899950, -20.80000000000000426 ) ) ;
#22723 = CARTESIAN_POINT ( 'NONE',  ( 3.677663764522614454, -6.364920264886869461, 26.00000000000000711 ) ) ;
#22724 = CARTESIAN_POINT ( 'NONE',  ( 283.0000000000000568, -42.50000000000000000, 15.10000000000000142 ) ) ;
#22725 = VERTEX_POINT ( 'NONE', #26403 ) ;
#22726 = LINE ( 'NONE', #6124, #55212 ) ;
#22728 = ORIENTED_EDGE ( 'NONE', *, *, #9017, .T. ) ;
#22727 = CARTESIAN_POINT ( 'NONE',  ( -11.99351654964679526, -7.826483450353362237, 455.0000000000000568 ) ) ;
#22729 = CARTESIAN_POINT ( 'NONE',  ( 10.74648345035337904, -1.690483450353491124, 455.0000000000000568 ) ) ;
#22730 = CARTESIAN_POINT ( 'NONE',  ( 41.09999999999999432, -0.2000000000000000111, 0.000000000000000000 ) ) ;
#22731 = AXIS2_PLACEMENT_3D ( 'NONE', #53598, #17838, #38039 ) ;
#22732 = CARTESIAN_POINT ( 'NONE',  ( 7.250000000000005329, -7.249999999999998224, -8.500000000000000000 ) ) ;
#22733 = LINE ( 'NONE', #40015, #35161 ) ;
#22734 = CARTESIAN_POINT ( 'NONE',  ( -3.710438382363119736, 7.394232575409525943, 54.00000000000000711 ) ) ;
#22735 = ORIENTED_EDGE ( 'NONE', *, *, #51271, .T. ) ;
#22737 = ORIENTED_EDGE ( 'NONE', *, *, #8882, .F. ) ;
#22736 = EDGE_CURVE ( 'NONE', #32917, #17706, #16614, .T. ) ;
#22738 = CARTESIAN_POINT ( 'NONE',  ( -10.08346604330788132, -2.706483450353354581, 455.0000000000000568 ) ) ;
#22739 = VECTOR ( 'NONE', #5780, 1000.000000000000000 ) ;
#22740 = CARTESIAN_POINT ( 'NONE',  ( 2.765062094116107705, 9.942044687070449527, 455.0000000000000568 ) ) ;
#22741 = VECTOR ( 'NONE', #34701, 999.9999999999998863 ) ;
#22742 = ORIENTED_EDGE ( 'NONE', *, *, #14636, .T. ) ;
#22743 = CARTESIAN_POINT ( 'NONE',  ( 78.77321854994620765, 47.95351654967443977, 39.00000000000000000 ) ) ;
#22744 = ORIENTED_EDGE ( 'NONE', *, *, #55725, .T. ) ;
#22745 = ORIENTED_EDGE ( 'NONE', *, *, #41744, .F. ) ;
#22746 = DIRECTION ( 'NONE',  ( -1.000000000000000000, 0.000000000000000000, 0.000000000000000000 ) ) ;
#22747 = CARTESIAN_POINT ( 'NONE',  ( 3.430747519065335815, 7.839518282750141509, 455.0000000000000568 ) ) ;
#22749 = ORIENTED_EDGE ( 'NONE', *, *, #48254, .F. ) ;
#22748 = EDGE_CURVE ( 'NONE', #32481, #38364, #31263, .T. ) ;
#22750 = LINE ( 'NONE', #50659, #11872 ) ;
#22751 = DIRECTION ( 'NONE',  ( -0.000000000000000000, -0.7071067811865474617, 0.7071067811865474617 ) ) ;
#22752 = VECTOR ( 'NONE', #59470, 1000.000000000000000 ) ;
#22753 = CIRCLE ( 'NONE', #30684, 2.000000000000001776 ) ;
#22754 = SURFACE_SIDE_STYLE ('',( #55287 ) ) ;
#22755 = EDGE_CURVE ( 'NONE', #8602, #2847, #69878, .T. ) ;
#22756 = CARTESIAN_POINT ( 'NONE',  ( 11.08848345035334404, -10.20488345035352928, 455.0000000000000568 ) ) ;
#22757 = ORIENTED_EDGE ( 'NONE', *, *, #33950, .F. ) ;
#22759 = VERTEX_POINT ( 'NONE', #47969 ) ;
#22758 = PLANE ( 'NONE',  #18155 ) ;
#22760 = AXIS2_PLACEMENT_3D ( 'NONE', #33290, #43199, #54864 ) ;
#22761 = DIRECTION ( 'NONE',  ( 4.336808689942043768E-15, 1.000000000000000000, 0.000000000000000000 ) ) ;
#22762 = DIRECTION ( 'NONE',  ( 1.836970198721029934E-16, 1.836970198721010706E-16, -1.000000000000000000 ) ) ;
#22763 = FACE_OUTER_BOUND ( 'NONE', #67659, .T. ) ;
#22764 = VERTEX_POINT ( 'NONE', #26065 ) ;
#22765 = AXIS2_PLACEMENT_3D ( 'NONE', #25177, #19858, #40386 ) ;
#22766 = CARTESIAN_POINT ( 'NONE',  ( 276.8775010008008053, -21.00000000000000000, 17.50000000000000000 ) ) ;
#22767 = DIRECTION ( 'NONE',  ( -0.000000000000000000, -0.000000000000000000, 1.000000000000000000 ) ) ;
#22768 = EDGE_LOOP ( 'NONE', ( #39570, #53522, #52750, #11997 ) ) ;
#22769 = VERTEX_POINT ( 'NONE', #15791 ) ;
#22770 = VERTEX_POINT ( 'NONE', #58928 ) ;
#22771 = CARTESIAN_POINT ( 'NONE',  ( -11.11351654964670743, 2.893516549646604208, 455.0000000000000568 ) ) ;
#22772 = PLANE ( 'NONE',  #67056 ) ;
#22774 = ADVANCED_FACE ( 'NONE', ( #16490 ), #59626, .F. ) ;
#22773 = DIRECTION ( 'NONE',  ( 0.000000000000000000, 1.000000000000000000, 0.000000000000000000 ) ) ;
#22775 = CARTESIAN_POINT ( 'NONE',  ( 0.000000000000000000, 0.000000000000000000, 0.000000000000000000 ) ) ;
#22776 = AXIS2_PLACEMENT_3D ( 'NONE', #9682, #68373, #58485 ) ;
#22777 = ADVANCED_FACE ( 'NONE', ( #32744 ), #69187, .T. ) ;
#22778 = ORIENTED_EDGE ( 'NONE', *, *, #49525, .F. ) ;
#22779 = ORIENTED_EDGE ( 'NONE', *, *, #56994, .T. ) ;
#22780 = EDGE_CURVE ( 'NONE', #66616, #41194, #69536, .T. ) ;
#22781 = ORIENTED_EDGE ( 'NONE', *, *, #59779, .T. ) ;
#22782 = CARTESIAN_POINT ( 'NONE',  ( 0.000000000000000000, -7.449999999999998401, -8.500000000000000000 ) ) ;
#22783 = ORIENTED_EDGE ( 'NONE', *, *, #69352, .F. ) ;
#22784 = EDGE_CURVE ( 'NONE', #50247, #14428, #32413, .T. ) ;
#22785 = EDGE_LOOP ( 'NONE', ( #14958, #46418, #33895, #41151 ) ) ;
#22786 = ORIENTED_EDGE ( 'NONE', *, *, #62841, .T. ) ;
#22787 = ORIENTED_EDGE ( 'NONE', *, *, #5361, .F. ) ;
#22788 = DIRECTION ( 'NONE',  ( -1.000000000000000000, 0.000000000000000000, 0.000000000000000000 ) ) ;
#22789 = EDGE_CURVE ( 'NONE', #28744, #65501, #42308, .T. ) ;
#22790 = AXIS2_PLACEMENT_3D ( 'NONE', #66107, #7399, #17676 ) ;
#22792 = ORIENTED_EDGE ( 'NONE', *, *, #69155, .F. ) ;
#22791 = CARTESIAN_POINT ( 'NONE',  ( 11.90000000000000036, 0.000000000000000000, 4.309871990004491277E-16 ) ) ;
#22793 = EDGE_CURVE ( 'NONE', #61464, #2063, #42661, .T. ) ;
#22794 = PLANE ( 'NONE',  #69568 ) ;
#22795 = PRODUCT_DEFINITION_SHAPE ( 'NONE', 'NONE',  #69981 ) ;
#22796 = CIRCLE ( 'NONE', #66786, 0.2000000000005226763 ) ;
#22797 = LINE ( 'NONE', #5508, #18260 ) ;
#22798 = CARTESIAN_POINT ( 'NONE',  ( 10.31452373788280141, 6.835476262117187396, 26.00000000000000711 ) ) ;
#22799 = ORIENTED_EDGE ( 'NONE', *, *, #19650, .F. ) ;
#22800 = FACE_OUTER_BOUND ( 'NONE', #66533, .T. ) ;
#22801 = AXIS2_PLACEMENT_3D ( 'NONE', #19624, #67018, #57110 ) ;
#22802 = VECTOR ( 'NONE', #45436, 1000.000000000000000 ) ;
#22803 = CARTESIAN_POINT ( 'NONE',  ( 4.149127210878726935, -6.836383711242993044, 26.00000000000000000 ) ) ;
#22804 = LINE ( 'NONE', #50366, #32718 ) ;
#22805 = ORIENTED_EDGE ( 'NONE', *, *, #18582, .T. ) ;
#22806 = CONICAL_SURFACE ( 'NONE', #23911, 2.458500000000000796, 1.047019301333029784 ) ;
#22807 = PLANE ( 'NONE',  #26960 ) ;
#22808 = CARTESIAN_POINT ( 'NONE',  ( 41.09999999999999432, -0.2000000000000000111, 0.000000000000000000 ) ) ;
#22809 = CYLINDRICAL_SURFACE ( 'NONE', #25532, 0.5000000000009302559 ) ;
#22810 = EDGE_CURVE ( 'NONE', #1208, #8765, #5189, .T. ) ;
#22811 = EDGE_LOOP ( 'NONE', ( #16816, #18318, #42054, #35245 ) ) ;
#22812 = DIRECTION ( 'NONE',  ( 0.000000000000000000, 0.000000000000000000, -1.000000000000000000 ) ) ;
#22813 = VECTOR ( 'NONE', #67259, 1000.000000000000000 ) ;
#22814 = CARTESIAN_POINT ( 'NONE',  ( 46.39999999999999858, 21.00000000000000000, 0.2500000000000000000 ) ) ;
#22815 = DIRECTION ( 'NONE',  ( 0.000000000000000000, 0.000000000000000000, -1.000000000000000000 ) ) ;
#22816 = ADVANCED_FACE ( 'NONE', ( #47271 ), #63885, .F. ) ;
#22817 = CARTESIAN_POINT ( 'NONE',  ( 289.5000000000000000, 0.000000000000000000, 50.00000000000000000 ) ) ;
#22818 = FACE_OUTER_BOUND ( 'NONE', #18793, .T. ) ;
#22819 = LINE ( 'NONE', #60650, #40713 ) ;
#22820 = FACE_OUTER_BOUND ( 'NONE', #45566, .T. ) ;
#22821 = EDGE_CURVE ( 'NONE', #2624, #69031, #20395, .T. ) ;
#22822 = CARTESIAN_POINT ( 'NONE',  ( -9.897976262117257562, 3.667976262117184749, 54.00000000000000711 ) ) ;
#22823 = ORIENTED_EDGE ( 'NONE', *, *, #36402, .F. ) ;
#22824 = DIRECTION ( 'NONE',  ( 1.000000000000000000, 0.000000000000000000, 0.000000000000000000 ) ) ;
#22825 = CARTESIAN_POINT ( 'NONE',  ( 41.09999999999999432, -21.00000000000000000, -13.86939075806900057 ) ) ;
#22826 = CARTESIAN_POINT ( 'NONE',  ( 10.05377373788278739, -8.930623737882845248, 26.00000000000000000 ) ) ;
#22827 = CARTESIAN_POINT ( 'NONE',  ( 25.57999999999999829, 0.000000000000000000, 0.000000000000000000 ) ) ;
#22828 = ORIENTED_EDGE ( 'NONE', *, *, #14152, .F. ) ;
#22829 = CARTESIAN_POINT ( 'NONE',  ( 40.90000000000000568, -0.2000000000000000111, 0.000000000000000000 ) ) ;
#22830 = CARTESIAN_POINT ( 'NONE',  ( -7.447976262117260049, 9.880476262117177555, 54.00000000000000711 ) ) ;
#22831 = VECTOR ( 'NONE', #12275, 1000.000000000000000 ) ;
#22832 = DIRECTION ( 'NONE',  ( 0.000000000000000000, 1.000000000000000000, 3.673940397442059868E-16 ) ) ;
#22833 = DIRECTION ( 'NONE',  ( 0.000000000000000000, 1.000000000000000000, 0.000000000000000000 ) ) ;
#22834 = ADVANCED_FACE ( 'NONE', ( #16136 ), #53982, .F. ) ;
#22835 = DIRECTION ( 'NONE',  ( 0.000000000000000000, -0.7071067811865474617, 0.7071067811865474617 ) ) ;
#22836 = VECTOR ( 'NONE', #1000, 1000.000000000000000 ) ;
#22837 = EDGE_LOOP ( 'NONE', ( #36031, #46616, #5230, #7977 ) ) ;
#22838 = CARTESIAN_POINT ( 'NONE',  ( 25.57999999999999829, 0.000000000000000000, 0.000000000000000000 ) ) ;
#22839 = DIRECTION ( 'NONE',  ( 1.000000000000000000, -0.000000000000000000, -0.000000000000000000 ) ) ;
#22841 = ORIENTED_EDGE ( 'NONE', *, *, #41518, .F. ) ;
#22840 = ADVANCED_FACE ( 'NONE', ( #63542, #15098 ), #31380, .F. ) ;
#22842 = VECTOR ( 'NONE', #50940, 1000.000000000000000 ) ;
#22843 = EDGE_CURVE ( 'NONE', #44680, #62302, #18210, .T. ) ;
#22844 = CARTESIAN_POINT ( 'NONE',  ( -25.50000000000000355, -15.50000000000000000, -25.99999999999985079 ) ) ;
#22845 = EDGE_CURVE ( 'NONE', #23822, #11704, #27445, .T. ) ;
#22846 = ORIENTED_EDGE ( 'NONE', *, *, #32259, .T. ) ;
#22848 = EDGE_CURVE ( 'NONE', #50228, #43197, #49323, .T. ) ;
#22847 = AXIS2_PLACEMENT_3D ( 'NONE', #9738, #30595, #52162 ) ;
#22849 = EDGE_CURVE ( 'NONE', #69381, #22338, #59509, .T. ) ;
#22850 = CARTESIAN_POINT ( 'NONE',  ( 3.664523737882778853, -10.50702373788281285, 54.00000000000000711 ) ) ;
#22851 = ORIENTED_EDGE ( 'NONE', *, *, #52928, .F. ) ;
#22852 = VERTEX_POINT ( 'NONE', #12889 ) ;
#22853 = CARTESIAN_POINT ( 'NONE',  ( -9.689726262117321909, -9.703773737882720241, 26.00000000000000000 ) ) ;
#22854 = LINE ( 'NONE', #12228, #51211 ) ;
#22855 = EDGE_CURVE ( 'NONE', #49549, #45382, #49016, .T. ) ;
#22856 = FACE_OUTER_BOUND ( 'NONE', #31496, .T. ) ;
#22857 = FACE_OUTER_BOUND ( 'NONE', #36974, .T. ) ;
#22858 = VECTOR ( 'NONE', #15734, 1000.000000000000000 ) ;
#22859 = ADVANCED_FACE ( 'NONE', ( #49701 ), #12205, .F. ) ;
#22860 = VERTEX_POINT ( 'NONE', #22826 ) ;
#22861 = ORIENTED_EDGE ( 'NONE', *, *, #16410, .T. ) ;
#22862 = CARTESIAN_POINT ( 'NONE',  ( 11.19368345035336709, -12.00648345035349251, 455.0000000000000568 ) ) ;
#22863 = ADVANCED_FACE ( 'NONE', ( #61333 ), #44375, .T. ) ;
#22864 = VECTOR ( 'NONE', #40901, 1000.000000000000000 ) ;
#22865 = DIRECTION ( 'NONE',  ( 7.665540703601096574E-15, 1.000000000000000000, -0.000000000000000000 ) ) ;
#22866 = VERTEX_POINT ( 'NONE', #60660 ) ;
#22867 = VERTEX_POINT ( 'NONE', #54325 ) ;
#22868 = VERTEX_POINT ( 'NONE', #39426 ) ;
#22869 = CARTESIAN_POINT ( 'NONE',  ( 181.4833316329832940, 9.000000000000001776, 320.8239988703753056 ) ) ;
#22870 = CARTESIAN_POINT ( 'NONE',  ( 7.250000000000004441, 7.450000000000001954, -23.00000000000000000 ) ) ;
#22871 = EDGE_CURVE ( 'NONE', #47459, #38948, #62879, .T. ) ;
#22873 = ORIENTED_EDGE ( 'NONE', *, *, #66897, .T. ) ;
#22872 = FACE_OUTER_BOUND ( 'NONE', #65726, .T. ) ;
#22874 = EDGE_CURVE ( 'NONE', #3520, #9024, #574, .T. ) ;
#22875 = PLANE ( 'NONE',  #37930 ) ;
#22876 = DIRECTION ( 'NONE',  ( -1.000000000000000000, 0.000000000000000000, 0.000000000000000000 ) ) ;
#22877 = ORIENTED_EDGE ( 'NONE', *, *, #44270, .F. ) ;
#22878 = ORIENTED_EDGE ( 'NONE', *, *, #56035, .T. ) ;
#22879 = ORIENTED_EDGE ( 'NONE', *, *, #44053, .F. ) ;
#22880 = CIRCLE ( 'NONE', #1426, 0.3499999999999996447 ) ;
#22881 = PLANE ( 'NONE',  #64270 ) ;
#22882 = LINE ( 'NONE', #44099, #59526 ) ;
#22883 = AXIS2_PLACEMENT_3D ( 'NONE', #25882, #68667, #51428 ) ;
#22884 = DIRECTION ( 'NONE',  ( 1.000000000000000000, 0.000000000000000000, -0.000000000000000000 ) ) ;
#22885 = DIRECTION ( 'NONE',  ( 0.000000000000000000, 1.000000000000000000, 0.000000000000000000 ) ) ;
#22886 = CARTESIAN_POINT ( 'NONE',  ( 6.619341603356827974, 7.252248008019368974, 195.0000000000000284 ) ) ;
#22888 = ORIENTED_EDGE ( 'NONE', *, *, #55202, .F. ) ;
#22887 =( LENGTH_UNIT ( ) NAMED_UNIT ( * ) SI_UNIT ( .MILLI., .METRE. ) );
#22889 = VERTEX_POINT ( 'NONE', #43710 ) ;
#22890 = CIRCLE ( 'NONE', #45441, 0.9999999999999991118 ) ;
#22891 = FACE_OUTER_BOUND ( 'NONE', #53043, .T. ) ;
#22892 = CARTESIAN_POINT ( 'NONE',  ( 40.90000000000000568, -0.2000000000000000111, 0.000000000000000000 ) ) ;
#22893 = CARTESIAN_POINT ( 'NONE',  ( -11.00000000000000000, -11.50000000000000000, 11.00000000000000000 ) ) ;
#22894 = LINE ( 'NONE', #6631, #9145 ) ;
#22895 = EDGE_CURVE ( 'NONE', #51826, #45978, #7221, .T. ) ;
#22896 = DIRECTION ( 'NONE',  ( 0.000000000000000000, 0.000000000000000000, -1.000000000000000000 ) ) ;
#22897 = VERTEX_POINT ( 'NONE', #16834 ) ;
#22898 = FACE_OUTER_BOUND ( 'NONE', #68039, .T. ) ;
#22899 = CARTESIAN_POINT ( 'NONE',  ( 55.00000000000000000, 16.96999999999999886, 21.00000000000000000 ) ) ;
#22900 = EDGE_CURVE ( 'NONE', #62860, #54169, #6905, .T. ) ;
#22901 = LINE ( 'NONE', #11928, #20938 ) ;
#22902 = CIRCLE ( 'NONE', #56810, 0.6000000000000006439 ) ;
#22903 = LINE ( 'NONE', #22568, #28116 ) ;
#22904 = LINE ( 'NONE', #55100, #33016 ) ;
#22905 = EDGE_CURVE ( 'NONE', #48285, #43972, #6224, .T. ) ;
#22906 = AXIS2_PLACEMENT_3D ( 'NONE', #35589, #8737, #51875 ) ;
#22907 = CARTESIAN_POINT ( 'NONE',  ( 15.50000000000000000, -2.500000000000000000, 21.05662432702600029 ) ) ;
#22908 = STYLED_ITEM ( 'NONE', ( #35243 ), #65828 ) ;
#22909 = ORIENTED_EDGE ( 'NONE', *, *, #28192, .F. ) ;
#22910 = FACE_OUTER_BOUND ( 'NONE', #62851, .T. ) ;
#22911 = EDGE_CURVE ( 'NONE', #42804, #34394, #60990, .T. ) ;
#22912 = CARTESIAN_POINT ( 'NONE',  ( -29.25000000000000000, -5.000000000000000000, -26.25000000000000000 ) ) ;
#22913 = ORIENTED_EDGE ( 'NONE', *, *, #6861, .T. ) ;
#22914 = DIRECTION ( 'NONE',  ( 0.000000000000000000, -1.000000000000000000, 0.000000000000000000 ) ) ;
#22915 = FACE_BOUND ( 'NONE', #59748, .T. ) ;
#22916 = DIRECTION ( 'NONE',  ( -1.000000000000000000, 0.000000000000000000, 0.000000000000000000 ) ) ;
#22918 = CIRCLE ( 'NONE', #4863, 5.000000000000000000 ) ;
#22917 = CARTESIAN_POINT ( 'NONE',  ( -7.250000000000001776, -7.249999999999998224, -23.50000000000000000 ) ) ;
#22919 = EDGE_CURVE ( 'NONE', #62636, #43565, #55697, .T. ) ;
#22920 = LINE ( 'NONE', #27535, #36179 ) ;
#22921 = DIRECTION ( 'NONE',  ( -1.000000000000000000, 0.000000000000000000, 0.000000000000000000 ) ) ;
#22922 = AXIS2_PLACEMENT_3D ( 'NONE', #42800, #64383, #65754 ) ;
#22923 = VERTEX_POINT ( 'NONE', #44724 ) ;
#22924 = FACE_OUTER_BOUND ( 'NONE', #10782, .T. ) ;
#22925 = EDGE_LOOP ( 'NONE', ( #65437, #63480, #68683, #2575 ) ) ;
#22926 = DIRECTION ( 'NONE',  ( 0.7071067811865348052, -0.7071067811865602293, -3.278703137324831017E-30 ) ) ;
#22927 = VECTOR ( 'NONE', #62745, 1000.000000000000114 ) ;
#22928 = ADVANCED_FACE ( 'NONE', ( #66317 ), #17870, .F. ) ;
#22929 = DIRECTION ( 'NONE',  ( -0.000000000000000000, -0.000000000000000000, -1.000000000000000000 ) ) ;
#22930 = ORIENTED_EDGE ( 'NONE', *, *, #19313, .T. ) ;
#22931 = EDGE_LOOP ( 'NONE', ( #44928, #35972 ) ) ;
#22932 = VECTOR ( 'NONE', #60522, 1000.000000000000000 ) ;
#22933 = CARTESIAN_POINT ( 'NONE',  ( 283.0000000000000568, -42.00000000000000000, -7.000000000000000000 ) ) ;
#22934 = ORIENTED_EDGE ( 'NONE', *, *, #18116, .T. ) ;
#22935 = ORIENTED_EDGE ( 'NONE', *, *, #69227, .T. ) ;
#22936 = CARTESIAN_POINT ( 'NONE',  ( 11.00000000000000000, -8.959999999999999076, -12.95475478405700009 ) ) ;
#22937 = CARTESIAN_POINT ( 'NONE',  ( 75.42576880091934299, 0.000000000000000000, 327.4830310981788557 ) ) ;
#22938 = DIRECTION ( 'NONE',  ( -0.000000000000000000, -0.000000000000000000, -1.000000000000000000 ) ) ;
#22939 = VERTEX_POINT ( 'NONE', #1958 ) ;
#22940 = VECTOR ( 'NONE', #6348, 1000.000000000000000 ) ;
#22941 = LINE ( 'NONE', #39205, #69616 ) ;
#22943 = FACE_OUTER_BOUND ( 'NONE', #4166, .T. ) ;
#22942 = CARTESIAN_POINT ( 'NONE',  ( 283.0000000000000568, -25.93000000000544958, -9.412893218815410634 ) ) ;
#22944 = ORIENTED_EDGE ( 'NONE', *, *, #14021, .T. ) ;
#22946 = VERTEX_POINT ( 'NONE', #50733 ) ;
#22945 = CARTESIAN_POINT ( 'NONE',  ( 36.90000000000000568, 0.000000000000000000, 2.458500000000000796 ) ) ;
#22947 = ORIENTED_EDGE ( 'NONE', *, *, #63724, .T. ) ;
#22948 = DIRECTION ( 'NONE',  ( 1.000000000000000000, 0.000000000000000000, 0.000000000000000000 ) ) ;
#22949 = DIRECTION ( 'NONE',  ( -0.7671651518153074223, -0.6414496315691484707, -2.587583378555112027E-16 ) ) ;
#22950 = EDGE_CURVE ( 'NONE', #57065, #18463, #61689, .T. ) ;
#22951 = EDGE_CURVE ( 'NONE', #12647, #26351, #23868, .T. ) ;
#22952 = CARTESIAN_POINT ( 'NONE',  ( 9.703773737882812611, 10.03972626211715813, 26.00000000000000711 ) ) ;
#22953 = AXIS2_PLACEMENT_3D ( 'NONE', #7968, #45104, #50069 ) ;
#22954 = EDGE_LOOP ( 'NONE', ( #51362, #31090, #35915, #66013 ) ) ;
#22955 = ORIENTED_EDGE ( 'NONE', *, *, #65636, .F. ) ;
#22956 = VECTOR ( 'NONE', #53549, 1000.000000000000000 ) ;
#22958 = CYLINDRICAL_SURFACE ( 'NONE', #14336, 1.929199999999998028 ) ;
#22957 = AXIS2_PLACEMENT_3D ( 'NONE', #12213, #60997, #6586 ) ;
#22959 = CIRCLE ( 'NONE', #12798, 2.458500000000000796 ) ;
#22960 = CARTESIAN_POINT ( 'NONE',  ( -8.250000000000000000, 7.250000000000001776, -13.00000000000000178 ) ) ;
#22961 = ORIENTED_EDGE ( 'NONE', *, *, #9025, .F. ) ;
#22962 = DIRECTION ( 'NONE',  ( -0.000000000000000000, 1.000000000000000000, -0.000000000000000000 ) ) ;
#22963 = DIRECTION ( 'NONE',  ( 1.000000000000000000, -3.491481338843133750E-15, -1.836970198721036590E-16 ) ) ;
#22964 = VECTOR ( 'NONE', #59337, 1000.000000000000000 ) ;
#22965 = AXIS2_PLACEMENT_3D ( 'NONE', #1335, #22896, #66020 ) ;
#22966 = PLANE ( 'NONE',  #55401 ) ;
#22967 = ORIENTED_EDGE ( 'NONE', *, *, #14484, .F. ) ;
#22968 = DIRECTION ( 'NONE',  ( 0.000000000000000000, -0.8650311892618017806, 0.5017180897718488408 ) ) ;
#22969 = CARTESIAN_POINT ( 'NONE',  ( -4.947141984184534991, -7.357023737882802727, 26.00000000000000711 ) ) ;
#22970 = VERTEX_POINT ( 'NONE', #34815 ) ;
#22972 = ORIENTED_EDGE ( 'NONE', *, *, #59187, .T. ) ;
#22971 = DIRECTION ( 'NONE',  ( -0.000000000000000000, 1.000000000000000000, -0.000000000000000000 ) ) ;
#22973 = DIRECTION ( 'NONE',  ( 0.6414496315691494699, -0.7671651518153064231, 0.000000000000000000 ) ) ;
#22974 = DIRECTION ( 'NONE',  ( 0.000000000000000000, -3.673940397442059868E-16, 1.000000000000000000 ) ) ;
#22975 = CIRCLE ( 'NONE', #56834, 0.2000000000005261458 ) ;
#22976 = DIRECTION ( 'NONE',  ( 3.717264591378875951E-15, 1.000000000000000000, 0.000000000000000000 ) ) ;
#22977 = DIRECTION ( 'NONE',  ( -1.000000000000000000, 0.000000000000000000, 0.000000000000000000 ) ) ;
#22978 = CARTESIAN_POINT ( 'NONE',  ( -9.547976262117254365, 2.355476262117183417, 54.00000000000000711 ) ) ;
#22979 = CARTESIAN_POINT ( 'NONE',  ( 7.000000000000000000, -26.50000000000000000, -5.530822723609929881 ) ) ;
#22980 = VERTEX_POINT ( 'NONE', #41536 ) ;
#22981 = CARTESIAN_POINT ( 'NONE',  ( -28.00000000000000000, -17.50000000000000000, -15.70500000000000007 ) ) ;
#22982 = CARTESIAN_POINT ( 'NONE',  ( -7.250000000000000888, 8.250000000000001776, -21.50000000000000000 ) ) ;
#22983 = CARTESIAN_POINT ( 'NONE',  ( -4.188533722949417282, -4.740315990920195510, 455.0000000000000568 ) ) ;
#22984 = ADVANCED_FACE ( 'NONE', ( #45425 ), #24220, .F. ) ;
#22986 = ORIENTED_EDGE ( 'NONE', *, *, #58161, .F. ) ;
#22985 = CARTESIAN_POINT ( 'NONE',  ( 7.969523737882813208, 9.722976262117192903, 26.00000000000000711 ) ) ;
#22987 = CARTESIAN_POINT ( 'NONE',  ( -7.250000000000000000, -7.449999999999998401, -19.50000000000000000 ) ) ;
#22988 = DIRECTION ( 'NONE',  ( -0.000000000000000000, -0.000000000000000000, 1.000000000000000000 ) ) ;
#22989 = ADVANCED_FACE ( 'NONE', ( #68409 ), #29166, .F. ) ;
#22990 = ORIENTED_EDGE ( 'NONE', *, *, #21040, .T. ) ;
#22991 = CARTESIAN_POINT ( 'NONE',  ( -0.9414762621172249046, 9.915476262117151052, 54.00000000000000711 ) ) ;
#22992 = ADVANCED_FACE ( 'NONE', ( #46828 ), #68055, .F. ) ;
#22993 = CARTESIAN_POINT ( 'NONE',  ( 9.912023737882799779, 6.817976262117189989, 26.00000000000000711 ) ) ;
#22994 = ADVANCED_FACE ( 'NONE', ( #67699 ), #63103, .F. ) ;
#22995 = ORIENTED_EDGE ( 'NONE', *, *, #28881, .T. ) ;
#22996 = CARTESIAN_POINT ( 'NONE',  ( 41.09999999999999432, 13.66939075806899950, 20.80000000000000426 ) ) ;
#22997 = CARTESIAN_POINT ( 'NONE',  ( 29.50000000000000355, -11.50000000000000000, 19.00000000000000000 ) ) ;
#22998 = DIRECTION ( 'NONE',  ( 0.000000000000000000, 0.000000000000000000, 1.000000000000000000 ) ) ;
#22999 = EDGE_CURVE ( 'NONE', #22939, #50838, #14335, .T. ) ;
#23000 = EDGE_CURVE ( 'NONE', #19035, #59906, #52143, .T. ) ;
#23001 = DIRECTION ( 'NONE',  ( -0.5773502691896268413, 0.5773502691896275074, -0.5773502691896227335 ) ) ;
#23002 = FACE_OUTER_BOUND ( 'NONE', #9891, .T. ) ;
#23003 = CIRCLE ( 'NONE', #62508, 25.39999999999999858 ) ;
#23004 = VECTOR ( 'NONE', #69574, 1000.000000000000000 ) ;
#23005 = EDGE_CURVE ( 'NONE', #9490, #39690, #17703, .T. ) ;
#23006 = ORIENTED_EDGE ( 'NONE', *, *, #18988, .F. ) ;
#23007 = CARTESIAN_POINT ( 'NONE',  ( 3.606483450353397568, 4.609516549646590633, 455.0000000000000568 ) ) ;
#23008 = EDGE_LOOP ( 'NONE', ( #46922, #17030, #45030, #33421 ) ) ;
#23009 = VERTEX_POINT ( 'NONE', #56391 ) ;
#23010 = CARTESIAN_POINT ( 'NONE',  ( 11.12648345035337982, -7.806483450353395526, 195.0000000000000284 ) ) ;
#23011 = CARTESIAN_POINT ( 'NONE',  ( -11.11351654964679270, -7.806483450353373321, 455.0000000000000568 ) ) ;
#23012 = VECTOR ( 'NONE', #22478, 1000.000000000000000 ) ;
#23013 = CARTESIAN_POINT ( 'NONE',  ( 41.09999999999999432, 20.60000000000000142, 13.86939075806900057 ) ) ;
#23014 = AXIS2_PLACEMENT_3D ( 'NONE', #65142, #69747, #11035 ) ;
#23015 = AXIS2_PLACEMENT_3D ( 'NONE', #22817, #28457, #11844 ) ;
#23016 = CARTESIAN_POINT ( 'NONE',  ( 7.250000000000004441, 7.450000000000001954, -20.50000000000000000 ) ) ;
#23017 = ORIENTED_EDGE ( 'NONE', *, *, #19345, .T. ) ;
#23018 = ORIENTED_EDGE ( 'NONE', *, *, #42538, .T. ) ;
#23019 = LINE ( 'NONE', #44569, #14896 ) ;
#23020 = EDGE_LOOP ( 'NONE', ( #11216, #6763, #51581, #18878 ) ) ;
#23021 = DIRECTION ( 'NONE',  ( 0.000000000000000000, 0.000000000000000000, 1.000000000000000000 ) ) ;
#23022 = DIRECTION ( 'NONE',  ( -1.836970198721029934E-16, 1.836970198721036344E-16, -1.000000000000000000 ) ) ;
#23023 = CARTESIAN_POINT ( 'NONE',  ( -4.031976262117261456, 3.142976262117183506, 26.00000000000000711 ) ) ;
#23025 = DIRECTION ( 'NONE',  ( -1.836970198721029934E-16, 1.836970198721036590E-16, -1.000000000000000000 ) ) ;
#23024 = DIRECTION ( 'NONE',  ( -0.000000000000000000, -0.000000000000000000, -1.000000000000000000 ) ) ;
#23026 = ORIENTED_EDGE ( 'NONE', *, *, #51636, .T. ) ;
#23028 = ORIENTED_EDGE ( 'NONE', *, *, #63917, .F. ) ;
#23027 = DIRECTION ( 'NONE',  ( -0.000000000000000000, -1.000000000000000000, -0.000000000000000000 ) ) ;
#23029 = ORIENTED_EDGE ( 'NONE', *, *, #32771, .F. ) ;
#23030 = ORIENTED_EDGE ( 'NONE', *, *, #32377, .F. ) ;
#23031 = LINE ( 'NONE', #28334, #25328 ) ;
#23032 = EDGE_CURVE ( 'NONE', #39907, #26623, #40476, .T. ) ;
#23033 = FACE_OUTER_BOUND ( 'NONE', #20796, .T. ) ;
#23034 = DIRECTION ( 'NONE',  ( -1.836970198721029934E-16, 1.836970198721036344E-16, -1.000000000000000000 ) ) ;
#23035 = ORIENTED_EDGE ( 'NONE', *, *, #67472, .F. ) ;
#23036 = ORIENTED_EDGE ( 'NONE', *, *, #48075, .T. ) ;
#23037 = EDGE_CURVE ( 'NONE', #19031, #48215, #48353, .T. ) ;
#23038 = EDGE_CURVE ( 'NONE', #9556, #43562, #19981, .T. ) ;
#23039 = PLANE ( 'NONE',  #50111 ) ;
#23040 = DIRECTION ( 'NONE',  ( -1.000000000000000000, 0.000000000000000000, 0.000000000000000000 ) ) ;
#23041 = VECTOR ( 'NONE', #10234, 1000.000000000000000 ) ;
#23042 = ADVANCED_FACE ( 'NONE', ( #3705 ), #51795, .T. ) ;
#23043 = ORIENTED_EDGE ( 'NONE', *, *, #37299, .T. ) ;
#23044 = ORIENTED_EDGE ( 'NONE', *, *, #12876, .F. ) ;
#23045 = CARTESIAN_POINT ( 'NONE',  ( 283.0000000000000568, -39.79999999999905214, -12.69999999999999929 ) ) ;
#23046 = CARTESIAN_POINT ( 'NONE',  ( -29.50000000000000355, -12.00000000000000000, 11.00000000000000000 ) ) ;
#23047 = ORIENTED_EDGE ( 'NONE', *, *, #63111, .T. ) ;
#23048 = VECTOR ( 'NONE', #54068, 1000.000000000000114 ) ;
#23049 = VECTOR ( 'NONE', #4787, 1000.000000000000000 ) ;
#23050 = DIRECTION ( 'NONE',  ( -1.000000000000000000, 0.000000000000000000, 0.000000000000000000 ) ) ;
#23052 = ORIENTED_EDGE ( 'NONE', *, *, #8302, .F. ) ;
#23051 = CYLINDRICAL_SURFACE ( 'NONE', #8032, 4.000000000000000000 ) ;
#23053 = ORIENTED_EDGE ( 'NONE', *, *, #10262, .F. ) ;
#23054 = CARTESIAN_POINT ( 'NONE',  ( 7.250000000000005329, 7.250000000000000888, -10.50000000000000000 ) ) ;
#23055 = CARTESIAN_POINT ( 'NONE',  ( 22.90000000000000213, -21.00000000000001421, -13.86939075806900945 ) ) ;
#23056 = CIRCLE ( 'NONE', #53570, 4.000000000000000000 ) ;
#23057 = AXIS2_PLACEMENT_3D ( 'NONE', #34016, #55257, #6801 ) ;
#23058 = DIRECTION ( 'NONE',  ( 0.5773502691896175154, 0.5773502691896339467, 0.5773502691896257311 ) ) ;
#23059 = CARTESIAN_POINT ( 'NONE',  ( 289.2330000000000041, 0.000000000000000000, 4.000000000000000000 ) ) ;
#23060 = CARTESIAN_POINT ( 'NONE',  ( 6.832023737882818359, -9.737023737882811503, 26.00000000000000000 ) ) ;
#23061 = DIRECTION ( 'NONE',  ( 0.000000000000000000, 1.000000000000000000, 0.000000000000000000 ) ) ;
#23062 = AXIS2_PLACEMENT_3D ( 'NONE', #17969, #66064, #7011 ) ;
#23063 = EDGE_LOOP ( 'NONE', ( #52290, #54710 ) ) ;
#23064 = DIRECTION ( 'NONE',  ( 1.000000000000000000, -0.000000000000000000, -0.000000000000000000 ) ) ;
#23066 = ORIENTED_EDGE ( 'NONE', *, *, #38966, .T. ) ;
#23065 = LINE ( 'NONE', #8537, #34407 ) ;
#23067 = EDGE_CURVE ( 'NONE', #20590, #50665, #29867, .T. ) ;
#23068 = CYLINDRICAL_SURFACE ( 'NONE', #60347, 1.399999999999999245 ) ;
#23069 = DIRECTION ( 'NONE',  ( 0.000000000000000000, 1.000000000000000000, 0.000000000000000000 ) ) ;
#23070 = AXIS2_PLACEMENT_3D ( 'NONE', #3945, #8527, #13841 ) ;
#23071 = DIRECTION ( 'NONE',  ( -1.000000000000000000, 0.000000000000000000, 0.000000000000000000 ) ) ;
#23072 = CIRCLE ( 'NONE', #36610, 0.1999999999999987899 ) ;
#23073 = CARTESIAN_POINT ( 'NONE',  ( 0.5000000000000000000, -21.00000000000000000, -18.00000000000000355 ) ) ;
#23074 = CARTESIAN_POINT ( 'NONE',  ( 30.00000000000000000, -5.200000000000001066, -26.59999999999999787 ) ) ;
#23075 = ORIENTED_EDGE ( 'NONE', *, *, #20857, .F. ) ;
#23076 = VERTEX_POINT ( 'NONE', #35509 ) ;
#23077 = DIRECTION ( 'NONE',  ( -0.000000000000000000, -0.000000000000000000, -1.000000000000000000 ) ) ;
#23078 = EDGE_CURVE ( 'NONE', #35467, #51761, #57093, .T. ) ;
#23079 = FACE_OUTER_BOUND ( 'NONE', #33701, .T. ) ;
#23080 = EDGE_CURVE ( 'NONE', #36191, #6937, #30823, .T. ) ;
#23081 = ORIENTED_EDGE ( 'NONE', *, *, #43961, .F. ) ;
#23082 = DIRECTION ( 'NONE',  ( 0.000000000000000000, 0.000000000000000000, 1.000000000000000000 ) ) ;
#23083 = EDGE_LOOP ( 'NONE', ( #66860, #46680, #9463, #5128 ) ) ;
#23084 = VECTOR ( 'NONE', #33014, 1000.000000000000000 ) ;
#23085 = EDGE_LOOP ( 'NONE', ( #14355, #14447, #14759, #22792, #23795, #4222, #9534, #3102, #67666, #60357, #14758, #23441, #52011, #51414, #13243, #27208, #31781 ) ) ;
#23086 = DIRECTION ( 'NONE',  ( 0.000000000000000000, 1.000000000000000000, 0.000000000000000000 ) ) ;
#23087 = DIRECTION ( 'NONE',  ( 1.000000000000000000, 0.000000000000000000, 0.000000000000000000 ) ) ;
#23088 = ORIENTED_EDGE ( 'NONE', *, *, #11160, .F. ) ;
#23089 = DIRECTION ( 'NONE',  ( 1.000000000000000000, -6.308085367188447236E-15, -2.317552966102676720E-30 ) ) ;
#23090 = CIRCLE ( 'NONE', #33305, 0.7499999999999997780 ) ;
#23091 = CARTESIAN_POINT ( 'NONE',  ( -8.079219948824961861, -8.711985858128649340, 54.00000000000000711 ) ) ;
#23092 = CYLINDRICAL_SURFACE ( 'NONE', #10300, 1.621000000000000885 ) ;
#23093 = EDGE_LOOP ( 'NONE', ( #61809, #30164, #16836, #56436 ) ) ;
#23095 = EDGE_LOOP ( 'NONE', ( #20151, #59295, #60898, #13610 ) ) ;
#23094 = DIRECTION ( 'NONE',  ( -1.000000000000000000, 1.079558018506126467E-14, 1.836970198721049656E-16 ) ) ;
#23096 = VECTOR ( 'NONE', #10487, 1000.000000000000114 ) ;
#23097 = AXIS2_PLACEMENT_3D ( 'NONE', #8864, #41392, #35025 ) ;
#23098 = CARTESIAN_POINT ( 'NONE',  ( -7.250000000000001776, -7.249999999999998224, -9.500000000000001776 ) ) ;
#23099 = CARTESIAN_POINT ( 'NONE',  ( -30.00000000000000000, -16.28999999999999915, 14.50000000000000000 ) ) ;
#23100 = DIRECTION ( 'NONE',  ( -0.000000000000000000, -0.000000000000000000, 1.000000000000000000 ) ) ;
#23101 = CARTESIAN_POINT ( 'NONE',  ( 0.000000000000000000, -7.449999999999998401, -15.00000000000000000 ) ) ;
#23102 = ORIENTED_EDGE ( 'NONE', *, *, #64860, .F. ) ;
#23103 = DIRECTION ( 'NONE',  ( 1.000000000000000000, -0.000000000000000000, -0.000000000000000000 ) ) ;
#23104 = VECTOR ( 'NONE', #48774, 1000.000000000000000 ) ;
#23105 = DIRECTION ( 'NONE',  ( 0.000000000000000000, -1.000000000000000000, 0.000000000000000000 ) ) ;
#23106 = ORIENTED_EDGE ( 'NONE', *, *, #33430, .T. ) ;
#23107 = ORIENTED_EDGE ( 'NONE', *, *, #67048, .T. ) ;
#23109 = ORIENTED_EDGE ( 'NONE', *, *, #53850, .T. ) ;
#23108 = VECTOR ( 'NONE', #38689, 1000.000000000000000 ) ;
#23110 = CYLINDRICAL_SURFACE ( 'NONE', #24229, 0.4999999999991868727 ) ;
#23111 = CYLINDRICAL_SURFACE ( 'NONE', #45602, 4.000000000000000000 ) ;
#23112 = DIRECTION ( 'NONE',  ( -1.000000000000000000, 0.000000000000000000, 0.000000000000000000 ) ) ;
#23113 =( LENGTH_UNIT ( ) NAMED_UNIT ( * ) SI_UNIT ( .MILLI., .METRE. ) );
#23114 = AXIS2_PLACEMENT_3D ( 'NONE', #38814, #45497, #55773 ) ;
#23115 = DIRECTION ( 'NONE',  ( -0.000000000000000000, -0.000000000000000000, -1.000000000000000000 ) ) ;
#23116 = ORIENTED_EDGE ( 'NONE', *, *, #6972, .F. ) ;
#23117 = ORIENTED_EDGE ( 'NONE', *, *, #66701, .F. ) ;
#23118 = ORIENTED_EDGE ( 'NONE', *, *, #11126, .T. ) ;
#23119 = EDGE_CURVE ( 'NONE', #31070, #22317, #5106, .T. ) ;
#23120 = AXIS2_PLACEMENT_3D ( 'NONE', #23286, #39880, #44849 ) ;
#23121 = CARTESIAN_POINT ( 'NONE',  ( 0.9555237378828163042, 9.390476262117214645, 54.00000000000000711 ) ) ;
#23122 = ORIENTED_EDGE ( 'NONE', *, *, #27103, .F. ) ;
#23123 = ORIENTED_EDGE ( 'NONE', *, *, #38619, .T. ) ;
#23124 = ADVANCED_FACE ( 'NONE', ( #30926, #68763 ), #52498, .T. ) ;
#23125 = ORIENTED_EDGE ( 'NONE', *, *, #34185, .F. ) ;
#23126 = ORIENTED_EDGE ( 'NONE', *, *, #37486, .F. ) ;
#23127 = DIRECTION ( 'NONE',  ( 1.000000000000000000, -0.000000000000000000, -0.000000000000000000 ) ) ;
#23129 = VERTEX_POINT ( 'NONE', #4763 ) ;
#23128 = DIRECTION ( 'NONE',  ( -0.000000000000000000, 1.000000000000000000, -0.000000000000000000 ) ) ;
#23130 = DIRECTION ( 'NONE',  ( -1.000000000000000000, 0.000000000000000000, 0.000000000000000000 ) ) ;
#23131 = CARTESIAN_POINT ( 'NONE',  ( -14.10805890929250062, -5.000000000000000000, -26.25000000000000000 ) ) ;
#23132 = PLANE ( 'NONE',  #36962 ) ;
#23133 = CIRCLE ( 'NONE', #38940, 24.99999999998789946 ) ;
#23135 = EDGE_LOOP ( 'NONE', ( #1350, #64240, #30866, #13727 ) ) ;
#23134 = DIRECTION ( 'NONE',  ( 0.000000000000000000, 0.000000000000000000, -1.000000000000000000 ) ) ;
#23136 = AXIS2_PLACEMENT_3D ( 'NONE', #64175, #15723, #59550 ) ;
#23137 = PLANE ( 'NONE',  #48639 ) ;
#23138 = PLANE ( 'NONE',  #13047 ) ;
#23139 = CARTESIAN_POINT ( 'NONE',  ( 11.00000000000000000, -5.599999999999999645, 27.00000000000000000 ) ) ;
#23140 = ADVANCED_FACE ( 'NONE', ( #4068 ), #3069, .F. ) ;
#23141 = ORIENTED_EDGE ( 'NONE', *, *, #65118, .F. ) ;
#23142 = DIRECTION ( 'NONE',  ( 0.000000000000000000, 0.000000000000000000, 1.000000000000000000 ) ) ;
#23143 = AXIS2_PLACEMENT_3D ( 'NONE', #62545, #57256, #8820 ) ;
#23145 = CARTESIAN_POINT ( 'NONE',  ( -10.30047626211728762, -6.657023737882746595, 26.00000000000000000 ) ) ;
#23144 = AXIS2_PLACEMENT_3D ( 'NONE', #15925, #64368, #59054 ) ;
#23146 = CARTESIAN_POINT ( 'NONE',  ( 6.749999999999996447, -7.348062532928000934, 5.000000000000000000 ) ) ;
#23147 = VECTOR ( 'NONE', #9570, 1000.000000000000000 ) ;
#23148 = VERTEX_POINT ( 'NONE', #36947 ) ;
#23149 = DIRECTION ( 'NONE',  ( 9.912705577010336396E-15, 1.000000000000000000, 0.000000000000000000 ) ) ;
#23150 = AXIS2_PLACEMENT_3D ( 'NONE', #45541, #62155, #28938 ) ;
#23151 = VECTOR ( 'NONE', #54964, 1000.000000000000000 ) ;
#23152 = FACE_OUTER_BOUND ( 'NONE', #65974, .T. ) ;
#23153 = DIRECTION ( 'NONE',  ( 1.836970198721029934E-16, 1.836970198721010706E-16, -1.000000000000000000 ) ) ;
#23154 = ORIENTED_EDGE ( 'NONE', *, *, #60185, .F. ) ;
#23155 = VECTOR ( 'NONE', #31926, 1000.000000000000000 ) ;
#23156 = CARTESIAN_POINT ( 'NONE',  ( -9.897976262117257562, 6.817976262117182884, 54.00000000000000711 ) ) ;
#23157 = CARTESIAN_POINT ( 'NONE',  ( 7.811466277050697293, 4.727349090213374794, 195.0000000000000284 ) ) ;
#23158 = DIRECTION ( 'NONE',  ( -1.836970198721029934E-16, 1.836970198721036590E-16, -1.000000000000000000 ) ) ;
#23159 = FACE_OUTER_BOUND ( 'NONE', #28972, .T. ) ;
#23160 = ADVANCED_FACE ( 'NONE', ( #21366 ), #64171, .F. ) ;
#23161 = COLOUR_RGB ( '', 0.40784314, 0.44705882, 0.49803922) ;
#23162 = EDGE_CURVE ( 'NONE', #14966, #27877, #66307, .T. ) ;
#23163 = ORIENTED_EDGE ( 'NONE', *, *, #8366, .F. ) ;
#23164 = DIRECTION ( 'NONE',  ( 1.000000000000000000, 0.000000000000000000, 0.000000000000000000 ) ) ;
#23165 = CARTESIAN_POINT ( 'NONE',  ( 10.09643294401454661, -9.106483450353492159, 455.0000000000000568 ) ) ;
#23166 = EDGE_CURVE ( 'NONE', #5963, #34600, #68593, .T. ) ;
#23167 = DIRECTION ( 'NONE',  ( 0.000000000000000000, 0.000000000000000000, -1.000000000000000000 ) ) ;
#23168 = AXIS2_PLACEMENT_3D ( 'NONE', #56448, #29570, #57501 ) ;
#23169 = DIRECTION ( 'NONE',  ( 0.000000000000000000, 1.000000000000000000, -0.000000000000000000 ) ) ;
#23170 = FACE_OUTER_BOUND ( 'NONE', #52840, .T. ) ;
#23171 = VERTEX_POINT ( 'NONE', #15014 ) ;
#23172 = LINE ( 'NONE', #17873, #69398 ) ;
#23173 = DIRECTION ( 'NONE',  ( 0.000000000000000000, 0.000000000000000000, 1.000000000000000000 ) ) ;
#23174 = EDGE_CURVE ( 'NONE', #34997, #52164, #69107, .T. ) ;
#23175 = DIRECTION ( 'NONE',  ( -2.135044278125299371E-15, 1.000000000000000000, 0.000000000000000000 ) ) ;
#23176 = EDGE_CURVE ( 'NONE', #42678, #49724, #36572, .T. ) ;
#23177 = EDGE_CURVE ( 'NONE', #65336, #19785, #31298, .T. ) ;
#23178 = CARTESIAN_POINT ( 'NONE',  ( 25.90000000000000213, -0.000000000000000000, -20.80000000000000071 ) ) ;
#23179 = EDGE_CURVE ( 'NONE', #66712, #26265, #42581, .T. ) ;
#23180 = DIRECTION ( 'NONE',  ( 0.000000000000000000, 1.000000000000000000, 0.000000000000000000 ) ) ;
#23181 = ORIENTED_EDGE ( 'NONE', *, *, #42634, .F. ) ;
#23182 = VERTEX_POINT ( 'NONE', #25983 ) ;
#23183 = EDGE_CURVE ( 'NONE', #49229, #41582, #52766, .T. ) ;
#23184 = CARTESIAN_POINT ( 'NONE',  ( -7.750000000000001776, 7.750000000000001776, 5.000000000000000000 ) ) ;
#23185 = DIRECTION ( 'NONE',  ( -0.000000000000000000, -0.000000000000000000, -1.000000000000000000 ) ) ;
#23186 = ORIENTED_EDGE ( 'NONE', *, *, #43721, .F. ) ;
#23187 = CARTESIAN_POINT ( 'NONE',  ( -3.650476262117333892, -10.31452373788281740, 54.00000000000000711 ) ) ;
#23188 = CIRCLE ( 'NONE', #20982, 0.5249999999999994671 ) ;
#23189 = ORIENTED_EDGE ( 'NONE', *, *, #56944, .T. ) ;
#23190 = VECTOR ( 'NONE', #28139, 1000.000000000000000 ) ;
#23191 = DIRECTION ( 'NONE',  ( 0.000000000000000000, 0.000000000000000000, 1.000000000000000000 ) ) ;
#23192 = ORIENTED_EDGE ( 'NONE', *, *, #2472, .F. ) ;
#23193 = ORIENTED_EDGE ( 'NONE', *, *, #41431, .T. ) ;
#23194 = CARTESIAN_POINT ( 'NONE',  ( -6.775514141871385121, 7.394232575409538377, 54.00000000000000711 ) ) ;
#23195 = CARTESIAN_POINT ( 'NONE',  ( 39.00000000000000000, -0.2000000000000000111, 0.000000000000000000 ) ) ;
#23196 = DIRECTION ( 'NONE',  ( 0.6414496315691420314, -0.7671651518153128624, 0.000000000000000000 ) ) ;
#23197 = CARTESIAN_POINT ( 'NONE',  ( 7.250000000000005329, 7.250000000000000888, -11.00000000000000000 ) ) ;
#23198 = VECTOR ( 'NONE', #44005, 1000.000000000000000 ) ;
#23199 = CIRCLE ( 'NONE', #29961, 1.449999999999996403 ) ;
#23200 = VECTOR ( 'NONE', #36901, 1000.000000000000000 ) ;
#23201 = ORIENTED_EDGE ( 'NONE', *, *, #56490, .F. ) ;
#23202 = VERTEX_POINT ( 'NONE', #15719 ) ;
#23203 = DIRECTION ( 'NONE',  ( 0.000000000000000000, -1.000000000000000000, 0.000000000000000000 ) ) ;
#23204 = DIRECTION ( 'NONE',  ( 1.000000000000000000, -0.000000000000000000, -0.000000000000000000 ) ) ;
#23205 = VECTOR ( 'NONE', #36329, 1000.000000000000114 ) ;
#23206 = ORIENTED_EDGE ( 'NONE', *, *, #15059, .T. ) ;
#23207 = ORIENTED_EDGE ( 'NONE', *, *, #63154, .T. ) ;
#23208 = VERTEX_POINT ( 'NONE', #42225 ) ;
#23209 = VECTOR ( 'NONE', #63228, 1000.000000000000000 ) ;
#23210 = DIRECTION ( 'NONE',  ( 0.000000000000000000, 0.000000000000000000, 1.000000000000000000 ) ) ;
#23212 = ORIENTED_EDGE ( 'NONE', *, *, #55280, .T. ) ;
#23211 = DIRECTION ( 'NONE',  ( 0.000000000000000000, -1.000000000000000000, 0.000000000000000000 ) ) ;
#23213 = DIRECTION ( 'NONE',  ( 1.000000000000000000, 0.000000000000000000, 0.000000000000000000 ) ) ;
#23214 = VECTOR ( 'NONE', #15555, 1000.000000000000000 ) ;
#23215 = DIRECTION ( 'NONE',  ( -0.000000000000000000, 3.673940397442059868E-16, -1.000000000000000000 ) ) ;
#23216 = ORIENTED_EDGE ( 'NONE', *, *, #56768, .F. ) ;
#23217 = VECTOR ( 'NONE', #55174, 1000.000000000000000 ) ;
#23218 = EDGE_LOOP ( 'NONE', ( #26373, #49403, #67963, #13357 ) ) ;
#23219 = ADVANCED_FACE ( 'NONE', ( #48588 ), #10066, .T. ) ;
#23220 = CARTESIAN_POINT ( 'NONE',  ( -7.250000000000000000, -7.449999999999998401, -25.00000000000000000 ) ) ;
#23221 = CARTESIAN_POINT ( 'NONE',  ( -8.250000000000001776, 7.250000000000000888, -26.00000000000001066 ) ) ;
#23222 = ADVANCED_FACE ( 'NONE', ( #53551 ), #69453, .T. ) ;
#23223 = CARTESIAN_POINT ( 'NONE',  ( 29.25000000000000000, -5.200000000000001066, 26.25000000000000000 ) ) ;
#23224 = CARTESIAN_POINT ( 'NONE',  ( -11.00000000000000000, -11.70000000000000284, 12.50000000000000000 ) ) ;
#23225 = DIRECTION ( 'NONE',  ( 0.7071067811865451302, -0.7071067811865500152, 0.000000000000000000 ) ) ;
#23226 = EDGE_CURVE ( 'NONE', #39124, #34907, #26674, .T. ) ;
#23227 =( GEOMETRIC_REPRESENTATION_CONTEXT ( 3 ) GLOBAL_UNCERTAINTY_ASSIGNED_CONTEXT ( ( #69845 ) ) GLOBAL_UNIT_ASSIGNED_CONTEXT ( ( #9067, #63158, #57848 ) ) REPRESENTATION_CONTEXT ( 'NONE', 'WORKASPACE' ) );
#23229 = ORIENTED_EDGE ( 'NONE', *, *, #36280, .T. ) ;
#23228 = LINE ( 'NONE', #34170, #12801 ) ;
#23230 = ORIENTED_EDGE ( 'NONE', *, *, #40947, .T. ) ;
#23231 = CARTESIAN_POINT ( 'NONE',  ( 9.247904806590725002, 9.942044687070426434, 455.0000000000000568 ) ) ;
#23232 = CARTESIAN_POINT ( 'NONE',  ( 10.92648345035336099, 9.093516549646611935, 195.0000000000000284 ) ) ;
#23233 = VECTOR ( 'NONE', #36320, 1000.000000000000000 ) ;
#23234 = LINE ( 'NONE', #8358, #35898 ) ;
#23235 = EDGE_CURVE ( 'NONE', #18501, #15780, #23408, .T. ) ;
#23236 = DIRECTION ( 'NONE',  ( 0.000000000000000000, -0.9921567416492215186, 0.1249999999999996531 ) ) ;
#23237 = CIRCLE ( 'NONE', #62768, 1.500000000000000444 ) ;
#23238 = DIRECTION ( 'NONE',  ( -1.000000000000000000, 0.000000000000000000, 0.000000000000000000 ) ) ;
#23239 = ORIENTED_EDGE ( 'NONE', *, *, #67053, .T. ) ;
#23240 = CARTESIAN_POINT ( 'NONE',  ( 152.0064834503532722, 2.160375375128253950, 5.000000000000000000 ) ) ;
#23241 = CARTESIAN_POINT ( 'NONE',  ( 7.250000000000005329, -7.449999999999998401, -25.50000000000000355 ) ) ;
#23242 = CARTESIAN_POINT ( 'NONE',  ( 276.8775010008008053, -21.00000000000000000, 17.50000000000000000 ) ) ;
#23243 = CARTESIAN_POINT ( 'NONE',  ( 283.0000000000000568, -20.50000000000000000, 13.00000000000000178 ) ) ;
#23244 = VECTOR ( 'NONE', #41839, 1000.000000000000000 ) ;
#23245 = VECTOR ( 'NONE', #47267, 1000.000000000000000 ) ;
#23246 = VECTOR ( 'NONE', #1144, 1000.000000000000000 ) ;
#23247 = EDGE_CURVE ( 'NONE', #26502, #53142, #823, .T. ) ;
#23248 = FACE_BOUND ( 'NONE', #58372, .T. ) ;
#23249 = CARTESIAN_POINT ( 'NONE',  ( 11.00000000000000000, -15.97213595500069871, 14.50000000000000000 ) ) ;
#23250 = VECTOR ( 'NONE', #51063, 1000.000000000000000 ) ;
#23251 = VECTOR ( 'NONE', #23025, 1000.000000000000000 ) ;
#23252 = AXIS2_PLACEMENT_3D ( 'NONE', #14871, #69672, #62961 ) ;
#23253 = LINE ( 'NONE', #65366, #26230 ) ;
#23254 = EDGE_LOOP ( 'NONE', ( #57560, #61046, #24309, #56370 ) ) ;
#23255 = CARTESIAN_POINT ( 'NONE',  ( 8.930623737882818602, -8.580623737882845603, 26.00000000000000000 ) ) ;
#23256 = DIRECTION ( 'NONE',  ( 0.000000000000000000, 0.000000000000000000, 1.000000000000000000 ) ) ;
#23257 = EDGE_LOOP ( 'NONE', ( #53916, #22075, #301, #7667 ) ) ;
#23258 = CARTESIAN_POINT ( 'NONE',  ( 14.50000000000000000, -42.50000000000000000, 27.00000000000000000 ) ) ;
#23259 = DIRECTION ( 'NONE',  ( -1.000000000000000000, 0.000000000000000000, 0.000000000000000000 ) ) ;
#23260 = VECTOR ( 'NONE', #45388, 1000.000000000000000 ) ;
#23261 = CARTESIAN_POINT ( 'NONE',  ( 20.90000000000000213, 20.60000000000000142, -13.86939075806900057 ) ) ;
#23262 = DIRECTION ( 'NONE',  ( 1.000000000000000000, 0.000000000000000000, 0.000000000000000000 ) ) ;
#23263 = EDGE_CURVE ( 'NONE', #35740, #23540, #55618, .T. ) ;
#23264 = CARTESIAN_POINT ( 'NONE',  ( 7.450000000000004619, -1.336933437520057563E-15, -24.00000000000000000 ) ) ;
#23265 = ORIENTED_EDGE ( 'NONE', *, *, #64622, .T. ) ;
#23266 = EDGE_CURVE ( 'NONE', #29173, #54436, #28389, .T. ) ;
#23267 = DIRECTION ( 'NONE',  ( 0.000000000000000000, 1.000000000000000000, -0.000000000000000000 ) ) ;
#23268 = CIRCLE ( 'NONE', #65082, 3.500000000000003109 ) ;
#23269 = ORIENTED_EDGE ( 'NONE', *, *, #9099, .F. ) ;
#23270 = DIRECTION ( 'NONE',  ( 1.000000000000000000, 0.000000000000000000, 0.000000000000000000 ) ) ;
#23271 = ORIENTED_EDGE ( 'NONE', *, *, #49989, .T. ) ;
#23272 = DIRECTION ( 'NONE',  ( -5.120954910632640039E-15, -1.000000000000000000, -3.673940397442059868E-16 ) ) ;
#23273 = EDGE_CURVE ( 'NONE', #16440, #69650, #13204, .T. ) ;
#23274 = CARTESIAN_POINT ( 'NONE',  ( 7.272650909786598561, -7.811466277050860718, 455.0000000000000568 ) ) ;
#23275 = DIRECTION ( 'NONE',  ( -1.000000000000000000, 0.000000000000000000, 0.000000000000000000 ) ) ;
#23276 = EDGE_LOOP ( 'NONE', ( #63397, #26318, #18335, #6459 ) ) ;
#23277 = VERTEX_POINT ( 'NONE', #16762 ) ;
#23278 = DIRECTION ( 'NONE',  ( -0.000000000000000000, -0.000000000000000000, -1.000000000000000000 ) ) ;
#23279 = ORIENTED_EDGE ( 'NONE', *, *, #18068, .F. ) ;
#23280 = ORIENTED_EDGE ( 'NONE', *, *, #54940, .T. ) ;
#23281 = DIRECTION ( 'NONE',  ( 0.9375000000000006661, 0.000000000000000000, -0.3479852726768744020 ) ) ;
#23282 = CARTESIAN_POINT ( 'NONE',  ( 15.00000000000000000, -26.42999999999999972, -5.874955318979029784 ) ) ;
#23283 = DIRECTION ( 'NONE',  ( 0.000000000000000000, 0.000000000000000000, -1.000000000000000000 ) ) ;
#23284 = ORIENTED_EDGE ( 'NONE', *, *, #12368, .T. ) ;
#23285 = PLANE ( 'NONE',  #53827 ) ;
#23287 = LINE ( 'NONE', #44850, #33364 ) ;
#23286 = CARTESIAN_POINT ( 'NONE',  ( 30.00000000000000000, -16.28999999999999915, 14.50000000000000000 ) ) ;
#23288 = ORIENTED_EDGE ( 'NONE', *, *, #32454, .F. ) ;
#23290 = ORIENTED_EDGE ( 'NONE', *, *, #30535, .F. ) ;
#23289 = CARTESIAN_POINT ( 'NONE',  ( 7.000000000000000000, -23.65000000000000568, -12.40000000000000213 ) ) ;
#23291 = AXIS2_PLACEMENT_3D ( 'NONE', #64869, #54262, #37650 ) ;
#23292 = EDGE_LOOP ( 'NONE', ( #38283, #43683, #26462, #9577 ) ) ;
#23293 = EDGE_CURVE ( 'NONE', #44220, #28197, #12092, .T. ) ;
#23294 = CIRCLE ( 'NONE', #49263, 4.000000000000000888 ) ;
#23295 = AXIS2_PLACEMENT_3D ( 'NONE', #53088, #52745, #14187 ) ;
#23296 = FACE_OUTER_BOUND ( 'NONE', #3501, .T. ) ;
#23297 = EDGE_LOOP ( 'NONE', ( #60413, #9232, #46862, #54305 ) ) ;
#23298 = EDGE_CURVE ( 'NONE', #1375, #65337, #58412, .T. ) ;
#23299 = VECTOR ( 'NONE', #61567, 1000.000000000000000 ) ;
#23300 = VECTOR ( 'NONE', #64085, 1000.000000000000000 ) ;
#23301 = CARTESIAN_POINT ( 'NONE',  ( 10.00000000000000000, -21.00000000000000000, 18.00000000000000355 ) ) ;
#23302 = DIRECTION ( 'NONE',  ( 0.000000000000000000, 0.000000000000000000, -1.000000000000000000 ) ) ;
#23303 = EDGE_LOOP ( 'NONE', ( #40856, #39900, #67194, #49579 ) ) ;
#23304 = ORIENTED_EDGE ( 'NONE', *, *, #43537, .F. ) ;
#23305 = ADVANCED_FACE ( 'NONE', ( #28735 ), #34035, .F. ) ;
#23306 = AXIS2_PLACEMENT_3D ( 'NONE', #38980, #55248, #11752 ) ;
#23307 = VECTOR ( 'NONE', #35629, 1000.000000000000114 ) ;
#23308 = DIRECTION ( 'NONE',  ( 0.000000000000000000, -1.000000000000000000, 0.000000000000000000 ) ) ;
#23309 = ADVANCED_FACE ( 'NONE', ( #37987 ), #22416, .F. ) ;
#23310 = FACE_OUTER_BOUND ( 'NONE', #43006, .T. ) ;
#23311 = VERTEX_POINT ( 'NONE', #1193 ) ;
#23312 = LINE ( 'NONE', #50179, #61313 ) ;
#23313 = FACE_OUTER_BOUND ( 'NONE', #49288, .T. ) ;
#23314 = ADVANCED_FACE ( 'NONE', ( #1876 ), #38329, .F. ) ;
#23315 = PLANE ( 'NONE',  #38453 ) ;
#23316 = VERTEX_POINT ( 'NONE', #49294 ) ;
#23317 = AXIS2_PLACEMENT_3D ( 'NONE', #15258, #10298, #30812 ) ;
#23318 = CARTESIAN_POINT ( 'NONE',  ( 275.0000000000000000, -26.79000000000000625, 0.000000000000000000 ) ) ;
#23319 = PLANE ( 'NONE',  #52073 ) ;
#23320 = ADVANCED_FACE ( 'NONE', ( #866 ), #17788, .T. ) ;
#23322 = VERTEX_POINT ( 'NONE', #65208 ) ;
#23321 = CARTESIAN_POINT ( 'NONE',  ( -29.25000000000000000, -5.200000000000001066, 26.25000000000000000 ) ) ;
#23324 = VERTEX_POINT ( 'NONE', #11777 ) ;
#23323 = DIRECTION ( 'NONE',  ( -0.6414496315691445849, 0.7671651518153106419, 2.818519042764040096E-16 ) ) ;
#23325 = EDGE_CURVE ( 'NONE', #23844, #58579, #59883, .T. ) ;
#23326 = CARTESIAN_POINT ( 'NONE',  ( 25.50000000000000355, -15.12100000000000044, -22.50000000000000000 ) ) ;
#23327 = PLANE ( 'NONE',  #25065 ) ;
#23328 = DIRECTION ( 'NONE',  ( -1.000000000000000000, 3.491481338843133355E-15, 1.836970198721036344E-16 ) ) ;
#23329 = EDGE_CURVE ( 'NONE', #30577, #38571, #54248, .T. ) ;
#23330 = EDGE_CURVE ( 'NONE', #46437, #10205, #6460, .T. ) ;
#23331 = PLANE ( 'NONE',  #17021 ) ;
#23332 = CARTESIAN_POINT ( 'NONE',  ( -13.00000000000000178, -16.28999999999710369, -14.50000000000000000 ) ) ;
#23333 = ORIENTED_EDGE ( 'NONE', *, *, #63786, .F. ) ;
#23334 = DIRECTION ( 'NONE',  ( 0.000000000000000000, -0.6857142857147903170, -0.7278708115913530285 ) ) ;
#23335 = CARTESIAN_POINT ( 'NONE',  ( -5.242976262117280406, -5.257023737882805747, 54.00000000000000711 ) ) ;
#23336 = ADVANCED_FACE ( 'NONE', ( #28063 ), #60911, .T. ) ;
#23337 = CARTESIAN_POINT ( 'NONE',  ( -17.00000000000000000, -17.35230188589299871, -15.35019951917099945 ) ) ;
#23339 = ORIENTED_EDGE ( 'NONE', *, *, #55276, .T. ) ;
#23338 = LINE ( 'NONE', #1764, #62669 ) ;
#23340 = PLANE ( 'NONE',  #18847 ) ;
#23341 = AXIS2_PLACEMENT_3D ( 'NONE', #56216, #34274, #55861 ) ;
#23342 = CARTESIAN_POINT ( 'NONE',  ( -11.77351654964670935, 4.393516549646602876, 455.0000000000000568 ) ) ;
#23343 = ADVANCED_FACE ( 'NONE', ( #22063 ), #43631, .F. ) ;
#23344 = VECTOR ( 'NONE', #34520, 1000.000000000000000 ) ;
#23345 = ORIENTED_EDGE ( 'NONE', *, *, #9509, .F. ) ;
#23346 = DIRECTION ( 'NONE',  ( 0.000000000000000000, 0.000000000000000000, 1.000000000000000000 ) ) ;
#23347 = LINE ( 'NONE', #27614, #48649 ) ;
#23348 = ORIENTED_EDGE ( 'NONE', *, *, #63563, .T. ) ;
#23349 = CARTESIAN_POINT ( 'NONE',  ( -2.530476262117325792, -9.562023737882828556, 54.00000000000000711 ) ) ;
#23350 = DIRECTION ( 'NONE',  ( 0.000000000000000000, 0.000000000000000000, -1.000000000000000000 ) ) ;
#23351 = CIRCLE ( 'NONE', #59504, 5.000000000000000000 ) ;
#23352 = CARTESIAN_POINT ( 'NONE',  ( -11.29351654964668583, 8.513516549646642062, 194.9999952000000292 ) ) ;
#23353 = ADVANCED_FACE ( 'NONE', ( #6819 ), #61247, .F. ) ;
#23354 = DIRECTION ( 'NONE',  ( 0.5001543609659999667, 0.000000000000000000, -0.8659362650950080953 ) ) ;
#23355 = EDGE_CURVE ( 'NONE', #34313, #46798, #24138, .T. ) ;
#23356 = AXIS2_PLACEMENT_3D ( 'NONE', #34457, #14321, #57444 ) ;
#23357 = PLANE ( 'NONE',  #65861 ) ;
#23358 = ORIENTED_EDGE ( 'NONE', *, *, #16335, .T. ) ;
#23359 = AXIS2_PLACEMENT_3D ( 'NONE', #23472, #67124, #46599 ) ;
#23360 = CARTESIAN_POINT ( 'NONE',  ( 7.811466277050736373, -7.272650909786728235, 455.0000000000000568 ) ) ;
#23361 = ORIENTED_EDGE ( 'NONE', *, *, #35701, .F. ) ;
#23362 = EDGE_LOOP ( 'NONE', ( #7784, #51482, #64548, #35673 ) ) ;
#23363 = DIRECTION ( 'NONE',  ( -0.000000000000000000, -0.000000000000000000, -1.000000000000000000 ) ) ;
#23364 = AXIS2_PLACEMENT_3D ( 'NONE', #27946, #38227, #59778 ) ;
#23365 = VECTOR ( 'NONE', #57909, 1000.000000000000000 ) ;
#23366 = CIRCLE ( 'NONE', #838, 2.215251240775983899 ) ;
#23367 = DIRECTION ( 'NONE',  ( 0.000000000000000000, 0.000000000000000000, 1.000000000000000000 ) ) ;
#23368 = CARTESIAN_POINT ( 'NONE',  ( -11.00000000000000000, -10.85999999999999943, 9.000000000000001776 ) ) ;
#23369 = ORIENTED_EDGE ( 'NONE', *, *, #36262, .T. ) ;
#23370 = VERTEX_POINT ( 'NONE', #62656 ) ;
#23371 = CARTESIAN_POINT ( 'NONE',  ( 29.50000000000000355, -12.00000000000000000, -11.00000000000000000 ) ) ;
#23372 = VERTEX_POINT ( 'NONE', #39693 ) ;
#23373 = PRODUCT_DEFINITION_SHAPE ( 'NONE', 'NONE',  #63345 ) ;
#23374 = AXIS2_PLACEMENT_3D ( 'NONE', #25520, #58031, #9961 ) ;
#23375 = DIRECTION ( 'NONE',  ( -1.034072152899300747E-14, -1.000000000000000000, 0.000000000000000000 ) ) ;
#23376 = FACE_OUTER_BOUND ( 'NONE', #13572, .T. ) ;
#23377 = CYLINDRICAL_SURFACE ( 'NONE', #52286, 1.000000000000001776 ) ;
#23378 = FACE_OUTER_BOUND ( 'NONE', #18024, .T. ) ;
#23380 = DIRECTION ( 'NONE',  ( 0.000000000000000000, -1.000000000000000000, -0.000000000000000000 ) ) ;
#23379 = DIRECTION ( 'NONE',  ( -1.000000000000000000, 0.000000000000000000, 0.000000000000000000 ) ) ;
#23381 = EDGE_LOOP ( 'NONE', ( #67770, #10098, #47600, #17787 ) ) ;
#23383 = ORIENTED_EDGE ( 'NONE', *, *, #24948, .F. ) ;
#23382 = CARTESIAN_POINT ( 'NONE',  ( 46.39999999999999858, 33.00000000000000000, -0.2500000000000000000 ) ) ;
#23384 = ORIENTED_EDGE ( 'NONE', *, *, #20985, .T. ) ;
#23385 = VERTEX_POINT ( 'NONE', #19181 ) ;
#23386 = CARTESIAN_POINT ( 'NONE',  ( 25.90000000000000213, -14.06939075806902117, -20.80000000000000426 ) ) ;
#23387 = ADVANCED_FACE ( 'NONE', ( #12810 ), #62307, .F. ) ;
#23388 = CARTESIAN_POINT ( 'NONE',  ( -11.18071654964681372, -11.19368345035335821, 455.0000000000000568 ) ) ;
#23389 = CARTESIAN_POINT ( 'NONE',  ( 10.31452373788278187, 3.842976262117144159, 54.00000000000000711 ) ) ;
#23390 = ORIENTED_EDGE ( 'NONE', *, *, #36008, .T. ) ;
#23391 = AXIS2_PLACEMENT_3D ( 'NONE', #20132, #57258, #63268 ) ;
#23392 = ORIENTED_EDGE ( 'NONE', *, *, #56515, .F. ) ;
#23393 = EDGE_CURVE ( 'NONE', #36809, #39691, #3627, .T. ) ;
#23394 = CARTESIAN_POINT ( 'NONE',  ( 7.450000000000003730, -7.249999999999997335, -19.50000000000000000 ) ) ;
#23395 = ADVANCED_FACE ( 'NONE', ( #51718 ), #14230, .F. ) ;
#23396 = CARTESIAN_POINT ( 'NONE',  ( 0.000000000000000000, -20.50000000000000000, 17.79289321881345032 ) ) ;
#23397 = EDGE_CURVE ( 'NONE', #58971, #66435, #27908, .T. ) ;
#23398 = ORIENTED_EDGE ( 'NONE', *, *, #40087, .T. ) ;
#23399 = ORIENTED_EDGE ( 'NONE', *, *, #55194, .F. ) ;
#23400 = VECTOR ( 'NONE', #64295, 1000.000000000000000 ) ;
#23401 = VECTOR ( 'NONE', #4229, 1000.000000000000000 ) ;
#23403 = CARTESIAN_POINT ( 'NONE',  ( -11.50000000000000000, -11.70000000000012008, 10.70000000000011831 ) ) ;
#23402 = VECTOR ( 'NONE', #53962, 1000.000000000000000 ) ;
#23404 = ADVANCED_FACE ( 'NONE', ( #46398 ), #44998, .F. ) ;
#23405 = EDGE_CURVE ( 'NONE', #47564, #7150, #67625, .T. ) ;
#23406 = LINE ( 'NONE', #18787, #56012 ) ;
#23407 = VERTEX_POINT ( 'NONE', #29432 ) ;
#23408 = CIRCLE ( 'NONE', #45966, 0.1999999999999987899 ) ;
#23409 = VECTOR ( 'NONE', #27415, 1000.000000000000000 ) ;
#23410 = VECTOR ( 'NONE', #20671, 1000.000000000000000 ) ;
#23411 = CARTESIAN_POINT ( 'NONE',  ( 7.250000000000005329, -7.249999999999998224, -23.50000000000000000 ) ) ;
#23412 = ORIENTED_EDGE ( 'NONE', *, *, #50464, .F. ) ;
#23413 = ORIENTED_EDGE ( 'NONE', *, *, #59572, .F. ) ;
#23414 = CARTESIAN_POINT ( 'NONE',  ( 39.90000000000000568, 14.08845687959340331, 21.00000000000000000 ) ) ;
#23415 = VECTOR ( 'NONE', #60639, 1000.000000000000000 ) ;
#23416 = DIRECTION ( 'NONE',  ( 0.000000000000000000, 1.000000000000000000, 0.000000000000000000 ) ) ;
#23417 = VECTOR ( 'NONE', #59737, 1000.000000000000000 ) ;
#23418 = FACE_OUTER_BOUND ( 'NONE', #25752, .T. ) ;
#23419 = DIRECTION ( 'NONE',  ( 0.000000000000000000, 0.000000000000000000, 1.000000000000000000 ) ) ;
#23420 = DIRECTION ( 'NONE',  ( -1.000000000000000000, 0.000000000000000000, 0.000000000000000000 ) ) ;
#23421 = DIRECTION ( 'NONE',  ( 1.000000000000000000, 0.000000000000000000, 0.000000000000000000 ) ) ;
#23422 = CARTESIAN_POINT ( 'NONE',  ( 7.450000000000003730, -7.249999999999997335, -16.00000000000000000 ) ) ;
#23423 = ORIENTED_EDGE ( 'NONE', *, *, #42532, .T. ) ;
#23424 = CARTESIAN_POINT ( 'NONE',  ( 7.250000000000004441, 7.450000000000001954, -18.50000000000000000 ) ) ;
#23426 = EDGE_LOOP ( 'NONE', ( #24603, #18041, #45133, #973 ) ) ;
#23425 = PLANE ( 'NONE',  #12957 ) ;
#23427 = AXIS2_PLACEMENT_3D ( 'NONE', #32485, #44444, #48390 ) ;
#23428 = CARTESIAN_POINT ( 'NONE',  ( -11.50000000000000000, -11.50000000000100009, 10.50000000000065903 ) ) ;
#23429 = DIRECTION ( 'NONE',  ( -1.047444401652940007E-14, -1.000000000000000000, 0.000000000000000000 ) ) ;
#23430 = DIRECTION ( 'NONE',  ( 0.000000000000000000, 1.000000000000000000, 0.000000000000000000 ) ) ;
#23431 = DIRECTION ( 'NONE',  ( -1.000000000000000000, 0.000000000000000000, 0.000000000000000000 ) ) ;
#23432 = CARTESIAN_POINT ( 'NONE',  ( 15.50000000000000000, -0.4000000000005274892, -22.50000000000000000 ) ) ;
#23433 = ORIENTED_EDGE ( 'NONE', *, *, #55599, .F. ) ;
#23434 = ORIENTED_EDGE ( 'NONE', *, *, #47854, .F. ) ;
#23435 = DIRECTION ( 'NONE',  ( -1.000000000000000000, -1.084202172485504434E-16, 0.000000000000000000 ) ) ;
#23436 = PLANE ( 'NONE',  #26619 ) ;
#23437 = ADVANCED_FACE ( 'NONE', ( #35080 ), #35430, .T. ) ;
#23438 = PLANE ( 'NONE',  #21764 ) ;
#23439 = EDGE_LOOP ( 'NONE', ( #10268, #7112, #50658, #18343 ) ) ;
#23440 = CARTESIAN_POINT ( 'NONE',  ( -9.189999999999999503, 9.750000000000000000, -5.000000000000000000 ) ) ;
#23441 = ORIENTED_EDGE ( 'NONE', *, *, #879, .F. ) ;
#23442 = AXIS2_PLACEMENT_3D ( 'NONE', #46388, #7154, #23435 ) ;
#23443 = EDGE_CURVE ( 'NONE', #11065, #8763, #8563, .T. ) ;
#23444 = ORIENTED_EDGE ( 'NONE', *, *, #46795, .T. ) ;
#23445 = DIRECTION ( 'NONE',  ( 0.000000000000000000, 0.000000000000000000, 1.000000000000000000 ) ) ;
#23446 = DIRECTION ( 'NONE',  ( 0.000000000000000000, 1.000000000000000000, 0.000000000000000000 ) ) ;
#23447 = VERTEX_POINT ( 'NONE', #61598 ) ;
#23448 = FACE_OUTER_BOUND ( 'NONE', #51614, .T. ) ;
#23449 = AXIS2_PLACEMENT_3D ( 'NONE', #16195, #1320, #6954 ) ;
#23450 = LINE ( 'NONE', #29436, #36593 ) ;
#23451 = CARTESIAN_POINT ( 'NONE',  ( 8.900000000000005684, -14.06939075806900874, 20.80000000000001137 ) ) ;
#23452 = ORIENTED_EDGE ( 'NONE', *, *, #27172, .F. ) ;
#23454 = ORIENTED_EDGE ( 'NONE', *, *, #61880, .F. ) ;
#23453 = LINE ( 'NONE', #66582, #19279 ) ;
#23455 = CIRCLE ( 'NONE', #12141, 0.3000000000005412781 ) ;
#23456 = VECTOR ( 'NONE', #27676, 1000.000000000000000 ) ;
#23457 = DIRECTION ( 'NONE',  ( 1.000000000000000000, -0.000000000000000000, -0.000000000000000000 ) ) ;
#23458 = DIRECTION ( 'NONE',  ( 0.000000000000000000, 0.000000000000000000, -1.000000000000000000 ) ) ;
#23459 = CYLINDRICAL_SURFACE ( 'NONE', #62814, 24.99999999998794920 ) ;
#23460 = DIRECTION ( 'NONE',  ( -1.000000000000000000, 0.000000000000000000, 0.000000000000000000 ) ) ;
#23461 = AXIS2_PLACEMENT_3D ( 'NONE', #9162, #18347, #40629 ) ;
#23462 = VECTOR ( 'NONE', #61580, 1000.000000000000000 ) ;
#23464 = DIRECTION ( 'NONE',  ( 0.000000000000000000, 0.000000000000000000, -1.000000000000000000 ) ) ;
#23463 = AXIS2_PLACEMENT_3D ( 'NONE', #28162, #16523, #61015 ) ;
#23465 = DIRECTION ( 'NONE',  ( 1.836970198721029934E-16, 1.836970198721010706E-16, -1.000000000000000000 ) ) ;
#23466 = ORIENTED_EDGE ( 'NONE', *, *, #15952, .F. ) ;
#23467 = VERTEX_POINT ( 'NONE', #3269 ) ;
#23468 = ORIENTED_EDGE ( 'NONE', *, *, #40324, .T. ) ;
#23469 = CARTESIAN_POINT ( 'NONE',  ( 47.00000000000000000, 0.7500000000000000000, 3.418698582794334584 ) ) ;
#23470 = CARTESIAN_POINT ( 'NONE',  ( 4.740315990920191958, 4.188533722949208560, 455.0000000000000568 ) ) ;
#23471 = DIRECTION ( 'NONE',  ( 1.000000000000000000, -1.088659024508174415E-14, 1.836970198721009966E-16 ) ) ;
#23472 = CARTESIAN_POINT ( 'NONE',  ( 0.000000000000000000, 0.000000000000000000, 0.000000000000000000 ) ) ;
#23473 = EDGE_CURVE ( 'NONE', #42663, #47684, #18831, .T. ) ;
#23474 = ORIENTED_EDGE ( 'NONE', *, *, #5221, .T. ) ;
#23475 = EDGE_LOOP ( 'NONE', ( #15649, #15478, #8244, #10327 ) ) ;
#23476 = ORIENTED_EDGE ( 'NONE', *, *, #28835, .F. ) ;
#23477 = CYLINDRICAL_SURFACE ( 'NONE', #32811, 24.99999999998794920 ) ;
#23478 = EDGE_LOOP ( 'NONE', ( #36718, #56184, #65500, #52691 ) ) ;
#23479 = ORIENTED_EDGE ( 'NONE', *, *, #11430, .F. ) ;
#23480 = EDGE_CURVE ( 'NONE', #127, #33326, #19525, .T. ) ;
#23481 = ADVANCED_FACE ( 'NONE', ( #23787 ), #67974, .F. ) ;
#23482 = ORIENTED_EDGE ( 'NONE', *, *, #49667, .T. ) ;
#23483 = ORIENTED_EDGE ( 'NONE', *, *, #38452, .F. ) ;
#23484 = DIRECTION ( 'NONE',  ( 0.000000000000000000, 0.000000000000000000, -1.000000000000000000 ) ) ;
#23485 = EDGE_CURVE ( 'NONE', #9508, #26490, #16665, .T. ) ;
#23486 = EDGE_CURVE ( 'NONE', #68001, #13851, #34738, .T. ) ;
#23488 = ORIENTED_EDGE ( 'NONE', *, *, #16896, .T. ) ;
#23487 = CARTESIAN_POINT ( 'NONE',  ( 7.186223737882800222, 5.242976262117193365, 54.00000000000000711 ) ) ;
#23489 = CARTESIAN_POINT ( 'NONE',  ( 46.39999999999999858, 21.00000000000000000, -2.250000000000000444 ) ) ;
#23490 = DIRECTION ( 'NONE',  ( 0.000000000000000000, 1.000000000000000000, 0.000000000000000000 ) ) ;
#23491 = EDGE_CURVE ( 'NONE', #37646, #25470, #7860, .T. ) ;
#23492 = LINE ( 'NONE', #13577, #38165 ) ;
#23493 = VECTOR ( 'NONE', #69366, 1000.000000000000000 ) ;
#23495 = ORIENTED_EDGE ( 'NONE', *, *, #41114, .T. ) ;
#23494 = CARTESIAN_POINT ( 'NONE',  ( -11.00000000000000000, -9.454754784057099570, 17.53999999999999915 ) ) ;
#23496 = ORIENTED_EDGE ( 'NONE', *, *, #68175, .T. ) ;
#23497 = DIRECTION ( 'NONE',  ( 1.000000000000000000, 0.000000000000000000, 0.000000000000000000 ) ) ;
#23498 = CYLINDRICAL_SURFACE ( 'NONE', #63908, 1.000000000000000000 ) ;
#23499 = PLANE ( 'NONE',  #50765 ) ;
#23500 = ORIENTED_EDGE ( 'NONE', *, *, #45403, .T. ) ;
#23501 = LINE ( 'NONE', #51066, #15655 ) ;
#23502 = AXIS2_PLACEMENT_3D ( 'NONE', #48771, #32852, #10585 ) ;
#23503 = FACE_OUTER_BOUND ( 'NONE', #51824, .T. ) ;
#23504 = DIRECTION ( 'NONE',  ( -1.000000000000000000, 0.000000000000000000, 0.000000000000000000 ) ) ;
#23505 = ORIENTED_EDGE ( 'NONE', *, *, #21550, .F. ) ;
#23506 = FACE_OUTER_BOUND ( 'NONE', #59486, .T. ) ;
#23507 = CARTESIAN_POINT ( 'NONE',  ( 11.00000000000000000, -17.14999999999900027, 27.00000000000000000 ) ) ;
#23508 = LINE ( 'NONE', #34802, #22381 ) ;
#23509 = VERTEX_POINT ( 'NONE', #52788 ) ;
#23510 = CARTESIAN_POINT ( 'NONE',  ( 30.00000000000000000, -9.199999999999999289, -12.69999999999986073 ) ) ;
#23511 = CYLINDRICAL_SURFACE ( 'NONE', #49751, 0.3499999999999996447 ) ;
#23512 = FACE_OUTER_BOUND ( 'NONE', #37057, .T. ) ;
#23513 = DIRECTION ( 'NONE',  ( -1.836970198721029934E-16, 1.836970198721036344E-16, -1.000000000000000000 ) ) ;
#23514 = AXIS2_PLACEMENT_3D ( 'NONE', #39074, #13596, #7228 ) ;
#23515 = ORIENTED_EDGE ( 'NONE', *, *, #28482, .T. ) ;
#23516 = DIRECTION ( 'NONE',  ( 0.000000000000000000, 0.000000000000000000, 1.000000000000000000 ) ) ;
#23517 = PLANE ( 'NONE',  #38789 ) ;
#23518 = CARTESIAN_POINT ( 'NONE',  ( 283.0000000000000568, -37.15000000000001279, -7.700000000000000178 ) ) ;
#23519 = EDGE_CURVE ( 'NONE', #4367, #46404, #29103, .T. ) ;
#23520 = ADVANCED_FACE ( 'NONE', ( #5023 ), #69022, .F. ) ;
#23521 = EDGE_CURVE ( 'NONE', #17119, #56196, #25190, .T. ) ;
#23522 = DIRECTION ( 'NONE',  ( -1.000000000000000000, 0.000000000000000000, 0.000000000000000000 ) ) ;
#23523 = LINE ( 'NONE', #12550, #46542 ) ;
#23524 = ORIENTED_EDGE ( 'NONE', *, *, #30536, .F. ) ;
#23525 = CARTESIAN_POINT ( 'NONE',  ( -14.45366306705349224, -0.2717122460102528447, -21.66072723692568402 ) ) ;
#23526 = DIRECTION ( 'NONE',  ( -1.000000000000000000, 0.000000000000000000, 0.000000000000000000 ) ) ;
#23527 = DIRECTION ( 'NONE',  ( 1.000000000000000000, 0.000000000000000000, 0.000000000000000000 ) ) ;
#23528 = EDGE_CURVE ( 'NONE', #15458, #22255, #14577, .T. ) ;
#23529 = DIRECTION ( 'NONE',  ( 1.836970198721029934E-16, 1.836970198721010706E-16, -1.000000000000000000 ) ) ;
#23530 = PLANE ( 'NONE',  #68947 ) ;
#23531 = ORIENTED_EDGE ( 'NONE', *, *, #27274, .T. ) ;
#23533 = ORIENTED_EDGE ( 'NONE', *, *, #56636, .T. ) ;
#23532 = CARTESIAN_POINT ( 'NONE',  ( 0.5000000000000000000, 0.000000000000000000, 26.50000000000000000 ) ) ;
#23534 = CARTESIAN_POINT ( 'NONE',  ( -11.75000000000000000, -5.000000000000000000, 11.75000000000000000 ) ) ;
#23535 = CARTESIAN_POINT ( 'NONE',  ( 9.899999999999998579, -0.1999999999911430404, -8.864436962241481021E-12 ) ) ;
#23536 = ORIENTED_EDGE ( 'NONE', *, *, #53073, .T. ) ;
#23537 = CARTESIAN_POINT ( 'NONE',  ( 283.0000000000000568, -32.45000000000000995, -12.69999999999999929 ) ) ;
#23538 = ORIENTED_EDGE ( 'NONE', *, *, #35555, .F. ) ;
#23539 = CARTESIAN_POINT ( 'NONE',  ( 25.57999999999999829, 0.000000000000000000, 0.000000000000000000 ) ) ;
#23540 = VERTEX_POINT ( 'NONE', #36866 ) ;
#23541 = ORIENTED_EDGE ( 'NONE', *, *, #26296, .F. ) ;
#23542 = DIRECTION ( 'NONE',  ( 0.000000000000000000, 0.000000000000000000, 1.000000000000000000 ) ) ;
#23543 = DIRECTION ( 'NONE',  ( -1.000000000000000000, 0.000000000000000000, 0.000000000000000000 ) ) ;
#23544 = VECTOR ( 'NONE', #66584, 1000.000000000000000 ) ;
#23545 = PLANE ( 'NONE',  #51924 ) ;
#23547 =( BOUNDED_CURVE ( )  B_SPLINE_CURVE ( 3, ( #22766, #12488, #18145, #1535 ),
 .UNSPECIFIED., .F., .F. ) 
 B_SPLINE_CURVE_WITH_KNOTS ( ( 4, 4 ),
 ( 5.387520513321721438, 5.560451059366169346 ),
 .UNSPECIFIED. ) 
 CURVE ( )  GEOMETRIC_REPRESENTATION_ITEM ( )  RATIONAL_B_SPLINE_CURVE ( ( 1.000000000000000000, 0.9975094710839674805, 0.9975094710839674805, 1.000000000000000000 ) ) 
 REPRESENTATION_ITEM ( '' )  );
#23546 = CARTESIAN_POINT ( 'NONE',  ( -5.993516549646711766, 5.993516549646603409, 195.0000000000000284 ) ) ;
#23548 = ORIENTED_EDGE ( 'NONE', *, *, #5693, .T. ) ;
#23549 = EDGE_LOOP ( 'NONE', ( #5935, #63999, #22967, #54912 ) ) ;
#23550 = DIRECTION ( 'NONE',  ( 0.000000000000000000, 1.000000000000000000, 0.000000000000000000 ) ) ;
#23551 = AXIS2_PLACEMENT_3D ( 'NONE', #45755, #51415, #19242 ) ;
#23552 = LINE ( 'NONE', #12926, #27119 ) ;
#23553 = ORIENTED_EDGE ( 'NONE', *, *, #69952, .F. ) ;
#23554 = ORIENTED_EDGE ( 'NONE', *, *, #50061, .F. ) ;
#23555 = ORIENTED_EDGE ( 'NONE', *, *, #4609, .F. ) ;
#23556 = DIRECTION ( 'NONE',  ( -1.000000000000000000, 0.000000000000000000, 0.000000000000000000 ) ) ;
#23558 = EDGE_LOOP ( 'NONE', ( #31416, #45995, #42623, #41411 ) ) ;
#23557 = DIRECTION ( 'NONE',  ( 0.000000000000000000, -3.673940397442059868E-16, 1.000000000000000000 ) ) ;
#23559 = EDGE_CURVE ( 'NONE', #28681, #31048, #37210, .T. ) ;
#23560 = CIRCLE ( 'NONE', #20144, 0.3999999999999993006 ) ;
#23561 = CARTESIAN_POINT ( 'NONE',  ( -8.250000000000001776, -8.249999999999998224, -26.00000000000001066 ) ) ;
#23562 = DIRECTION ( 'NONE',  ( 0.000000000000000000, 0.000000000000000000, 1.000000000000000000 ) ) ;
#23563 = EDGE_CURVE ( 'NONE', #44820, #57287, #51676, .T. ) ;
#23564 = EDGE_CURVE ( 'NONE', #12532, #49486, #63022, .T. ) ;
#23565 = ORIENTED_EDGE ( 'NONE', *, *, #14774, .T. ) ;
#23566 = EDGE_LOOP ( 'NONE', ( #3482, #12691, #46249, #17575 ) ) ;
#23567 = ADVANCED_FACE ( 'NONE', ( #9988, #63374 ), #41796, .T. ) ;
#23568 = FACE_OUTER_BOUND ( 'NONE', #12494, .T. ) ;
#23569 = CARTESIAN_POINT ( 'NONE',  ( -7.259684009079963474, -4.201500623656036382, 455.0000000000000568 ) ) ;
#23570 = EDGE_CURVE ( 'NONE', #44289, #58177, #53824, .T. ) ;
#23571 = PLANE ( 'NONE',  #16857 ) ;
#23572 = EDGE_CURVE ( 'NONE', #61504, #34324, #58435, .T. ) ;
#23573 = DIRECTION ( 'NONE',  ( 0.000000000000000000, 0.000000000000000000, -1.000000000000000000 ) ) ;
#23574 = CARTESIAN_POINT ( 'NONE',  ( 11.00000000000000000, -11.50000000000100009, 10.50000000000065903 ) ) ;
#23575 = ORIENTED_EDGE ( 'NONE', *, *, #15900, .F. ) ;
#23576 = ORIENTED_EDGE ( 'NONE', *, *, #69592, .F. ) ;
#23577 = DIRECTION ( 'NONE',  ( -1.836970198721029934E-16, 1.836970198721036590E-16, -1.000000000000000000 ) ) ;
#23578 = CARTESIAN_POINT ( 'NONE',  ( 49.00000000000000000, -0.2000000000089119934, 8.909539772616881237E-12 ) ) ;
#23579 = LINE ( 'NONE', #29932, #8786 ) ;
#23580 = AXIS2_PLACEMENT_3D ( 'NONE', #68788, #58541, #8686 ) ;
#23581 = CARTESIAN_POINT ( 'NONE',  ( 10.31452373788281562, -6.657023737882825642, 54.00000000000000711 ) ) ;
#23582 = ORIENTED_EDGE ( 'NONE', *, *, #38895, .T. ) ;
#23583 = CARTESIAN_POINT ( 'NONE',  ( 290.0000000000000000, -42.00000000000000000, 26.50000000000000000 ) ) ;
#23584 = CARTESIAN_POINT ( 'NONE',  ( 7.450000000000004619, -1.336933437520057563E-15, -25.50000000000000355 ) ) ;
#23585 = DIRECTION ( 'NONE',  ( 0.000000000000000000, 0.000000000000000000, -1.000000000000000000 ) ) ;
#23586 = AXIS2_PLACEMENT_3D ( 'NONE', #38264, #54870, #48869 ) ;
#23587 = CYLINDRICAL_SURFACE ( 'NONE', #14169, 4.000000000000000000 ) ;
#23588 = CARTESIAN_POINT ( 'NONE',  ( 11.18999999999999950, 11.18999999999999950, -4.250000000000000000 ) ) ;
#23589 = DIRECTION ( 'NONE',  ( 1.836970198721029934E-16, 1.836970198721010706E-16, -1.000000000000000000 ) ) ;
#23590 = DIRECTION ( 'NONE',  ( 1.000000000000000000, 0.000000000000000000, 0.000000000000000000 ) ) ;
#23591 = ORIENTED_EDGE ( 'NONE', *, *, #2716, .T. ) ;
#23592 = CARTESIAN_POINT ( 'NONE',  ( -3.842976262117221875, 10.30047626211716860, 54.00000000000000711 ) ) ;
#23593 = CARTESIAN_POINT ( 'NONE',  ( -7.250000000000000000, -7.449999999999998401, -23.50000000000000000 ) ) ;
#23594 = ORIENTED_EDGE ( 'NONE', *, *, #47761, .F. ) ;
#23595 = DIRECTION ( 'NONE',  ( 0.000000000000000000, -1.000000000000000000, 0.000000000000000000 ) ) ;
#23596 = CARTESIAN_POINT ( 'NONE',  ( 7.000000000000000000, -26.42999999999999972, -9.412893218813501051 ) ) ;
#23597 = EDGE_CURVE ( 'NONE', #19158, #57625, #880, .T. ) ;
#23598 = CIRCLE ( 'NONE', #20233, 0.2000000000000005107 ) ;
#23599 = CARTESIAN_POINT ( 'NONE',  ( 8.835729544836290472, 2.530476262117160591, 54.00000000000000711 ) ) ;
#23600 = DIRECTION ( 'NONE',  ( -0.6414496315691617934, -0.7671651518152962090, -2.818519042763987834E-16 ) ) ;
#23601 = CARTESIAN_POINT ( 'NONE',  ( -11.77351654964679106, -7.606483450353366038, 455.0000000000000568 ) ) ;
#23602 = EDGE_LOOP ( 'NONE', ( #3280, #46266, #28348, #34303 ) ) ;
#23604 = VECTOR ( 'NONE', #39477, 1000.000000000000000 ) ;
#23603 = VECTOR ( 'NONE', #3090, 1000.000000000000000 ) ;
#23605 = DIRECTION ( 'NONE',  ( 0.8660254037844375974, -0.5000000000000019984, 0.000000000000000000 ) ) ;
#23606 = ORIENTED_EDGE ( 'NONE', *, *, #27971, .T. ) ;
#23607 = CARTESIAN_POINT ( 'NONE',  ( -8.566576262117260754, 8.916576262117214213, 54.00000000000000711 ) ) ;
#23608 = ORIENTED_EDGE ( 'NONE', *, *, #23632, .T. ) ;
#23609 = DIRECTION ( 'NONE',  ( 1.000000000000000000, -0.000000000000000000, 1.224646799147353207E-16 ) ) ;
#23610 = VECTOR ( 'NONE', #63704, 1000.000000000000000 ) ;
#23611 = EDGE_CURVE ( 'NONE', #4446, #8645, #26245, .T. ) ;
#23612 = DIRECTION ( 'NONE',  ( 1.000000000000000000, 0.000000000000000000, 0.000000000000000000 ) ) ;
#23613 = EDGE_CURVE ( 'NONE', #21626, #23904, #14429, .T. ) ;
#23614 = LINE ( 'NONE', #50832, #49225 ) ;
#23615 = ORIENTED_EDGE ( 'NONE', *, *, #9436, .T. ) ;
#23616 = ORIENTED_EDGE ( 'NONE', *, *, #49909, .F. ) ;
#23617 = CARTESIAN_POINT ( 'NONE',  ( 7.000000000000000000, -39.79999999999954952, -8.900000000000419575 ) ) ;
#23618 = ORIENTED_EDGE ( 'NONE', *, *, #19975, .T. ) ;
#23619 = ORIENTED_EDGE ( 'NONE', *, *, #48647, .F. ) ;
#23620 = CARTESIAN_POINT ( 'NONE',  ( 17.89999999999999858, -21.00000000000001421, -13.86939075806900945 ) ) ;
#23621 = CARTESIAN_POINT ( 'NONE',  ( -4.947141984184481700, 7.342976262117180575, 54.00000000000000711 ) ) ;
#23622 = CARTESIAN_POINT ( 'NONE',  ( 11.50000000000000000, -11.50000000000100009, 15.00000000000084910 ) ) ;
#23623 = CIRCLE ( 'NONE', #10120, 2.215251240775983899 ) ;
#23624 = ORIENTED_EDGE ( 'NONE', *, *, #57962, .T. ) ;
#23625 = DIRECTION ( 'NONE',  ( -9.912705577010336396E-15, -1.000000000000000000, 0.000000000000000000 ) ) ;
#23627 = CARTESIAN_POINT ( 'NONE',  ( -24.00000000000000000, -15.50000000000000000, 2.000000000000000000 ) ) ;
#23626 = CARTESIAN_POINT ( 'NONE',  ( 78.77321854994620765, 47.95351654967443977, 29.00000000000000000 ) ) ;
#23628 = VERTEX_POINT ( 'NONE', #64093 ) ;
#23630 = VERTEX_POINT ( 'NONE', #15642 ) ;
#23629 = LINE ( 'NONE', #23289, #37653 ) ;
#23631 = ORIENTED_EDGE ( 'NONE', *, *, #37882, .T. ) ;
#23632 = EDGE_CURVE ( 'NONE', #9398, #17833, #10329, .T. ) ;
#23633 = VECTOR ( 'NONE', #23909, 1000.000000000000000 ) ;
#23634 = CARTESIAN_POINT ( 'NONE',  ( -164.0134625397179207, 11.99351654964650216, 16.17170636239081816 ) ) ;
#23635 = CARTESIAN_POINT ( 'NONE',  ( -7.250000000000000888, -8.249999999999998224, -9.000000000000001776 ) ) ;
#23636 = AXIS2_PLACEMENT_3D ( 'NONE', #34830, #34469, #40128 ) ;
#23637 = AXIS2_PLACEMENT_3D ( 'NONE', #27909, #12306, #21560 ) ;
#23638 = VERTEX_POINT ( 'NONE', #21290 ) ;
#23639 = CYLINDRICAL_SURFACE ( 'NONE', #64170, 0.5000000000009302559 ) ;
#23640 = DIRECTION ( 'NONE',  ( -1.000000000000000000, 0.000000000000000000, 0.000000000000000000 ) ) ;
#23641 = EDGE_CURVE ( 'NONE', #52042, #68236, #4304, .T. ) ;
#23642 = ORIENTED_EDGE ( 'NONE', *, *, #45744, .F. ) ;
#23643 = ORIENTED_EDGE ( 'NONE', *, *, #18453, .F. ) ;
#23644 = VECTOR ( 'NONE', #59439, 1000.000000000000000 ) ;
#23645 = DIRECTION ( 'NONE',  ( -1.000000000000000000, 0.000000000000000000, 0.000000000000000000 ) ) ;
#23646 = LINE ( 'NONE', #45211, #1856 ) ;
#23647 = ADVANCED_FACE ( 'NONE', ( #36137 ), #41451, .T. ) ;
#23648 = EDGE_LOOP ( 'NONE', ( #42782, #45549, #38823, #40625 ) ) ;
#23649 = AXIS2_PLACEMENT_3D ( 'NONE', #52493, #58141, #4060 ) ;
#23650 = CARTESIAN_POINT ( 'NONE',  ( 8.250000000000005329, 7.250000000000000888, -14.00000000000000000 ) ) ;
#23651 = DIRECTION ( 'NONE',  ( 1.047444401652940007E-14, 1.000000000000000000, 1.836970198721029934E-16 ) ) ;
#23652 = EDGE_CURVE ( 'NONE', #57801, #47666, #52418, .T. ) ;
#23653 = CARTESIAN_POINT ( 'NONE',  ( 32.89999999999999858, -0.2000000000089119934, -8.913009219568841313E-12 ) ) ;
#23654 = ORIENTED_EDGE ( 'NONE', *, *, #14255, .F. ) ;
#23655 = EDGE_CURVE ( 'NONE', #30525, #50924, #59807, .T. ) ;
#23656 = AXIS2_PLACEMENT_3D ( 'NONE', #66310, #24217, #56736 ) ;
#23657 = DIRECTION ( 'NONE',  ( -1.000000000000000000, 0.000000000000000000, 0.000000000000000000 ) ) ;
#23658 = CARTESIAN_POINT ( 'NONE',  ( -7.252248008019455128, 6.606374702650072983, 455.0000000000000568 ) ) ;
#23659 = ORIENTED_EDGE ( 'NONE', *, *, #22469, .F. ) ;
#23661 = VERTEX_POINT ( 'NONE', #59463 ) ;
#23660 = CARTESIAN_POINT ( 'NONE',  ( 289.2330000000000041, 0.000000000000000000, 0.000000000000000000 ) ) ;
#23662 = CARTESIAN_POINT ( 'NONE',  ( -23.75054448485400016, -17.50000000000000000, 25.53140320652400064 ) ) ;
#23663 = AXIS2_PLACEMENT_3D ( 'NONE', #12864, #11831, #61306 ) ;
#23664 = DIRECTION ( 'NONE',  ( 1.000000000000000000, 1.671920889371702854E-15, 6.142537696789956391E-31 ) ) ;
#23665 = EDGE_CURVE ( 'NONE', #8340, #6513, #37902, .T. ) ;
#23666 = DIRECTION ( 'NONE',  ( 0.000000000000000000, 0.000000000000000000, -1.000000000000000000 ) ) ;
#23667 = CARTESIAN_POINT ( 'NONE',  ( -6.858227778582867806, 2.989207322240119868, 26.00000000000000711 ) ) ;
#23668 = CARTESIAN_POINT ( 'NONE',  ( -8.250000000000001776, -7.249999999999998224, -26.00000000000001066 ) ) ;
#23669 = VERTEX_POINT ( 'NONE', #43190 ) ;
#23670 = CARTESIAN_POINT ( 'NONE',  ( -30.00000000000000000, -12.00000000000000000, -10.20500000000000007 ) ) ;
#23671 = DIRECTION ( 'NONE',  ( 0.4999999999989410693, 0.000000000000000000, -0.8660254037850499964 ) ) ;
#23672 = DIRECTION ( 'NONE',  ( 1.000000000000000000, -4.121462285523434458E-16, 0.000000000000000000 ) ) ;
#23673 = ORIENTED_EDGE ( 'NONE', *, *, #23793, .T. ) ;
#23674 = CARTESIAN_POINT ( 'NONE',  ( 23.75054448485400016, -17.50000000000000000, -25.53140320652400064 ) ) ;
#23675 = AXIS2_PLACEMENT_3D ( 'NONE', #21404, #4799, #4460 ) ;
#23676 = ADVANCED_FACE ( 'NONE', ( #66143, #48507 ), #416, .T. ) ;
#23677 = CARTESIAN_POINT ( 'NONE',  ( 5.257023737882795977, 5.242976262117205799, 26.00000000000000711 ) ) ;
#23678 = ORIENTED_EDGE ( 'NONE', *, *, #19906, .T. ) ;
#23679 = FACE_OUTER_BOUND ( 'NONE', #47822, .T. ) ;
#23680 = DIRECTION ( 'NONE',  ( 0.000000000000000000, 0.000000000000000000, -1.000000000000000000 ) ) ;
#23681 = EDGE_LOOP ( 'NONE', ( #29974, #60530, #51585, #27150 ) ) ;
#23682 = EDGE_CURVE ( 'NONE', #10783, #5708, #8767, .T. ) ;
#23683 = LINE ( 'NONE', #12026, #24418 ) ;
#23684 = FACE_OUTER_BOUND ( 'NONE', #32543, .T. ) ;
#23685 = DIRECTION ( 'NONE',  ( 0.000000000000000000, 1.000000000000000000, 0.000000000000000000 ) ) ;
#23686 = APPLICATION_CONTEXT ( 'automotive_design' ) ;
#23687 = CYLINDRICAL_SURFACE ( 'NONE', #27104, 1.399999999999999245 ) ;
#23688 = VECTOR ( 'NONE', #14337, 1000.000000000000000 ) ;
#23689 = AXIS2_PLACEMENT_3D ( 'NONE', #43738, #10861, #54352 ) ;
#23690 = ADVANCED_FACE ( 'NONE', ( #49543, #38593 ), #21977, .F. ) ;
#23691 = CARTESIAN_POINT ( 'NONE',  ( 8.250000000000005329, -8.249999999999998224, -26.00000000000001066 ) ) ;
#23692 = AXIS2_PLACEMENT_3D ( 'NONE', #68138, #40557, #45868 ) ;
#23693 = ORIENTED_EDGE ( 'NONE', *, *, #16236, .F. ) ;
#23694 = DIRECTION ( 'NONE',  ( 0.000000000000000000, -1.000000000000000000, -3.673940397442060361E-16 ) ) ;
#23695 = ORIENTED_EDGE ( 'NONE', *, *, #9660, .T. ) ;
#23696 = EDGE_CURVE ( 'NONE', #48304, #23277, #44563, .T. ) ;
#23697 = ORIENTED_EDGE ( 'NONE', *, *, #18550, .T. ) ;
#23698 = AXIS2_PLACEMENT_3D ( 'NONE', #31454, #26140, #53019 ) ;
#23699 = LINE ( 'NONE', #61888, #37003 ) ;
#23700 = EDGE_CURVE ( 'NONE', #66129, #7579, #35874, .T. ) ;
#23701 = AXIS2_PLACEMENT_3D ( 'NONE', #66041, #49460, #43439 ) ;
#23702 = CYLINDRICAL_SURFACE ( 'NONE', #12891, 1.621000000000000885 ) ;
#23703 = EDGE_CURVE ( 'NONE', #9194, #6389, #6069, .T. ) ;
#23705 = CARTESIAN_POINT ( 'NONE',  ( -10.49297626211726175, 3.650476262117184234, 54.00000000000000711 ) ) ;
#23704 = DIRECTION ( 'NONE',  ( 0.000000000000000000, 0.000000000000000000, -1.000000000000000000 ) ) ;
#23706 = ORIENTED_EDGE ( 'NONE', *, *, #16421, .T. ) ;
#23707 = ORIENTED_EDGE ( 'NONE', *, *, #65636, .T. ) ;
#23708 = CIRCLE ( 'NONE', #63245, 0.1999999999999996503 ) ;
#23709 = CYLINDRICAL_SURFACE ( 'NONE', #5856, 0.3499999999998886224 ) ;
#23710 = ORIENTED_EDGE ( 'NONE', *, *, #6932, .T. ) ;
#23711 = VECTOR ( 'NONE', #3265, 1000.000000000000000 ) ;
#23712 = CARTESIAN_POINT ( 'NONE',  ( -11.31351654964674047, -4.206483450353332820, 455.0000000000000568 ) ) ;
#23713 = LINE ( 'NONE', #18394, #14022 ) ;
#23714 = CARTESIAN_POINT ( 'NONE',  ( -4.173516549646837603, -11.78648345035344214, 455.0000000000000568 ) ) ;
#23715 = EDGE_CURVE ( 'NONE', #56475, #803, #26947, .T. ) ;
#23716 = EDGE_CURVE ( 'NONE', #57835, #29890, #64120, .T. ) ;
#23717 = CARTESIAN_POINT ( 'NONE',  ( 3.606483450353369147, -7.428221114745003462, 195.0000000000000284 ) ) ;
#23718 = VECTOR ( 'NONE', #10041, 1000.000000000000000 ) ;
#23719 = VECTOR ( 'NONE', #12578, 1000.000000000000000 ) ;
#23721 = DIRECTION ( 'NONE',  ( -1.000000000000000000, 0.000000000000000000, 0.000000000000000000 ) ) ;
#23720 = CARTESIAN_POINT ( 'NONE',  ( 7.000000000000000000, -39.80000000000000426, 8.400000000000000355 ) ) ;
#23722 = ORIENTED_EDGE ( 'NONE', *, *, #17366, .T. ) ;
#23725 = EDGE_CURVE ( 'NONE', #56183, #64226, #39273, .T. ) ;
#23724 = ORIENTED_EDGE ( 'NONE', *, *, #56609, .T. ) ;
#23723 = CARTESIAN_POINT ( 'NONE',  ( -4.193516549646833624, -11.32648345035344128, 455.0000000000000568 ) ) ;
#23726 = ORIENTED_EDGE ( 'NONE', *, *, #24528, .T. ) ;
#23727 = VERTEX_POINT ( 'NONE', #32598 ) ;
#23728 = EDGE_CURVE ( 'NONE', #21706, #62668, #22365, .T. ) ;
#23729 = ADVANCED_FACE ( 'NONE', ( #16687 ), #38253, .F. ) ;
#23730 = DIRECTION ( 'NONE',  ( 0.000000000000000000, 0.000000000000000000, 1.000000000000000000 ) ) ;
#23731 = EDGE_CURVE ( 'NONE', #32488, #48332, #47188, .T. ) ;
#23732 = LINE ( 'NONE', #67920, #55535 ) ;
#23733 = VECTOR ( 'NONE', #34939, 1000.000000000000000 ) ;
#23734 = EDGE_CURVE ( 'NONE', #29129, #26202, #55196, .T. ) ;
#23735 = ORIENTED_EDGE ( 'NONE', *, *, #53243, .T. ) ;
#23736 = VERTEX_POINT ( 'NONE', #44221 ) ;
#23737 = ADVANCED_FACE ( 'NONE', ( #1439 ), #65801, .F. ) ;
#23738 = CARTESIAN_POINT ( 'NONE',  ( 15.50000000000000000, -2.500000000000000000, 23.94337567297399971 ) ) ;
#23739 = DIRECTION ( 'NONE',  ( 0.000000000000000000, 0.000000000000000000, 1.000000000000000000 ) ) ;
#23740 = ORIENTED_EDGE ( 'NONE', *, *, #29111, .F. ) ;
#23741 = ORIENTED_EDGE ( 'NONE', *, *, #16783, .F. ) ;
#23742 = CARTESIAN_POINT ( 'NONE',  ( -10.73351654964671020, 1.677516549646603794, 455.0000000000000568 ) ) ;
#23743 = EDGE_CURVE ( 'NONE', #18330, #20587, #6743, .T. ) ;
#23744 = FACE_OUTER_BOUND ( 'NONE', #4866, .T. ) ;
#23745 = AXIS2_PLACEMENT_3D ( 'NONE', #32558, #48461, #21592 ) ;
#23746 = VERTEX_POINT ( 'NONE', #56235 ) ;
#23747 = EDGE_CURVE ( 'NONE', #67807, #20681, #2832, .T. ) ;
#23748 = VECTOR ( 'NONE', #53987, 1000.000000000000000 ) ;
#23749 = CARTESIAN_POINT ( 'NONE',  ( -7.793516549646712477, 11.31351654964660014, 195.0000000000000284 ) ) ;
#23750 = DIRECTION ( 'NONE',  ( -1.000000000000000000, 0.000000000000000000, 0.000000000000000000 ) ) ;
#23752 = EDGE_LOOP ( 'NONE', ( #75, #26966 ) ) ;
#23751 = DIRECTION ( 'NONE',  ( -0.000000000000000000, -0.000000000000000000, -1.000000000000000000 ) ) ;
#23753 = ORIENTED_EDGE ( 'NONE', *, *, #65792, .F. ) ;
#23754 = AXIS2_PLACEMENT_3D ( 'NONE', #33436, #59264, #49689 ) ;
#23755 = CYLINDRICAL_SURFACE ( 'NONE', #26523, 0.5249999999999994671 ) ;
#23756 = DIRECTION ( 'NONE',  ( 1.000000000000000000, -0.000000000000000000, 0.000000000000000000 ) ) ;
#23757 = PLANE ( 'NONE',  #5799 ) ;
#23758 = DIRECTION ( 'NONE',  ( -1.000000000000000000, 0.000000000000000000, 0.000000000000000000 ) ) ;
#23759 = DIRECTION ( 'NONE',  ( -1.000000000000000000, 1.794541526872559352E-16, 0.000000000000000000 ) ) ;
#23760 = AXIS2_PLACEMENT_3D ( 'NONE', #23878, #24927, #67706 ) ;
#23761 = CARTESIAN_POINT ( 'NONE',  ( 283.0000000000000568, -42.50000000000000000, -14.49999999999904077 ) ) ;
#23763 = CIRCLE ( 'NONE', #33900, 0.2000000000000005107 ) ;
#23762 = PLANE ( 'NONE',  #65431 ) ;
#23764 = ORIENTED_EDGE ( 'NONE', *, *, #8445, .T. ) ;
#23765 = DIRECTION ( 'NONE',  ( 0.8660254037844383745, 0.5000000000000005551, -0.000000000000000000 ) ) ;
#23767 = ORIENTED_EDGE ( 'NONE', *, *, #43236, .F. ) ;
#23766 = LINE ( 'NONE', #34352, #20913 ) ;
#23768 = CARTESIAN_POINT ( 'NONE',  ( -1.077516549646670541, 11.33351654964656596, 195.0000000000000284 ) ) ;
#23769 = CARTESIAN_POINT ( 'NONE',  ( 9.106483450353419329, 11.11351654964656710, 455.0000000000000568 ) ) ;
#23770 = CARTESIAN_POINT ( 'NONE',  ( -24.00000000000000000, -17.35230188589299871, 15.35019951917099945 ) ) ;
#23771 = LINE ( 'NONE', #1504, #49867 ) ;
#23772 = CIRCLE ( 'NONE', #53185, 3.499999999999999556 ) ;
#23773 = VECTOR ( 'NONE', #14969, 1000.000000000000000 ) ;
#23774 = CARTESIAN_POINT ( 'NONE',  ( 30.00000000000000000, -5.200000000000001066, -9.400000000000000355 ) ) ;
#23775 = ORIENTED_EDGE ( 'NONE', *, *, #63237, .F. ) ;
#23776 = ORIENTED_EDGE ( 'NONE', *, *, #13487, .T. ) ;
#23777 = CARTESIAN_POINT ( 'NONE',  ( 9.899999999999998579, 20.60000000000000142, -13.86939075806900057 ) ) ;
#23778 = DIRECTION ( 'NONE',  ( 0.000000000000000000, 0.000000000000000000, 1.000000000000000000 ) ) ;
#23779 = EDGE_CURVE ( 'NONE', #49938, #32123, #66488, .T. ) ;
#23780 = DIRECTION ( 'NONE',  ( -1.000000000000000000, 9.799566706031580591E-15, 1.836970198721048176E-16 ) ) ;
#23781 = EDGE_LOOP ( 'NONE', ( #4088, #28730, #47134, #42071 ) ) ;
#23782 = VECTOR ( 'NONE', #47665, 1000.000000000000000 ) ;
#23783 = CARTESIAN_POINT ( 'NONE',  ( 39.00000000000000000, -21.00000000000000000, 16.96999999999999886 ) ) ;
#23784 = ORIENTED_EDGE ( 'NONE', *, *, #28044, .F. ) ;
#23785 = EDGE_CURVE ( 'NONE', #5610, #40926, #2136, .T. ) ;
#23786 = ORIENTED_EDGE ( 'NONE', *, *, #13063, .T. ) ;
#23787 = FACE_OUTER_BOUND ( 'NONE', #44501, .T. ) ;
#23788 = CYLINDRICAL_SURFACE ( 'NONE', #44363, 1.000000000000000000 ) ;
#23789 = ORIENTED_EDGE ( 'NONE', *, *, #16510, .T. ) ;
#23790 = DIRECTION ( 'NONE',  ( 0.7071067811865550112, 0.7071067811865401342, 2.597868168706466792E-16 ) ) ;
#23791 = EDGE_CURVE ( 'NONE', #31344, #58112, #13788, .T. ) ;
#23792 = DIRECTION ( 'NONE',  ( 1.000000000000000000, 0.000000000000000000, 0.000000000000000000 ) ) ;
#23793 = EDGE_CURVE ( 'NONE', #2123, #37879, #23699, .T. ) ;
#23794 = DIRECTION ( 'NONE',  ( 0.000000000000000000, 0.000000000000000000, -1.000000000000000000 ) ) ;
#23795 = ORIENTED_EDGE ( 'NONE', *, *, #52881, .F. ) ;
#23796 = ORIENTED_EDGE ( 'NONE', *, *, #32161, .F. ) ;
#23798 = ORIENTED_EDGE ( 'NONE', *, *, #69036, .T. ) ;
#23797 = PLANE ( 'NONE',  #38519 ) ;
#23799 = ORIENTED_EDGE ( 'NONE', *, *, #4814, .F. ) ;
#23800 = VECTOR ( 'NONE', #66097, 1000.000000000000000 ) ;
#23801 = CARTESIAN_POINT ( 'NONE',  ( 39.00000000000000000, -16.96999999999999886, -21.00000000000000000 ) ) ;
#23802 = DIRECTION ( 'NONE',  ( 1.000000000000000000, -3.491481338843133355E-15, -1.836970198721036344E-16 ) ) ;
#23803 = FACE_OUTER_BOUND ( 'NONE', #61611, .T. ) ;
#23804 = CARTESIAN_POINT ( 'NONE',  ( -8.250000000000001776, -7.249999999999998224, -23.00000000000000000 ) ) ;
#23805 = CIRCLE ( 'NONE', #2351, 0.5000000000000000000 ) ;
#23806 = CARTESIAN_POINT ( 'NONE',  ( 11.00000000000000000, -17.50000000000000000, -26.64999999999900027 ) ) ;
#23807 = ORIENTED_EDGE ( 'NONE', *, *, #11009, .T. ) ;
#23808 = ORIENTED_EDGE ( 'NONE', *, *, #1585, .T. ) ;
#23809 = ORIENTED_EDGE ( 'NONE', *, *, #23785, .T. ) ;
#23810 = CIRCLE ( 'NONE', #30581, 0.7499999999999997780 ) ;
#23811 = EDGE_CURVE ( 'NONE', #15112, #49163, #44924, .T. ) ;
#23812 = CIRCLE ( 'NONE', #63347, 0.3499999999999996447 ) ;
#23813 = ORIENTED_EDGE ( 'NONE', *, *, #17282, .T. ) ;
#23814 = CARTESIAN_POINT ( 'NONE',  ( -17.00000000000000000, -17.35230188589299516, -15.35019951917100478 ) ) ;
#23815 = LINE ( 'NONE', #45718, #51262 ) ;
#23816 = VECTOR ( 'NONE', #7869, 1000.000000000000000 ) ;
#23817 = CARTESIAN_POINT ( 'NONE',  ( 4.396432944014526889, -8.606483450353477949, 455.0000000000000568 ) ) ;
#23818 =( LENGTH_UNIT ( ) NAMED_UNIT ( * ) SI_UNIT ( .MILLI., .METRE. ) );
#23819 = CARTESIAN_POINT ( 'NONE',  ( 28.90000000000000213, -14.06939075806900874, 20.80000000000001137 ) ) ;
#23820 = ORIENTED_EDGE ( 'NONE', *, *, #47823, .F. ) ;
#23821 = ORIENTED_EDGE ( 'NONE', *, *, #45202, .F. ) ;
#23822 = VERTEX_POINT ( 'NONE', #7779 ) ;
#23823 = CARTESIAN_POINT ( 'NONE',  ( -8.821682069070741150, -2.369523737882737624, 26.00000000000000711 ) ) ;
#23824 = ORIENTED_EDGE ( 'NONE', *, *, #48662, .F. ) ;
#23825 = EDGE_LOOP ( 'NONE', ( #32071, #16882, #5939, #62904 ) ) ;
#23826 = ORIENTED_EDGE ( 'NONE', *, *, #56325, .F. ) ;
#23827 = VERTEX_POINT ( 'NONE', #14140 ) ;
#23828 = FACE_OUTER_BOUND ( 'NONE', #13207, .T. ) ;
#23829 = EDGE_CURVE ( 'NONE', #62902, #48603, #3197, .T. ) ;
#23831 = VERTEX_POINT ( 'NONE', #7084 ) ;
#23830 = DIRECTION ( 'NONE',  ( -1.000000000000000000, 0.000000000000000000, 0.000000000000000000 ) ) ;
#23832 = DIRECTION ( 'NONE',  ( -1.000000000000000000, 1.794541526872559352E-16, 0.000000000000000000 ) ) ;
#23833 = EDGE_CURVE ( 'NONE', #64699, #3316, #6515, .T. ) ;
#23834 = LINE ( 'NONE', #8259, #34061 ) ;
#23835 = DIRECTION ( 'NONE',  ( -0.000000000000000000, -0.000000000000000000, -1.000000000000000000 ) ) ;
#23836 = ADVANCED_FACE ( 'NONE', ( #50918 ), #24755, .F. ) ;
#23838 = ORIENTED_EDGE ( 'NONE', *, *, #52038, .T. ) ;
#23837 = PLANE ( 'NONE',  #63980 ) ;
#23839 = ORIENTED_EDGE ( 'NONE', *, *, #68346, .T. ) ;
#23840 = DIRECTION ( 'NONE',  ( -1.000000000000000000, 0.000000000000000000, 0.000000000000000000 ) ) ;
#23841 = LINE ( 'NONE', #50365, #18709 ) ;
#23842 = CARTESIAN_POINT ( 'NONE',  ( 9.106483450353369591, 10.08346604330778362, 195.0000000000000284 ) ) ;
#23843 = VECTOR ( 'NONE', #57416, 1000.000000000000000 ) ;
#23844 = VERTEX_POINT ( 'NONE', #45259 ) ;
#23845 = DIRECTION ( 'NONE',  ( -1.000000000000000000, 0.000000000000000000, 0.000000000000000000 ) ) ;
#23846 = CARTESIAN_POINT ( 'NONE',  ( -2.406732575409590069, 8.697938382363036069, 54.00000000000000711 ) ) ;
#23847 = AXIS2_PLACEMENT_3D ( 'NONE', #40710, #3236, #9592 ) ;
#23848 = DIRECTION ( 'NONE',  ( -0.3479852726768751237, 0.000000000000000000, 0.9375000000000004441 ) ) ;
#23849 = ORIENTED_EDGE ( 'NONE', *, *, #66895, .T. ) ;
#23851 = LINE ( 'NONE', #67349, #40315 ) ;
#23850 = CIRCLE ( 'NONE', #42892, 0.4999999999945519691 ) ;
#23852 = CARTESIAN_POINT ( 'NONE',  ( -2.693516549646675529, 10.91351654964657314, 195.0000000000000284 ) ) ;
#23853 = CARTESIAN_POINT ( 'NONE',  ( -10.30047626211729295, -6.657023737882751924, 54.00000000000000711 ) ) ;
#23854 = AXIS2_PLACEMENT_3D ( 'NONE', #57011, #30496, #41458 ) ;
#23855 = CIRCLE ( 'NONE', #35103, 2.000000000000001776 ) ;
#23856 = VERTEX_POINT ( 'NONE', #18745 ) ;
#23857 = CARTESIAN_POINT ( 'NONE',  ( -11.75000000000000000, -5.200000000000001066, -11.75000000000000000 ) ) ;
#23858 = CARTESIAN_POINT ( 'NONE',  ( 47.00000000000000000, 0.000000000000000000, 0.000000000000000000 ) ) ;
#23859 = DIRECTION ( 'NONE',  ( 0.000000000000000000, 0.000000000000000000, -1.000000000000000000 ) ) ;
#23860 = LINE ( 'NONE', #66992, #35656 ) ;
#23861 = EDGE_CURVE ( 'NONE', #68300, #36802, #23455, .T. ) ;
#23862 = ORIENTED_EDGE ( 'NONE', *, *, #10662, .F. ) ;
#23863 = CARTESIAN_POINT ( 'NONE',  ( 6.500000000000000888, -6.500000000000002665, -1.000000000000000000 ) ) ;
#23864 = CARTESIAN_POINT ( 'NONE',  ( -11.31351654964671027, 4.393516549646604652, 195.0000000000000284 ) ) ;
#23865 = CARTESIAN_POINT ( 'NONE',  ( 5.552858015815581361, -7.357023737882824044, 54.00000000000000711 ) ) ;
#23866 = EDGE_CURVE ( 'NONE', #28596, #12012, #50231, .T. ) ;
#23867 = VECTOR ( 'NONE', #60558, 1000.000000000000000 ) ;
#23868 = LINE ( 'NONE', #2644, #24474 ) ;
#23869 = LINE ( 'NONE', #45426, #27431 ) ;
#23870 = ORIENTED_EDGE ( 'NONE', *, *, #60447, .T. ) ;
#23871 = CARTESIAN_POINT ( 'NONE',  ( -4.141586236041130853, -5.793274621760842180, 54.00000000000000711 ) ) ;
#23872 = CARTESIAN_POINT ( 'NONE',  ( 11.50000000000000000, -11.50000000000100009, 19.50000000000103739 ) ) ;
#23873 = EDGE_CURVE ( 'NONE', #35140, #66944, #7435, .T. ) ;
#23874 = EDGE_CURVE ( 'NONE', #54299, #11406, #45973, .T. ) ;
#23875 = FACE_OUTER_BOUND ( 'NONE', #66332, .T. ) ;
#23876 = CARTESIAN_POINT ( 'NONE',  ( 283.0000000000000568, -25.69999999999924967, -14.52500000000000213 ) ) ;
#23877 = EDGE_CURVE ( 'NONE', #6538, #23628, #51269, .T. ) ;
#23878 = CARTESIAN_POINT ( 'NONE',  ( -7.250000000000000888, 7.250000000000001776, -12.50000000000000000 ) ) ;
#23879 = EDGE_CURVE ( 'NONE', #68528, #41558, #8124, .T. ) ;
#23880 = ORIENTED_EDGE ( 'NONE', *, *, #24319, .T. ) ;
#23882 = VERTEX_POINT ( 'NONE', #40664 ) ;
#23881 = DIRECTION ( 'NONE',  ( 0.000000000000000000, 0.000000000000000000, 1.000000000000000000 ) ) ;
#23883 = EDGE_CURVE ( 'NONE', #14054, #61969, #31456, .T. ) ;
#23884 = PLANE ( 'NONE',  #20273 ) ;
#23885 = VECTOR ( 'NONE', #42274, 1000.000000000000000 ) ;
#23886 = CARTESIAN_POINT ( 'NONE',  ( 283.0000000000000568, -32.44999999999905071, -13.20000000000091944 ) ) ;
#23887 = EDGE_LOOP ( 'NONE', ( #6151, #15962, #48857, #43313 ) ) ;
#23888 = CARTESIAN_POINT ( 'NONE',  ( -3.593516549646701197, 7.415254214038210279, 455.0000000000000568 ) ) ;
#23889 = ORIENTED_EDGE ( 'NONE', *, *, #64928, .T. ) ;
#23890 = PLANE ( 'NONE',  #45863 ) ;
#23891 = ORIENTED_EDGE ( 'NONE', *, *, #15726, .T. ) ;
#23892 = EDGE_LOOP ( 'NONE', ( #54362, #62473, #26022, #3665 ) ) ;
#23893 = CARTESIAN_POINT ( 'NONE',  ( 19.90000000000000213, -21.00000000000000000, 13.86939075806900057 ) ) ;
#23894 = VECTOR ( 'NONE', #45574, 1000.000000000000000 ) ;
#23895 = LINE ( 'NONE', #45806, #12791 ) ;
#23896 = CYLINDRICAL_SURFACE ( 'NONE', #65508, 24.99999999998794920 ) ;
#23897 = CARTESIAN_POINT ( 'NONE',  ( 0.000000000000000000, 0.000000000000000000, -14.50000000000000000 ) ) ;
#23898 = VECTOR ( 'NONE', #25419, 1000.000000000000000 ) ;
#23899 = ORIENTED_EDGE ( 'NONE', *, *, #35563, .F. ) ;
#23900 = ORIENTED_EDGE ( 'NONE', *, *, #53075, .T. ) ;
#23901 = DIRECTION ( 'NONE',  ( 0.8660254037844482555, 0.000000000000000000, 0.4999999999999831801 ) ) ;
#23902 = CARTESIAN_POINT ( 'NONE',  ( 275.0000000000000000, -0.5000000000000000000, -26.50000000000000000 ) ) ;
#23903 = EDGE_LOOP ( 'NONE', ( #14517, #20758, #28851, #26795 ) ) ;
#23904 = VERTEX_POINT ( 'NONE', #56916 ) ;
#23905 = VECTOR ( 'NONE', #9282, 1000.000000000000000 ) ;
#23906 = AXIS2_PLACEMENT_3D ( 'NONE', #52331, #57279, #67546 ) ;
#23907 = ORIENTED_EDGE ( 'NONE', *, *, #8200, .T. ) ;
#23908 = DIRECTION ( 'NONE',  ( 0.000000000000000000, -1.000000000000000000, 0.000000000000000000 ) ) ;
#23910 = ORIENTED_EDGE ( 'NONE', *, *, #29502, .T. ) ;
#23909 = DIRECTION ( 'NONE',  ( 0.000000000000000000, 0.000000000000000000, -1.000000000000000000 ) ) ;
#23911 = AXIS2_PLACEMENT_3D ( 'NONE', #29353, #65807, #60495 ) ;
#23912 = LINE ( 'NONE', #51129, #59367 ) ;
#23913 = EDGE_CURVE ( 'NONE', #13668, #60332, #30056, .T. ) ;
#23914 = DIRECTION ( 'NONE',  ( 1.836970198721029934E-16, 1.836970198721010706E-16, -1.000000000000000000 ) ) ;
#23915 = VERTEX_POINT ( 'NONE', #41006 ) ;
#23916 = ADVANCED_FACE ( 'NONE', ( #62568 ), #14856, .F. ) ;
#23917 = ORIENTED_EDGE ( 'NONE', *, *, #58646, .T. ) ;
#23918 = EDGE_CURVE ( 'NONE', #6834, #902, #63648, .T. ) ;
#23919 = AXIS2_PLACEMENT_3D ( 'NONE', #14209, #63360, #25884 ) ;
#23920 = EDGE_CURVE ( 'NONE', #53694, #56954, #21252, .T. ) ;
#23921 = CARTESIAN_POINT ( 'NONE',  ( -10.19191654964686578, -11.08848345035334759, 455.0000000000000568 ) ) ;
#23922 = DIRECTION ( 'NONE',  ( 0.000000000000000000, 0.000000000000000000, -1.000000000000000000 ) ) ;
#23923 = LINE ( 'NONE', #9773, #12331 ) ;
#23924 = CYLINDRICAL_SURFACE ( 'NONE', #10939, 1.000000000000000000 ) ;
#23925 = CARTESIAN_POINT ( 'NONE',  ( 39.00000000000000000, 21.00000000000000000, -16.96999999999999886 ) ) ;
#23926 = AXIS2_PLACEMENT_3D ( 'NONE', #52466, #63067, #63775 ) ;
#23928 = ORIENTED_EDGE ( 'NONE', *, *, #56112, .F. ) ;
#23927 = CARTESIAN_POINT ( 'NONE',  ( 6.657023737882818537, -9.912023737882810437, 26.00000000000000000 ) ) ;
#23929 = VERTEX_POINT ( 'NONE', #25820 ) ;
#23930 = DIRECTION ( 'NONE',  ( -0.4999999999999832356, 0.000000000000000000, -0.8660254037844483666 ) ) ;
#23931 = CARTESIAN_POINT ( 'NONE',  ( -8.079219948824906794, 8.697938382363059162, 54.00000000000000711 ) ) ;
#23932 = DIRECTION ( 'NONE',  ( -1.000000000000000000, 0.000000000000000000, 0.000000000000000000 ) ) ;
#23933 = AXIS2_PLACEMENT_3D ( 'NONE', #11552, #10880, #977 ) ;
#23934 = DIRECTION ( 'NONE',  ( 5.163402228214836012E-15, 1.000000000000000000, 0.000000000000000000 ) ) ;
#23935 = ORIENTED_EDGE ( 'NONE', *, *, #63377, .T. ) ;
#23936 = DIRECTION ( 'NONE',  ( 1.053224967557347660E-14, 1.000000000000000000, 0.000000000000000000 ) ) ;
#23937 = CARTESIAN_POINT ( 'NONE',  ( -2.989207322240185594, 6.858227778582772771, 54.00000000000000711 ) ) ;
#23938 = VECTOR ( 'NONE', #50462, 1000.000000000000000 ) ;
#23939 = CARTESIAN_POINT ( 'NONE',  ( 8.211283450353400681, 5.993516549646574099, 455.0000000000000568 ) ) ;
#23940 = DIRECTION ( 'NONE',  ( 0.000000000000000000, 0.000000000000000000, 1.000000000000000000 ) ) ;
#23941 = CARTESIAN_POINT ( 'NONE',  ( -8.452095193409402185, 4.242044687070461784, 455.0000000000000568 ) ) ;
#23942 = CARTESIAN_POINT ( 'NONE',  ( 7.900000000000000355, 21.00000000000000000, -18.00000000000000355 ) ) ;
#23943 = VECTOR ( 'NONE', #1460, 1000.000000000000000 ) ;
#23944 = CARTESIAN_POINT ( 'NONE',  ( 11.00000000000000000, -15.46862696659690073, -14.50000000000000000 ) ) ;
#23945 = ORIENTED_EDGE ( 'NONE', *, *, #18268, .T. ) ;
#23946 = DIRECTION ( 'NONE',  ( -1.000000000000000000, 0.000000000000000000, 0.000000000000000000 ) ) ;
#23947 = CARTESIAN_POINT ( 'NONE',  ( 0.000000000000000000, -8.249999999999998224, -24.00000000000000000 ) ) ;
#23948 = ORIENTED_EDGE ( 'NONE', *, *, #4849, .F. ) ;
#23949 = PLANE ( 'NONE',  #7411 ) ;
#23950 = AXIS2_PLACEMENT_3D ( 'NONE', #15036, #64529, #53571 ) ;
#23951 = FACE_OUTER_BOUND ( 'NONE', #32009, .T. ) ;
#23952 = DIRECTION ( 'NONE',  ( -0.000000000000000000, 3.673940397442059868E-16, -1.000000000000000000 ) ) ;
#23953 = DIRECTION ( 'NONE',  ( -1.000000000000000000, 0.000000000000000000, 0.000000000000000000 ) ) ;
#23954 = EDGE_CURVE ( 'NONE', #43073, #13160, #42066, .T. ) ;
#23955 = VECTOR ( 'NONE', #31833, 1000.000000000000114 ) ;
#23956 = VERTEX_POINT ( 'NONE', #21216 ) ;
#23957 = DIRECTION ( 'NONE',  ( 0.5000000000000019984, 0.8660254037844375974, 0.000000000000000000 ) ) ;
#23958 = CIRCLE ( 'NONE', #2661, 0.3999999999999993006 ) ;
#23959 = ORIENTED_EDGE ( 'NONE', *, *, #15851, .F. ) ;
#23960 = ADVANCED_FACE ( 'NONE', ( #58349 ), #62941, .F. ) ;
#23961 = DIRECTION ( 'NONE',  ( 0.000000000000000000, 0.000000000000000000, 1.000000000000000000 ) ) ;
#23962 = VERTEX_POINT ( 'NONE', #53045 ) ;
#23963 = DIRECTION ( 'NONE',  ( -1.000000000000000000, 0.000000000000000000, 0.000000000000000000 ) ) ;
#23964 = VECTOR ( 'NONE', #42745, 1000.000000000000000 ) ;
#23965 = ORIENTED_EDGE ( 'NONE', *, *, #64569, .T. ) ;
#23966 = CARTESIAN_POINT ( 'NONE',  ( -7.450000000000001954, 7.250000000000000000, -24.00000000000000000 ) ) ;
#23967 = DIRECTION ( 'NONE',  ( -0.000000000000000000, 3.673940397442059868E-16, -1.000000000000000000 ) ) ;
#23968 = VERTEX_POINT ( 'NONE', #64005 ) ;
#23969 = ORIENTED_EDGE ( 'NONE', *, *, #66697, .F. ) ;
#23970 = DIRECTION ( 'NONE',  ( -1.073876437509453175E-14, -1.000000000000000000, 0.000000000000000000 ) ) ;
#23971 = EDGE_LOOP ( 'NONE', ( #9933, #40645, #28083, #28089 ) ) ;
#23972 = ORIENTED_EDGE ( 'NONE', *, *, #6675, .T. ) ;
#23973 = EDGE_CURVE ( 'NONE', #19060, #34012, #31479, .T. ) ;
#23974 = CARTESIAN_POINT ( 'NONE',  ( -3.663616288757055806, 6.350872789121238426, 54.00000000000000711 ) ) ;
#23975 = DIRECTION ( 'NONE',  ( -1.794541526872559352E-16, -1.000000000000000000, 0.000000000000000000 ) ) ;
#23976 = CARTESIAN_POINT ( 'NONE',  ( 30.00000000000000000, -15.46862696659690073, -14.50000000000000000 ) ) ;
#23977 = ORIENTED_EDGE ( 'NONE', *, *, #54771, .T. ) ;
#23978 = DIRECTION ( 'NONE',  ( 0.000000000000000000, -1.000000000000000000, 0.000000000000000000 ) ) ;
#23980 = FACE_OUTER_BOUND ( 'NONE', #30421, .T. ) ;
#23979 = CARTESIAN_POINT ( 'NONE',  ( 3.848229544836324845, 7.342976262117209885, 26.00000000000000711 ) ) ;
#23981 = ORIENTED_EDGE ( 'NONE', *, *, #31964, .T. ) ;
#23983 = VERTEX_POINT ( 'NONE', #20154 ) ;
#23982 = CARTESIAN_POINT ( 'NONE',  ( 7.250000000000005329, 8.250000000000001776, -11.00000000000000000 ) ) ;
#23984 = CIRCLE ( 'NONE', #36413, 1.399999999999999245 ) ;
#23985 = VERTEX_POINT ( 'NONE', #25107 ) ;
#23986 = APPLICATION_PROTOCOL_DEFINITION ( 'draft international standard', 'automotive_design', 1998, #17819 ) ;
#23987 = LINE ( 'NONE', #55825, #51366 ) ;
#23988 = ORIENTED_EDGE ( 'NONE', *, *, #57919, .T. ) ;
#23989 = LINE ( 'NONE', #56862, #32571 ) ;
#23990 = LINE ( 'NONE', #9142, #14712 ) ;
#23991 = ORIENTED_EDGE ( 'NONE', *, *, #4204, .F. ) ;
#23992 = ORIENTED_EDGE ( 'NONE', *, *, #52477, .T. ) ;
#23993 = CONICAL_SURFACE ( 'NONE', #19507, 1732.050807568789651, 1.047197551196575871 ) ;
#23994 = EDGE_CURVE ( 'NONE', #5636, #16184, #35926, .T. ) ;
#23995 = CARTESIAN_POINT ( 'NONE',  ( 7.250000000000005329, -7.449999999999998401, -14.00000000000000000 ) ) ;
#23996 = FACE_BOUND ( 'NONE', #52956, .T. ) ;
#23997 = ORIENTED_EDGE ( 'NONE', *, *, #39676, .T. ) ;
#23998 = EDGE_CURVE ( 'NONE', #15622, #30530, #42766, .T. ) ;
#23999 = DIRECTION ( 'NONE',  ( -1.000000000000000000, 0.000000000000000000, 0.000000000000000000 ) ) ;
#24000 = DIRECTION ( 'NONE',  ( 0.000000000000000000, 0.000000000000000000, 1.000000000000000000 ) ) ;
#24001 = LINE ( 'NONE', #9150, #11387 ) ;
#24002 = ORIENTED_EDGE ( 'NONE', *, *, #26576, .F. ) ;
#24003 = VECTOR ( 'NONE', #1890, 1000.000000000000114 ) ;
#24004 = DIRECTION ( 'NONE',  ( -1.000000000000000000, 0.000000000000000000, 0.000000000000000000 ) ) ;
#24005 = DIRECTION ( 'NONE',  ( 0.000000000000000000, 0.7071067811865450192, 0.7071067811865500152 ) ) ;
#24007 = ORIENTED_EDGE ( 'NONE', *, *, #65412, .F. ) ;
#24006 = FACE_OUTER_BOUND ( 'NONE', #38668, .T. ) ;
#24009 = ORIENTED_EDGE ( 'NONE', *, *, #30540, .T. ) ;
#24008 = CARTESIAN_POINT ( 'NONE',  ( 16.89999999999999858, 13.66939075806899950, 20.80000000000000426 ) ) ;
#24011 = FACE_OUTER_BOUND ( 'NONE', #44766, .T. ) ;
#24010 = VECTOR ( 'NONE', #58227, 1000.000000000000000 ) ;
#24012 = VECTOR ( 'NONE', #62650, 1000.000000000000000 ) ;
#24013 = FACE_OUTER_BOUND ( 'NONE', #43446, .T. ) ;
#24014 = LINE ( 'NONE', #14107, #13223 ) ;
#24015 = DIRECTION ( 'NONE',  ( 0.4999999999989371835, 0.000000000000000000, 0.8660254037850523279 ) ) ;
#24016 = EDGE_CURVE ( 'NONE', #35816, #39001, #68946, .T. ) ;
#24017 = AXIS2_PLACEMENT_3D ( 'NONE', #62540, #41683, #9166 ) ;
#24018 = CARTESIAN_POINT ( 'NONE',  ( 40.90000000000000568, 21.00000000000000000, 16.96999999999999886 ) ) ;
#24019 = VERTEX_POINT ( 'NONE', #25461 ) ;
#24020 = DIRECTION ( 'NONE',  ( 0.000000000000000000, -0.7096009616570518874, -0.7046037717862339012 ) ) ;
#24021 = DIRECTION ( 'NONE',  ( -1.000000000000000000, 0.000000000000000000, 0.000000000000000000 ) ) ;
#24022 = LINE ( 'NONE', #45233, #23217 ) ;
#24024 = ORIENTED_EDGE ( 'NONE', *, *, #21872, .T. ) ;
#24023 = LINE ( 'NONE', #14115, #52546 ) ;
#24025 = CARTESIAN_POINT ( 'NONE',  ( -11.77351654964670935, 7.593516549646604830, 455.0000000000000568 ) ) ;
#24026 = AXIS2_PLACEMENT_3D ( 'NONE', #44961, #49248, #44599 ) ;
#24027 = CARTESIAN_POINT ( 'NONE',  ( 11.78648345035337819, -4.186483450353396307, 195.0000000000000284 ) ) ;
#24028 = EDGE_LOOP ( 'NONE', ( #26116, #65613, #9300, #25827 ) ) ;
#24029 = CARTESIAN_POINT ( 'NONE',  ( 2.765062094116041980, -9.955011587777324422, 455.0000000000000568 ) ) ;
#24030 = LINE ( 'NONE', #36044, #27211 ) ;
#24031 = AXIS2_PLACEMENT_3D ( 'NONE', #158, #27373, #21717 ) ;
#24032 = VERTEX_POINT ( 'NONE', #19787 ) ;
#24033 = DIRECTION ( 'NONE',  ( -1.000000000000000000, 0.000000000000000000, 0.000000000000000000 ) ) ;
#24034 = CARTESIAN_POINT ( 'NONE',  ( -4.173516549646839380, -12.00648345035344811, 455.0000000000000568 ) ) ;
#24035 = VECTOR ( 'NONE', #24206, 1000.000000000000000 ) ;
#24036 = CARTESIAN_POINT ( 'NONE',  ( 9.929523737882817613, -0.9555237378828257411, 54.00000000000000711 ) ) ;
#24037 = EDGE_CURVE ( 'NONE', #12650, #9391, #26167, .T. ) ;
#24038 = DIRECTION ( 'NONE',  ( 0.000000000000000000, 0.000000000000000000, 1.000000000000000000 ) ) ;
#24039 = ORIENTED_EDGE ( 'NONE', *, *, #1664, .T. ) ;
#24040 = ADVANCED_FACE ( 'NONE', ( #68601 ), #36057, .T. ) ;
#24041 = DIRECTION ( 'NONE',  ( 0.000000000000000000, 0.000000000000000000, 1.000000000000000000 ) ) ;
#24042 = ORIENTED_EDGE ( 'NONE', *, *, #39684, .T. ) ;
#24043 = EDGE_CURVE ( 'NONE', #1385, #44762, #52695, .T. ) ;
#24044 = ORIENTED_EDGE ( 'NONE', *, *, #11056, .F. ) ;
#24045 = AXIS2_PLACEMENT_3D ( 'NONE', #25047, #46250, #41294 ) ;
#24046 = CARTESIAN_POINT ( 'NONE',  ( -5.242976262117280406, -5.257023737882805747, 54.00000000000000711 ) ) ;
#24047 = EDGE_CURVE ( 'NONE', #13228, #9204, #32560, .T. ) ;
#24048 = EDGE_CURVE ( 'NONE', #39173, #2080, #69290, .T. ) ;
#24049 = DIRECTION ( 'NONE',  ( -0.7071067811865463515, 0.7071067811865487940, -0.000000000000000000 ) ) ;
#24051 = LINE ( 'NONE', #51640, #55841 ) ;
#24050 = FACE_OUTER_BOUND ( 'NONE', #62819, .T. ) ;
#24052 = ORIENTED_EDGE ( 'NONE', *, *, #14884, .F. ) ;
#24053 = ADVANCED_FACE ( 'NONE', ( #41715 ), #37128, .F. ) ;
#24054 = ORIENTED_EDGE ( 'NONE', *, *, #4386, .F. ) ;
#24055 = DIRECTION ( 'NONE',  ( -1.000000000000000000, 0.000000000000000000, 0.000000000000000000 ) ) ;
#24057 = ORIENTED_EDGE ( 'NONE', *, *, #39611, .T. ) ;
#24056 = EDGE_CURVE ( 'NONE', #69051, #51618, #10247, .T. ) ;
#24058 = LINE ( 'NONE', #13800, #4448 ) ;
#24059 = CARTESIAN_POINT ( 'NONE',  ( 39.00000000000000000, 21.00000000000000000, 16.96999999999999886 ) ) ;
#24060 = VECTOR ( 'NONE', #27994, 1000.000000000000000 ) ;
#24061 = CARTESIAN_POINT ( 'NONE',  ( -7.250000000000000888, 7.250000000000001776, -18.50000000000000000 ) ) ;
#24062 = DIRECTION ( 'NONE',  ( -1.000000000000000000, 0.000000000000000000, 0.000000000000000000 ) ) ;
#24063 = ORIENTED_EDGE ( 'NONE', *, *, #13586, .F. ) ;
#24064 = VECTOR ( 'NONE', #50223, 1000.000000000000000 ) ;
#24065 = DIRECTION ( 'NONE',  ( 1.836970198721029934E-16, 1.836970198721010706E-16, -1.000000000000000000 ) ) ;
#24067 = CARTESIAN_POINT ( 'NONE',  ( 49.00000000000000000, -0.1999999999911430404, -8.864436962241481021E-12 ) ) ;
#24066 = DIRECTION ( 'NONE',  ( 0.000000000000000000, 1.000000000000000000, 0.000000000000000000 ) ) ;
#24068 = VECTOR ( 'NONE', #20056, 1000.000000000000000 ) ;
#24069 = ORIENTED_EDGE ( 'NONE', *, *, #847, .T. ) ;
#24071 = VERTEX_POINT ( 'NONE', #53391 ) ;
#24070 = DIRECTION ( 'NONE',  ( 1.000000000000000000, 0.000000000000000000, 0.000000000000000000 ) ) ;
#24072 = ORIENTED_EDGE ( 'NONE', *, *, #63778, .T. ) ;
#24073 = ORIENTED_EDGE ( 'NONE', *, *, #44000, .T. ) ;
#24074 = VECTOR ( 'NONE', #30015, 1000.000000000000000 ) ;
#24075 = AXIS2_PLACEMENT_3D ( 'NONE', #34178, #55769, #44798 ) ;
#24076 = CARTESIAN_POINT ( 'NONE',  ( -25.50000000000000355, -15.12100000000000044, -24.12099999999999511 ) ) ;
#24077 = CARTESIAN_POINT ( 'NONE',  ( 29.50000000000000355, -11.50000000000100009, 15.00000000000084910 ) ) ;
#24078 = ADVANCED_FACE ( 'NONE', ( #49466 ), #44478, .T. ) ;
#24079 = EDGE_LOOP ( 'NONE', ( #64091, #25694, #42011, #42607 ) ) ;
#24080 = VERTEX_POINT ( 'NONE', #32519 ) ;
#24081 = DIRECTION ( 'NONE',  ( 0.000000000000000000, 0.000000000000000000, -1.000000000000000000 ) ) ;
#24082 = LINE ( 'NONE', #23396, #43551 ) ;
#24083 = CIRCLE ( 'NONE', #32035, 0.5000000000009441337 ) ;
#24084 = ORIENTED_EDGE ( 'NONE', *, *, #30756, .T. ) ;
#24085 = EDGE_CURVE ( 'NONE', #46497, #59150, #54085, .T. ) ;
#24086 = VERTEX_POINT ( 'NONE', #5642 ) ;
#24087 = FACE_BOUND ( 'NONE', #29510, .T. ) ;
#24088 = CIRCLE ( 'NONE', #31890, 3.499999999999849454 ) ;
#24089 = LINE ( 'NONE', #56269, #46977 ) ;
#24090 = ORIENTED_EDGE ( 'NONE', *, *, #58903, .F. ) ;
#24091 = CARTESIAN_POINT ( 'NONE',  ( -23.75054448485400016, -17.50000000000000000, -25.53140320652400064 ) ) ;
#24092 = FACE_OUTER_BOUND ( 'NONE', #40821, .T. ) ;
#24094 = ORIENTED_EDGE ( 'NONE', *, *, #38423, .T. ) ;
#24093 = CARTESIAN_POINT ( 'NONE',  ( -9.293516549646710700, 10.91351654964659801, 455.0000000000000568 ) ) ;
#24095 = EDGE_LOOP ( 'NONE', ( #4256, #25792, #35543, #22728 ) ) ;
#24096 = DIRECTION ( 'NONE',  ( -1.000000000000000000, -2.135044278125299371E-15, 0.000000000000000000 ) ) ;
#24097 = CARTESIAN_POINT ( 'NONE',  ( 275.0000000000001137, -0.5000000000000603961, 26.49999999999996092 ) ) ;
#24098 = CARTESIAN_POINT ( 'NONE',  ( 24.00000000000000000, -15.50000000000000000, -2.000000000000000000 ) ) ;
#24099 = CARTESIAN_POINT ( 'NONE',  ( 289.2330000000000041, 0.000000000000000000, -4.000000000000000000 ) ) ;
#24100 = CARTESIAN_POINT ( 'NONE',  ( -7.250000000000000888, 7.250000000000001776, -9.000000000000001776 ) ) ;
#24101 = DIRECTION ( 'NONE',  ( -1.000000000000000000, 0.000000000000000000, 0.000000000000000000 ) ) ;
#24102 = EDGE_CURVE ( 'NONE', #47832, #65081, #27212, .T. ) ;
#24103 = PLANE ( 'NONE',  #33762 ) ;
#24104 = EDGE_LOOP ( 'NONE', ( #46662, #43113, #59502, #54863, #22602, #60083, #69611, #47357 ) ) ;
#24105 = DIRECTION ( 'NONE',  ( 0.000000000000000000, 1.000000000000000000, 0.000000000000000000 ) ) ;
#24107 = EDGE_LOOP ( 'NONE', ( #9396, #10365, #33752, #19241, #25588, #14365, #44535, #26771 ) ) ;
#24106 = DIRECTION ( 'NONE',  ( 0.000000000000000000, 1.000000000000000000, 0.000000000000000000 ) ) ;
#24108 = CARTESIAN_POINT ( 'NONE',  ( 277.3542486889354564, -20.50000000000000000, 17.00000000000000000 ) ) ;
#24109 = CIRCLE ( 'NONE', #11689, 1.399999999999998579 ) ;
#24110 = AXIS2_PLACEMENT_3D ( 'NONE', #58957, #35013, #67564 ) ;
#24111 = CARTESIAN_POINT ( 'NONE',  ( -8.249999999999996447, -7.848062532927998269, 5.000000000000000000 ) ) ;
#24112 = EDGE_CURVE ( 'NONE', #32193, #5395, #47241, .T. ) ;
#24113 = LINE ( 'NONE', #51704, #23462 ) ;
#24114 = EDGE_CURVE ( 'NONE', #26801, #36169, #1364, .T. ) ;
#24116 = FACE_OUTER_BOUND ( 'NONE', #46108, .T. ) ;
#24115 = CIRCLE ( 'NONE', #39749, 0.9999999999999991118 ) ;
#24117 = CIRCLE ( 'NONE', #17300, 2.000000000000001776 ) ;
#24118 = DIRECTION ( 'NONE',  ( 1.000000000000000000, -0.000000000000000000, 0.000000000000000000 ) ) ;
#24119 = AXIS2_PLACEMENT_3D ( 'NONE', #14606, #29470, #2597 ) ;
#24120 = EDGE_CURVE ( 'NONE', #31671, #18501, #43452, .T. ) ;
#24121 = VERTEX_POINT ( 'NONE', #59724 ) ;
#24122 = LINE ( 'NONE', #3257, #40352 ) ;
#24123 = EDGE_CURVE ( 'NONE', #56148, #20589, #49799, .T. ) ;
#24124 = EDGE_CURVE ( 'NONE', #38982, #8022, #64165, .T. ) ;
#24125 = ORIENTED_EDGE ( 'NONE', *, *, #58978, .T. ) ;
#24126 = VECTOR ( 'NONE', #58786, 1000.000000000000000 ) ;
#24127 = LINE ( 'NONE', #45681, #60728 ) ;
#24128 = CIRCLE ( 'NONE', #4969, 2.458500000000000796 ) ;
#24129 = LINE ( 'NONE', #41702, #67290 ) ;
#24130 = EDGE_CURVE ( 'NONE', #4729, #1941, #53737, .T. ) ;
#24131 = CARTESIAN_POINT ( 'NONE',  ( 7.900000000000000355, -21.00000000000000000, 14.57806571531351914 ) ) ;
#24132 = EDGE_LOOP ( 'NONE', ( #66483, #12456, #18305, #64983, #56257, #36001 ) ) ;
#24133 = EDGE_CURVE ( 'NONE', #38291, #65451, #1033, .T. ) ;
#24134 = CARTESIAN_POINT ( 'NONE',  ( -7.250000000000000888, 7.250000000000001776, -21.00000000000000000 ) ) ;
#24135 = ORIENTED_EDGE ( 'NONE', *, *, #31966, .T. ) ;
#24136 = VERTEX_POINT ( 'NONE', #15899 ) ;
#24137 = EDGE_CURVE ( 'NONE', #62476, #38230, #58508, .T. ) ;
#24138 = LINE ( 'NONE', #40027, #11003 ) ;
#24139 = LINE ( 'NONE', #34371, #25161 ) ;
#24140 = ORIENTED_EDGE ( 'NONE', *, *, #59288, .T. ) ;
#24141 = CARTESIAN_POINT ( 'NONE',  ( 49.00000000000000000, -14.06939075806900163, -20.80000000000000426 ) ) ;
#24142 = CARTESIAN_POINT ( 'NONE',  ( 48.50000000000000000, 0.7500000000000000000, -3.418698582794335028 ) ) ;
#24143 = LINE ( 'NONE', #18837, #52085 ) ;
#24144 = ORIENTED_EDGE ( 'NONE', *, *, #444, .T. ) ;
#24145 = EDGE_CURVE ( 'NONE', #8910, #20164, #12186, .T. ) ;
#24146 = ORIENTED_EDGE ( 'NONE', *, *, #48720, .T. ) ;
#24148 = VERTEX_POINT ( 'NONE', #11609 ) ;
#24147 = DIRECTION ( 'NONE',  ( 1.000000000000000000, 0.000000000000000000, 0.000000000000000000 ) ) ;
#24150 = ORIENTED_EDGE ( 'NONE', *, *, #4209, .F. ) ;
#24149 = EDGE_CURVE ( 'NONE', #61865, #17044, #22249, .T. ) ;
#24151 = CARTESIAN_POINT ( 'NONE',  ( 7.250000000000005329, 8.250000000000001776, -26.00000000000001066 ) ) ;
#24152 = LINE ( 'NONE', #40414, #46736 ) ;
#24153 = DIRECTION ( 'NONE',  ( -1.000000000000000000, 0.000000000000000000, 0.000000000000000000 ) ) ;
#24154 = DIRECTION ( 'NONE',  ( 0.000000000000000000, 0.000000000000000000, 1.000000000000000000 ) ) ;
#24155 = FACE_OUTER_BOUND ( 'NONE', #6682, .T. ) ;
#24156 = CARTESIAN_POINT ( 'NONE',  ( -3.663616288757090000, -6.364920264886882784, 26.00000000000000711 ) ) ;
#24157 = ORIENTED_EDGE ( 'NONE', *, *, #28561, .F. ) ;
#24158 = EDGE_CURVE ( 'NONE', #50749, #19531, #6327, .T. ) ;
#24159 = ORIENTED_EDGE ( 'NONE', *, *, #28026, .T. ) ;
#24160 = EDGE_LOOP ( 'NONE', ( #52558, #26673, #63435, #36763 ) ) ;
#24161 = ORIENTED_EDGE ( 'NONE', *, *, #44079, .F. ) ;
#24162 = CARTESIAN_POINT ( 'NONE',  ( 39.90000000000000568, -16.96999999999999886, 21.00000000000000000 ) ) ;
#24163 = DIRECTION ( 'NONE',  ( 1.214636490590110272E-14, 1.000000000000000000, 1.836970198721032892E-16 ) ) ;
#24164 =( NAMED_UNIT ( * ) PLANE_ANGLE_UNIT ( ) SI_UNIT ( $, .RADIAN. ) );
#24165 = AXIS2_PLACEMENT_3D ( 'NONE', #18284, #6982, #29239 ) ;
#24167 = LINE ( 'NONE', #5422, #59115 ) ;
#24166 = AXIS2_PLACEMENT_3D ( 'NONE', #8240, #44669, #2248 ) ;
#24168 = VERTEX_POINT ( 'NONE', #65384 ) ;
#24169 = EDGE_LOOP ( 'NONE', ( #19622, #31925, #64043, #14863 ) ) ;
#24170 = ORIENTED_EDGE ( 'NONE', *, *, #60529, .F. ) ;
#24171 = DIRECTION ( 'NONE',  ( 1.000000000000000000, -0.000000000000000000, -0.000000000000000000 ) ) ;
#24172 = ORIENTED_EDGE ( 'NONE', *, *, #38873, .F. ) ;
#24173 = VECTOR ( 'NONE', #4221, 1000.000000000000000 ) ;
#24174 = VERTEX_POINT ( 'NONE', #16937 ) ;
#24175 = FACE_OUTER_BOUND ( 'NONE', #1142, .T. ) ;
#24176 = ORIENTED_EDGE ( 'NONE', *, *, #47102, .T. ) ;
#24177 = EDGE_CURVE ( 'NONE', #59322, #11827, #11951, .T. ) ;
#24178 = ORIENTED_EDGE ( 'NONE', *, *, #49204, .F. ) ;
#24179 = DIRECTION ( 'NONE',  ( 0.000000000000000000, 0.000000000000000000, -1.000000000000000000 ) ) ;
#24181 = VERTEX_POINT ( 'NONE', #55118 ) ;
#24180 = PLANE ( 'NONE',  #54867 ) ;
#24182 = VERTEX_POINT ( 'NONE', #38509 ) ;
#24183 = EDGE_CURVE ( 'NONE', #51332, #17638, #54766, .T. ) ;
#24184 = DIRECTION ( 'NONE',  ( 1.000000000000000000, 0.000000000000000000, 0.000000000000000000 ) ) ;
#24185 = VECTOR ( 'NONE', #62811, 1000.000000000000000 ) ;
#24186 = DIRECTION ( 'NONE',  ( 0.000000000000000000, 0.000000000000000000, 1.000000000000000000 ) ) ;
#24187 = CARTESIAN_POINT ( 'NONE',  ( -8.250000000000001776, 7.250000000000000888, -9.500000000000001776 ) ) ;
#24188 = ADVANCED_FACE ( 'NONE', ( #65719 ), #27895, .F. ) ;
#24190 = ORIENTED_EDGE ( 'NONE', *, *, #68107, .T. ) ;
#24189 = PLANE ( 'NONE',  #51542 ) ;
#24191 = AXIS2_PLACEMENT_3D ( 'NONE', #52437, #63041, #58792 ) ;
#24192 = VERTEX_POINT ( 'NONE', #50828 ) ;
#24193 = EDGE_CURVE ( 'NONE', #46075, #69141, #26907, .T. ) ;
#24194 = DIRECTION ( 'NONE',  ( -1.000000000000000000, 0.000000000000000000, 0.000000000000000000 ) ) ;
#24195 = DIRECTION ( 'NONE',  ( -0.000000000000000000, -0.000000000000000000, -1.000000000000000000 ) ) ;
#24196 = CARTESIAN_POINT ( 'NONE',  ( 12.90000000000000213, -21.00000000000000000, 13.86939075806900057 ) ) ;
#24197 = EDGE_CURVE ( 'NONE', #42854, #16184, #2048, .T. ) ;
#24198 = ORIENTED_EDGE ( 'NONE', *, *, #62341, .T. ) ;
#24199 = CARTESIAN_POINT ( 'NONE',  ( 4.186483450353335023, -12.00648345035347830, 455.0000000000000568 ) ) ;
#24200 = DIRECTION ( 'NONE',  ( -0.5000000000000019984, -0.8660254037844375974, 0.000000000000000000 ) ) ;
#24201 = DIRECTION ( 'NONE',  ( -0.000000000000000000, 0.000000000000000000, 1.000000000000000000 ) ) ;
#24202 = ORIENTED_EDGE ( 'NONE', *, *, #59726, .F. ) ;
#24203 = EDGE_CURVE ( 'NONE', #21453, #56437, #3109, .T. ) ;
#24204 = PLANE ( 'NONE',  #34705 ) ;
#24205 = EDGE_CURVE ( 'NONE', #24424, #46212, #40223, .T. ) ;
#24206 = DIRECTION ( 'NONE',  ( -0.000000000000000000, -0.000000000000000000, 1.000000000000000000 ) ) ;
#24207 = CARTESIAN_POINT ( 'NONE',  ( -15.50000000000000000, -2.500000000000000000, -21.05662432702600029 ) ) ;
#24208 = EDGE_CURVE ( 'NONE', #15685, #67578, #12641, .T. ) ;
#24209 = EDGE_CURVE ( 'NONE', #5145, #12839, #44949, .T. ) ;
#24210 = ORIENTED_EDGE ( 'NONE', *, *, #31252, .F. ) ;
#24211 = CARTESIAN_POINT ( 'NONE',  ( -10.03972626211731978, -8.930623737882752877, 54.00000000000000711 ) ) ;
#24212 = DIRECTION ( 'NONE',  ( 1.060575238724892987E-16, 0.5000000000000199840, -0.8660254037844271613 ) ) ;
#24213 = ADVANCED_FACE ( 'NONE', ( #2398 ), #39863, .T. ) ;
#24214 = AXIS2_PLACEMENT_3D ( 'NONE', #32060, #26760, #60304 ) ;
#24215 = VECTOR ( 'NONE', #46693, 1000.000000000000000 ) ;
#24216 = EDGE_LOOP ( 'NONE', ( #62255, #63696, #68889, #24930 ) ) ;
#24217 = DIRECTION ( 'NONE',  ( 1.000000000000000000, 0.000000000000000000, 0.000000000000000000 ) ) ;
#24218 = PLANE ( 'NONE',  #58024 ) ;
#24219 = CARTESIAN_POINT ( 'NONE',  ( 275.5000000000000000, -42.50000000000000000, -15.10000000000000142 ) ) ;
#24220 = PLANE ( 'NONE',  #36909 ) ;
#24221 = CARTESIAN_POINT ( 'NONE',  ( 15.50000000000000000, -15.50000000000000000, -22.50000000000000000 ) ) ;
#24222 = CIRCLE ( 'NONE', #37764, 0.1999999999999987899 ) ;
#24223 = AXIS2_PLACEMENT_3D ( 'NONE', #17023, #49885, #32935 ) ;
#24224 = ORIENTED_EDGE ( 'NONE', *, *, #33690, .F. ) ;
#24225 = AXIS2_PLACEMENT_3D ( 'NONE', #12789, #13153, #17079 ) ;
#24226 = CARTESIAN_POINT ( 'NONE',  ( -14.66434062215826017, -0.3156604612126701626, -21.53909249377373669 ) ) ;
#24227 = DIRECTION ( 'NONE',  ( 1.000000000000000000, 0.000000000000000000, 0.000000000000000000 ) ) ;
#24228 = LINE ( 'NONE', #40120, #56007 ) ;
#24229 = AXIS2_PLACEMENT_3D ( 'NONE', #11802, #66255, #53320 ) ;
#24230 = DIRECTION ( 'NONE',  ( 1.836970198721029934E-16, 1.836970198721010706E-16, -1.000000000000000000 ) ) ;
#24231 = DIRECTION ( 'NONE',  ( 0.000000000000000000, 0.000000000000000000, -1.000000000000000000 ) ) ;
#24232 = ADVANCED_FACE ( 'NONE', ( #51184 ), #55460, .F. ) ;
#24233 = ORIENTED_EDGE ( 'NONE', *, *, #67595, .F. ) ;
#24235 = VERTEX_POINT ( 'NONE', #34206 ) ;
#24234 = PLANE ( 'NONE',  #46514 ) ;
#24236 = EDGE_CURVE ( 'NONE', #24071, #4441, #34565, .T. ) ;
#24237 = LINE ( 'NONE', #12905, #54212 ) ;
#24238 = CARTESIAN_POINT ( 'NONE',  ( -30.00000000000000000, -16.28999999999710369, 15.00000000000794920 ) ) ;
#24239 = ORIENTED_EDGE ( 'NONE', *, *, #15841, .T. ) ;
#24240 = CARTESIAN_POINT ( 'NONE',  ( 7.500000000000000000, -20.40000000000000213, -20.00000000000000000 ) ) ;
#24241 = ORIENTED_EDGE ( 'NONE', *, *, #54384, .F. ) ;
#24242 = CARTESIAN_POINT ( 'NONE',  ( -10.91351654964670637, 9.293516549646604119, 195.0000000000000284 ) ) ;
#24243 = VERTEX_POINT ( 'NONE', #66408 ) ;
#24244 = ORIENTED_EDGE ( 'NONE', *, *, #4736, .T. ) ;
#24245 = DIRECTION ( 'NONE',  ( 0.000000000000000000, 1.000000000000000000, 0.000000000000000000 ) ) ;
#24246 = DIRECTION ( 'NONE',  ( 1.836970198721029934E-16, -1.836970198721036344E-16, 1.000000000000000000 ) ) ;
#24247 = CYLINDRICAL_SURFACE ( 'NONE', #56303, 0.9999999999984570120 ) ;
#24248 = CARTESIAN_POINT ( 'NONE',  ( 7.000000000000000000, -26.42999999999999972, 9.412893218813501051 ) ) ;
#24249 = ORIENTED_EDGE ( 'NONE', *, *, #19924, .T. ) ;
#24250 = VECTOR ( 'NONE', #51276, 1000.000000000000000 ) ;
#24251 = ORIENTED_EDGE ( 'NONE', *, *, #28901, .T. ) ;
#24252 = CARTESIAN_POINT ( 'NONE',  ( -7.450000000000001954, 0.000000000000000000, -17.50000000000000000 ) ) ;
#24253 = LINE ( 'NONE', #45817, #51950 ) ;
#24254 = ORIENTED_EDGE ( 'NONE', *, *, #28901, .F. ) ;
#24255 = CIRCLE ( 'NONE', #20881, 0.3499999999999996447 ) ;
#24256 = VERTEX_POINT ( 'NONE', #45521 ) ;
#24257 = ORIENTED_EDGE ( 'NONE', *, *, #66509, .T. ) ;
#24258 = FACE_OUTER_BOUND ( 'NONE', #34203, .T. ) ;
#24260 = VERTEX_POINT ( 'NONE', #66049 ) ;
#24259 = DIRECTION ( 'NONE',  ( -1.000000000000000000, 0.000000000000000000, 0.000000000000000000 ) ) ;
#24261 = EDGE_CURVE ( 'NONE', #22368, #62934, #35252, .T. ) ;
#24262 = DIRECTION ( 'NONE',  ( -1.000000000000000000, 0.000000000000000000, 0.000000000000000000 ) ) ;
#24263 = AXIS2_PLACEMENT_3D ( 'NONE', #4660, #26221, #64745 ) ;
#24264 = VECTOR ( 'NONE', #65743, 1000.000000000000000 ) ;
#24265 = LINE ( 'NONE', #34513, #20410 ) ;
#24266 = ORIENTED_EDGE ( 'NONE', *, *, #69411, .T. ) ;
#24267 = EDGE_CURVE ( 'NONE', #22188, #31070, #25796, .T. ) ;
#24268 = ORIENTED_EDGE ( 'NONE', *, *, #66981, .T. ) ;
#24269 = VECTOR ( 'NONE', #59382, 1000.000000000000000 ) ;
#24270 = ADVANCED_FACE ( 'NONE', ( #18652 ), #13358, .F. ) ;
#24271 = ADVANCED_FACE ( 'NONE', ( #56488 ), #29967, .T. ) ;
#24272 = CARTESIAN_POINT ( 'NONE',  ( 39.00000000000000000, 14.08845687959340331, -21.00000000000000000 ) ) ;
#24273 = CARTESIAN_POINT ( 'NONE',  ( 8.250000000000005329, 7.250000000000000888, -19.50000000000000000 ) ) ;
#24274 = AXIS2_PLACEMENT_3D ( 'NONE', #5047, #58800, #31237 ) ;
#24275 = EDGE_CURVE ( 'NONE', #65451, #57577, #50493, .T. ) ;
#24276 = EDGE_CURVE ( 'NONE', #13431, #41511, #19013, .T. ) ;
#24277 = CARTESIAN_POINT ( 'NONE',  ( 7.250000000000005329, -7.249999999999998224, -7.500000000000000000 ) ) ;
#24278 = CIRCLE ( 'NONE', #43517, 0.7112000000000124889 ) ;
#24279 = DIRECTION ( 'NONE',  ( 1.000000000000000000, 0.000000000000000000, 0.000000000000000000 ) ) ;
#24280 = CARTESIAN_POINT ( 'NONE',  ( -9.791916549646856538, -10.20488345035338718, 455.0000000000000568 ) ) ;
#24282 = ORIENTED_EDGE ( 'NONE', *, *, #36367, .T. ) ;
#24281 = CARTESIAN_POINT ( 'NONE',  ( 21.90000000000000213, -21.00000000000000000, 13.86939075806900057 ) ) ;
#24283 = ORIENTED_EDGE ( 'NONE', *, *, #33929, .F. ) ;
#24284 = CIRCLE ( 'NONE', #68308, 2.458500000000000796 ) ;
#24285 = LINE ( 'NONE', #56113, #11759 ) ;
#24286 = CARTESIAN_POINT ( 'NONE',  ( 13.00000000000000178, -17.00000000000000000, -15.70499999999969809 ) ) ;
#24287 = CARTESIAN_POINT ( 'NONE',  ( -25.50000000000000355, -5.578999999999999737, 22.50000000000000000 ) ) ;
#24288 = CARTESIAN_POINT ( 'NONE',  ( 31.89999999999999858, 20.60000000000000142, 13.86939075806899702 ) ) ;
#24289 = FACE_OUTER_BOUND ( 'NONE', #34817, .T. ) ;
#24290 = ORIENTED_EDGE ( 'NONE', *, *, #48380, .F. ) ;
#24291 = PLANE ( 'NONE',  #24516 ) ;
#24292 = DIRECTION ( 'NONE',  ( 1.000000000000000000, -0.000000000000000000, -0.000000000000000000 ) ) ;
#24293 = CARTESIAN_POINT ( 'NONE',  ( -7.250000000000001776, -7.249999999999998224, -7.500000000000000000 ) ) ;
#24294 = DIRECTION ( 'NONE',  ( 0.000000000000000000, 1.000000000000000000, 0.000000000000000000 ) ) ;
#24295 = DIRECTION ( 'NONE',  ( 0.000000000000000000, 0.000000000000000000, 1.000000000000000000 ) ) ;
#24296 = DIRECTION ( 'NONE',  ( 0.000000000000000000, 1.000000000000000000, 0.000000000000000000 ) ) ;
#24297 = DIRECTION ( 'NONE',  ( 0.000000000000000000, 0.000000000000000000, 1.000000000000000000 ) ) ;
#24298 = ORIENTED_EDGE ( 'NONE', *, *, #11632, .T. ) ;
#24299 = LINE ( 'NONE', #67448, #19657 ) ;
#24300 = FACE_OUTER_BOUND ( 'NONE', #15440, .T. ) ;
#24301 = VECTOR ( 'NONE', #55621, 1000.000000000000114 ) ;
#24302 = EDGE_LOOP ( 'NONE', ( #47554, #55744 ) ) ;
#24303 = DIRECTION ( 'NONE',  ( 0.7071067811865490160, 0.000000000000000000, -0.7071067811865461294 ) ) ;
#24304 = DIRECTION ( 'NONE',  ( -1.000000000000000000, 0.000000000000000000, 0.000000000000000000 ) ) ;
#24305 = CARTESIAN_POINT ( 'NONE',  ( 9.899999999999998579, -0.2000000000000000111, 0.000000000000000000 ) ) ;
#24306 = CIRCLE ( 'NONE', #69492, 0.5000000000079367624 ) ;
#24307 = SURFACE_SIDE_STYLE ('',( #19344 ) ) ;
#24308 = FACE_OUTER_BOUND ( 'NONE', #16087, .T. ) ;
#24309 = ORIENTED_EDGE ( 'NONE', *, *, #11632, .F. ) ;
#24310 = LINE ( 'NONE', #2393, #39895 ) ;
#24311 = ADVANCED_FACE ( 'NONE', ( #62135 ), #28919, .F. ) ;
#24312 = CIRCLE ( 'NONE', #63851, 5.000000000000000000 ) ;
#24313 = VECTOR ( 'NONE', #65359, 1000.000000000000000 ) ;
#24314 = AXIS2_PLACEMENT_3D ( 'NONE', #57221, #31052, #35276 ) ;
#24315 = ORIENTED_EDGE ( 'NONE', *, *, #1750, .T. ) ;
#24316 = CARTESIAN_POINT ( 'NONE',  ( 35.89999999999999858, -0.000000000000000000, -20.80000000000000071 ) ) ;
#24317 = CARTESIAN_POINT ( 'NONE',  ( 29.50000000000000355, -11.50000000000000000, -15.00000000000000000 ) ) ;
#24318 = ORIENTED_EDGE ( 'NONE', *, *, #47606, .T. ) ;
#24319 = EDGE_CURVE ( 'NONE', #29208, #48285, #2054, .T. ) ;
#24320 = DIRECTION ( 'NONE',  ( 0.000000000000000000, 0.000000000000000000, 1.000000000000000000 ) ) ;
#24321 = VECTOR ( 'NONE', #21478, 1000.000000000000000 ) ;
#24322 = VECTOR ( 'NONE', #23464, 1000.000000000000000 ) ;
#24323 = ORIENTED_EDGE ( 'NONE', *, *, #60602, .F. ) ;
#24324 = VECTOR ( 'NONE', #56092, 1000.000000000000000 ) ;
#24325 = DIRECTION ( 'NONE',  ( 1.000000000000000000, -0.000000000000000000, -0.000000000000000000 ) ) ;
#24326 = ORIENTED_EDGE ( 'NONE', *, *, #25915, .T. ) ;
#24327 = VERTEX_POINT ( 'NONE', #36323 ) ;
#24328 = DIRECTION ( 'NONE',  ( -1.000000000000000000, 0.000000000000000000, 0.000000000000000000 ) ) ;
#24329 = EDGE_LOOP ( 'NONE', ( #12773, #20578, #16650, #37757 ) ) ;
#24330 = VERTEX_POINT ( 'NONE', #46926 ) ;
#24331 = CARTESIAN_POINT ( 'NONE',  ( -11.50000000000000000, -15.97213595500069871, 14.50000000000000000 ) ) ;
#24332 = DIRECTION ( 'NONE',  ( 0.000000000000000000, 1.000000000000000000, 0.000000000000000000 ) ) ;
#24333 = VECTOR ( 'NONE', #24212, 999.9999999999998863 ) ;
#24334 = DIRECTION ( 'NONE',  ( 1.000000000000000000, 0.000000000000000000, 0.000000000000000000 ) ) ;
#24335 = ORIENTED_EDGE ( 'NONE', *, *, #5484, .F. ) ;
#24336 = VECTOR ( 'NONE', #63001, 1000.000000000000000 ) ;
#24337 = CARTESIAN_POINT ( 'NONE',  ( 9.690000000000001279, -9.690000000000001279, -5.000000000000000000 ) ) ;
#24339 = DIRECTION ( 'NONE',  ( 0.000000000000000000, -0.7046037717859411353, -0.7096009616573427659 ) ) ;
#24338 = FACE_OUTER_BOUND ( 'NONE', #26594, .T. ) ;
#24340 = ORIENTED_EDGE ( 'NONE', *, *, #3922, .T. ) ;
#24342 = ORIENTED_EDGE ( 'NONE', *, *, #50059, .F. ) ;
#24341 = DIRECTION ( 'NONE',  ( 0.000000000000000000, 0.000000000000000000, 1.000000000000000000 ) ) ;
#24343 = EDGE_LOOP ( 'NONE', ( #68359, #53502, #63396, #28279 ) ) ;
#24344 = CARTESIAN_POINT ( 'NONE',  ( -4.609516549646713202, 3.593516549646603941, 195.0000000000000284 ) ) ;
#24345 = VERTEX_POINT ( 'NONE', #57889 ) ;
#24346 = EDGE_CURVE ( 'NONE', #4281, #12232, #47290, .T. ) ;
#24347 = CYLINDRICAL_SURFACE ( 'NONE', #52918, 2.204799999999997429 ) ;
#24348 = LINE ( 'NONE', #30711, #23733 ) ;
#24349 = EDGE_LOOP ( 'NONE', ( #39333, #65661, #48169, #65250 ) ) ;
#24350 = VERTEX_POINT ( 'NONE', #40921 ) ;
#24351 = DIRECTION ( 'NONE',  ( -1.000000000000000000, 0.000000000000000000, 0.000000000000000000 ) ) ;
#24352 = CARTESIAN_POINT ( 'NONE',  ( 9.841277389592647751, 1.677516549646587363, 195.0000000000000284 ) ) ;
#24353 = AXIS2_PLACEMENT_3D ( 'NONE', #9279, #30846, #3979 ) ;
#24354 = ORIENTED_EDGE ( 'NONE', *, *, #9502, .F. ) ;
#24355 = PLANE ( 'NONE',  #50018 ) ;
#24356 = PLANE ( 'NONE',  #36926 ) ;
#24357 = EDGE_CURVE ( 'NONE', #7353, #12401, #9460, .T. ) ;
#24358 = DIRECTION ( 'NONE',  ( -1.000000000000000000, 0.000000000000000000, 0.000000000000000000 ) ) ;
#24359 = ADVANCED_FACE ( 'NONE', ( #25371 ), #52604, .F. ) ;
#24360 = ORIENTED_EDGE ( 'NONE', *, *, #6684, .F. ) ;
#24361 = VECTOR ( 'NONE', #32975, 1000.000000000000000 ) ;
#24362 = VECTOR ( 'NONE', #11063, 1000.000000000000000 ) ;
#24363 = EDGE_CURVE ( 'NONE', #30244, #26273, #25734, .T. ) ;
#24364 = DIRECTION ( 'NONE',  ( -1.000000000000000000, 0.000000000000000000, 0.000000000000000000 ) ) ;
#24365 = DIRECTION ( 'NONE',  ( -1.000000000000000000, 3.016910393003147986E-15, 0.000000000000000000 ) ) ;
#24367 = ORIENTED_EDGE ( 'NONE', *, *, #4287, .F. ) ;
#24366 = CARTESIAN_POINT ( 'NONE',  ( 46.39999999999999858, 21.00000000000000000, 2.250000000000000444 ) ) ;
#24369 = ORIENTED_EDGE ( 'NONE', *, *, #28658, .F. ) ;
#24368 = CARTESIAN_POINT ( 'NONE',  ( 30.00000000000000000, -5.000000000000000000, -27.00000000000000000 ) ) ;
#24370 = FACE_OUTER_BOUND ( 'NONE', #40170, .T. ) ;
#24371 = AXIS2_PLACEMENT_3D ( 'NONE', #32036, #32386, #63153 ) ;
#24372 = VECTOR ( 'NONE', #35257, 1000.000000000000114 ) ;
#24373 = VECTOR ( 'NONE', #65144, 1000.000000000000000 ) ;
#24374 = DIRECTION ( 'NONE',  ( 0.000000000000000000, -0.1249999999999996531, -0.9921567416492215186 ) ) ;
#24375 = CARTESIAN_POINT ( 'NONE',  ( 9.737023737882781305, 3.667976262117152775, 54.00000000000000711 ) ) ;
#24376 = DIRECTION ( 'NONE',  ( 0.000000000000000000, -0.1111111111108840643, -0.9938079899999319178 ) ) ;
#24377 = CIRCLE ( 'NONE', #27817, 0.1749999999999993783 ) ;
#24378 = CARTESIAN_POINT ( 'NONE',  ( -15.50000000000000000, -0.4000000000000000222, -19.00000000000000355 ) ) ;
#24379 = ORIENTED_EDGE ( 'NONE', *, *, #55040, .F. ) ;
#24380 = LINE ( 'NONE', #62199, #69657 ) ;
#24381 = FACE_OUTER_BOUND ( 'NONE', #51900, .T. ) ;
#24382 = LINE ( 'NONE', #49860, #42418 ) ;
#24384 = ORIENTED_EDGE ( 'NONE', *, *, #57385, .T. ) ;
#24383 = LINE ( 'NONE', #18721, #51417 ) ;
#24385 = VECTOR ( 'NONE', #34364, 1000.000000000000000 ) ;
#24386 = DIRECTION ( 'NONE',  ( 1.000000000000000000, 0.000000000000000000, 0.000000000000000000 ) ) ;
#24387 = VECTOR ( 'NONE', #2031, 1000.000000000000114 ) ;
#24388 = DIRECTION ( 'NONE',  ( -1.836970198721029934E-16, 1.836970198721036344E-16, -1.000000000000000000 ) ) ;
#24389 = ORIENTED_EDGE ( 'NONE', *, *, #54856, .F. ) ;
#24390 = ORIENTED_EDGE ( 'NONE', *, *, #58468, .T. ) ;
#24391 = DIRECTION ( 'NONE',  ( 1.836970198721029934E-16, 1.836970198721010706E-16, -1.000000000000000000 ) ) ;
#24392 = CARTESIAN_POINT ( 'NONE',  ( -3.650476262117331228, -10.50702373788281641, 26.00000000000000000 ) ) ;
#24393 = VERTEX_POINT ( 'NONE', #30677 ) ;
#24394 = PLANE ( 'NONE',  #27853 ) ;
#24395 = DIRECTION ( 'NONE',  ( 1.000000000000000000, 0.000000000000000000, 0.000000000000000000 ) ) ;
#24396 = CARTESIAN_POINT ( 'NONE',  ( -9.722976262117258628, 6.817976262117182884, 54.00000000000000711 ) ) ;
#24397 = CARTESIAN_POINT ( 'NONE',  ( 7.250000000000005329, 7.250000000000000888, -23.50000000000000000 ) ) ;
#24398 = ORIENTED_EDGE ( 'NONE', *, *, #47372, .T. ) ;
#24399 = FACE_OUTER_BOUND ( 'NONE', #48688, .T. ) ;
#24400 = DIRECTION ( 'NONE',  ( 1.000000000000000000, 0.000000000000000000, 0.000000000000000000 ) ) ;
#24401 = VECTOR ( 'NONE', #69087, 999.9999999999998863 ) ;
#24402 = EDGE_LOOP ( 'NONE', ( #21403, #59579, #14669, #21327 ) ) ;
#24403 = EDGE_CURVE ( 'NONE', #53423, #51193, #14523, .T. ) ;
#24404 = ADVANCED_FACE ( 'NONE', ( #8757 ), #10155, .T. ) ;
#24405 = DIRECTION ( 'NONE',  ( -1.000000000000000000, 0.000000000000000000, 0.000000000000000000 ) ) ;
#24406 = EDGE_CURVE ( 'NONE', #35196, #7192, #58557, .T. ) ;
#24407 = VECTOR ( 'NONE', #47983, 1000.000000000000000 ) ;
#24408 = EDGE_CURVE ( 'NONE', #60221, #52778, #2098, .T. ) ;
#24409 = CARTESIAN_POINT ( 'NONE',  ( 7.811466277050736373, -7.272650909786728235, 455.0000000000000568 ) ) ;
#24410 = VECTOR ( 'NONE', #17099, 1000.000000000000000 ) ;
#24411 = CARTESIAN_POINT ( 'NONE',  ( 78.77321854994620765, 47.95351654967443977, 26.00000000000000355 ) ) ;
#24412 = VERTEX_POINT ( 'NONE', #15118 ) ;
#24413 = ORIENTED_EDGE ( 'NONE', *, *, #28802, .F. ) ;
#24414 = DIRECTION ( 'NONE',  ( 0.000000000000000000, 0.000000000000000000, 1.000000000000000000 ) ) ;
#24415 = VERTEX_POINT ( 'NONE', #14050 ) ;
#24416 = ORIENTED_EDGE ( 'NONE', *, *, #38445, .T. ) ;
#24417 = VECTOR ( 'NONE', #60876, 1000.000000000000000 ) ;
#24418 = VECTOR ( 'NONE', #66477, 1000.000000000000000 ) ;
#24419 = VECTOR ( 'NONE', #12328, 1000.000000000000000 ) ;
#24420 = DIRECTION ( 'NONE',  ( -1.000000000000000000, 0.000000000000000000, 0.000000000000000000 ) ) ;
#24421 = DIRECTION ( 'NONE',  ( 0.000000000000000000, 0.000000000000000000, 1.000000000000000000 ) ) ;
#24422 = DIRECTION ( 'NONE',  ( 0.7071067811865510144, 0.7071067811865441310, -8.343721112914546325E-31 ) ) ;
#24423 = DIRECTION ( 'NONE',  ( -1.836970198721029934E-16, 1.836970198721036344E-16, -1.000000000000000000 ) ) ;
#24424 = VERTEX_POINT ( 'NONE', #68153 ) ;
#24425 = DIRECTION ( 'NONE',  ( -1.000000000000000000, 0.000000000000000000, 0.000000000000000000 ) ) ;
#24426 = VECTOR ( 'NONE', #35137, 1000.000000000000114 ) ;
#24427 = VECTOR ( 'NONE', #69752, 1000.000000000000000 ) ;
#24428 = CIRCLE ( 'NONE', #63966, 0.1999999999999987899 ) ;
#24430 = FACE_OUTER_BOUND ( 'NONE', #57744, .T. ) ;
#24429 = FACE_OUTER_BOUND ( 'NONE', #26976, .T. ) ;
#24431 = ORIENTED_EDGE ( 'NONE', *, *, #56547, .F. ) ;
#24433 = VERTEX_POINT ( 'NONE', #36681 ) ;
#24432 = CARTESIAN_POINT ( 'NONE',  ( -7.450000000000001954, 0.000000000000000000, -25.50000000000000355 ) ) ;
#24434 = ORIENTED_EDGE ( 'NONE', *, *, #15533, .F. ) ;
#24435 = ORIENTED_EDGE ( 'NONE', *, *, #18267, .F. ) ;
#24436 = VECTOR ( 'NONE', #55496, 1000.000000000000000 ) ;
#24437 = CYLINDRICAL_SURFACE ( 'NONE', #5099, 0.1999999999999987899 ) ;
#24438 = VECTOR ( 'NONE', #41258, 1000.000000000000000 ) ;
#24439 = DIRECTION ( 'NONE',  ( -1.000000000000000000, 0.000000000000000000, 0.000000000000000000 ) ) ;
#24440 = VERTEX_POINT ( 'NONE', #52242 ) ;
#24441 = VERTEX_POINT ( 'NONE', #19356 ) ;
#24442 = FACE_BOUND ( 'NONE', #41404, .T. ) ;
#24443 = CARTESIAN_POINT ( 'NONE',  ( -7.342976262117259623, 6.651770455163663165, 26.00000000000000711 ) ) ;
#24444 = ORIENTED_EDGE ( 'NONE', *, *, #55321, .T. ) ;
#24445 = ORIENTED_EDGE ( 'NONE', *, *, #61800, .F. ) ;
#24446 = DIRECTION ( 'NONE',  ( 0.5773502691896175154, 0.5773502691896339467, 0.5773502691896257311 ) ) ;
#24447 = FACE_OUTER_BOUND ( 'NONE', #46702, .T. ) ;
#24448 = EDGE_LOOP ( 'NONE', ( #42353, #23505, #6748, #56352 ) ) ;
#24449 = EDGE_CURVE ( 'NONE', #42297, #30976, #63907, .T. ) ;
#24450 = ADVANCED_FACE ( 'NONE', ( #3802 ), #9822, .F. ) ;
#24451 = DIRECTION ( 'NONE',  ( 0.000000000000000000, 0.000000000000000000, 1.000000000000000000 ) ) ;
#24452 = DIRECTION ( 'NONE',  ( 0.000000000000000000, -1.000000000000000000, 0.000000000000000000 ) ) ;
#24453 = EDGE_CURVE ( 'NONE', #62784, #6004, #37104, .T. ) ;
#24454 = VECTOR ( 'NONE', #58043, 1000.000000000000000 ) ;
#24456 = ORIENTED_EDGE ( 'NONE', *, *, #60108, .T. ) ;
#24455 = CARTESIAN_POINT ( 'NONE',  ( -9.093516549646711411, 10.91351654964659978, 195.0000000000000284 ) ) ;
#24457 = ORIENTED_EDGE ( 'NONE', *, *, #17801, .F. ) ;
#24458 = DIRECTION ( 'NONE',  ( 1.000000000000000000, 0.000000000000000000, 0.000000000000000000 ) ) ;
#24459 = LINE ( 'NONE', #13136, #5257 ) ;
#24460 = ADVANCED_FACE ( 'NONE', ( #30326 ), #52957, .T. ) ;
#24461 = AXIS2_PLACEMENT_3D ( 'NONE', #46759, #8931, #19194 ) ;
#24462 = DIRECTION ( 'NONE',  ( 0.000000000000000000, 1.000000000000000000, 0.000000000000000000 ) ) ;
#24463 = LINE ( 'NONE', #46715, #32380 ) ;
#24464 = CARTESIAN_POINT ( 'NONE',  ( 15.50000000000000000, -0.1999999999999999556, -23.94999999999999574 ) ) ;
#24465 = LINE ( 'NONE', #46029, #1224 ) ;
#24466 = AXIS2_PLACEMENT_3D ( 'NONE', #36, #21597, #43150 ) ;
#24467 = ADVANCED_FACE ( 'NONE', ( #69202 ), #25025, .T. ) ;
#24468 = DIRECTION ( 'NONE',  ( 0.000000000000000000, -1.000000000000000000, 6.036837696397648868E-13 ) ) ;
#24469 = ORIENTED_EDGE ( 'NONE', *, *, #38896, .F. ) ;
#24470 = CARTESIAN_POINT ( 'NONE',  ( 30.90000000000000213, -0.2000000000089119934, 8.909539772616881237E-12 ) ) ;
#24471 = EDGE_CURVE ( 'NONE', #33622, #20378, #53307, .T. ) ;
#24473 = ORIENTED_EDGE ( 'NONE', *, *, #1934, .T. ) ;
#24472 = DIRECTION ( 'NONE',  ( -1.813998472013049822E-14, -1.000000000000000000, -1.836970198721044232E-16 ) ) ;
#24474 = VECTOR ( 'NONE', #25271, 1000.000000000000000 ) ;
#24475 = AXIS2_PLACEMENT_3D ( 'NONE', #14408, #46561, #63185 ) ;
#24477 = DIRECTION ( 'NONE',  ( 0.000000000000000000, 0.000000000000000000, 1.000000000000000000 ) ) ;
#24476 = VECTOR ( 'NONE', #49496, 1000.000000000000000 ) ;
#24478 = DIRECTION ( 'NONE',  ( 1.000000000000000000, 0.000000000000000000, 0.000000000000000000 ) ) ;
#24479 = DIRECTION ( 'NONE',  ( 1.000000000000000000, -0.000000000000000000, -0.000000000000000000 ) ) ;
#24480 = CARTESIAN_POINT ( 'NONE',  ( 7.250000000000005329, -8.249999999999998224, -14.50000000000000000 ) ) ;
#24481 = CIRCLE ( 'NONE', #64026, 1.224999999999998757 ) ;
#24482 = AXIS2_PLACEMENT_3D ( 'NONE', #65321, #38104, #43039 ) ;
#24483 = CARTESIAN_POINT ( 'NONE',  ( 30.00000000000000000, -9.199999999999999289, -12.69999999999986073 ) ) ;
#24484 = ORIENTED_EDGE ( 'NONE', *, *, #44100, .F. ) ;
#24485 = CARTESIAN_POINT ( 'NONE',  ( 10.74648345035337904, -1.690483450353395645, 195.0000000000000284 ) ) ;
#24486 = ORIENTED_EDGE ( 'NONE', *, *, #25749, .T. ) ;
#24487 = VECTOR ( 'NONE', #37853, 1000.000000000000000 ) ;
#24488 = CARTESIAN_POINT ( 'NONE',  ( 5.552858015815581361, -7.357023737882824044, 54.00000000000000711 ) ) ;
#24489 = CIRCLE ( 'NONE', #9817, 0.5000000000079362072 ) ;
#24490 = DIRECTION ( 'NONE',  ( 9.973078850062115052E-15, 1.000000000000000000, 1.836970198721028948E-16 ) ) ;
#24491 = ORIENTED_EDGE ( 'NONE', *, *, #7420, .F. ) ;
#24492 = PLANE ( 'NONE',  #32757 ) ;
#24493 = ORIENTED_EDGE ( 'NONE', *, *, #60050, .T. ) ;
#24494 = ORIENTED_EDGE ( 'NONE', *, *, #17068, .T. ) ;
#24495 = DIRECTION ( 'NONE',  ( -0.000000000000000000, -0.000000000000000000, -1.000000000000000000 ) ) ;
#24496 = LINE ( 'NONE', #66913, #51137 ) ;
#24497 = DIRECTION ( 'NONE',  ( 1.000000000000000000, -1.671920889371702657E-15, 0.000000000000000000 ) ) ;
#24498 = DIRECTION ( 'NONE',  ( 0.000000000000000000, -1.000000000000000000, -0.000000000000000000 ) ) ;
#24499 = CARTESIAN_POINT ( 'NONE',  ( -7.394232575409614761, 6.775514141871308738, 26.00000000000000711 ) ) ;
#24500 = ORIENTED_EDGE ( 'NONE', *, *, #9207, .T. ) ;
#24501 = ORIENTED_EDGE ( 'NONE', *, *, #26218, .T. ) ;
#24503 = ORIENTED_EDGE ( 'NONE', *, *, #69179, .T. ) ;
#24502 = CARTESIAN_POINT ( 'NONE',  ( -8.079219948824906794, 8.697938382363059162, 54.00000000000000711 ) ) ;
#24504 = VERTEX_POINT ( 'NONE', #64596 ) ;
#24505 = DIRECTION ( 'NONE',  ( 0.000000000000000000, 0.000000000000000000, -1.000000000000000000 ) ) ;
#24506 = FACE_OUTER_BOUND ( 'NONE', #24958, .T. ) ;
#24507 = DIRECTION ( 'NONE',  ( 1.000000000000000000, -0.000000000000000000, 0.000000000000000000 ) ) ;
#24508 = DIRECTION ( 'NONE',  ( 0.000000000000000000, 1.000000000000000000, 0.000000000000000000 ) ) ;
#24509 = VECTOR ( 'NONE', #58753, 1000.000000000000000 ) ;
#24510 = FACE_OUTER_BOUND ( 'NONE', #11128, .T. ) ;
#24511 = ADVANCED_FACE ( 'NONE', ( #43368 ), #10847, .T. ) ;
#24512 = LINE ( 'NONE', #46416, #33226 ) ;
#24513 = EDGE_LOOP ( 'NONE', ( #20494, #59402, #35020, #51683 ) ) ;
#24514 = VERTEX_POINT ( 'NONE', #12143 ) ;
#24515 = VERTEX_POINT ( 'NONE', #16157 ) ;
#24516 = AXIS2_PLACEMENT_3D ( 'NONE', #23240, #12963, #18272 ) ;
#24517 = AXIS2_PLACEMENT_3D ( 'NONE', #42026, #63606, #63249 ) ;
#24518 = ORIENTED_EDGE ( 'NONE', *, *, #50520, .T. ) ;
#24519 = EDGE_CURVE ( 'NONE', #10256, #44295, #59289, .T. ) ;
#24520 = LINE ( 'NONE', #46078, #67226 ) ;
#24521 = CARTESIAN_POINT ( 'NONE',  ( 8.406483450353379183, -7.616533956692325802, 455.0000000000000568 ) ) ;
#24522 = AXIS2_PLACEMENT_3D ( 'NONE', #34370, #35791, #13172 ) ;
#24523 = VECTOR ( 'NONE', #52915, 1000.000000000000000 ) ;
#24524 = DIRECTION ( 'NONE',  ( 0.000000000000000000, -1.000000000000000000, -1.880440247955360336E-12 ) ) ;
#24525 = AXIS2_PLACEMENT_3D ( 'NONE', #30518, #37237, #35819 ) ;
#24526 = VERTEX_POINT ( 'NONE', #60584 ) ;
#24528 = EDGE_CURVE ( 'NONE', #41197, #59963, #26776, .T. ) ;
#24527 = VERTEX_POINT ( 'NONE', #39020 ) ;
#24529 = ORIENTED_EDGE ( 'NONE', *, *, #59604, .T. ) ;
#24530 = CARTESIAN_POINT ( 'NONE',  ( 25.50000000000000355, 0.000000000000000000, -20.87899999999999778 ) ) ;
#24531 = VECTOR ( 'NONE', #33076, 1000.000000000000000 ) ;
#24532 = VECTOR ( 'NONE', #50151, 1000.000000000000000 ) ;
#24533 = VERTEX_POINT ( 'NONE', #39705 ) ;
#24534 = ORIENTED_EDGE ( 'NONE', *, *, #50212, .F. ) ;
#24535 = DIRECTION ( 'NONE',  ( 0.000000000000000000, 0.7071067811865495711, -0.7071067811865455743 ) ) ;
#24536 = EDGE_CURVE ( 'NONE', #50773, #64510, #61260, .T. ) ;
#24537 = VERTEX_POINT ( 'NONE', #12821 ) ;
#24538 = EDGE_LOOP ( 'NONE', ( #20406, #53735, #35548, #10441 ) ) ;
#24539 = CARTESIAN_POINT ( 'NONE',  ( -15.50000000000000000, -0.2038245569916614930, -23.94337567297399971 ) ) ;
#24541 = VERTEX_POINT ( 'NONE', #21807 ) ;
#24540 = CARTESIAN_POINT ( 'NONE',  ( 35.89999999999999858, -0.1999999999911430404, -8.864436962241481021E-12 ) ) ;
#24542 = EDGE_LOOP ( 'NONE', ( #40297, #38524, #10619, #52676 ) ) ;
#24543 = DIRECTION ( 'NONE',  ( 0.000000000000000000, 0.000000000000000000, -1.000000000000000000 ) ) ;
#24544 = CARTESIAN_POINT ( 'NONE',  ( 283.0000000000000568, -38.15000000000000568, -14.50000000000000000 ) ) ;
#24545 = EDGE_CURVE ( 'NONE', #56003, #69389, #6830, .T. ) ;
#24546 = FACE_OUTER_BOUND ( 'NONE', #9118, .T. ) ;
#24548 = EDGE_LOOP ( 'NONE', ( #29238, #38820, #46734, #49925 ) ) ;
#24547 = DIRECTION ( 'NONE',  ( 0.000000000000000000, 1.000000000000000000, 0.000000000000000000 ) ) ;
#24549 = ORIENTED_EDGE ( 'NONE', *, *, #64059, .T. ) ;
#24550 = CARTESIAN_POINT ( 'NONE',  ( 9.795823737882807691, 10.49297626211718537, 54.00000000000000711 ) ) ;
#24551 = PLANE ( 'NONE',  #9705 ) ;
#24552 = DIRECTION ( 'NONE',  ( -9.050731179009442381E-15, -1.000000000000000000, 0.000000000000000000 ) ) ;
#24553 = ADVANCED_FACE ( 'NONE', ( #32432 ), #60923, .F. ) ;
#24554 = ORIENTED_EDGE ( 'NONE', *, *, #35327, .F. ) ;
#24555 = LINE ( 'NONE', #4042, #52958 ) ;
#24556 = ADVANCED_FACE ( 'NONE', ( #5552 ), #17803, .F. ) ;
#24557 = LINE ( 'NONE', #25257, #51321 ) ;
#24558 = LINE ( 'NONE', #13939, #26640 ) ;
#24559 = AXIS2_PLACEMENT_3D ( 'NONE', #15544, #21869, #21523 ) ;
#24560 = ORIENTED_EDGE ( 'NONE', *, *, #44430, .T. ) ;
#24561 = DIRECTION ( 'NONE',  ( -1.000000000000000000, 0.000000000000000000, 0.000000000000000000 ) ) ;
#24562 = DIRECTION ( 'NONE',  ( 0.000000000000000000, -0.7071067811865474617, 0.7071067811865474617 ) ) ;
#24563 = CARTESIAN_POINT ( 'NONE',  ( 40.90000000000000568, 13.66939075806899240, -20.79999999999999361 ) ) ;
#24564 = LINE ( 'NONE', #13944, #13314 ) ;
#24565 = ORIENTED_EDGE ( 'NONE', *, *, #9376, .F. ) ;
#24566 = AXIS2_PLACEMENT_3D ( 'NONE', #24708, #19394, #9148 ) ;
#24567 = VECTOR ( 'NONE', #33082, 1000.000000000000000 ) ;
#24568 = CIRCLE ( 'NONE', #7590, 1.000000000000000000 ) ;
#24569 = LINE ( 'NONE', #57434, #30159 ) ;
#24570 = FACE_OUTER_BOUND ( 'NONE', #47753, .T. ) ;
#24571 = VECTOR ( 'NONE', #49201, 1000.000000000000000 ) ;
#24572 = VECTOR ( 'NONE', #54908, 1000.000000000000000 ) ;
#24573 = ORIENTED_EDGE ( 'NONE', *, *, #20699, .F. ) ;
#24574 = CARTESIAN_POINT ( 'NONE',  ( -7.450000000000001954, 0.000000000000000000, -9.500000000000001776 ) ) ;
#24575 = CARTESIAN_POINT ( 'NONE',  ( -7.250000000000000888, 7.450000000000003730, -24.50000000000000000 ) ) ;
#24576 = CARTESIAN_POINT ( 'NONE',  ( 11.75000000000000000, -5.200000000000001066, -11.75000000000000000 ) ) ;
#24577 = AXIS2_PLACEMENT_3D ( 'NONE', #60557, #1502, #66214 ) ;
#24578 = CARTESIAN_POINT ( 'NONE',  ( -30.00000000000000000, -17.00000000000000000, -15.70499999999969809 ) ) ;
#24579 = VECTOR ( 'NONE', #12231, 1000.000000000000000 ) ;
#24580 = CARTESIAN_POINT ( 'NONE',  ( 21.90000000000000213, -0.1999999999911430404, -8.864436962241481021E-12 ) ) ;
#24581 = ORIENTED_EDGE ( 'NONE', *, *, #37549, .T. ) ;
#24582 = CARTESIAN_POINT ( 'NONE',  ( -7.250000000000001776, -7.249999999999998224, -15.00000000000000000 ) ) ;
#24583 = DIRECTION ( 'NONE',  ( 0.000000000000000000, 0.000000000000000000, 1.000000000000000000 ) ) ;
#24584 = CARTESIAN_POINT ( 'NONE',  ( -30.00000000000000000, -17.35230188589299871, 15.35019951917099945 ) ) ;
#24585 = EDGE_CURVE ( 'NONE', #35090, #5797, #51777, .T. ) ;
#24586 = CARTESIAN_POINT ( 'NONE',  ( 7.250000000000005329, -8.249999999999998224, -25.00000000000000000 ) ) ;
#24587 = CARTESIAN_POINT ( 'NONE',  ( 25.50000000000000355, -5.578999999999999737, 24.12099999999999866 ) ) ;
#24588 = VERTEX_POINT ( 'NONE', #246 ) ;
#24590 = ORIENTED_EDGE ( 'NONE', *, *, #56112, .T. ) ;
#24589 = DIRECTION ( 'NONE',  ( 0.000000000000000000, 1.000000000000000000, 0.000000000000000000 ) ) ;
#24591 = EDGE_CURVE ( 'NONE', #10643, #33426, #17447, .T. ) ;
#24592 = AXIS2_PLACEMENT_3D ( 'NONE', #3082, #55429, #56803 ) ;
#24593 = CARTESIAN_POINT ( 'NONE',  ( 30.00000000000000000, -11.10796162543699950, -9.102987789146602893 ) ) ;
#24594 = DIRECTION ( 'NONE',  ( -0.000000000000000000, 3.673940397442059868E-16, -1.000000000000000000 ) ) ;
#24595 = DIRECTION ( 'NONE',  ( 0.000000000000000000, 0.7071067811865474617, -0.7071067811865474617 ) ) ;
#24596 = ORIENTED_EDGE ( 'NONE', *, *, #30793, .T. ) ;
#24597 = EDGE_CURVE ( 'NONE', #42376, #42028, #29188, .T. ) ;
#24598 = DIRECTION ( 'NONE',  ( 0.000000000000000000, -0.1249999999999996531, -0.9921567416492215186 ) ) ;
#24599 = EDGE_CURVE ( 'NONE', #4106, #29489, #15651, .T. ) ;
#24600 = ORIENTED_EDGE ( 'NONE', *, *, #36262, .F. ) ;
#24601 = ORIENTED_EDGE ( 'NONE', *, *, #29347, .T. ) ;
#24602 = EDGE_CURVE ( 'NONE', #49081, #42236, #34386, .T. ) ;
#24603 = ORIENTED_EDGE ( 'NONE', *, *, #15083, .T. ) ;
#24604 = CARTESIAN_POINT ( 'NONE',  ( 35.89999999999999858, -0.1999999999911795112, 8.826273045769999343E-12 ) ) ;
#24605 = LINE ( 'NONE', #56077, #7142 ) ;
#24606 = FACE_OUTER_BOUND ( 'NONE', #67842, .T. ) ;
#24607 = CARTESIAN_POINT ( 'NONE',  ( 283.0000000000000568, -42.00000000000000000, -15.00000000000000000 ) ) ;
#24608 = CIRCLE ( 'NONE', #67513, 24.99999999998794920 ) ;
#24609 = VERTEX_POINT ( 'NONE', #21459 ) ;
#24610 = EDGE_CURVE ( 'NONE', #27121, #35722, #9998, .T. ) ;
#24611 = VERTEX_POINT ( 'NONE', #69558 ) ;
#24612 = LINE ( 'NONE', #67735, #50461 ) ;
#24613 = EDGE_CURVE ( 'NONE', #12341, #28734, #64258, .T. ) ;
#24614 = CARTESIAN_POINT ( 'NONE',  ( -7.793516549646829716, -11.32648345035340576, 455.0000000000000568 ) ) ;
#24615 = VERTEX_POINT ( 'NONE', #15809 ) ;
#24616 = ADVANCED_FACE ( 'NONE', ( #10499 ), #5211, .F. ) ;
#24617 = ORIENTED_EDGE ( 'NONE', *, *, #66657, .T. ) ;
#24618 = ADVANCED_FACE ( 'NONE', ( #13886 ), #51729, .T. ) ;
#24619 = EDGE_CURVE ( 'NONE', #34317, #22594, #60791, .T. ) ;
#24620 = ORIENTED_EDGE ( 'NONE', *, *, #52744, .T. ) ;
#24621 = LINE ( 'NONE', #29907, #25979 ) ;
#24623 = EDGE_LOOP ( 'NONE', ( #52628, #53251, #56658, #66634 ) ) ;
#24622 = DIRECTION ( 'NONE',  ( 0.000000000000000000, 1.000000000000000000, 0.000000000000000000 ) ) ;
#24624 = EDGE_CURVE ( 'NONE', #31019, #62485, #66926, .T. ) ;
#24625 = AXIS2_PLACEMENT_3D ( 'NONE', #9549, #31126, #30765 ) ;
#24626 = CARTESIAN_POINT ( 'NONE',  ( 8.930623737882848800, 10.03972626211715635, 54.00000000000000711 ) ) ;
#24627 = CARTESIAN_POINT ( 'NONE',  ( 0.000000000000000000, -7.449999999999998401, -10.50000000000000000 ) ) ;
#24628 = ORIENTED_EDGE ( 'NONE', *, *, #18273, .F. ) ;
#24629 = ORIENTED_EDGE ( 'NONE', *, *, #5875, .F. ) ;
#24630 = AXIS2_PLACEMENT_3D ( 'NONE', #51231, #2787, #24365 ) ;
#24631 = CARTESIAN_POINT ( 'NONE',  ( 9.737023737882816832, -3.682023737882826886, 54.00000000000000711 ) ) ;
#24632 = DIRECTION ( 'NONE',  ( -1.836970198721029934E-16, 1.836970198721036344E-16, -1.000000000000000000 ) ) ;
#24633 = EDGE_CURVE ( 'NONE', #55193, #66404, #12229, .T. ) ;
#24634 = DIRECTION ( 'NONE',  ( 0.000000000000000000, 0.000000000000000000, -1.000000000000000000 ) ) ;
#24635 = ADVANCED_FACE ( 'NONE', ( #67638 ), #57019, .F. ) ;
#24636 = AXIS2_PLACEMENT_3D ( 'NONE', #24907, #52130, #19596 ) ;
#24637 = DIRECTION ( 'NONE',  ( 1.836970198721029934E-16, 1.836970198721010706E-16, -1.000000000000000000 ) ) ;
#24638 = CARTESIAN_POINT ( 'NONE',  ( -1.991476262117310325, -8.612468434717257537, 26.00000000000000711 ) ) ;
#24640 = ORIENTED_EDGE ( 'NONE', *, *, #37321, .F. ) ;
#24639 = DIRECTION ( 'NONE',  ( 1.836970198721029934E-16, 1.836970198721010706E-16, -1.000000000000000000 ) ) ;
#24641 = EDGE_LOOP ( 'NONE', ( #51916, #67604, #57015, #50479 ) ) ;
#24642 = LINE ( 'NONE', #2703, #60311 ) ;
#24643 = DIRECTION ( 'NONE',  ( 1.000000000000000000, -0.000000000000000000, 0.000000000000000000 ) ) ;
#24644 = DIRECTION ( 'NONE',  ( 1.000000000000000000, -0.000000000000000000, -0.000000000000000000 ) ) ;
#24645 = DIRECTION ( 'NONE',  ( 1.000000000000000000, 0.000000000000000000, 0.000000000000000000 ) ) ;
#24646 = CARTESIAN_POINT ( 'NONE',  ( 11.78648345035337996, 4.393516549646516722, 455.0000000000000568 ) ) ;
#24647 = VERTEX_POINT ( 'NONE', #29798 ) ;
#24648 = CARTESIAN_POINT ( 'NONE',  ( -9.547976262117304103, -7.969523737882760805, 54.00000000000000711 ) ) ;
#24649 = DIRECTION ( 'NONE',  ( -1.000000000000000000, 0.000000000000000000, 0.000000000000000000 ) ) ;
#24650 = CARTESIAN_POINT ( 'NONE',  ( 15.00000000000000000, -0.5000000000000000000, 30.00000000000000000 ) ) ;
#24651 = FACE_OUTER_BOUND ( 'NONE', #34261, .T. ) ;
#24652 = CARTESIAN_POINT ( 'NONE',  ( -9.249999999999998224, 8.250000000000001776, -5.000000000000000000 ) ) ;
#24653 = CARTESIAN_POINT ( 'NONE',  ( -8.333516549646715177, 11.11351654964659907, 455.0000000000000568 ) ) ;
#24654 = DIRECTION ( 'NONE',  ( 1.000000000000000000, 0.000000000000000000, 0.000000000000000000 ) ) ;
#24655 = EDGE_LOOP ( 'NONE', ( #61893, #1716, #20841, #35562, #52620, #60942 ) ) ;
#24656 = DIRECTION ( 'NONE',  ( -1.819560449471430698E-15, -1.000000000000000000, 0.000000000000000000 ) ) ;
#24657 = DIRECTION ( 'NONE',  ( -1.084202172485511060E-14, -1.000000000000000000, 0.000000000000000000 ) ) ;
#24658 = EDGE_LOOP ( 'NONE', ( #19772, #20097, #34117, #33953 ) ) ;
#24659 = DIRECTION ( 'NONE',  ( -1.000000000000000000, 1.349135440953254805E-14, -1.836970198721005529E-16 ) ) ;
#24660 = CARTESIAN_POINT ( 'NONE',  ( 283.0000000000000568, -26.28355339059299922, -9.766446609406699508 ) ) ;
#24661 = CARTESIAN_POINT ( 'NONE',  ( -8.198316549646726514, -6.006483450353354847, 195.0000000000000284 ) ) ;
#24662 = CARTESIAN_POINT ( 'NONE',  ( -11.00000000000000000, -8.959999999999999076, -12.95475478405700009 ) ) ;
#24663 = DIRECTION ( 'NONE',  ( 1.000000000000000000, 0.000000000000000000, 0.000000000000000000 ) ) ;
#24664 = VERTEX_POINT ( 'NONE', #8580 ) ;
#24665 = VECTOR ( 'NONE', #21120, 1000.000000000000114 ) ;
#24666 = EDGE_CURVE ( 'NONE', #8384, #24071, #42739, .T. ) ;
#24667 = DIRECTION ( 'NONE',  ( 3.596772705736698833E-15, 1.000000000000000000, 0.000000000000000000 ) ) ;
#24668 = ORIENTED_EDGE ( 'NONE', *, *, #7597, .T. ) ;
#24669 = DIRECTION ( 'NONE',  ( -1.000000000000000000, 8.339399738404099512E-15, -1.836970198721014650E-16 ) ) ;
#24670 = LINE ( 'NONE', #39860, #45799 ) ;
#24671 = ORIENTED_EDGE ( 'NONE', *, *, #27336, .T. ) ;
#24672 = EDGE_CURVE ( 'NONE', #34593, #31382, #2581, .T. ) ;
#24673 = DIRECTION ( 'NONE',  ( 1.000000000000000000, -3.491481338843133355E-15, -1.836970198721036344E-16 ) ) ;
#24674 = CIRCLE ( 'NONE', #59704, 0.2000000000000005107 ) ;
#24675 = EDGE_CURVE ( 'NONE', #51724, #41366, #35093, .T. ) ;
#24676 = ORIENTED_EDGE ( 'NONE', *, *, #22046, .F. ) ;
#24677 = DIRECTION ( 'NONE',  ( 1.000000000000000000, -0.000000000000000000, -0.000000000000000000 ) ) ;
#24678 = EDGE_LOOP ( 'NONE', ( #43104, #64403, #24783, #40917 ) ) ;
#24679 = EDGE_CURVE ( 'NONE', #48765, #68595, #39343, .T. ) ;
#24680 = VERTEX_POINT ( 'NONE', #51367 ) ;
#24681 = LINE ( 'NONE', #68518, #7992 ) ;
#24682 = VERTEX_POINT ( 'NONE', #29448 ) ;
#24683 = ORIENTED_EDGE ( 'NONE', *, *, #62949, .F. ) ;
#24684 = CIRCLE ( 'NONE', #17908, 24.99999999998789946 ) ;
#24685 = CARTESIAN_POINT ( 'NONE',  ( 4.747751991980655895, 6.606374702650043673, 455.0000000000000568 ) ) ;
#24686 = CARTESIAN_POINT ( 'NONE',  ( 11.12648345035337627, -2.906483450353491094, 455.0000000000000568 ) ) ;
#24687 = PLANE ( 'NONE',  #35519 ) ;
#24688 = VERTEX_POINT ( 'NONE', #19192 ) ;
#24689 = CARTESIAN_POINT ( 'NONE',  ( 8.930623737882818602, -8.930623737882845248, 26.00000000000000000 ) ) ;
#24691 = CARTESIAN_POINT ( 'NONE',  ( -8.079219948824956532, -8.711985858128644011, 26.00000000000000000 ) ) ;
#24690 = DIRECTION ( 'NONE',  ( -0.5773502691896257311, -0.5773502691896257311, 0.5773502691896257311 ) ) ;
#24692 = ORIENTED_EDGE ( 'NONE', *, *, #17512, .T. ) ;
#24694 = ORIENTED_EDGE ( 'NONE', *, *, #4372, .T. ) ;
#24693 = DIRECTION ( 'NONE',  ( -0.7071067811865470176, 0.000000000000000000, 0.7071067811865480168 ) ) ;
#24695 = ORIENTED_EDGE ( 'NONE', *, *, #64605, .T. ) ;
#24696 = EDGE_CURVE ( 'NONE', #24963, #33875, #62671, .T. ) ;
#24697 = APPLICATION_PROTOCOL_DEFINITION ( 'draft international standard', 'automotive_design', 1998, #45367 ) ;
#24698 = LINE ( 'NONE', #2771, #17494 ) ;
#24700 = ORIENTED_EDGE ( 'NONE', *, *, #47324, .F. ) ;
#24699 = CARTESIAN_POINT ( 'NONE',  ( 7.969523737882809655, 8.821682069070714505, 26.00000000000000711 ) ) ;
#24701 = DIRECTION ( 'NONE',  ( -1.000000000000000000, 0.000000000000000000, 0.000000000000000000 ) ) ;
#24702 = LINE ( 'NONE', #14086, #44118 ) ;
#24703 = ORIENTED_EDGE ( 'NONE', *, *, #68283, .T. ) ;
#24704 = ORIENTED_EDGE ( 'NONE', *, *, #27187, .F. ) ;
#24705 = CARTESIAN_POINT ( 'NONE',  ( -10.50000000000000178, 9.690000000000001279, -4.250000000000000000 ) ) ;
#24706 = ORIENTED_EDGE ( 'NONE', *, *, #18507, .T. ) ;
#24707 = AXIS2_PLACEMENT_3D ( 'NONE', #34488, #56079, #28494 ) ;
#24708 = CARTESIAN_POINT ( 'NONE',  ( 49.00000000000000000, -14.06939075806900163, -20.80000000000000426 ) ) ;
#24709 = CARTESIAN_POINT ( 'NONE',  ( 41.09999999999999432, 20.60000000000000142, 13.86939075806900057 ) ) ;
#24710 = DIRECTION ( 'NONE',  ( 0.000000000000000000, 1.000000000000000000, 0.000000000000000000 ) ) ;
#24711 = EDGE_CURVE ( 'NONE', #54124, #16704, #50668, .T. ) ;
#24712 = ORIENTED_EDGE ( 'NONE', *, *, #27239, .F. ) ;
#24713 = AXIS2_PLACEMENT_3D ( 'NONE', #65141, #54524, #11034 ) ;
#24714 = ADVANCED_FACE ( 'NONE', ( #40041 ), #61974, .F. ) ;
#24715 = CARTESIAN_POINT ( 'NONE',  ( -8.249999999999996447, 8.250000000000001776, 5.000000000000000000 ) ) ;
#24716 = CYLINDRICAL_SURFACE ( 'NONE', #21306, 0.1750000000000002387 ) ;
#24719 = VERTEX_POINT ( 'NONE', #52074 ) ;
#24718 = ADVANCED_FACE ( 'NONE', ( #14590 ), #67988, .T. ) ;
#24717 = DIRECTION ( 'NONE',  ( 0.000000000000000000, 0.000000000000000000, -1.000000000000000000 ) ) ;
#24721 = ORIENTED_EDGE ( 'NONE', *, *, #44744, .T. ) ;
#24720 = CARTESIAN_POINT ( 'NONE',  ( 25.57999999999999829, 3.010794155703768650E-16, -2.458500000000000796 ) ) ;
#24722 = DIRECTION ( 'NONE',  ( 1.000000000000000000, -3.491481338843133355E-15, -1.836970198721036344E-16 ) ) ;
#24723 = AXIS2_PLACEMENT_3D ( 'NONE', #34351, #17769, #60884 ) ;
#24724 = DIRECTION ( 'NONE',  ( 0.000000000000000000, 0.7071067811865474617, 0.7071067811865474617 ) ) ;
#24725 = FACE_OUTER_BOUND ( 'NONE', #11557, .T. ) ;
#24726 = LINE ( 'NONE', #9165, #59919 ) ;
#24727 = AXIS2_PLACEMENT_3D ( 'NONE', #25455, #2828, #57626 ) ;
#24728 = CARTESIAN_POINT ( 'NONE',  ( 9.841277389592654856, 2.277516549646586785, 195.0000000000000284 ) ) ;
#24729 = ORIENTED_EDGE ( 'NONE', *, *, #1530, .T. ) ;
#24730 = DIRECTION ( 'NONE',  ( -1.671920889371702854E-15, -1.000000000000000000, -3.673940397442059868E-16 ) ) ;
#24731 = DIRECTION ( 'NONE',  ( 0.000000000000000000, 0.000000000000000000, 1.000000000000000000 ) ) ;
#24732 = CARTESIAN_POINT ( 'NONE',  ( -9.791916549646810353, -10.20488345035334099, 195.0000000000000284 ) ) ;
#24734 = AXIS2_PLACEMENT_3D ( 'NONE', #43765, #60348, #54724 ) ;
#24733 = VECTOR ( 'NONE', #18630, 1000.000000000000000 ) ;
#24736 = ORIENTED_EDGE ( 'NONE', *, *, #2679, .F. ) ;
#24735 = FACE_OUTER_BOUND ( 'NONE', #39251, .T. ) ;
#24737 = DIRECTION ( 'NONE',  ( 0.000000000000000000, 0.000000000000000000, -1.000000000000000000 ) ) ;
#24738 = DIRECTION ( 'NONE',  ( -1.000000000000000000, 0.000000000000000000, 0.000000000000000000 ) ) ;
#24739 = VECTOR ( 'NONE', #57685, 1000.000000000000114 ) ;
#24740 = ORIENTED_EDGE ( 'NONE', *, *, #50614, .F. ) ;
#24741 = ORIENTED_EDGE ( 'NONE', *, *, #35118, .T. ) ;
#24742 = PLANE ( 'NONE',  #8306 ) ;
#24743 = CARTESIAN_POINT ( 'NONE',  ( -30.00000000000000000, -5.000000000000000000, 27.00000000000000000 ) ) ;
#24744 = ORIENTED_EDGE ( 'NONE', *, *, #36231, .T. ) ;
#24745 = CARTESIAN_POINT ( 'NONE',  ( 30.00000000000000000, -9.200000000000120082, 17.64999999999993108 ) ) ;
#24746 = DIRECTION ( 'NONE',  ( -1.836970198721029934E-16, 1.836970198721036590E-16, -1.000000000000000000 ) ) ;
#24747 = CARTESIAN_POINT ( 'NONE',  ( 8.406483450353356091, 6.331612867284063917, 195.0000000000000284 ) ) ;
#24748 = EDGE_CURVE ( 'NONE', #64891, #63857, #29106, .T. ) ;
#24749 = CARTESIAN_POINT ( 'NONE',  ( 24.00000000000000000, -16.28999999999999915, -14.50000000000000000 ) ) ;
#24750 = ORIENTED_EDGE ( 'NONE', *, *, #51989, .T. ) ;
#24751 = DIRECTION ( 'NONE',  ( 0.000000000000000000, -0.9921567416492215186, 0.1249999999999996531 ) ) ;
#24752 = ORIENTED_EDGE ( 'NONE', *, *, #13359, .F. ) ;
#24753 = ORIENTED_EDGE ( 'NONE', *, *, #20781, .F. ) ;
#24754 = VERTEX_POINT ( 'NONE', #56326 ) ;
#24755 = CYLINDRICAL_SURFACE ( 'NONE', #59605, 1.224999999999998757 ) ;
#24756 = EDGE_CURVE ( 'NONE', #18487, #32701, #51021, .T. ) ;
#24757 = ADVANCED_FACE ( 'NONE', ( #19895 ), #41465, .F. ) ;
#24758 = VECTOR ( 'NONE', #22773, 1000.000000000000000 ) ;
#24759 = LINE ( 'NONE', #50920, #9550 ) ;
#24760 = CARTESIAN_POINT ( 'NONE',  ( 175.4206970127264356, -30.42541106249864313, 5.000000000000000000 ) ) ;
#24761 = ORIENTED_EDGE ( 'NONE', *, *, #51593, .T. ) ;
#24762 = ADVANCED_FACE ( 'NONE', ( #68700 ), #26255, .F. ) ;
#24763 = VERTEX_POINT ( 'NONE', #16337 ) ;
#24764 = ADVANCED_FACE ( 'NONE', ( #58785 ), #63387, .F. ) ;
#24765 = DIRECTION ( 'NONE',  ( 0.000000000000000000, 0.000000000000000000, -1.000000000000000000 ) ) ;
#24766 = CIRCLE ( 'NONE', #7835, 24.99999999998794920 ) ;
#24767 = ORIENTED_EDGE ( 'NONE', *, *, #674, .F. ) ;
#24768 = AXIS2_PLACEMENT_3D ( 'NONE', #60761, #7009, #65393 ) ;
#24769 = EDGE_LOOP ( 'NONE', ( #25819, #4797, #43668, #27058 ) ) ;
#24770 = DIRECTION ( 'NONE',  ( 1.000000000000000000, 0.000000000000000000, 0.000000000000000000 ) ) ;
#24771 = CARTESIAN_POINT ( 'NONE',  ( 6.006483450353379716, -6.006483450353490738, 455.0000000000000568 ) ) ;
#24772 = FACE_OUTER_BOUND ( 'NONE', #38407, .T. ) ;
#24773 = ADVANCED_FACE ( 'NONE', ( #42857 ), #58445, .T. ) ;
#24774 = CARTESIAN_POINT ( 'NONE',  ( 4.406483450353420928, 11.31351654964658593, 455.0000000000000568 ) ) ;
#24775 = ORIENTED_EDGE ( 'NONE', *, *, #3185, .T. ) ;
#24776 = VECTOR ( 'NONE', #45581, 1000.000000000000000 ) ;
#24777 = LINE ( 'NONE', #46332, #66162 ) ;
#24779 = CYLINDRICAL_SURFACE ( 'NONE', #55911, 24.99999999998789946 ) ;
#24778 = LINE ( 'NONE', #68258, #16325 ) ;
#24780 = VERTEX_POINT ( 'NONE', #52430 ) ;
#24782 = ORIENTED_EDGE ( 'NONE', *, *, #38296, .T. ) ;
#24781 = DIRECTION ( 'NONE',  ( 0.000000000000000000, 0.000000000000000000, -1.000000000000000000 ) ) ;
#24783 = ORIENTED_EDGE ( 'NONE', *, *, #61774, .F. ) ;
#24784 = VERTEX_POINT ( 'NONE', #5033 ) ;
#24785 = TOROIDAL_SURFACE ( 'NONE', #21402, 3.299999999999470024, 0.2000000000005275058 ) ;
#24786 = LINE ( 'NONE', #8504, #1694 ) ;
#24787 = AXIS2_PLACEMENT_3D ( 'NONE', #30922, #13950, #46823 ) ;
#24788 = FACE_OUTER_BOUND ( 'NONE', #34151, .T. ) ;
#24789 = EDGE_LOOP ( 'NONE', ( #1263, #5616, #58358, #18943 ) ) ;
#24790 = ORIENTED_EDGE ( 'NONE', *, *, #23879, .T. ) ;
#24791 = AXIS2_PLACEMENT_3D ( 'NONE', #63215, #51562, #35630 ) ;
#24792 = DIRECTION ( 'NONE',  ( -1.000000000000000000, 0.000000000000000000, 0.000000000000000000 ) ) ;
#24793 = DIRECTION ( 'NONE',  ( 0.000000000000000000, 0.000000000000000000, -1.000000000000000000 ) ) ;
#24794 = VERTEX_POINT ( 'NONE', #3991 ) ;
#24795 = VERTEX_POINT ( 'NONE', #15996 ) ;
#24796 = DIRECTION ( 'NONE',  ( 0.000000000000000000, -1.000000000000000000, 0.000000000000000000 ) ) ;
#24797 = DIRECTION ( 'NONE',  ( 1.000000000000000000, 0.000000000000000000, 0.000000000000000000 ) ) ;
#24798 = ORIENTED_EDGE ( 'NONE', *, *, #34476, .T. ) ;
#24799 = FACE_OUTER_BOUND ( 'NONE', #56091, .T. ) ;
#24800 = CIRCLE ( 'NONE', #33820, 2.000000000000001776 ) ;
#24801 = LINE ( 'NONE', #57674, #28292 ) ;
#24804 = ORIENTED_EDGE ( 'NONE', *, *, #19778, .T. ) ;
#24803 = EDGE_CURVE ( 'NONE', #25888, #20510, #54109, .T. ) ;
#24802 = CARTESIAN_POINT ( 'NONE',  ( 283.0000000000000568, -37.15000000000001279, -7.700000000000000178 ) ) ;
#24805 = ORIENTED_EDGE ( 'NONE', *, *, #47778, .T. ) ;
#24806 = EDGE_CURVE ( 'NONE', #14976, #41912, #4356, .T. ) ;
#24807 = CARTESIAN_POINT ( 'NONE',  ( -10.73351654964668533, -1.090483450353341155, 455.0000000000000568 ) ) ;
#24808 = FACE_OUTER_BOUND ( 'NONE', #22226, .T. ) ;
#24809 = DIRECTION ( 'NONE',  ( -1.000000000000000000, 0.000000000000000000, 0.000000000000000000 ) ) ;
#24810 = DIRECTION ( 'NONE',  ( 0.000000000000000000, 0.000000000000000000, -1.000000000000000000 ) ) ;
#24811 = LINE ( 'NONE', #46368, #61763 ) ;
#24812 = ADVANCED_FACE ( 'NONE', ( #14948 ), #19107, .F. ) ;
#24813 = DIRECTION ( 'NONE',  ( 0.000000000000000000, -1.000000000000000000, 0.000000000000000000 ) ) ;
#24814 = CARTESIAN_POINT ( 'NONE',  ( -23.75054448485400016, -15.50000000000000000, 25.53140320652400064 ) ) ;
#24815 = ORIENTED_EDGE ( 'NONE', *, *, #63353, .T. ) ;
#24816 = CARTESIAN_POINT ( 'NONE',  ( -10.49297626211726175, 3.650476262117184234, 26.00000000000000711 ) ) ;
#24817 = VECTOR ( 'NONE', #11868, 1000.000000000000000 ) ;
#24819 = ORIENTED_EDGE ( 'NONE', *, *, #31518, .F. ) ;
#24818 = DIRECTION ( 'NONE',  ( 1.000000000000000000, 0.000000000000000000, 0.000000000000000000 ) ) ;
#24820 = DIRECTION ( 'NONE',  ( 0.000000000000000000, 0.000000000000000000, -1.000000000000000000 ) ) ;
#24821 = DIRECTION ( 'NONE',  ( 0.000000000000000000, 1.000000000000000000, 0.000000000000000000 ) ) ;
#24822 = DIRECTION ( 'NONE',  ( -1.047444401652939849E-14, -1.000000000000000000, 0.000000000000000000 ) ) ;
#24823 = DIRECTION ( 'NONE',  ( 0.000000000000000000, -1.000000000000000000, 0.000000000000000000 ) ) ;
#24824 = VECTOR ( 'NONE', #62106, 1000.000000000000000 ) ;
#24825 = CARTESIAN_POINT ( 'NONE',  ( -3.417780618358674971, -7.852485183456956896, 195.0000000000000284 ) ) ;
#24826 = VERTEX_POINT ( 'NONE', #10681 ) ;
#24827 = DIRECTION ( 'NONE',  ( 0.000000000000000000, 0.000000000000000000, 1.000000000000000000 ) ) ;
#24828 = DIRECTION ( 'NONE',  ( -0.6414496315691367023, 0.7671651518153173033, 0.000000000000000000 ) ) ;
#24829 = EDGE_LOOP ( 'NONE', ( #5530, #47834, #49944, #17546, #19200, #27391 ) ) ;
#24830 = AXIS2_PLACEMENT_3D ( 'NONE', #3888, #7772, #2823 ) ;
#24831 = LINE ( 'NONE', #19514, #60686 ) ;
#24832 = CIRCLE ( 'NONE', #53123, 0.6000000000000006439 ) ;
#24833 = AXIS2_PLACEMENT_3D ( 'NONE', #48585, #16407, #862 ) ;
#24834 = DIRECTION ( 'NONE',  ( 0.000000000000000000, 0.000000000000000000, -1.000000000000000000 ) ) ;
#24835 = ORIENTED_EDGE ( 'NONE', *, *, #49300, .T. ) ;
#24836 = LINE ( 'NONE', #41793, #36131 ) ;
#24837 = VERTEX_POINT ( 'NONE', #47811 ) ;
#24838 = ORIENTED_EDGE ( 'NONE', *, *, #61774, .T. ) ;
#24839 = CARTESIAN_POINT ( 'NONE',  ( -8.250000000000001776, 0.000000000000000000, -21.50000000000000000 ) ) ;
#24840 = CIRCLE ( 'NONE', #42913, 0.1999999999999996503 ) ;
#24841 = CARTESIAN_POINT ( 'NONE',  ( -9.293516549646817282, -10.09643294401455904, 455.0000000000000568 ) ) ;
#24842 = CARTESIAN_POINT ( 'NONE',  ( -10.30047626211725742, 6.835476262117182955, 54.00000000000000711 ) ) ;
#24843 = DIRECTION ( 'NONE',  ( -1.000000000000000000, 0.000000000000000000, 0.000000000000000000 ) ) ;
#24844 = DIRECTION ( 'NONE',  ( -1.794541526872559352E-16, -1.000000000000000000, 0.000000000000000000 ) ) ;
#24845 = VERTEX_POINT ( 'NONE', #57721 ) ;
#24846 = ORIENTED_EDGE ( 'NONE', *, *, #39473, .T. ) ;
#24847 = ADVANCED_FACE ( 'NONE', ( #26602 ), #9290, .T. ) ;
#24849 = ORIENTED_EDGE ( 'NONE', *, *, #4855, .F. ) ;
#24848 = CARTESIAN_POINT ( 'NONE',  ( 11.48848345035337104, 10.19191654964660820, 195.0000000000000284 ) ) ;
#24850 = ORIENTED_EDGE ( 'NONE', *, *, #65663, .F. ) ;
#24851 = DIRECTION ( 'NONE',  ( 1.836970198721029934E-16, 1.836970198721010706E-16, -1.000000000000000000 ) ) ;
#24852 = CARTESIAN_POINT ( 'NONE',  ( 11.50000000000000000, -11.50000000000100009, 15.00000000000084910 ) ) ;
#24853 = EDGE_CURVE ( 'NONE', #17390, #11892, #6639, .T. ) ;
#24854 = CARTESIAN_POINT ( 'NONE',  ( 15.50000000000000000, -0.1999999999999999556, 21.05000000000000426 ) ) ;
#24855 = AXIS2_PLACEMENT_3D ( 'NONE', #45116, #18245, #7640 ) ;
#24856 = FACE_OUTER_BOUND ( 'NONE', #14469, .T. ) ;
#24857 = EDGE_CURVE ( 'NONE', #59597, #9482, #9647, .T. ) ;
#24858 = DIRECTION ( 'NONE',  ( 0.000000000000000000, 0.7057491738665938596, 0.7084617869628679898 ) ) ;
#24859 = ORIENTED_EDGE ( 'NONE', *, *, #66500, .F. ) ;
#24860 = EDGE_LOOP ( 'NONE', ( #31188, #4228, #67981, #1444 ) ) ;
#24861 = ORIENTED_EDGE ( 'NONE', *, *, #25843, .F. ) ;
#24862 = ORIENTED_EDGE ( 'NONE', *, *, #51681, .F. ) ;
#24863 = CYLINDRICAL_SURFACE ( 'NONE', #25396, 0.1999999999999987899 ) ;
#24864 = LINE ( 'NONE', #63048, #47894 ) ;
#24865 = VECTOR ( 'NONE', #39365, 1000.000000000000114 ) ;
#24866 = EDGE_CURVE ( 'NONE', #63673, #66056, #16846, .T. ) ;
#24867 = DIRECTION ( 'NONE',  ( -1.836970198721029934E-16, -1.836970198721010706E-16, 1.000000000000000000 ) ) ;
#24868 = VECTOR ( 'NONE', #36309, 1000.000000000000000 ) ;
#24869 = VERTEX_POINT ( 'NONE', #69034 ) ;
#24870 = ORIENTED_EDGE ( 'NONE', *, *, #61649, .T. ) ;
#24871 = EDGE_LOOP ( 'NONE', ( #54451, #35925, #20755, #64450 ) ) ;
#24872 = CIRCLE ( 'NONE', #44096, 1.399999999999998579 ) ;
#24873 = CARTESIAN_POINT ( 'NONE',  ( -7.249999999999995559, 8.250000000000001776, 5.000000000000000000 ) ) ;
#24874 = ORIENTED_EDGE ( 'NONE', *, *, #5256, .T. ) ;
#24875 = ORIENTED_EDGE ( 'NONE', *, *, #57857, .T. ) ;
#24876 = LINE ( 'NONE', #41132, #31099 ) ;
#24877 = EDGE_LOOP ( 'NONE', ( #17718, #26543, #3737, #33962 ) ) ;
#24878 = VECTOR ( 'NONE', #5291, 1000.000000000000000 ) ;
#24879 = VERTEX_POINT ( 'NONE', #20591 ) ;
#24880 = PLANE ( 'NONE',  #24881 ) ;
#24881 = AXIS2_PLACEMENT_3D ( 'NONE', #19566, #41135, #2606 ) ;
#24883 = ORIENTED_EDGE ( 'NONE', *, *, #45821, .T. ) ;
#24882 = DIRECTION ( 'NONE',  ( 0.000000000000000000, 0.000000000000000000, 1.000000000000000000 ) ) ;
#24884 = ORIENTED_EDGE ( 'NONE', *, *, #55797, .F. ) ;
#24885 = PLANE ( 'NONE',  #28907 ) ;
#24886 = DIRECTION ( 'NONE',  ( 1.000000000000000000, -0.000000000000000000, 0.000000000000000000 ) ) ;
#24887 = CARTESIAN_POINT ( 'NONE',  ( 50.83090410532631864, 3.657408540445007628, 10.00000000000000000 ) ) ;
#24889 = ORIENTED_EDGE ( 'NONE', *, *, #68744, .F. ) ;
#24888 = DIRECTION ( 'NONE',  ( -3.491481338843132961E-15, -1.000000000000000000, -1.836970198721029934E-16 ) ) ;
#24890 = VERTEX_POINT ( 'NONE', #42158 ) ;
#24891 = CIRCLE ( 'NONE', #49716, 4.000000000000000000 ) ;
#24892 = CARTESIAN_POINT ( 'NONE',  ( 7.000000000000000000, -26.28355339059299922, -9.766446609406699508 ) ) ;
#24893 = AXIS2_PLACEMENT_3D ( 'NONE', #27830, #43743, #60690 ) ;
#24894 = LINE ( 'NONE', #69076, #40808 ) ;
#24895 = DIRECTION ( 'NONE',  ( -1.000000000000000000, 0.000000000000000000, 0.000000000000000000 ) ) ;
#24896 = EDGE_CURVE ( 'NONE', #8571, #19298, #2146, .T. ) ;
#24897 = LINE ( 'NONE', #57420, #45153 ) ;
#24898 = ORIENTED_EDGE ( 'NONE', *, *, #63069, .F. ) ;
#24899 = CARTESIAN_POINT ( 'NONE',  ( 7.450000000000004619, -1.336933437520057563E-15, -9.000000000000001776 ) ) ;
#24900 = DIRECTION ( 'NONE',  ( 0.000000000000000000, 0.000000000000000000, -1.000000000000000000 ) ) ;
#24901 = CARTESIAN_POINT ( 'NONE',  ( 50.00000000000000711, 0.7500000000000000000, -4.943429983321300902 ) ) ;
#24902 = AXIS2_PLACEMENT_3D ( 'NONE', #10703, #59497, #11396 ) ;
#24903 = ORIENTED_EDGE ( 'NONE', *, *, #10326, .F. ) ;
#24904 = PLANE ( 'NONE',  #3128 ) ;
#24905 = DIRECTION ( 'NONE',  ( 0.000000000000000000, 0.000000000000000000, -1.000000000000000000 ) ) ;
#24906 = EDGE_CURVE ( 'NONE', #55585, #57937, #20222, .T. ) ;
#24907 = CARTESIAN_POINT ( 'NONE',  ( -2.893516549646681035, 10.08346604330774632, 455.0000000000000568 ) ) ;
#24908 = ORIENTED_EDGE ( 'NONE', *, *, #4827, .T. ) ;
#24909 = EDGE_CURVE ( 'NONE', #64954, #58759, #19056, .T. ) ;
#24910 = DIRECTION ( 'NONE',  ( -1.836970198721029934E-16, 1.836970198721036590E-16, -1.000000000000000000 ) ) ;
#24911 = CIRCLE ( 'NONE', #67814, 0.1999999999999987899 ) ;
#24912 = PLANE ( 'NONE',  #61559 ) ;
#24913 = AXIS2_PLACEMENT_3D ( 'NONE', #41755, #63333, #37175 ) ;
#24914 = DIRECTION ( 'NONE',  ( -1.000000000000000000, 0.000000000000000000, 0.000000000000000000 ) ) ;
#24915 = ORIENTED_EDGE ( 'NONE', *, *, #59107, .F. ) ;
#24916 = FACE_OUTER_BOUND ( 'NONE', #26079, .T. ) ;
#24917 = DIRECTION ( 'NONE',  ( 1.836970198721029934E-16, 1.836970198721010706E-16, -1.000000000000000000 ) ) ;
#24918 = CARTESIAN_POINT ( 'NONE',  ( 10.00000000000000000, -21.00000000000000000, -18.00000000000000355 ) ) ;
#24919 = VECTOR ( 'NONE', #52405, 1000.000000000000000 ) ;
#24920 = DIRECTION ( 'NONE',  ( 0.000000000000000000, 0.000000000000000000, 1.000000000000000000 ) ) ;
#24921 = CARTESIAN_POINT ( 'NONE',  ( 36.90000000000000568, -14.06939075806902117, -20.80000000000000426 ) ) ;
#24922 = ORIENTED_EDGE ( 'NONE', *, *, #43339, .F. ) ;
#24923 = CARTESIAN_POINT ( 'NONE',  ( 30.00000000000000000, -12.00000000000000000, 10.69999999999999929 ) ) ;
#24924 = DIRECTION ( 'NONE',  ( 0.000000000000000000, 0.000000000000000000, -1.000000000000000000 ) ) ;
#24925 = CYLINDRICAL_SURFACE ( 'NONE', #41313, 0.5000000000001374456 ) ;
#24926 = VECTOR ( 'NONE', #7952, 1000.000000000000000 ) ;
#24927 = DIRECTION ( 'NONE',  ( 0.000000000000000000, 0.000000000000000000, -1.000000000000000000 ) ) ;
#24928 = ORIENTED_EDGE ( 'NONE', *, *, #53082, .F. ) ;
#24930 = ORIENTED_EDGE ( 'NONE', *, *, #66361, .T. ) ;
#24929 = CARTESIAN_POINT ( 'NONE',  ( 4.961189459950039904, -7.357023737882811609, 26.00000000000000000 ) ) ;
#24931 = EDGE_CURVE ( 'NONE', #36045, #37589, #4691, .T. ) ;
#24932 = LINE ( 'NONE', #13271, #59799 ) ;
#24933 = EDGE_CURVE ( 'NONE', #42376, #36190, #43552, .T. ) ;
#24934 = CARTESIAN_POINT ( 'NONE',  ( -24.00000000000000000, -15.50000000000000000, -14.50000000000000000 ) ) ;
#24935 = CARTESIAN_POINT ( 'NONE',  ( -2.530476262117325792, -9.562023737882828556, 54.00000000000000711 ) ) ;
#24936 = ORIENTED_EDGE ( 'NONE', *, *, #31085, .F. ) ;
#24937 = ADVANCED_FACE ( 'NONE', ( #22351 ), #60153, .F. ) ;
#24938 = CIRCLE ( 'NONE', #33958, 0.5999999999999989786 ) ;
#24939 = DIRECTION ( 'NONE',  ( 0.000000000000000000, 0.000000000000000000, -1.000000000000000000 ) ) ;
#24940 = EDGE_CURVE ( 'NONE', #40904, #5241, #43896, .T. ) ;
#24941 = ORIENTED_EDGE ( 'NONE', *, *, #27331, .T. ) ;
#24942 = EDGE_CURVE ( 'NONE', #5476, #65266, #15700, .T. ) ;
#24943 = ORIENTED_EDGE ( 'NONE', *, *, #55883, .F. ) ;
#24944 = ORIENTED_EDGE ( 'NONE', *, *, #46826, .T. ) ;
#24946 = EDGE_CURVE ( 'NONE', #65821, #54028, #59751, .T. ) ;
#24945 = CARTESIAN_POINT ( 'NONE',  ( -7.839518282750280065, -3.430747519065322049, 455.0000000000000568 ) ) ;
#24947 = CARTESIAN_POINT ( 'NONE',  ( 6.006483450353401921, 5.993516549646582092, 455.0000000000000568 ) ) ;
#24948 = EDGE_CURVE ( 'NONE', #34171, #66149, #12393, .T. ) ;
#24949 = DIRECTION ( 'NONE',  ( 1.000000000000000000, 0.000000000000000000, 0.000000000000000000 ) ) ;
#24950 = DIRECTION ( 'NONE',  ( 9.756599977372196271E-15, 1.000000000000000000, 0.000000000000000000 ) ) ;
#24951 = CIRCLE ( 'NONE', #47520, 0.2999999999998732569 ) ;
#24952 = ORIENTED_EDGE ( 'NONE', *, *, #17318, .F. ) ;
#24953 = EDGE_LOOP ( 'NONE', ( #19301, #47776, #65738, #7703 ) ) ;
#24954 = CARTESIAN_POINT ( 'NONE',  ( 30.00000000000000000, -5.599999999999999645, -9.000000000000001776 ) ) ;
#24955 = DIRECTION ( 'NONE',  ( -1.000000000000000000, 0.000000000000000000, 0.000000000000000000 ) ) ;
#24956 = ORIENTED_EDGE ( 'NONE', *, *, #13202, .T. ) ;
#24957 = VERTEX_POINT ( 'NONE', #66156 ) ;
#24958 = EDGE_LOOP ( 'NONE', ( #10445, #67973, #29603, #13214 ) ) ;
#24959 = ORIENTED_EDGE ( 'NONE', *, *, #56854, .F. ) ;
#24960 = DIRECTION ( 'NONE',  ( -0.000000000000000000, -0.000000000000000000, 1.000000000000000000 ) ) ;
#24961 = AXIS2_PLACEMENT_3D ( 'NONE', #67846, #40618, #24358 ) ;
#24963 = VERTEX_POINT ( 'NONE', #38604 ) ;
#24962 = CARTESIAN_POINT ( 'NONE',  ( 19.90000000000000213, -14.06939075806902117, -20.80000000000000426 ) ) ;
#24964 = CARTESIAN_POINT ( 'NONE',  ( 12.90000000000000213, 20.60000000000000142, 13.86939075806900057 ) ) ;
#24965 = AXIS2_PLACEMENT_3D ( 'NONE', #16563, #1659, #28198 ) ;
#24966 = VECTOR ( 'NONE', #51316, 1000.000000000000000 ) ;
#24967 = DIRECTION ( 'NONE',  ( 0.000000000000000000, 0.000000000000000000, -1.000000000000000000 ) ) ;
#24968 = EDGE_CURVE ( 'NONE', #43669, #28734, #32947, .T. ) ;
#24969 = ORIENTED_EDGE ( 'NONE', *, *, #27444, .T. ) ;
#24970 = CIRCLE ( 'NONE', #26096, 0.3499999999998875677 ) ;
#24971 = ORIENTED_EDGE ( 'NONE', *, *, #69854, .F. ) ;
#24972 = CIRCLE ( 'NONE', #14843, 0.1749999999999989342 ) ;
#24973 = AXIS2_PLACEMENT_3D ( 'NONE', #12570, #44068, #43735 ) ;
#24974 = EDGE_CURVE ( 'NONE', #62844, #63906, #17032, .T. ) ;
#24975 = DIRECTION ( 'NONE',  ( 0.000000000000000000, 0.000000000000000000, 1.000000000000000000 ) ) ;
#24976 = CYLINDRICAL_SURFACE ( 'NONE', #68395, 0.1999999999999987899 ) ;
#24977 = CARTESIAN_POINT ( 'NONE',  ( -11.18999999999999950, 12.00000000000000000, -5.000000000000000000 ) ) ;
#24978 = EDGE_CURVE ( 'NONE', #60909, #24080, #11183, .T. ) ;
#24979 = VECTOR ( 'NONE', #13046, 1000.000000000000000 ) ;
#24980 = CYLINDRICAL_SURFACE ( 'NONE', #36848, 1.000000000000000000 ) ;
#24981 = PLANE ( 'NONE',  #67469 ) ;
#24983 = VERTEX_POINT ( 'NONE', #59477 ) ;
#24982 = DIRECTION ( 'NONE',  ( 0.000000000000000000, 0.000000000000000000, -1.000000000000000000 ) ) ;
#24984 = ORIENTED_EDGE ( 'NONE', *, *, #46564, .T. ) ;
#24985 = DIRECTION ( 'NONE',  ( -0.000000000000000000, 3.673940397442059868E-16, -1.000000000000000000 ) ) ;
#24986 = FACE_OUTER_BOUND ( 'NONE', #37947, .T. ) ;
#24987 = CIRCLE ( 'NONE', #4711, 1.000000000000000000 ) ;
#24988 = CARTESIAN_POINT ( 'NONE',  ( 11.75000000000000000, -5.000000000000000000, -23.89194109070750116 ) ) ;
#24989 = CARTESIAN_POINT ( 'NONE',  ( 15.50000000000000000, -1.037157890325000054, 22.50000000000000000 ) ) ;
#24990 = EDGE_CURVE ( 'NONE', #56861, #16796, #5739, .T. ) ;
#24991 = DIRECTION ( 'NONE',  ( 0.000000000000000000, 1.000000000000000000, 0.000000000000000000 ) ) ;
#24992 = VERTEX_POINT ( 'NONE', #60502 ) ;
#24993 = DIRECTION ( 'NONE',  ( 1.000000000000000000, -0.000000000000000000, -0.000000000000000000 ) ) ;
#24994 = LINE ( 'NONE', #66720, #58755 ) ;
#24995 = PLANE ( 'NONE',  #25402 ) ;
#24996 = CARTESIAN_POINT ( 'NONE',  ( -4.031976262117261456, 3.142976262117183506, 54.00000000000000711 ) ) ;
#24997 = VECTOR ( 'NONE', #31346, 1000.000000000000000 ) ;
#24998 = CARTESIAN_POINT ( 'NONE',  ( 10.09643294401454661, -2.906483450353491094, 455.0000000000000568 ) ) ;
#24999 = ADVANCED_FACE ( 'NONE', ( #33294 ), #22681, .T. ) ;
#25000 = DIRECTION ( 'NONE',  ( 1.836970198721029934E-16, -1.836970198721036344E-16, 1.000000000000000000 ) ) ;
#25001 = EDGE_CURVE ( 'NONE', #35248, #16863, #49218, .T. ) ;
#25002 = LINE ( 'NONE', #29946, #45381 ) ;
#25003 = ORIENTED_EDGE ( 'NONE', *, *, #34899, .T. ) ;
#25004 = DIRECTION ( 'NONE',  ( 1.000000000000000000, 0.000000000000000000, 0.000000000000000000 ) ) ;
#25005 = DIRECTION ( 'NONE',  ( 0.000000000000000000, 0.000000000000000000, 1.000000000000000000 ) ) ;
#25006 = ADVANCED_FACE ( 'NONE', ( #21990 ), #59820, .F. ) ;
#25007 = ORIENTED_EDGE ( 'NONE', *, *, #11052, .T. ) ;
#25008 = DIRECTION ( 'NONE',  ( 0.000000000000000000, 0.000000000000000000, 1.000000000000000000 ) ) ;
#25009 = ADVANCED_FACE ( 'NONE', ( #17367 ), #793, .F. ) ;
#25010 = ADVANCED_FACE ( 'NONE', ( #28322 ), #49893, .T. ) ;
#25011 = CYLINDRICAL_SURFACE ( 'NONE', #24475, 1.224999999999998757 ) ;
#25012 = CARTESIAN_POINT ( 'NONE',  ( 6.832023737882812142, 9.722976262117196455, 26.00000000000000711 ) ) ;
#25013 = FILL_AREA_STYLE ('',( #3446 ) ) ;
#25014 = DIRECTION ( 'NONE',  ( -1.000000000000000000, 0.000000000000000000, 0.000000000000000000 ) ) ;
#25015 = VECTOR ( 'NONE', #43596, 1000.000000000000000 ) ;
#25016 = ORIENTED_EDGE ( 'NONE', *, *, #57389, .T. ) ;
#25017 = ADVANCED_FACE ( 'NONE', ( #39283 ), #60840, .T. ) ;
#25018 = CARTESIAN_POINT ( 'NONE',  ( 11.08848345035341865, 11.07551654964652776, 455.0000000000000568 ) ) ;
#25019 = PRESENTATION_LAYER_ASSIGNMENT (  '', '', ( #28384 ) ) ;
#25020 = EDGE_LOOP ( 'NONE', ( #58086, #36545, #21310, #41644 ) ) ;
#25021 = DIRECTION ( 'NONE',  ( -1.000000000000000000, 0.000000000000000000, 0.000000000000000000 ) ) ;
#25022 = ADVANCED_FACE ( 'NONE', ( #8851 ), #18759, .F. ) ;
#25023 = CYLINDRICAL_SURFACE ( 'NONE', #30057, 0.1749999999999998224 ) ;
#25024 = ORIENTED_EDGE ( 'NONE', *, *, #34479, .F. ) ;
#25025 = PLANE ( 'NONE',  #50647 ) ;
#25026 = EDGE_CURVE ( 'NONE', #37598, #65595, #45984, .T. ) ;
#25027 = ORIENTED_EDGE ( 'NONE', *, *, #47941, .T. ) ;
#25028 = AXIS2_PLACEMENT_3D ( 'NONE', #40321, #57542, #12050 ) ;
#25029 = CLOSED_SHELL ( 'NONE', ( #56369, #61287, #17014, #23320, #40966, #19396 ) ) ;
#25030 = FACE_OUTER_BOUND ( 'NONE', #7959, .T. ) ;
#25031 = ORIENTED_EDGE ( 'NONE', *, *, #34150, .F. ) ;
#25032 = ORIENTED_EDGE ( 'NONE', *, *, #36677, .F. ) ;
#25034 = EDGE_CURVE ( 'NONE', #62579, #66346, #24058, .T. ) ;
#25033 = DIRECTION ( 'NONE',  ( -1.000000000000000000, 0.000000000000000000, 0.000000000000000000 ) ) ;
#25035 = ORIENTED_EDGE ( 'NONE', *, *, #14788, .F. ) ;
#25036 = ORIENTED_EDGE ( 'NONE', *, *, #63993, .F. ) ;
#25037 = EDGE_CURVE ( 'NONE', #44153, #35248, #53002, .T. ) ;
#25038 = LINE ( 'NONE', #31746, #38397 ) ;
#25039 = CARTESIAN_POINT ( 'NONE',  ( -11.00000000000000000, -5.200000000000001066, 9.400000000000000355 ) ) ;
#25040 = DIRECTION ( 'NONE',  ( 1.334402673828312846E-16, 1.000000000000000000, 0.000000000000000000 ) ) ;
#25041 = ORIENTED_EDGE ( 'NONE', *, *, #1664, .F. ) ;
#25042 = CARTESIAN_POINT ( 'NONE',  ( -9.722976262117256852, 7.955476262117183062, 54.00000000000000711 ) ) ;
#25043 = AXIS2_PLACEMENT_3D ( 'NONE', #2812, #24388, #36391 ) ;
#25045 = DIRECTION ( 'NONE',  ( -1.261617073437657577E-14, -1.000000000000000000, 0.000000000000000000 ) ) ;
#25044 = FACE_OUTER_BOUND ( 'NONE', #49848, .T. ) ;
#25046 = VERTEX_POINT ( 'NONE', #50928 ) ;
#25048 = VERTEX_POINT ( 'NONE', #56245 ) ;
#25047 = CARTESIAN_POINT ( 'NONE',  ( -1.853252480934882929, -9.417013320880883498, 455.0000000000000568 ) ) ;
#25049 = ORIENTED_EDGE ( 'NONE', *, *, #57700, .F. ) ;
#25050 = APPLICATION_CONTEXT ( 'automotive_design' ) ;
#25051 = DIRECTION ( 'NONE',  ( 0.000000000000000000, 0.000000000000000000, 1.000000000000000000 ) ) ;
#25053 = EDGE_LOOP ( 'NONE', ( #35489, #11567, #26586, #46231, #5805, #65088, #4478, #42700, #4290, #68693, #32911 ) ) ;
#25052 = DIRECTION ( 'NONE',  ( 0.000000000000000000, 1.000000000000000000, 0.000000000000000000 ) ) ;
#25054 = CARTESIAN_POINT ( 'NONE',  ( -15.50000000000000000, -1.037157890325000054, 19.00000000000000000 ) ) ;
#25055 = CARTESIAN_POINT ( 'NONE',  ( 276.8000000000000682, -53.81370849898476649, -17.60000000000000142 ) ) ;
#25056 = VECTOR ( 'NONE', #29136, 1000.000000000000000 ) ;
#25057 = ORIENTED_EDGE ( 'NONE', *, *, #23266, .F. ) ;
#25058 = ORIENTED_EDGE ( 'NONE', *, *, #14865, .T. ) ;
#25059 = CARTESIAN_POINT ( 'NONE',  ( -10.30047626211729472, -6.849523737882750929, 54.00000000000000711 ) ) ;
#25060 = EDGE_LOOP ( 'NONE', ( #68497, #56759, #41100, #42916 ) ) ;
#25061 = ADVANCED_FACE ( 'NONE', ( #3556 ), #45269, .F. ) ;
#25062 = DIRECTION ( 'NONE',  ( 0.000000000000000000, 0.000000000000000000, -1.000000000000000000 ) ) ;
#25063 = CARTESIAN_POINT ( 'NONE',  ( 14.25000000000000000, -2.500000000000000000, 21.77831216351300014 ) ) ;
#25064 = CARTESIAN_POINT ( 'NONE',  ( -10.91351654964670814, 2.893516549646604208, 455.0000000000000568 ) ) ;
#25065 = AXIS2_PLACEMENT_3D ( 'NONE', #66458, #18010, #12695 ) ;
#25066 = EDGE_LOOP ( 'NONE', ( #18308, #14427, #66262, #26785 ) ) ;
#25067 = ADVANCED_FACE ( 'NONE', ( #51647 ), #39620, .F. ) ;
#25068 = CARTESIAN_POINT ( 'NONE',  ( 15.00000000000000000, -20.40000000000000213, 17.60000000000000142 ) ) ;
#25069 = CARTESIAN_POINT ( 'NONE',  ( 15.00000000000000000, -25.93000000000544958, 9.412893218815410634 ) ) ;
#25071 = ORIENTED_EDGE ( 'NONE', *, *, #49866, .T. ) ;
#25070 = LINE ( 'NONE', #46982, #39851 ) ;
#25073 = ORIENTED_EDGE ( 'NONE', *, *, #30037, .T. ) ;
#25072 = DIRECTION ( 'NONE',  ( 1.836970198721029934E-16, 1.836970198721010706E-16, -1.000000000000000000 ) ) ;
#25074 = EDGE_CURVE ( 'NONE', #53050, #22714, #39391, .T. ) ;
#25075 = LINE ( 'NONE', #68205, #43054 ) ;
#25076 = DIRECTION ( 'NONE',  ( -0.000000000000000000, 3.673940397442059868E-16, -1.000000000000000000 ) ) ;
#25077 = EDGE_CURVE ( 'NONE', #10205, #22677, #40604, .T. ) ;
#25078 = LINE ( 'NONE', #69618, #64087 ) ;
#25079 = AXIS2_PLACEMENT_3D ( 'NONE', #11528, #17884, #50057 ) ;
#25080 = AXIS2_PLACEMENT_3D ( 'NONE', #16932, #40485, #29174 ) ;
#25081 = DIRECTION ( 'NONE',  ( 0.000000000000000000, 1.000000000000000000, 0.000000000000000000 ) ) ;
#25082 = EDGE_CURVE ( 'NONE', #31241, #7152, #35718, .T. ) ;
#25083 = LINE ( 'NONE', #10215, #63567 ) ;
#25084 = ORIENTED_EDGE ( 'NONE', *, *, #55321, .F. ) ;
#25085 = PLANE ( 'NONE',  #32457 ) ;
#25086 = LINE ( 'NONE', #62200, #65463 ) ;
#25087 = PLANE ( 'NONE',  #1821 ) ;
#25089 = ORIENTED_EDGE ( 'NONE', *, *, #54335, .F. ) ;
#25088 = CARTESIAN_POINT ( 'NONE',  ( -15.50000000000000000, -5.000000000000000000, -22.50000000000000000 ) ) ;
#25090 = DIRECTION ( 'NONE',  ( 0.000000000000000000, 0.000000000000000000, 1.000000000000000000 ) ) ;
#25091 = DIRECTION ( 'NONE',  ( 0.000000000000000000, 0.000000000000000000, 1.000000000000000000 ) ) ;
#25092 = VECTOR ( 'NONE', #20826, 1000.000000000000000 ) ;
#25093 = VERTEX_POINT ( 'NONE', #29706 ) ;
#25094 = CARTESIAN_POINT ( 'NONE',  ( -4.242044687070550602, 8.452095193409279617, 455.0000000000000568 ) ) ;
#25095 = CARTESIAN_POINT ( 'NONE',  ( 3.664523737882781518, -10.31452373788281029, 54.00000000000000711 ) ) ;
#25096 = ORIENTED_EDGE ( 'NONE', *, *, #1229, .T. ) ;
#25097 = EDGE_CURVE ( 'NONE', #41013, #6189, #22547, .T. ) ;
#25098 = CARTESIAN_POINT ( 'NONE',  ( -8.821682069070828192, -7.969523737882767911, 54.00000000000000711 ) ) ;
#25099 = LINE ( 'NONE', #9899, #10634 ) ;
#25100 = CARTESIAN_POINT ( 'NONE',  ( 10.92648345035337343, -2.706483450353490916, 455.0000000000000568 ) ) ;
#25101 = DIRECTION ( 'NONE',  ( -0.000000000000000000, 0.000000000000000000, 1.000000000000000000 ) ) ;
#25102 = EDGE_LOOP ( 'NONE', ( #58279, #34740, #29098, #36266 ) ) ;
#25103 = FACE_OUTER_BOUND ( 'NONE', #840, .T. ) ;
#25104 = ORIENTED_EDGE ( 'NONE', *, *, #32697, .F. ) ;
#25105 = ORIENTED_EDGE ( 'NONE', *, *, #19426, .F. ) ;
#25106 = ORIENTED_EDGE ( 'NONE', *, *, #59683, .T. ) ;
#25107 = CARTESIAN_POINT ( 'NONE',  ( -25.50000000000000355, -15.50000000000000000, -20.49999999999999645 ) ) ;
#25108 = AXIS2_PLACEMENT_3D ( 'NONE', #59273, #64582, #32414 ) ;
#25109 = CARTESIAN_POINT ( 'NONE',  ( -7.172176262117273993, -5.257023737882780878, 26.00000000000000711 ) ) ;
#25110 = DIRECTION ( 'NONE',  ( -1.836970198721029934E-16, 1.836970198721036590E-16, -1.000000000000000000 ) ) ;
#25111 = EDGE_LOOP ( 'NONE', ( #13710, #12564, #67997, #68582 ) ) ;
#25112 = ORIENTED_EDGE ( 'NONE', *, *, #11126, .F. ) ;
#25113 = CIRCLE ( 'NONE', #34124, 25.39999999999999858 ) ;
#25115 = EDGE_CURVE ( 'NONE', #34859, #54853, #5593, .T. ) ;
#25114 = FACE_OUTER_BOUND ( 'NONE', #25173, .T. ) ;
#25116 = ORIENTED_EDGE ( 'NONE', *, *, #5930, .F. ) ;
#25117 = ORIENTED_EDGE ( 'NONE', *, *, #16236, .T. ) ;
#25118 = EDGE_CURVE ( 'NONE', #3209, #11172, #30423, .T. ) ;
#25119 = CARTESIAN_POINT ( 'NONE',  ( 36.90000000000000568, -14.06939075806900163, -20.80000000000000426 ) ) ;
#25120 = DIRECTION ( 'NONE',  ( 0.000000000000000000, 1.000000000000000000, 0.000000000000000000 ) ) ;
#25121 = LINE ( 'NONE', #30069, #69365 ) ;
#25122 = DIRECTION ( 'NONE',  ( 0.000000000000000000, 0.000000000000000000, 1.000000000000000000 ) ) ;
#25123 = ORIENTED_EDGE ( 'NONE', *, *, #45815, .T. ) ;
#25124 = VECTOR ( 'NONE', #18580, 1000.000000000000000 ) ;
#25125 = PLANE ( 'NONE',  #18711 ) ;
#25127 = DIRECTION ( 'NONE',  ( 0.000000000000000000, 0.000000000000000000, 1.000000000000000000 ) ) ;
#25126 = DIRECTION ( 'NONE',  ( -3.016910393003147986E-15, -1.000000000000000000, -3.673940397442060361E-16 ) ) ;
#25128 = ORIENTED_EDGE ( 'NONE', *, *, #62612, .F. ) ;
#25130 = ORIENTED_EDGE ( 'NONE', *, *, #19483, .T. ) ;
#25129 = DIRECTION ( 'NONE',  ( 0.000000000000000000, 0.000000000000000000, 1.000000000000000000 ) ) ;
#25131 = VERTEX_POINT ( 'NONE', #34306 ) ;
#25132 = ORIENTED_EDGE ( 'NONE', *, *, #3486, .F. ) ;
#25133 = VECTOR ( 'NONE', #67297, 1000.000000000000000 ) ;
#25134 = CARTESIAN_POINT ( 'NONE',  ( -9.547976262117222390, -2.369523737882729186, 54.00000000000000711 ) ) ;
#25135 = CARTESIAN_POINT ( 'NONE',  ( 283.0000000000000568, -37.61196062927500350, -8.008708659369300875 ) ) ;
#25136 = AXIS2_PLACEMENT_3D ( 'NONE', #38344, #59899, #10425 ) ;
#25137 = ORIENTED_EDGE ( 'NONE', *, *, #28010, .F. ) ;
#25138 = VERTEX_POINT ( 'NONE', #40677 ) ;
#25139 = CIRCLE ( 'NONE', #8210, 1.929199999999997139 ) ;
#25140 = AXIS2_PLACEMENT_3D ( 'NONE', #31788, #26474, #68565 ) ;
#25142 = LINE ( 'NONE', #12460, #36443 ) ;
#25141 = AXIS2_PLACEMENT_3D ( 'NONE', #45162, #12284, #23262 ) ;
#25143 = CARTESIAN_POINT ( 'NONE',  ( -24.00000000000000000, -15.50000000000000000, 14.50000000000000000 ) ) ;
#25144 = ORIENTED_EDGE ( 'NONE', *, *, #51177, .F. ) ;
#25145 = ORIENTED_EDGE ( 'NONE', *, *, #17643, .T. ) ;
#25146 = PLANE ( 'NONE',  #40935 ) ;
#25147 = VECTOR ( 'NONE', #29315, 1000.000000000000000 ) ;
#25148 = DIRECTION ( 'NONE',  ( 0.000000000000000000, 0.7071067811865474617, 0.7071067811865474617 ) ) ;
#25149 = VERTEX_POINT ( 'NONE', #55893 ) ;
#25150 = EDGE_CURVE ( 'NONE', #17757, #16609, #7788, .T. ) ;
#25151 = CIRCLE ( 'NONE', #15008, 1.929199999999998028 ) ;
#25152 = CYLINDRICAL_SURFACE ( 'NONE', #44731, 0.7112000000000124889 ) ;
#25153 = PLANE ( 'NONE',  #13651 ) ;
#25155 = EDGE_LOOP ( 'NONE', ( #4177, #34703, #11384, #28553 ) ) ;
#25154 = FACE_OUTER_BOUND ( 'NONE', #27110, .T. ) ;
#25156 = ORIENTED_EDGE ( 'NONE', *, *, #68188, .T. ) ;
#25157 = EDGE_CURVE ( 'NONE', #4457, #49409, #29357, .T. ) ;
#25158 = CARTESIAN_POINT ( 'NONE',  ( 7.250000000000005329, -7.249999999999998224, -23.50000000000000000 ) ) ;
#25159 = LINE ( 'NONE', #52753, #12616 ) ;
#25160 = ADVANCED_FACE ( 'NONE', ( #50593 ), #30067, .T. ) ;
#25161 = VECTOR ( 'NONE', #45341, 1000.000000000000000 ) ;
#25162 = CARTESIAN_POINT ( 'NONE',  ( 14.50000000000000000, 0.000000000000000000, 26.50000000000000000 ) ) ;
#25163 = EDGE_CURVE ( 'NONE', #14797, #68930, #67904, .T. ) ;
#25164 = DIRECTION ( 'NONE',  ( -0.000000000000000000, 3.673940397442059868E-16, -1.000000000000000000 ) ) ;
#25165 = DIRECTION ( 'NONE',  ( 0.000000000000000000, 1.000000000000000000, 0.000000000000000000 ) ) ;
#25166 = EDGE_CURVE ( 'NONE', #27562, #15739, #41016, .T. ) ;
#25167 = EDGE_CURVE ( 'NONE', #16770, #44864, #14510, .T. ) ;
#25168 = DIRECTION ( 'NONE',  ( 1.000000000000000000, 0.000000000000000000, 0.000000000000000000 ) ) ;
#25169 = VECTOR ( 'NONE', #10467, 1000.000000000000000 ) ;
#25170 = ORIENTED_EDGE ( 'NONE', *, *, #47362, .T. ) ;
#25171 = DIRECTION ( 'NONE',  ( 1.000000000000000000, -0.000000000000000000, -0.000000000000000000 ) ) ;
#25173 = EDGE_LOOP ( 'NONE', ( #63641, #27145, #3300, #6493 ) ) ;
#25172 = CYLINDRICAL_SURFACE ( 'NONE', #62742, 0.1749999999999998224 ) ;
#25174 = CARTESIAN_POINT ( 'NONE',  ( 275.0000000000000000, -21.00000000000000000, 0.000000000000000000 ) ) ;
#25175 = DIRECTION ( 'NONE',  ( -1.000000000000000000, 0.000000000000000000, 0.000000000000000000 ) ) ;
#25176 = ADVANCED_FACE ( 'NONE', ( #36070 ), #9211, .F. ) ;
#25177 = CARTESIAN_POINT ( 'NONE',  ( -9.689726262117318356, -8.930623737882756430, 54.00000000000000711 ) ) ;
#25178 = ORIENTED_EDGE ( 'NONE', *, *, #19011, .T. ) ;
#25179 = CARTESIAN_POINT ( 'NONE',  ( 11.50000000000000000, -11.50000000000000000, -19.00000000000000000 ) ) ;
#25180 = DIRECTION ( 'NONE',  ( 1.000000000000000000, 0.000000000000000000, 0.000000000000000000 ) ) ;
#25181 = ORIENTED_EDGE ( 'NONE', *, *, #14568, .T. ) ;
#25182 = LINE ( 'NONE', #25539, #52651 ) ;
#25183 = CARTESIAN_POINT ( 'NONE',  ( 2.544523737882792069, -8.835729544836324223, 54.00000000000000711 ) ) ;
#25184 = CIRCLE ( 'NONE', #19518, 24.99999999998789946 ) ;
#25185 = ORIENTED_EDGE ( 'NONE', *, *, #29624, .F. ) ;
#25186 = DIRECTION ( 'NONE',  ( -1.836970198721029934E-16, -1.836970198721010706E-16, 1.000000000000000000 ) ) ;
#25187 = ORIENTED_EDGE ( 'NONE', *, *, #38369, .T. ) ;
#25188 = VERTEX_POINT ( 'NONE', #47384 ) ;
#25189 = CIRCLE ( 'NONE', #6014, 4.500000000000191847 ) ;
#25190 = LINE ( 'NONE', #47452, #55070 ) ;
#25191 = DIRECTION ( 'NONE',  ( 0.000000000000000000, 0.000000000000000000, -1.000000000000000000 ) ) ;
#25192 = CARTESIAN_POINT ( 'NONE',  ( -9.390476262117203987, -1.480523737882726731, 26.00000000000000711 ) ) ;
#25193 = CIRCLE ( 'NONE', #69256, 0.1999999999999996503 ) ;
#25194 = DIRECTION ( 'NONE',  ( -1.000000000000000000, 0.000000000000000000, 0.000000000000000000 ) ) ;
#25195 = VECTOR ( 'NONE', #67069, 1000.000000000000114 ) ;
#25196 = DIRECTION ( 'NONE',  ( -1.000000000000000000, -1.671920889371702854E-15, -0.000000000000000000 ) ) ;
#25197 = ORIENTED_EDGE ( 'NONE', *, *, #60602, .T. ) ;
#25198 = ORIENTED_EDGE ( 'NONE', *, *, #13830, .F. ) ;
#25200 = ORIENTED_EDGE ( 'NONE', *, *, #40807, .F. ) ;
#25199 = DIRECTION ( 'NONE',  ( 0.000000000000000000, 1.000000000000000000, 0.000000000000000000 ) ) ;
#25201 = ORIENTED_EDGE ( 'NONE', *, *, #28502, .F. ) ;
#25202 = EDGE_CURVE ( 'NONE', #54282, #6582, #57641, .T. ) ;
#25203 = CARTESIAN_POINT ( 'NONE',  ( -8.227189898828694226, -1.634292677759810575, 26.00000000000000711 ) ) ;
#25204 = AXIS2_PLACEMENT_3D ( 'NONE', #58018, #69692, #4635 ) ;
#25205 = CARTESIAN_POINT ( 'NONE',  ( 8.406483450353379183, -4.396432944014657451, 455.0000000000000568 ) ) ;
#25206 = LINE ( 'NONE', #30504, #15435 ) ;
#25207 = PLANE ( 'NONE',  #57934 ) ;
#25208 = EDGE_CURVE ( 'NONE', #67341, #97, #62956, .T. ) ;
#25209 = EDGE_CURVE ( 'NONE', #27223, #30559, #29281, .T. ) ;
#25210 = DIRECTION ( 'NONE',  ( 0.000000000000000000, 0.000000000000000000, 1.000000000000000000 ) ) ;
#25211 = FACE_OUTER_BOUND ( 'NONE', #3463, .T. ) ;
#25212 = VECTOR ( 'NONE', #58067, 1000.000000000000000 ) ;
#25213 = EDGE_LOOP ( 'NONE', ( #21830, #43080, #39410, #49408 ) ) ;
#25214 = ORIENTED_EDGE ( 'NONE', *, *, #22133, .F. ) ;
#25215 = EDGE_CURVE ( 'NONE', #19912, #51662, #53746, .T. ) ;
#25216 = EDGE_LOOP ( 'NONE', ( #57827, #29712 ) ) ;
#25217 = ORIENTED_EDGE ( 'NONE', *, *, #6637, .F. ) ;
#25218 = DIRECTION ( 'NONE',  ( -1.000000000000000000, 1.610765207321970913E-14, 1.836970198721059516E-16 ) ) ;
#25219 = CIRCLE ( 'NONE', #2592, 0.3499999999999285905 ) ;
#25220 = DIRECTION ( 'NONE',  ( 0.000000000000000000, 1.000000000000000000, 3.673940397442059868E-16 ) ) ;
#25221 = CARTESIAN_POINT ( 'NONE',  ( 6.304152346236907789, -0.5000000000278984613, 345.7837994620737732 ) ) ;
#25222 = DIRECTION ( 'NONE',  ( -1.053224967557348291E-14, -1.000000000000000000, 0.000000000000000000 ) ) ;
#25223 = EDGE_LOOP ( 'NONE', ( #33044, #41876, #66320, #42139 ) ) ;
#25224 = ORIENTED_EDGE ( 'NONE', *, *, #18526, .T. ) ;
#25225 = ORIENTED_EDGE ( 'NONE', *, *, #17660, .F. ) ;
#25226 = CARTESIAN_POINT ( 'NONE',  ( -2.893516549646820035, -10.09643294401462654, 455.0000000000000568 ) ) ;
#25227 = VERTEX_POINT ( 'NONE', #20511 ) ;
#25228 = ORIENTED_EDGE ( 'NONE', *, *, #59604, .F. ) ;
#25229 = CARTESIAN_POINT ( 'NONE',  ( 3.677663764522620671, 4.135079735113112775, 54.00000000000000711 ) ) ;
#25230 = EDGE_LOOP ( 'NONE', ( #57013, #35708 ) ) ;
#25231 = ORIENTED_EDGE ( 'NONE', *, *, #33293, .T. ) ;
#25232 = CARTESIAN_POINT ( 'NONE',  ( -11.75000000000000000, -5.000000000000000000, -11.75000000000000000 ) ) ;
#25234 = EDGE_LOOP ( 'NONE', ( #42331, #21212, #39306, #40328 ) ) ;
#25233 = DIRECTION ( 'NONE',  ( 0.000000000000000000, 0.000000000000000000, -1.000000000000000000 ) ) ;
#25235 = VERTEX_POINT ( 'NONE', #26880 ) ;
#25236 = CARTESIAN_POINT ( 'NONE',  ( 0.000000000000000000, -7.449999999999998401, -17.00000000000000000 ) ) ;
#25237 = ADVANCED_FACE ( 'NONE', ( #68250 ), #4270, .F. ) ;
#25238 = AXIS2_PLACEMENT_3D ( 'NONE', #62551, #55526, #56900 ) ;
#25240 = CARTESIAN_POINT ( 'NONE',  ( 18.89999999999999858, -0.2000000000089119934, 8.909539772616881237E-12 ) ) ;
#25239 = AXIS2_PLACEMENT_3D ( 'NONE', #6248, #69907, #16521 ) ;
#25241 = DIRECTION ( 'NONE',  ( 0.000000000000000000, -0.1249999999999996531, -0.9921567416492215186 ) ) ;
#25243 = ORIENTED_EDGE ( 'NONE', *, *, #20920, .T. ) ;
#25242 = DIRECTION ( 'NONE',  ( -1.000000000000000000, 0.000000000000000000, 0.000000000000000000 ) ) ;
#25245 = ORIENTED_EDGE ( 'NONE', *, *, #39349, .F. ) ;
#25244 = AXIS2_PLACEMENT_3D ( 'NONE', #31119, #49103, #21883 ) ;
#25246 = DIRECTION ( 'NONE',  ( 0.000000000000000000, 0.000000000000000000, -1.000000000000000000 ) ) ;
#25247 = VECTOR ( 'NONE', #48889, 1000.000000000000000 ) ;
#25248 = DIRECTION ( 'NONE',  ( 0.8660254037844435926, 0.4999999999999913958, 2.509347957447859069E-16 ) ) ;
#25249 = CARTESIAN_POINT ( 'NONE',  ( 46.39999999999999858, 33.00000000000000000, -0.7500000000000000000 ) ) ;
#25250 = CYLINDRICAL_SURFACE ( 'NONE', #1127, 0.5249999999999994671 ) ;
#25251 = AXIS2_PLACEMENT_3D ( 'NONE', #63958, #54385, #4904 ) ;
#25252 = AXIS2_PLACEMENT_3D ( 'NONE', #65936, #17508, #66989 ) ;
#25253 = EDGE_CURVE ( 'NONE', #69832, #29208, #4489, .T. ) ;
#25254 = EDGE_CURVE ( 'NONE', #65843, #16435, #69299, .T. ) ;
#25255 = VERTEX_POINT ( 'NONE', #15581 ) ;
#25256 = FACE_OUTER_BOUND ( 'NONE', #11075, .T. ) ;
#25257 = CARTESIAN_POINT ( 'NONE',  ( 9.562023737882812569, -2.369523737882825998, 54.00000000000000711 ) ) ;
#25258 = ADVANCED_FACE ( 'NONE', ( #15911 ), #3909, .T. ) ;
#25259 = ORIENTED_EDGE ( 'NONE', *, *, #35873, .F. ) ;
#25260 = DIRECTION ( 'NONE',  ( 0.000000000000000000, 0.000000000000000000, 1.000000000000000000 ) ) ;
#25261 = LINE ( 'NONE', #46812, #67894 ) ;
#25262 = CYLINDRICAL_SURFACE ( 'NONE', #24636, 0.1999999999999992339 ) ;
#25263 = ORIENTED_EDGE ( 'NONE', *, *, #48066, .F. ) ;
#25264 = DIRECTION ( 'NONE',  ( 0.000000000000000000, 0.000000000000000000, -1.000000000000000000 ) ) ;
#25265 = PLANE ( 'NONE',  #40109 ) ;
#25266 = DIRECTION ( 'NONE',  ( -0.5000000000000129896, -0.8660254037844311581, -2.509347957447868930E-16 ) ) ;
#25267 = ORIENTED_EDGE ( 'NONE', *, *, #42725, .T. ) ;
#25268 = DIRECTION ( 'NONE',  ( 0.000000000000000000, 0.000000000000000000, 1.000000000000000000 ) ) ;
#25269 = CYLINDRICAL_SURFACE ( 'NONE', #37743, 0.1999999999999987899 ) ;
#25270 = DIRECTION ( 'NONE',  ( 1.000000000000000000, 0.000000000000000000, 0.000000000000000000 ) ) ;
#25271 = DIRECTION ( 'NONE',  ( 1.836970198721029934E-16, 1.836970198721010706E-16, -1.000000000000000000 ) ) ;
#25272 = LINE ( 'NONE', #10068, #35325 ) ;
#25273 = ORIENTED_EDGE ( 'NONE', *, *, #69147, .F. ) ;
#25274 = DIRECTION ( 'NONE',  ( -1.000000000000000000, 0.000000000000000000, 0.000000000000000000 ) ) ;
#25275 = CYLINDRICAL_SURFACE ( 'NONE', #2348, 4.000000000000000000 ) ;
#25276 = CARTESIAN_POINT ( 'NONE',  ( 0.000000000000000000, -8.249999999999998224, -8.500000000000000000 ) ) ;
#25277 = SURFACE_STYLE_FILL_AREA ( #57100 ) ;
#25278 = DIRECTION ( 'NONE',  ( 1.836970198721029934E-16, 1.836970198721010706E-16, -1.000000000000000000 ) ) ;
#25279 = ORIENTED_EDGE ( 'NONE', *, *, #17196, .F. ) ;
#25281 = VERTEX_POINT ( 'NONE', #25471 ) ;
#25280 = LINE ( 'NONE', #63113, #48663 ) ;
#25282 = CIRCLE ( 'NONE', #464, 2.000000000000001776 ) ;
#25283 = CIRCLE ( 'NONE', #44491, 0.9999999999984570120 ) ;
#25284 = CARTESIAN_POINT ( 'NONE',  ( -7.450000000000001954, 7.250000000000000000, -23.50000000000000000 ) ) ;
#25285 = DIRECTION ( 'NONE',  ( -1.000000000000000000, 0.000000000000000000, 0.000000000000000000 ) ) ;
#25286 = DIRECTION ( 'NONE',  ( 0.000000000000000000, 3.673940397442059868E-16, -1.000000000000000000 ) ) ;
#25287 = EDGE_LOOP ( 'NONE', ( #61080, #65151, #16585, #60482 ) ) ;
#25288 = EDGE_CURVE ( 'NONE', #596, #15713, #47037, .T. ) ;
#25289 = ADVANCED_FACE ( 'NONE', ( #63303 ), #26176, .F. ) ;
#25290 = EDGE_CURVE ( 'NONE', #21406, #6346, #15743, .T. ) ;
#25291 = FACE_OUTER_BOUND ( 'NONE', #43560, .T. ) ;
#25292 = CIRCLE ( 'NONE', #30947, 0.1749999999999998224 ) ;
#25293 = CARTESIAN_POINT ( 'NONE',  ( -11.11351654964670743, 9.093516549646603053, 455.0000000000000568 ) ) ;
#25294 = AXIS2_PLACEMENT_3D ( 'NONE', #37091, #38719, #25784 ) ;
#25295 = ORIENTED_EDGE ( 'NONE', *, *, #63492, .F. ) ;
#25296 = ORIENTED_EDGE ( 'NONE', *, *, #20539, .T. ) ;
#25297 = EDGE_CURVE ( 'NONE', #53470, #30033, #47732, .T. ) ;
#25298 = VECTOR ( 'NONE', #68909, 1000.000000000000000 ) ;
#25300 = ORIENTED_EDGE ( 'NONE', *, *, #24406, .F. ) ;
#25299 = VECTOR ( 'NONE', #26603, 1000.000000000000000 ) ;
#25301 = AXIS2_PLACEMENT_3D ( 'NONE', #46740, #58059, #8909 ) ;
#25302 = LINE ( 'NONE', #62771, #6892 ) ;
#25303 = DIRECTION ( 'NONE',  ( -1.000000000000000000, 0.000000000000000000, 0.000000000000000000 ) ) ;
#25304 = CARTESIAN_POINT ( 'NONE',  ( 14.25000000000000000, -0.2038245569916330158, 23.22168783648699986 ) ) ;
#25305 = ORIENTED_EDGE ( 'NONE', *, *, #57567, .F. ) ;
#25306 = ORIENTED_EDGE ( 'NONE', *, *, #33851, .F. ) ;
#25307 = FACE_OUTER_BOUND ( 'NONE', #43891, .T. ) ;
#25308 = VECTOR ( 'NONE', #44240, 1000.000000000000000 ) ;
#25309 = DIRECTION ( 'NONE',  ( -1.000000000000000000, 0.000000000000000000, 0.000000000000000000 ) ) ;
#25310 = EDGE_LOOP ( 'NONE', ( #52070, #48630, #9275, #65539 ) ) ;
#25311 = ORIENTED_EDGE ( 'NONE', *, *, #52253, .T. ) ;
#25312 = ORIENTED_EDGE ( 'NONE', *, *, #3126, .T. ) ;
#25313 = ORIENTED_EDGE ( 'NONE', *, *, #29751, .T. ) ;
#25314 = EDGE_CURVE ( 'NONE', #12401, #38480, #63509, .T. ) ;
#25315 = CARTESIAN_POINT ( 'NONE',  ( 8.250000000000005329, -7.249999999999998224, -26.00000000000001066 ) ) ;
#25316 = UNCERTAINTY_MEASURE_WITH_UNIT (LENGTH_MEASURE( 1.000000000000000082E-05 ), #43659, 'distance_accuracy_value', 'NONE');
#25318 = ORIENTED_EDGE ( 'NONE', *, *, #69182, .T. ) ;
#25317 = CARTESIAN_POINT ( 'NONE',  ( 11.50000000000000000, -12.00000000000000000, -11.03137303340310282 ) ) ;
#25319 = CARTESIAN_POINT ( 'NONE',  ( -6.835476262117260227, 10.49297626211718359, 26.00000000000000711 ) ) ;
#25320 = DIRECTION ( 'NONE',  ( 0.000000000000000000, 0.000000000000000000, -1.000000000000000000 ) ) ;
#25321 = ORIENTED_EDGE ( 'NONE', *, *, #58933, .T. ) ;
#25322 = EDGE_LOOP ( 'NONE', ( #50136, #43228, #58925, #49028 ) ) ;
#25323 = COLOUR_RGB ( '', 0.72549020, 0.75294118, 0.79215686) ;
#25324 = FACE_OUTER_BOUND ( 'NONE', #54967, .T. ) ;
#25325 = DIRECTION ( 'NONE',  ( 0.000000000000000000, 0.7071067811865474617, 0.7071067811865474617 ) ) ;
#25326 = ORIENTED_EDGE ( 'NONE', *, *, #38369, .F. ) ;
#25327 = EDGE_CURVE ( 'NONE', #47065, #46851, #64352, .T. ) ;
#25328 = VECTOR ( 'NONE', #12752, 1000.000000000000000 ) ;
#25329 = DIRECTION ( 'NONE',  ( 0.000000000000000000, 0.000000000000000000, -1.000000000000000000 ) ) ;
#25330 = DIRECTION ( 'NONE',  ( -1.000000000000000000, 1.047444401652940007E-14, -1.836970198721010706E-16 ) ) ;
#25331 = EDGE_CURVE ( 'NONE', #30714, #64997, #43820, .T. ) ;
#25332 = ADVANCED_FACE ( 'NONE', ( #65047 ), #48783, .F. ) ;
#25333 = CYLINDRICAL_SURFACE ( 'NONE', #23168, 0.1749999999999998224 ) ;
#25334 = VERTEX_POINT ( 'NONE', #697 ) ;
#25335 = CYLINDRICAL_SURFACE ( 'NONE', #26509, 0.1999999999999987899 ) ;
#25336 = CARTESIAN_POINT ( 'NONE',  ( -5.993516549646711766, 8.198316549646602169, 195.0000000000000284 ) ) ;
#25337 = VECTOR ( 'NONE', #31906, 1000.000000000000000 ) ;
#25339 = VECTOR ( 'NONE', #36933, 1000.000000000000000 ) ;
#25338 = LINE ( 'NONE', #51863, #3716 ) ;
#25340 = EDGE_CURVE ( 'NONE', #8160, #9204, #43465, .T. ) ;
#25341 = DIRECTION ( 'NONE',  ( 0.000000000000000000, -1.000000000000000000, 0.000000000000000000 ) ) ;
#25342 = EDGE_CURVE ( 'NONE', #33795, #25480, #55255, .T. ) ;
#25343 = VECTOR ( 'NONE', #47734, 1000.000000000000000 ) ;
#25344 = DIRECTION ( 'NONE',  ( -0.000000000000000000, 1.000000000000000000, -0.000000000000000000 ) ) ;
#25345 = EDGE_CURVE ( 'NONE', #67717, #18722, #54164, .T. ) ;
#25346 = VERTEX_POINT ( 'NONE', #43117 ) ;
#25347 = CARTESIAN_POINT ( 'NONE',  ( -1.466476262117324181, -9.404523737882843903, 54.00000000000000711 ) ) ;
#25348 = LINE ( 'NONE', #4486, #3418 ) ;
#25349 = EDGE_CURVE ( 'NONE', #47230, #37838, #11231, .T. ) ;
#25350 = CARTESIAN_POINT ( 'NONE',  ( 7.000000000000000000, -21.00000000000000000, 7.799999999999999822 ) ) ;
#25351 = DIRECTION ( 'NONE',  ( 1.000000000000000000, 0.000000000000000000, 0.000000000000000000 ) ) ;
#25352 = DIRECTION ( 'NONE',  ( -1.000000000000000000, 0.000000000000000000, 0.000000000000000000 ) ) ;
#25353 = CIRCLE ( 'NONE', #17472, 0.2000000000000005107 ) ;
#25354 = CYLINDRICAL_SURFACE ( 'NONE', #51575, 1.621000000000000885 ) ;
#25355 = CARTESIAN_POINT ( 'NONE',  ( 6.789561617636934443, 7.394232575409549035, 54.00000000000000711 ) ) ;
#25356 = ORIENTED_EDGE ( 'NONE', *, *, #68248, .T. ) ;
#25357 = CARTESIAN_POINT ( 'NONE',  ( -4.947141984184481700, 7.342976262117180575, 54.00000000000000711 ) ) ;
#25358 = DIRECTION ( 'NONE',  ( 1.836970198721029934E-16, 1.836970198721010706E-16, -1.000000000000000000 ) ) ;
#25359 = ORIENTED_EDGE ( 'NONE', *, *, #3889, .F. ) ;
#25360 = CARTESIAN_POINT ( 'NONE',  ( -7.450000000000001954, 0.000000000000000000, -24.00000000000000000 ) ) ;
#25361 = PLANE ( 'NONE',  #22052 ) ;
#25362 = DIRECTION ( 'NONE',  ( -0.000000000000000000, -0.000000000000000000, -1.000000000000000000 ) ) ;
#25363 = CARTESIAN_POINT ( 'NONE',  ( -10.49297626211732748, -9.795823737882738413, 54.00000000000000711 ) ) ;
#25364 = FACE_OUTER_BOUND ( 'NONE', #56621, .T. ) ;
#25365 = ORIENTED_EDGE ( 'NONE', *, *, #38239, .F. ) ;
#25366 = ORIENTED_EDGE ( 'NONE', *, *, #9446, .F. ) ;
#25367 = DIRECTION ( 'NONE',  ( 0.7071067811865500152, 0.7071067811865451302, 0.000000000000000000 ) ) ;
#25368 = DIRECTION ( 'NONE',  ( -1.836970198721029934E-16, 1.836970198721036590E-16, -1.000000000000000000 ) ) ;
#25369 = VERTEX_POINT ( 'NONE', #21900 ) ;
#25370 = AXIS2_PLACEMENT_3D ( 'NONE', #19448, #39954, #7783 ) ;
#25371 = FACE_OUTER_BOUND ( 'NONE', #50210, .T. ) ;
#25372 = DIRECTION ( 'NONE',  ( 0.000000000000000000, 0.000000000000000000, 1.000000000000000000 ) ) ;
#25373 = AXIS2_PLACEMENT_3D ( 'NONE', #9449, #31387, #52592 ) ;
#25374 = VERTEX_POINT ( 'NONE', #16249 ) ;
#25375 = DIRECTION ( 'NONE',  ( -0.000000000000000000, -0.000000000000000000, -1.000000000000000000 ) ) ;
#25376 = VERTEX_POINT ( 'NONE', #5655 ) ;
#25377 = EDGE_LOOP ( 'NONE', ( #41614, #7906, #11715, #34917, #33541, #15611, #56687, #30255 ) ) ;
#25378 = CARTESIAN_POINT ( 'NONE',  ( -9.722976262117303037, -7.969523737882757253, 54.00000000000000711 ) ) ;
#25379 = ORIENTED_EDGE ( 'NONE', *, *, #45066, .F. ) ;
#25380 = ORIENTED_EDGE ( 'NONE', *, *, #51363, .T. ) ;
#25381 = FACE_OUTER_BOUND ( 'NONE', #42024, .T. ) ;
#25382 = DIRECTION ( 'NONE',  ( 1.000000000000000000, -1.047444401652940007E-14, 1.836970198721010706E-16 ) ) ;
#25383 = CIRCLE ( 'NONE', #28790, 0.06000000000000102474 ) ;
#25384 = CIRCLE ( 'NONE', #49105, 0.7499999999999997780 ) ;
#25385 = CARTESIAN_POINT ( 'NONE',  ( 7.265214908726107090, 6.606374702650081865, 195.0000000000000284 ) ) ;
#25386 = ORIENTED_EDGE ( 'NONE', *, *, #33124, .T. ) ;
#25387 = DIRECTION ( 'NONE',  ( -1.000000000000000000, 0.000000000000000000, 0.000000000000000000 ) ) ;
#25389 = LINE ( 'NONE', #47306, #62677 ) ;
#25388 = DIRECTION ( 'NONE',  ( 1.000000000000000000, -0.000000000000000000, 0.000000000000000000 ) ) ;
#25390 = CIRCLE ( 'NONE', #49112, 4.000000000000000888 ) ;
#25391 = EDGE_CURVE ( 'NONE', #21660, #36053, #66060, .T. ) ;
#25392 = ORIENTED_EDGE ( 'NONE', *, *, #50933, .F. ) ;
#25394 = ORIENTED_EDGE ( 'NONE', *, *, #64453, .T. ) ;
#25393 = DIRECTION ( 'NONE',  ( 1.000000000000000000, -0.000000000000000000, 0.000000000000000000 ) ) ;
#25395 = ORIENTED_EDGE ( 'NONE', *, *, #60922, .T. ) ;
#25396 = AXIS2_PLACEMENT_3D ( 'NONE', #30170, #51743, #18492 ) ;
#25397 = EDGE_CURVE ( 'NONE', #18780, #28902, #47382, .T. ) ;
#25398 = CARTESIAN_POINT ( 'NONE',  ( 7.250000000000005329, -7.449999999999998401, -23.50000000000000000 ) ) ;
#25400 = ORIENTED_EDGE ( 'NONE', *, *, #59583, .T. ) ;
#25399 = DIRECTION ( 'NONE',  ( -0.000000000000000000, -0.000000000000000000, -1.000000000000000000 ) ) ;
#25401 = CARTESIAN_POINT ( 'NONE',  ( -11.50000000000000000, -11.50000000000000000, 11.00000000000000000 ) ) ;
#25402 = AXIS2_PLACEMENT_3D ( 'NONE', #24650, #30304, #46199 ) ;
#25403 = DIRECTION ( 'NONE',  ( -1.000000000000000000, 0.000000000000000000, 0.000000000000000000 ) ) ;
#25404 = EDGE_LOOP ( 'NONE', ( #4239, #48354, #18403, #29515 ) ) ;
#25405 = EDGE_CURVE ( 'NONE', #62633, #38291, #16951, .T. ) ;
#25406 = ORIENTED_EDGE ( 'NONE', *, *, #46259, .T. ) ;
#25407 = VECTOR ( 'NONE', #25698, 999.9999999999998863 ) ;
#25408 = DIRECTION ( 'NONE',  ( 1.000000000000000000, 0.000000000000000000, 0.000000000000000000 ) ) ;
#25409 = EDGE_CURVE ( 'NONE', #27271, #64422, #11619, .T. ) ;
#25410 = ORIENTED_EDGE ( 'NONE', *, *, #3434, .T. ) ;
#25411 = CARTESIAN_POINT ( 'NONE',  ( 6.364920264886885448, -3.677663764522628664, 54.00000000000000711 ) ) ;
#25412 = LINE ( 'NONE', #68556, #1919 ) ;
#25413 = FACE_OUTER_BOUND ( 'NONE', #43958, .T. ) ;
#25414 = ORIENTED_EDGE ( 'NONE', *, *, #31878, .F. ) ;
#25415 = CIRCLE ( 'NONE', #64943, 0.3500000000009988455 ) ;
#25416 = CARTESIAN_POINT ( 'NONE',  ( 8.900000000000005684, 13.66939075806899240, 20.79999999999999361 ) ) ;
#25417 = EDGE_CURVE ( 'NONE', #58452, #17797, #38187, .T. ) ;
#25418 = DIRECTION ( 'NONE',  ( 0.000000000000000000, 0.000000000000000000, 1.000000000000000000 ) ) ;
#25420 = ORIENTED_EDGE ( 'NONE', *, *, #36832, .T. ) ;
#25419 = DIRECTION ( 'NONE',  ( 0.000000000000000000, 0.000000000000000000, 1.000000000000000000 ) ) ;
#25422 = VERTEX_POINT ( 'NONE', #55472 ) ;
#25421 = DIRECTION ( 'NONE',  ( 1.000000000000000000, -0.000000000000000000, 0.000000000000000000 ) ) ;
#25423 = DIRECTION ( 'NONE',  ( -1.000000000000000000, 0.000000000000000000, 0.000000000000000000 ) ) ;
#25424 = LINE ( 'NONE', #14105, #56704 ) ;
#25425 = CARTESIAN_POINT ( 'NONE',  ( 75.42576880091934299, 0.000000000000000000, 334.4830310981790831 ) ) ;
#25426 = FACE_OUTER_BOUND ( 'NONE', #59922, .T. ) ;
#25427 = DIRECTION ( 'NONE',  ( 1.000000000000000000, -1.203165845134433242E-14, -1.836970198721052121E-16 ) ) ;
#25428 = EDGE_CURVE ( 'NONE', #15393, #27271, #59389, .T. ) ;
#25429 = VERTEX_POINT ( 'NONE', #27224 ) ;
#25430 = CARTESIAN_POINT ( 'NONE',  ( 8.250000000000005329, 0.000000000000000000, -24.50000000000000000 ) ) ;
#25431 = FACE_OUTER_BOUND ( 'NONE', #32351, .T. ) ;
#25433 = ADVANCED_FACE ( 'NONE', ( #33202 ), #27552, .T. ) ;
#25432 = CARTESIAN_POINT ( 'NONE',  ( 15.00000000000000000, -20.40000000000000213, 12.40000000000000213 ) ) ;
#25435 = ORIENTED_EDGE ( 'NONE', *, *, #53323, .F. ) ;
#25434 = CARTESIAN_POINT ( 'NONE',  ( 289.5000000000000000, -42.50000000000000000, 26.50000000000000000 ) ) ;
#25436 = AXIS2_PLACEMENT_3D ( 'NONE', #44340, #23830, #45038 ) ;
#25437 = CIRCLE ( 'NONE', #62721, 0.5000000000004167777 ) ;
#25438 = CARTESIAN_POINT ( 'NONE',  ( 30.00000000000000000, -14.04000000000000092, -14.80000000000000071 ) ) ;
#25439 = VECTOR ( 'NONE', #47391, 1000.000000000000000 ) ;
#25440 = DIRECTION ( 'NONE',  ( -1.000000000000000000, 0.000000000000000000, 0.000000000000000000 ) ) ;
#25441 = CIRCLE ( 'NONE', #63859, 0.1999999999999996503 ) ;
#25442 = CARTESIAN_POINT ( 'NONE',  ( -2.355476262117229158, 9.547976262117156665, 54.00000000000000711 ) ) ;
#25443 = ORIENTED_EDGE ( 'NONE', *, *, #50341, .F. ) ;
#25444 = LINE ( 'NONE', #68583, #29814 ) ;
#25445 = CYLINDRICAL_SURFACE ( 'NONE', #10295, 1.000000000000000000 ) ;
#25446 = ORIENTED_EDGE ( 'NONE', *, *, #59572, .T. ) ;
#25447 = LINE ( 'NONE', #37117, #59372 ) ;
#25448 = CARTESIAN_POINT ( 'NONE',  ( -9.249999999999998224, -7.848062532927998269, 5.000000000000000000 ) ) ;
#25449 = VECTOR ( 'NONE', #42399, 1000.000000000000000 ) ;
#25450 = CARTESIAN_POINT ( 'NONE',  ( -8.393516549646712122, 7.603567055985436696, 455.0000000000000568 ) ) ;
#25451 = LINE ( 'NONE', #53728, #60949 ) ;
#25452 = CARTESIAN_POINT ( 'NONE',  ( 7.250000000000005329, 8.250000000000001776, -10.00000000000000000 ) ) ;
#25453 = AXIS2_PLACEMENT_3D ( 'NONE', #58507, #69098, #10058 ) ;
#25454 = ORIENTED_EDGE ( 'NONE', *, *, #21701, .F. ) ;
#25455 = CARTESIAN_POINT ( 'NONE',  ( 8.835729544836338434, -7.969523737882814984, 26.00000000000000000 ) ) ;
#25456 = ORIENTED_EDGE ( 'NONE', *, *, #62511, .F. ) ;
#25457 = EDGE_LOOP ( 'NONE', ( #25561, #33476, #37469, #54727 ) ) ;
#25458 = ORIENTED_EDGE ( 'NONE', *, *, #62952, .T. ) ;
#25459 = ORIENTED_EDGE ( 'NONE', *, *, #50260, .T. ) ;
#25460 = VECTOR ( 'NONE', #51244, 1000.000000000000114 ) ;
#25461 = CARTESIAN_POINT ( 'NONE',  ( 7.000000000000000000, -39.80000000000000426, 12.69999999999999929 ) ) ;
#25462 = ADVANCED_FACE ( 'NONE', ( #5992 ), #1044, .F. ) ;
#25463 = CARTESIAN_POINT ( 'NONE',  ( -2.893516549646675706, 10.91351654964657669, 195.0000000000000284 ) ) ;
#25464 = FACE_OUTER_BOUND ( 'NONE', #64591, .T. ) ;
#25465 = ORIENTED_EDGE ( 'NONE', *, *, #49198, .T. ) ;
#25466 = ORIENTED_EDGE ( 'NONE', *, *, #63931, .T. ) ;
#25467 = LINE ( 'NONE', #47031, #28445 ) ;
#25468 = ORIENTED_EDGE ( 'NONE', *, *, #29105, .F. ) ;
#25469 = ADVANCED_FACE ( 'NONE', ( #55131 ), #6670, .F. ) ;
#25470 = VERTEX_POINT ( 'NONE', #22936 ) ;
#25471 = CARTESIAN_POINT ( 'NONE',  ( -7.250000000000000888, 8.250000000000001776, -24.00000000000000000 ) ) ;
#25472 = CARTESIAN_POINT ( 'NONE',  ( -7.450000000000001954, -7.249999999999998224, -19.50000000000000000 ) ) ;
#25473 = CARTESIAN_POINT ( 'NONE',  ( -15.70366306705059323, -0.2717122460101009662, -21.17420925361163953 ) ) ;
#25474 = VECTOR ( 'NONE', #23573, 1000.000000000000000 ) ;
#25475 = EDGE_LOOP ( 'NONE', ( #18007, #52721, #9774, #67852 ) ) ;
#25476 = EDGE_CURVE ( 'NONE', #51761, #30714, #48501, .T. ) ;
#25477 = LINE ( 'NONE', #53406, #37922 ) ;
#25479 = CARTESIAN_POINT ( 'NONE',  ( 41.09999999999999432, 20.60000000000000142, -13.86939075806900057 ) ) ;
#25478 = DIRECTION ( 'NONE',  ( 1.836970198721029934E-16, 1.836970198721010706E-16, -1.000000000000000000 ) ) ;
#25480 = VERTEX_POINT ( 'NONE', #40932 ) ;
#25481 = ADVANCED_FACE ( 'NONE', ( #28931 ), #1713, .F. ) ;
#25483 = EDGE_LOOP ( 'NONE', ( #30363, #22630, #67647, #39992 ) ) ;
#25482 = DIRECTION ( 'NONE',  ( -0.000000000000000000, -0.000000000000000000, 1.000000000000000000 ) ) ;
#25484 = AXIS2_PLACEMENT_3D ( 'NONE', #22585, #58437, #17269 ) ;
#25485 = ORIENTED_EDGE ( 'NONE', *, *, #33037, .T. ) ;
#25486 = AXIS2_PLACEMENT_3D ( 'NONE', #8024, #51883, #3098 ) ;
#25487 = EDGE_CURVE ( 'NONE', #52552, #40627, #39533, .T. ) ;
#25488 = CARTESIAN_POINT ( 'NONE',  ( -12.00000000000000000, 11.18999999999999950, -5.000000000000000000 ) ) ;
#25489 = VECTOR ( 'NONE', #62350, 1000.000000000000000 ) ;
#25490 = VECTOR ( 'NONE', #36037, 1000.000000000000000 ) ;
#25492 = DIRECTION ( 'NONE',  ( 0.000000000000000000, 0.7071067811865474617, 0.7071067811865474617 ) ) ;
#25491 = AXIS2_PLACEMENT_3D ( 'NONE', #28016, #65163, #6101 ) ;
#25493 = VERTEX_POINT ( 'NONE', #45180 ) ;
#25494 = VERTEX_POINT ( 'NONE', #23620 ) ;
#25495 = EDGE_CURVE ( 'NONE', #49302, #27615, #3121, .T. ) ;
#25496 = ADVANCED_FACE ( 'NONE', ( #34577 ), #56166, .T. ) ;
#25497 = AXIS2_PLACEMENT_3D ( 'NONE', #66003, #55082, #32799 ) ;
#25498 = VECTOR ( 'NONE', #54691, 1000.000000000000000 ) ;
#25499 = AXIS2_PLACEMENT_3D ( 'NONE', #45623, #51290, #3210 ) ;
#25500 = DIRECTION ( 'NONE',  ( 1.000000000000000000, -0.000000000000000000, -0.000000000000000000 ) ) ;
#25501 = DIRECTION ( 'NONE',  ( -0.000000000000000000, -0.000000000000000000, 1.000000000000000000 ) ) ;
#25502 = ORIENTED_EDGE ( 'NONE', *, *, #39297, .F. ) ;
#25503 = EDGE_CURVE ( 'NONE', #39516, #61131, #18309, .T. ) ;
#25504 = EDGE_CURVE ( 'NONE', #39228, #16506, #61436, .T. ) ;
#25505 = ORIENTED_EDGE ( 'NONE', *, *, #56442, .T. ) ;
#25506 = DIRECTION ( 'NONE',  ( 1.836970198721029934E-16, 1.836970198721010706E-16, -1.000000000000000000 ) ) ;
#25507 = VECTOR ( 'NONE', #35554, 1000.000000000000000 ) ;
#25508 = DIRECTION ( 'NONE',  ( 1.000000000000000000, -0.000000000000000000, 0.000000000000000000 ) ) ;
#25509 = EDGE_LOOP ( 'NONE', ( #8388, #25410, #11459, #46606, #14137, #40097, #16027, #62346, #40583, #51810 ) ) ;
#25510 = EDGE_CURVE ( 'NONE', #30361, #61947, #7706, .T. ) ;
#25511 = AXIS2_PLACEMENT_3D ( 'NONE', #49948, #11769, #60567 ) ;
#25512 = FACE_OUTER_BOUND ( 'NONE', #57872, .T. ) ;
#25513 = DIRECTION ( 'NONE',  ( 0.000000000000000000, 0.000000000000000000, 1.000000000000000000 ) ) ;
#25515 = VERTEX_POINT ( 'NONE', #45532 ) ;
#25514 = DIRECTION ( 'NONE',  ( -1.836970198721029934E-16, 1.836970198721036590E-16, -1.000000000000000000 ) ) ;
#25516 = VECTOR ( 'NONE', #59003, 1000.000000000000000 ) ;
#25517 = ORIENTED_EDGE ( 'NONE', *, *, #20444, .T. ) ;
#25518 = DIRECTION ( 'NONE',  ( 0.000000000000000000, 0.000000000000000000, -1.000000000000000000 ) ) ;
#25519 = CARTESIAN_POINT ( 'NONE',  ( -7.450000000000001954, 7.250000000000000000, -24.50000000000000000 ) ) ;
#25520 = CARTESIAN_POINT ( 'NONE',  ( 78.77321854994620765, 47.95351654967443977, 26.00000000000000355 ) ) ;
#25521 = CARTESIAN_POINT ( 'NONE',  ( 30.00000000000000000, -4.000000000000000000, 26.25000000000000000 ) ) ;
#25522 = LINE ( 'NONE', #34711, #29419 ) ;
#25523 = LINE ( 'NONE', #58746, #43917 ) ;
#25524 = EDGE_CURVE ( 'NONE', #65032, #60221, #56403, .T. ) ;
#25525 = VERTEX_POINT ( 'NONE', #35263 ) ;
#25526 = DIRECTION ( 'NONE',  ( 1.000000000000000000, 0.000000000000000000, 0.000000000000000000 ) ) ;
#25529 = ORIENTED_EDGE ( 'NONE', *, *, #39344, .F. ) ;
#25528 = EDGE_CURVE ( 'NONE', #13479, #14815, #62147, .T. ) ;
#25527 = DIRECTION ( 'NONE',  ( 1.836970198721029934E-16, 1.836970198721010706E-16, -1.000000000000000000 ) ) ;
#25530 = CARTESIAN_POINT ( 'NONE',  ( 40.90000000000000568, -21.00000000000000000, 16.96999999999999886 ) ) ;
#25531 = FACE_OUTER_BOUND ( 'NONE', #22509, .T. ) ;
#25532 = AXIS2_PLACEMENT_3D ( 'NONE', #16820, #64910, #59607 ) ;
#25533 = CARTESIAN_POINT ( 'NONE',  ( -8.250000000000001776, -8.249999999999998224, -26.00000000000001066 ) ) ;
#25534 = AXIS2_PLACEMENT_3D ( 'NONE', #16850, #22839, #26773 ) ;
#25535 = VERTEX_POINT ( 'NONE', #24331 ) ;
#25536 = CARTESIAN_POINT ( 'NONE',  ( -8.250000000000001776, -8.249999999999998224, -26.00000000000001066 ) ) ;
#25537 = FACE_OUTER_BOUND ( 'NONE', #8940, .T. ) ;
#25538 = ORIENTED_EDGE ( 'NONE', *, *, #10184, .T. ) ;
#25539 = CARTESIAN_POINT ( 'NONE',  ( 29.50000000000000355, -12.00000000000000000, -10.69999999999999929 ) ) ;
#25540 = VECTOR ( 'NONE', #33703, 1000.000000000000000 ) ;
#25541 = CYLINDRICAL_SURFACE ( 'NONE', #29138, 0.5000000000009354739 ) ;
#25542 = AXIS2_PLACEMENT_3D ( 'NONE', #60983, #43704, #22490 ) ;
#25543 = VECTOR ( 'NONE', #26900, 1000.000000000000000 ) ;
#25544 = CARTESIAN_POINT ( 'NONE',  ( -7.250000000000000000, -7.449999999999998401, -7.500000000000000000 ) ) ;
#25545 = VERTEX_POINT ( 'NONE', #66421 ) ;
#25546 = DIRECTION ( 'NONE',  ( 0.000000000000000000, -1.000000000000000000, 0.000000000000000000 ) ) ;
#25547 = ORIENTED_EDGE ( 'NONE', *, *, #17279, .F. ) ;
#25548 = VERTEX_POINT ( 'NONE', #29265 ) ;
#25549 = CARTESIAN_POINT ( 'NONE',  ( -29.50000000000000355, -11.50000000000000000, 19.00000000000000000 ) ) ;
#25551 = DIRECTION ( 'NONE',  ( 0.000000000000000000, 0.000000000000000000, 1.000000000000000000 ) ) ;
#25550 = VECTOR ( 'NONE', #5163, 1000.000000000000114 ) ;
#25552 = CIRCLE ( 'NONE', #57022, 0.3500000000002722600 ) ;
#25553 = VECTOR ( 'NONE', #10173, 1000.000000000000000 ) ;
#25554 = CARTESIAN_POINT ( 'NONE',  ( 30.00000000000000000, -8.959999999999999076, -12.95475478405700009 ) ) ;
#25555 = VECTOR ( 'NONE', #35928, 1000.000000000000000 ) ;
#25556 = PLANE ( 'NONE',  #12844 ) ;
#25557 = DIRECTION ( 'NONE',  ( 0.000000000000000000, 0.000000000000000000, -1.000000000000000000 ) ) ;
#25558 = ORIENTED_EDGE ( 'NONE', *, *, #51817, .F. ) ;
#25559 = ORIENTED_EDGE ( 'NONE', *, *, #30209, .F. ) ;
#25561 = ORIENTED_EDGE ( 'NONE', *, *, #27930, .F. ) ;
#25560 = DIRECTION ( 'NONE',  ( 1.000000000000000000, 0.000000000000000000, 0.000000000000000000 ) ) ;
#25562 = ORIENTED_EDGE ( 'NONE', *, *, #31259, .T. ) ;
#25563 = EDGE_CURVE ( 'NONE', #62241, #43177, #34991, .T. ) ;
#25564 = VECTOR ( 'NONE', #14753, 1000.000000000000000 ) ;
#25565 = DIRECTION ( 'NONE',  ( 0.000000000000000000, -0.7071067811865474617, -0.7071067811865474617 ) ) ;
#25566 = LINE ( 'NONE', #57374, #21920 ) ;
#25567 = DIRECTION ( 'NONE',  ( -0.000000000000000000, -0.000000000000000000, -1.000000000000000000 ) ) ;
#25568 = CARTESIAN_POINT ( 'NONE',  ( 10.90000000000000036, 13.66939075806899240, -20.79999999999999361 ) ) ;
#25569 = EDGE_CURVE ( 'NONE', #61947, #66569, #9010, .T. ) ;
#25570 = CARTESIAN_POINT ( 'NONE',  ( -17.00000000000000000, -17.00000000000000000, 15.70499999999969809 ) ) ;
#25572 = DIRECTION ( 'NONE',  ( -0.000000000000000000, 3.673940397442059868E-16, -1.000000000000000000 ) ) ;
#25571 = CARTESIAN_POINT ( 'NONE',  ( -9.093516549646711411, 10.08346604330776941, 455.0000000000000568 ) ) ;
#25573 = ADVANCED_FACE ( 'NONE', ( #8050 ), #2066, .F. ) ;
#25574 = VERTEX_POINT ( 'NONE', #24685 ) ;
#25575 = ORIENTED_EDGE ( 'NONE', *, *, #38294, .T. ) ;
#25576 = ORIENTED_EDGE ( 'NONE', *, *, #49204, .T. ) ;
#25577 = ORIENTED_EDGE ( 'NONE', *, *, #55043, .F. ) ;
#25578 = CARTESIAN_POINT ( 'NONE',  ( 30.00000000000000000, -5.599999999999999645, 27.00000000000000000 ) ) ;
#25579 = EDGE_CURVE ( 'NONE', #36648, #21659, #40589, .T. ) ;
#25580 = EDGE_CURVE ( 'NONE', #62370, #14977, #60938, .T. ) ;
#25581 = DIRECTION ( 'NONE',  ( 0.000000000000000000, 1.000000000000000000, 0.000000000000000000 ) ) ;
#25582 = CARTESIAN_POINT ( 'NONE',  ( -5.242976262117259978, 5.242976262117182706, 54.00000000000000711 ) ) ;
#25583 = ORIENTED_EDGE ( 'NONE', *, *, #40087, .F. ) ;
#25584 = ORIENTED_EDGE ( 'NONE', *, *, #57970, .F. ) ;
#25585 = AXIS2_PLACEMENT_3D ( 'NONE', #50372, #39409, #1938 ) ;
#25586 = ORIENTED_EDGE ( 'NONE', *, *, #41153, .F. ) ;
#25587 = DIRECTION ( 'NONE',  ( -0.000000000000000000, 0.000000000000000000, -1.000000000000000000 ) ) ;
#25588 = ORIENTED_EDGE ( 'NONE', *, *, #8572, .F. ) ;
#25589 = ORIENTED_EDGE ( 'NONE', *, *, #32642, .T. ) ;
#25590 = CARTESIAN_POINT ( 'NONE',  ( 7.811466277050727491, 7.259684009079840905, 195.0000000000000284 ) ) ;
#25591 = ORIENTED_EDGE ( 'NONE', *, *, #27213, .T. ) ;
#25592 = VERTEX_POINT ( 'NONE', #8398 ) ;
#25593 = CIRCLE ( 'NONE', #34589, 0.2000000000000005107 ) ;
#25595 = DIRECTION ( 'NONE',  ( -2.891205793294675467E-15, -1.000000000000000000, 0.000000000000000000 ) ) ;
#25594 = AXIS2_PLACEMENT_3D ( 'NONE', #5686, #21934, #38217 ) ;
#25597 = VERTEX_POINT ( 'NONE', #23974 ) ;
#25596 = CARTESIAN_POINT ( 'NONE',  ( -28.00000000000000000, -17.35230188589299871, -15.35019951917099945 ) ) ;
#25598 = ORIENTED_EDGE ( 'NONE', *, *, #26936, .T. ) ;
#25599 = VECTOR ( 'NONE', #60540, 1000.000000000000114 ) ;
#25600 = AXIS2_PLACEMENT_3D ( 'NONE', #66130, #8463, #19434 ) ;
#25601 = VECTOR ( 'NONE', #64986, 1000.000000000000000 ) ;
#25602 = DIRECTION ( 'NONE',  ( -1.000000000000000000, 0.000000000000000000, 0.000000000000000000 ) ) ;
#25603 = CARTESIAN_POINT ( 'NONE',  ( 7.826483450353421745, 11.99351654964657499, 455.0000000000000568 ) ) ;
#25605 = ORIENTED_EDGE ( 'NONE', *, *, #6772, .F. ) ;
#25604 = CARTESIAN_POINT ( 'NONE',  ( -7.393516549646776070, -6.006483450353426790, 455.0000000000000568 ) ) ;
#25606 = VERTEX_POINT ( 'NONE', #29978 ) ;
#25607 = CIRCLE ( 'NONE', #13104, 0.5999999999999989786 ) ;
#25608 = DIRECTION ( 'NONE',  ( 0.000000000000000000, -1.000000000000000000, 0.000000000000000000 ) ) ;
#25609 = AXIS2_PLACEMENT_3D ( 'NONE', #56423, #55734, #33809 ) ;
#25610 = DIRECTION ( 'NONE',  ( -1.794541526872559352E-16, -1.000000000000000000, 0.000000000000000000 ) ) ;
#25611 = CARTESIAN_POINT ( 'NONE',  ( 39.00000000000000000, 16.96999999999999886, -21.00000000000000000 ) ) ;
#25612 = FACE_OUTER_BOUND ( 'NONE', #63061, .T. ) ;
#25613 = VECTOR ( 'NONE', #15936, 1000.000000000000000 ) ;
#25614 = ORIENTED_EDGE ( 'NONE', *, *, #43121, .F. ) ;
#25615 = CARTESIAN_POINT ( 'NONE',  ( 6.358413763958968623, -5.793274621760859944, 54.00000000000000711 ) ) ;
#25616 = EDGE_CURVE ( 'NONE', #55345, #15054, #61816, .T. ) ;
#25617 = VECTOR ( 'NONE', #62628, 1000.000000000000114 ) ;
#25618 = DIRECTION ( 'NONE',  ( -1.000000000000000000, 1.883404846338789915E-14, 0.000000000000000000 ) ) ;
#25619 = CARTESIAN_POINT ( 'NONE',  ( -7.393516549646710345, 5.993516549646603409, 195.0000000000000284 ) ) ;
#25620 = VERTEX_POINT ( 'NONE', #14431 ) ;
#25621 = EDGE_CURVE ( 'NONE', #12677, #40597, #69214, .T. ) ;
#25622 = CARTESIAN_POINT ( 'NONE',  ( -7.342976262117259623, 3.834182069070703580, 26.00000000000000711 ) ) ;
#25623 = DIRECTION ( 'NONE',  ( -0.000000000000000000, 3.673940397442059868E-16, -1.000000000000000000 ) ) ;
#25624 = DIRECTION ( 'NONE',  ( 1.000000000000000000, 0.000000000000000000, 0.000000000000000000 ) ) ;
#25625 = ORIENTED_EDGE ( 'NONE', *, *, #40132, .T. ) ;
#25626 = CARTESIAN_POINT ( 'NONE',  ( 30.90000000000000213, -21.00000000000000000, 13.86939075806900057 ) ) ;
#25627 = PLANE ( 'NONE',  #22079 ) ;
#25628 = CARTESIAN_POINT ( 'NONE',  ( 7.250000000000005329, -7.249999999999998224, -26.00000000000001066 ) ) ;
#25629 = ORIENTED_EDGE ( 'NONE', *, *, #22653, .F. ) ;
#25630 = FACE_OUTER_BOUND ( 'NONE', #6244, .T. ) ;
#25632 = EDGE_CURVE ( 'NONE', #47780, #64355, #56441, .T. ) ;
#25631 = CARTESIAN_POINT ( 'NONE',  ( 25.50000000000000355, 0.000000000000000000, 24.75000000000000000 ) ) ;
#25633 = VECTOR ( 'NONE', #26572, 1000.000000000000000 ) ;
#25634 = DIRECTION ( 'NONE',  ( -0.000000000000000000, -0.000000000000000000, -1.000000000000000000 ) ) ;
#25635 = CARTESIAN_POINT ( 'NONE',  ( -14.25000000000000178, -0.2714405302574902090, 22.01253933645463690 ) ) ;
#25636 = CARTESIAN_POINT ( 'NONE',  ( 283.0000000000000568, -26.42999999999999972, 9.412893218813501051 ) ) ;
#25637 = EDGE_LOOP ( 'NONE', ( #38258, #68471, #25459, #27054 ) ) ;
#25638 = LINE ( 'NONE', #3012, #56959 ) ;
#25639 = LINE ( 'NONE', #4767, #35042 ) ;
#25640 = DIRECTION ( 'NONE',  ( 0.000000000000000000, 0.000000000000000000, -1.000000000000000000 ) ) ;
#25641 = VECTOR ( 'NONE', #41604, 1000.000000000000000 ) ;
#25642 = AXIS2_PLACEMENT_3D ( 'NONE', #13400, #34954, #56534 ) ;
#25643 = DIRECTION ( 'NONE',  ( 1.836970198721029934E-16, 1.836970198721010706E-16, -1.000000000000000000 ) ) ;
#25644 = LINE ( 'NONE', #47209, #59947 ) ;
#25645 = ORIENTED_EDGE ( 'NONE', *, *, #30353, .T. ) ;
#25647 = EDGE_LOOP ( 'NONE', ( #17919, #64132, #11838, #32130 ) ) ;
#25646 = DIRECTION ( 'NONE',  ( 0.000000000000000000, 0.000000000000000000, -1.000000000000000000 ) ) ;
#25648 = AXIS2_PLACEMENT_3D ( 'NONE', #57521, #44552, #52218 ) ;
#25649 = ADVANCED_FACE ( 'NONE', ( #9120 ), #63920, .T. ) ;
#25650 = CIRCLE ( 'NONE', #35821, 0.9999999999984534593 ) ;
#25651 = DIRECTION ( 'NONE',  ( -1.000000000000000000, 0.000000000000000000, 0.000000000000000000 ) ) ;
#25652 = AXIS2_PLACEMENT_3D ( 'NONE', #5419, #18324, #7718 ) ;
#25653 = DIRECTION ( 'NONE',  ( 0.000000000000000000, 1.000000000000000000, 0.000000000000000000 ) ) ;
#25654 = CYLINDRICAL_SURFACE ( 'NONE', #46569, 1.000000000000000000 ) ;
#25655 = VERTEX_POINT ( 'NONE', #51908 ) ;
#25656 = AXIS2_PLACEMENT_3D ( 'NONE', #19323, #62444, #68474 ) ;
#25658 = DIRECTION ( 'NONE',  ( 1.000000000000000000, 0.000000000000000000, 0.000000000000000000 ) ) ;
#25657 = AXIS2_PLACEMENT_3D ( 'NONE', #7356, #38522, #33548 ) ;
#25659 = CARTESIAN_POINT ( 'NONE',  ( 9.955011587777235604, -9.247904806590801385, 455.0000000000000568 ) ) ;
#25660 = ADVANCED_FACE ( 'NONE', ( #47646 ), #35987, .F. ) ;
#25661 = ORIENTED_EDGE ( 'NONE', *, *, #61318, .T. ) ;
#25662 = EDGE_LOOP ( 'NONE', ( #64477, #69476, #41115, #3181, #21579, #5829, #43014, #47381 ) ) ;
#25663 = EDGE_CURVE ( 'NONE', #23407, #41000, #4178, .T. ) ;
#25664 = VECTOR ( 'NONE', #1647, 1000.000000000000000 ) ;
#25665 = ORIENTED_EDGE ( 'NONE', *, *, #47956, .F. ) ;
#25666 = DIRECTION ( 'NONE',  ( -0.000000000000000000, 3.673940397442059868E-16, -1.000000000000000000 ) ) ;
#25667 = ADVANCED_FACE ( 'NONE', ( #8769 ), #58261, .F. ) ;
#25668 = EDGE_CURVE ( 'NONE', #15146, #42524, #62861, .T. ) ;
#25669 = DIRECTION ( 'NONE',  ( 0.7071067811865503483, 0.7071067811865446862, 0.000000000000000000 ) ) ;
#25670 = CARTESIAN_POINT ( 'NONE',  ( -7.593516549646711411, 11.77351654964660277, 195.0000000000000284 ) ) ;
#25671 = LINE ( 'NONE', #26701, #64172 ) ;
#25672 = VECTOR ( 'NONE', #13411, 1000.000000000000000 ) ;
#25673 = EDGE_CURVE ( 'NONE', #18841, #6609, #25038, .T. ) ;
#25674 = ORIENTED_EDGE ( 'NONE', *, *, #48178, .F. ) ;
#25675 = ORIENTED_EDGE ( 'NONE', *, *, #43985, .F. ) ;
#25676 = LINE ( 'NONE', #35916, #50417 ) ;
#25677 = FACE_OUTER_BOUND ( 'NONE', #60321, .T. ) ;
#25678 = VERTEX_POINT ( 'NONE', #64271 ) ;
#25679 = ORIENTED_EDGE ( 'NONE', *, *, #67049, .T. ) ;
#25680 = ORIENTED_EDGE ( 'NONE', *, *, #7110, .T. ) ;
#25681 = VERTEX_POINT ( 'NONE', #36336 ) ;
#25682 = LINE ( 'NONE', #47237, #56435 ) ;
#25684 = ORIENTED_EDGE ( 'NONE', *, *, #61282, .T. ) ;
#25683 = CARTESIAN_POINT ( 'NONE',  ( 283.0000000000000568, -32.44999999999905071, 13.20000000000091944 ) ) ;
#25685 = CARTESIAN_POINT ( 'NONE',  ( 39.00000000000000000, 6.429395695523604153E-16, -5.250000000000000000 ) ) ;
#25686 = LINE ( 'NONE', #47244, #66774 ) ;
#25687 = DIRECTION ( 'NONE',  ( 0.000000000000000000, 1.000000000000000000, 0.000000000000000000 ) ) ;
#25688 = EDGE_LOOP ( 'NONE', ( #7954, #22781, #18744, #65805 ) ) ;
#25689 = ORIENTED_EDGE ( 'NONE', *, *, #14252, .F. ) ;
#25690 = CYLINDRICAL_SURFACE ( 'NONE', #65072, 0.1749999999999998224 ) ;
#25691 = AXIS2_PLACEMENT_3D ( 'NONE', #56873, #25062, #57234 ) ;
#25692 = CIRCLE ( 'NONE', #13245, 24.99999999998789946 ) ;
#25693 = DIRECTION ( 'NONE',  ( 0.000000000000000000, 0.000000000000000000, 1.000000000000000000 ) ) ;
#25694 = ORIENTED_EDGE ( 'NONE', *, *, #43697, .T. ) ;
#25695 = AXIS2_PLACEMENT_3D ( 'NONE', #52550, #58561, #41929 ) ;
#25696 = LINE ( 'NONE', #47255, #45797 ) ;
#25697 = CARTESIAN_POINT ( 'NONE',  ( -10.30047626211729295, -6.657023737882751924, 54.00000000000000711 ) ) ;
#25698 = DIRECTION ( 'NONE',  ( -0.8660254037844363761, 0.5000000000000038858, -0.000000000000000000 ) ) ;
#25699 = ORIENTED_EDGE ( 'NONE', *, *, #26353, .T. ) ;
#25700 = ADVANCED_FACE ( 'NONE', ( #63208 ), #37054, .F. ) ;
#25701 = DIRECTION ( 'NONE',  ( 0.000000000000000000, 1.000000000000000000, 1.883909694907254982E-12 ) ) ;
#25702 = DIRECTION ( 'NONE',  ( -0.000000000000000000, -0.000000000000000000, -1.000000000000000000 ) ) ;
#25703 = ADVANCED_FACE ( 'NONE', ( #57904 ), #69576, .F. ) ;
#25704 = VECTOR ( 'NONE', #46811, 1000.000000000000000 ) ;
#25705 = VECTOR ( 'NONE', #28495, 1000.000000000000000 ) ;
#25706 = DIRECTION ( 'NONE',  ( 0.000000000000000000, -0.7071067811865470176, 0.7071067811865480168 ) ) ;
#25707 = LINE ( 'NONE', #46895, #18933 ) ;
#25708 = EDGE_CURVE ( 'NONE', #55302, #57112, #3470, .T. ) ;
#25709 = LINE ( 'NONE', #4138, #36497 ) ;
#25710 = ORIENTED_EDGE ( 'NONE', *, *, #30584, .F. ) ;
#25711 = CARTESIAN_POINT ( 'NONE',  ( -3.593516549646762481, -4.622483450353452206, 455.0000000000000568 ) ) ;
#25712 = LINE ( 'NONE', #41955, #30526 ) ;
#25713 = FILL_AREA_STYLE ('',( #52578 ) ) ;
#25714 = CARTESIAN_POINT ( 'NONE',  ( 10.50702373788278265, 3.650476262117142934, 54.00000000000000711 ) ) ;
#25715 = VECTOR ( 'NONE', #55013, 1000.000000000000000 ) ;
#25716 = DIRECTION ( 'NONE',  ( -0.7671651518153087546, -0.6414496315691469164, 2.309356642089053889E-17 ) ) ;
#25717 = CARTESIAN_POINT ( 'NONE',  ( 39.00000000000000000, 16.96999999999999886, -21.00000000000000000 ) ) ;
#25718 = DIRECTION ( 'NONE',  ( -0.7071067811865474617, 0.000000000000000000, -0.7071067811865474617 ) ) ;
#25719 = CARTESIAN_POINT ( 'NONE',  ( 9.703773737882816164, 9.689726262117153155, 54.00000000000000711 ) ) ;
#25720 = ORIENTED_EDGE ( 'NONE', *, *, #21484, .T. ) ;
#25721 = CARTESIAN_POINT ( 'NONE',  ( 283.0000000000000568, -40.30000000000000426, 8.900000000000000355 ) ) ;
#25722 = LINE ( 'NONE', #42313, #34994 ) ;
#25723 = FACE_OUTER_BOUND ( 'NONE', #7165, .T. ) ;
#25724 = CYLINDRICAL_SURFACE ( 'NONE', #17584, 1.000000000000000000 ) ;
#25725 = CARTESIAN_POINT ( 'NONE',  ( 9.737023737882799068, 6.817976262117189989, 26.00000000000000711 ) ) ;
#25726 = CARTESIAN_POINT ( 'NONE',  ( -29.25000000000000000, -5.000000000000000000, -26.25000000000000000 ) ) ;
#25727 = FACE_OUTER_BOUND ( 'NONE', #7079, .T. ) ;
#25728 = ORIENTED_EDGE ( 'NONE', *, *, #57008, .F. ) ;
#25729 = ORIENTED_EDGE ( 'NONE', *, *, #67780, .F. ) ;
#25730 = FACE_OUTER_BOUND ( 'NONE', #26992, .T. ) ;
#25731 = DIRECTION ( 'NONE',  ( 0.000000000000000000, 1.000000000000000000, 0.000000000000000000 ) ) ;
#25732 = VECTOR ( 'NONE', #23077, 1000.000000000000000 ) ;
#25733 = ORIENTED_EDGE ( 'NONE', *, *, #6199, .F. ) ;
#25734 = LINE ( 'NONE', #68859, #61953 ) ;
#25735 = DIRECTION ( 'NONE',  ( 0.000000000000000000, 0.000000000000000000, -1.000000000000000000 ) ) ;
#25736 = EDGE_LOOP ( 'NONE', ( #15229, #52107, #8850, #49317 ) ) ;
#25737 = LINE ( 'NONE', #52248, #23205 ) ;
#25738 = ORIENTED_EDGE ( 'NONE', *, *, #25345, .F. ) ;
#25739 = ORIENTED_EDGE ( 'NONE', *, *, #46531, .F. ) ;
#25740 = CARTESIAN_POINT ( 'NONE',  ( 11.75000000000000000, -5.200000000000001066, -26.25000000000000000 ) ) ;
#25741 = EDGE_CURVE ( 'NONE', #19531, #49979, #41992, .T. ) ;
#25742 = VERTEX_POINT ( 'NONE', #4524 ) ;
#25743 = ORIENTED_EDGE ( 'NONE', *, *, #1680, .F. ) ;
#25744 = ADVANCED_FACE ( 'NONE', ( #25381 ), #46941, .T. ) ;
#25745 = VECTOR ( 'NONE', #24405, 1000.000000000000000 ) ;
#25746 = DIRECTION ( 'NONE',  ( -1.000000000000000000, 0.000000000000000000, 0.000000000000000000 ) ) ;
#25747 = LINE ( 'NONE', #4179, #69772 ) ;
#25748 = DIRECTION ( 'NONE',  ( -3.540573132209558464E-15, -1.000000000000000000, 0.000000000000000000 ) ) ;
#25749 = EDGE_CURVE ( 'NONE', #55385, #56867, #14775, .T. ) ;
#25750 = TOROIDAL_SURFACE ( 'NONE', #62985, 0.06000000000000080963, 0.7500000000000000000 ) ;
#25751 = EDGE_CURVE ( 'NONE', #14563, #52575, #20177, .T. ) ;
#25752 = EDGE_LOOP ( 'NONE', ( #5506, #28444, #44895, #60572 ) ) ;
#25753 = LINE ( 'NONE', #3817, #37974 ) ;
#25754 = CIRCLE ( 'NONE', #40419, 0.9999999999999991118 ) ;
#25755 =( GEOMETRIC_REPRESENTATION_CONTEXT ( 3 ) GLOBAL_UNCERTAINTY_ASSIGNED_CONTEXT ( ( #69146 ) ) GLOBAL_UNIT_ASSIGNED_CONTEXT ( ( #23113, #22442, #65240 ) ) REPRESENTATION_CONTEXT ( 'NONE', 'WORKASPACE' ) );
#25757 = DIRECTION ( 'NONE',  ( 0.000000000000000000, 0.000000000000000000, -1.000000000000000000 ) ) ;
#25756 = FACE_OUTER_BOUND ( 'NONE', #9937, .T. ) ;
#25758 = ORIENTED_EDGE ( 'NONE', *, *, #33390, .F. ) ;
#25760 = ORIENTED_EDGE ( 'NONE', *, *, #50648, .F. ) ;
#25759 = EDGE_CURVE ( 'NONE', #23983, #34243, #42891, .T. ) ;
#25761 = ORIENTED_EDGE ( 'NONE', *, *, #37355, .T. ) ;
#25762 = PRODUCT_RELATED_PRODUCT_CATEGORY ( 'part', '', ( #44233 ) ) ;
#25764 = ORIENTED_EDGE ( 'NONE', *, *, #11246, .F. ) ;
#25763 = PRODUCT_CONTEXT ( 'NONE', #25050, 'mechanical' ) ;
#25765 = ADVANCED_FACE ( 'NONE', ( #11205 ), #59655, .T. ) ;
#25766 = PLANE ( 'NONE',  #54812 ) ;
#25767 = EDGE_CURVE ( 'NONE', #69660, #49465, #27086, .T. ) ;
#25769 = ORIENTED_EDGE ( 'NONE', *, *, #52239, .T. ) ;
#25768 = CARTESIAN_POINT ( 'NONE',  ( 16.75000000000000000, -0.2038245569916320166, -23.22168783648699986 ) ) ;
#25770 = VECTOR ( 'NONE', #28799, 1000.000000000000000 ) ;
#25771 = DIRECTION ( 'NONE',  ( -0.000000000000000000, 3.673940397442059868E-16, -1.000000000000000000 ) ) ;
#25772 = FACE_OUTER_BOUND ( 'NONE', #5150, .T. ) ;
#25773 = ORIENTED_EDGE ( 'NONE', *, *, #7251, .F. ) ;
#25774 = ORIENTED_EDGE ( 'NONE', *, *, #29151, .F. ) ;
#25775 = LINE ( 'NONE', #8793, #41373 ) ;
#25776 = EDGE_LOOP ( 'NONE', ( #32739, #58167, #26115, #11066 ) ) ;
#25777 = DIRECTION ( 'NONE',  ( 0.000000000000000000, -1.000000000000000000, 0.000000000000000000 ) ) ;
#25778 = LINE ( 'NONE', #58291, #50465 ) ;
#25779 = LINE ( 'NONE', #12181, #12526 ) ;
#25780 = ORIENTED_EDGE ( 'NONE', *, *, #42129, .T. ) ;
#25781 = DIRECTION ( 'NONE',  ( 9.756599977372196271E-15, 1.000000000000000000, 0.000000000000000000 ) ) ;
#25783 = ORIENTED_EDGE ( 'NONE', *, *, #57075, .F. ) ;
#25782 = CARTESIAN_POINT ( 'NONE',  ( 78.77321854994620765, 47.95351654967443977, 20.00000000000000000 ) ) ;
#25785 = ORIENTED_EDGE ( 'NONE', *, *, #10964, .F. ) ;
#25784 = DIRECTION ( 'NONE',  ( -1.000000000000000000, 0.000000000000000000, 0.000000000000000000 ) ) ;
#25786 = CARTESIAN_POINT ( 'NONE',  ( 10.20488345035338185, -10.20488345035352928, 455.0000000000000568 ) ) ;
#25787 = CARTESIAN_POINT ( 'NONE',  ( 7.250000000000005329, -8.749999999999998224, -30.00000000000001066 ) ) ;
#25788 = DIRECTION ( 'NONE',  ( 1.000000000000000000, -3.491481338843133355E-15, -1.836970198721036344E-16 ) ) ;
#25789 = CARTESIAN_POINT ( 'NONE',  ( 9.737023737882816832, -3.682023737882826886, 54.00000000000000711 ) ) ;
#25790 = ADVANCED_FACE ( 'NONE', ( #966 ), #38771, .F. ) ;
#25791 = DIRECTION ( 'NONE',  ( 0.000000000000000000, 1.000000000000000000, 0.000000000000000000 ) ) ;
#25792 = ORIENTED_EDGE ( 'NONE', *, *, #34732, .F. ) ;
#25793 = CARTESIAN_POINT ( 'NONE',  ( -10.91351654964675610, -9.306483450353326248, 195.0000000000000284 ) ) ;
#25794 = CARTESIAN_POINT ( 'NONE',  ( -7.250000000000000888, 7.250000000000001776, -15.00000000000000000 ) ) ;
#25795 = FACE_OUTER_BOUND ( 'NONE', #37446, .T. ) ;
#25796 = CIRCLE ( 'NONE', #65314, 0.8128000000000145109 ) ;
#25798 = ORIENTED_EDGE ( 'NONE', *, *, #45142, .T. ) ;
#25797 = CARTESIAN_POINT ( 'NONE',  ( 24.90000000000000213, -21.00000000000000000, 13.86939075806900057 ) ) ;
#25799 = LINE ( 'NONE', #30741, #21134 ) ;
#25800 = DIRECTION ( 'NONE',  ( -1.000000000000000000, 1.794541526872559352E-16, 0.000000000000000000 ) ) ;
#25801 = VECTOR ( 'NONE', #17989, 1000.000000000000000 ) ;
#25802 = EDGE_CURVE ( 'NONE', #30511, #47484, #58958, .T. ) ;
#25803 = CARTESIAN_POINT ( 'NONE',  ( 7.250000000000005329, -8.249999999999998224, -18.50000000000000000 ) ) ;
#25804 = ORIENTED_EDGE ( 'NONE', *, *, #36236, .T. ) ;
#25805 = DIRECTION ( 'NONE',  ( 0.000000000000000000, -1.000000000000000000, 0.000000000000000000 ) ) ;
#25806 = CYLINDRICAL_SURFACE ( 'NONE', #61083, 0.1999999999999996503 ) ;
#25807 = ORIENTED_EDGE ( 'NONE', *, *, #62749, .F. ) ;
#25808 = LINE ( 'NONE', #20139, #28858 ) ;
#25809 = DIRECTION ( 'NONE',  ( 0.000000000000000000, -1.000000000000000000, -0.000000000000000000 ) ) ;
#25810 = CARTESIAN_POINT ( 'NONE',  ( 30.00000000000000000, -14.33999999999999986, 14.50000000000000000 ) ) ;
#25811 = ADVANCED_FACE ( 'NONE', ( #17541 ), #5909, .F. ) ;
#25812 = CARTESIAN_POINT ( 'NONE',  ( -6.350872789121377870, -6.836383711242978833, 54.00000000000000711 ) ) ;
#25813 = VECTOR ( 'NONE', #56987, 1000.000000000000000 ) ;
#25814 = DIRECTION ( 'NONE',  ( 1.000000000000000000, 0.000000000000000000, 0.000000000000000000 ) ) ;
#25815 = EDGE_LOOP ( 'NONE', ( #14622, #63918, #19292, #13111 ) ) ;
#25816 = ORIENTED_EDGE ( 'NONE', *, *, #54556, .F. ) ;
#25817 = CARTESIAN_POINT ( 'NONE',  ( 8.900000000000002132, 18.00000000000000355, 21.00000000000000000 ) ) ;
#25818 = ORIENTED_EDGE ( 'NONE', *, *, #69856, .F. ) ;
#25819 = ORIENTED_EDGE ( 'NONE', *, *, #64705, .T. ) ;
#25820 = CARTESIAN_POINT ( 'NONE',  ( -7.450000000000001954, -7.249999999999998224, -13.50000000000000178 ) ) ;
#25821 = ADVANCED_FACE ( 'NONE', ( #59987 ), #59299, .T. ) ;
#25822 = CARTESIAN_POINT ( 'NONE',  ( 55.00000000000000000, 16.96999999999999886, -21.00000000000000000 ) ) ;
#25823 = LINE ( 'NONE', #32164, #37795 ) ;
#25824 = ORIENTED_EDGE ( 'NONE', *, *, #10466, .F. ) ;
#25825 = VERTEX_POINT ( 'NONE', #48351 ) ;
#25826 = DIRECTION ( 'NONE',  ( 1.000000000000000000, 0.000000000000000000, 0.000000000000000000 ) ) ;
#25827 = ORIENTED_EDGE ( 'NONE', *, *, #65958, .F. ) ;
#25828 = ORIENTED_EDGE ( 'NONE', *, *, #31938, .T. ) ;
#25829 = DIRECTION ( 'NONE',  ( 1.000000000000000000, 0.000000000000000000, 0.000000000000000000 ) ) ;
#25830 = LINE ( 'NONE', #48437, #3080 ) ;
#25831 = DIRECTION ( 'NONE',  ( 0.000000000000000000, 0.000000000000000000, 1.000000000000000000 ) ) ;
#25832 = EDGE_CURVE ( 'NONE', #65287, #69896, #32085, .T. ) ;
#25833 = EDGE_CURVE ( 'NONE', #14148, #45353, #21819, .T. ) ;
#25834 = ORIENTED_EDGE ( 'NONE', *, *, #60195, .F. ) ;
#25835 = DIRECTION ( 'NONE',  ( 1.000000000000000000, 0.000000000000000000, 0.000000000000000000 ) ) ;
#25837 = DIRECTION ( 'NONE',  ( 1.836970198721029934E-16, 1.836970198721010706E-16, -1.000000000000000000 ) ) ;
#25836 = DIRECTION ( 'NONE',  ( 1.000000000000000000, -0.000000000000000000, -0.000000000000000000 ) ) ;
#25838 = EDGE_LOOP ( 'NONE', ( #40599, #46482, #18148, #41735 ) ) ;
#25841 = EDGE_LOOP ( 'NONE', ( #37244, #40498, #55706, #58332 ) ) ;
#25840 = ADVANCED_FACE ( 'NONE', ( #64958, #22856 ), #21471, .F. ) ;
#25839 = CARTESIAN_POINT ( 'NONE',  ( 8.250000000000005329, -7.249999999999998224, -23.00000000000000000 ) ) ;
#25842 = ORIENTED_EDGE ( 'NONE', *, *, #65780, .T. ) ;
#25843 = EDGE_CURVE ( 'NONE', #55741, #41566, #27472, .T. ) ;
#25844 = CARTESIAN_POINT ( 'NONE',  ( 283.0000000000000568, -30.45000000000094786, -14.49999999999906031 ) ) ;
#25845 = EDGE_CURVE ( 'NONE', #36419, #48765, #55055, .T. ) ;
#25846 = AXIS2_PLACEMENT_3D ( 'NONE', #42679, #47986, #12482 ) ;
#25847 = SHAPE_REPRESENTATION ( '6266N13_Heavy Duty Locking-Slotted Fitting1_6266N13', ( #45918 ), #48210 ) ;
#25848 = CARTESIAN_POINT ( 'NONE',  ( -7.250000000000000888, -8.249999999999998224, -24.50000000000000000 ) ) ;
#25849 = ORIENTED_EDGE ( 'NONE', *, *, #35645, .F. ) ;
#25850 = ORIENTED_EDGE ( 'NONE', *, *, #15726, .F. ) ;
#25851 = AXIS2_PLACEMENT_3D ( 'NONE', #67342, #9697, #40810 ) ;
#25852 = CYLINDRICAL_SURFACE ( 'NONE', #43212, 2.458500000000000796 ) ;
#25853 = DIRECTION ( 'NONE',  ( -0.000000000000000000, -0.000000000000000000, -1.000000000000000000 ) ) ;
#25854 = ADVANCED_FACE ( 'NONE', ( #604 ), #48694, .F. ) ;
#25855 = ORIENTED_EDGE ( 'NONE', *, *, #5169, .F. ) ;
#25856 = ORIENTED_EDGE ( 'NONE', *, *, #53090, .T. ) ;
#25857 = DIRECTION ( 'NONE',  ( 0.000000000000000000, -1.000000000000000000, 0.000000000000000000 ) ) ;
#25858 = LINE ( 'NONE', #14894, #45176 ) ;
#25859 = ORIENTED_EDGE ( 'NONE', *, *, #31267, .T. ) ;
#25860 = VECTOR ( 'NONE', #32740, 1000.000000000000000 ) ;
#25861 = CARTESIAN_POINT ( 'NONE',  ( -8.593516549646745162, -7.616533956692185470, 195.0000000000000284 ) ) ;
#25862 = EDGE_CURVE ( 'NONE', #68801, #61197, #65648, .T. ) ;
#25863 = DIRECTION ( 'NONE',  ( -0.000000000000000000, 1.000000000000000000, -0.000000000000000000 ) ) ;
#25865 = ORIENTED_EDGE ( 'NONE', *, *, #29632, .F. ) ;
#25864 = DIRECTION ( 'NONE',  ( 0.000000000000000000, 1.000000000000000000, -0.000000000000000000 ) ) ;
#25867 = ORIENTED_EDGE ( 'NONE', *, *, #67786, .T. ) ;
#25866 = DIRECTION ( 'NONE',  ( -1.836970198721029934E-16, 1.836970198721036590E-16, -1.000000000000000000 ) ) ;
#25868 = DIRECTION ( 'NONE',  ( 0.000000000000000000, 0.000000000000000000, 1.000000000000000000 ) ) ;
#25869 = CARTESIAN_POINT ( 'NONE',  ( -7.450000000000001954, 7.250000000000000000, -12.00000000000000000 ) ) ;
#25870 = CARTESIAN_POINT ( 'NONE',  ( 18.89999999999999858, 13.66939075806899950, 20.80000000000000426 ) ) ;
#25871 = LINE ( 'NONE', #58032, #12043 ) ;
#25872 = EDGE_CURVE ( 'NONE', #44963, #68597, #17200, .T. ) ;
#25873 = DIRECTION ( 'NONE',  ( 0.000000000000000000, 0.000000000000000000, 1.000000000000000000 ) ) ;
#25874 = CARTESIAN_POINT ( 'NONE',  ( 283.0000000000000568, -26.50000000000000000, -0.5000000000000000000 ) ) ;
#25875 = ORIENTED_EDGE ( 'NONE', *, *, #35897, .T. ) ;
#25876 = CARTESIAN_POINT ( 'NONE',  ( 9.690000000000001279, -9.750000000000001776, -5.000000000000000000 ) ) ;
#25877 = ADVANCED_FACE ( 'NONE', ( #1293 ), #44404, .T. ) ;
#25879 = ORIENTED_EDGE ( 'NONE', *, *, #10347, .F. ) ;
#25878 = CARTESIAN_POINT ( 'NONE',  ( 5.257023737882819070, -5.257023737882825287, 54.00000000000000711 ) ) ;
#25880 = DIRECTION ( 'NONE',  ( -0.000000000000000000, -0.000000000000000000, -1.000000000000000000 ) ) ;
#25881 = FACE_BOUND ( 'NONE', #8551, .T. ) ;
#25882 = CARTESIAN_POINT ( 'NONE',  ( 8.406483450353382736, 4.383466043307721272, 455.0000000000000568 ) ) ;
#25883 = EDGE_CURVE ( 'NONE', #5458, #58797, #65977, .T. ) ;
#25884 = DIRECTION ( 'NONE',  ( 0.000000000000000000, 0.000000000000000000, -1.000000000000000000 ) ) ;
#25885 = ORIENTED_EDGE ( 'NONE', *, *, #17714, .F. ) ;
#25886 = CARTESIAN_POINT ( 'NONE',  ( -4.727349090213504468, -4.201500623656015065, 195.0000000000000284 ) ) ;
#25887 = CARTESIAN_POINT ( 'NONE',  ( 10.50702373788280752, 6.835476262117182067, 54.00000000000000711 ) ) ;
#25888 = VERTEX_POINT ( 'NONE', #1623 ) ;
#25889 = VECTOR ( 'NONE', #17823, 1000.000000000000000 ) ;
#25890 = CARTESIAN_POINT ( 'NONE',  ( 7.250000000000004441, 7.450000000000001954, -11.50000000000000000 ) ) ;
#25891 = CARTESIAN_POINT ( 'NONE',  ( 10.00000000000000000, 18.00000000000000355, -21.00000000000000000 ) ) ;
#25892 = EDGE_CURVE ( 'NONE', #48101, #14855, #55309, .T. ) ;
#25893 = AXIS2_PLACEMENT_3D ( 'NONE', #33636, #6754, #17723 ) ;
#25894 = DIRECTION ( 'NONE',  ( 0.000000000000000000, 1.000000000000000000, 0.000000000000000000 ) ) ;
#25895 = VERTEX_POINT ( 'NONE', #51468 ) ;
#25896 = CARTESIAN_POINT ( 'NONE',  ( 7.250000000000005329, -7.249999999999998224, -9.000000000000001776 ) ) ;
#25897 = ORIENTED_EDGE ( 'NONE', *, *, #18138, .T. ) ;
#25898 = ADVANCED_FACE ( 'NONE', ( #18947 ), #23896, .T. ) ;
#25899 = EDGE_LOOP ( 'NONE', ( #49471, #61500, #39763, #17625 ) ) ;
#25900 = EDGE_CURVE ( 'NONE', #58759, #64954, #33827, .T. ) ;
#25901 = VECTOR ( 'NONE', #58497, 1000.000000000000000 ) ;
#25902 = DIRECTION ( 'NONE',  ( 0.000000000000000000, -0.9921567416492215186, -0.1249999999999996531 ) ) ;
#25903 = DIRECTION ( 'NONE',  ( 0.4999999999989417354, 0.000000000000000000, 0.8660254037850495523 ) ) ;
#25904 = DIRECTION ( 'NONE',  ( -1.000000000000000000, 0.000000000000000000, -0.000000000000000000 ) ) ;
#25905 = ADVANCED_FACE ( 'NONE', ( #8323 ), #12572, .T. ) ;
#25906 = ADVANCED_FACE ( 'NONE', ( #67393 ), #23545, .F. ) ;
#25907 = EDGE_CURVE ( 'NONE', #26074, #57794, #30468, .T. ) ;
#25908 = CIRCLE ( 'NONE', #3331, 0.1999999999999987899 ) ;
#25909 = DIRECTION ( 'NONE',  ( -1.000000000000000000, 0.000000000000000000, 0.000000000000000000 ) ) ;
#25910 = DIRECTION ( 'NONE',  ( -1.836970198721029934E-16, 1.836970198721036344E-16, -1.000000000000000000 ) ) ;
#25911 = ORIENTED_EDGE ( 'NONE', *, *, #52293, .T. ) ;
#25912 = VERTEX_POINT ( 'NONE', #61724 ) ;
#25914 = EDGE_LOOP ( 'NONE', ( #58303, #10961, #49057, #32568 ) ) ;
#25913 = DIRECTION ( 'NONE',  ( 0.000000000000000000, 0.000000000000000000, -1.000000000000000000 ) ) ;
#25915 = EDGE_CURVE ( 'NONE', #41272, #30271, #68783, .T. ) ;
#25916 = ORIENTED_EDGE ( 'NONE', *, *, #31297, .T. ) ;
#25917 = CIRCLE ( 'NONE', #23656, 4.000000000000000888 ) ;
#25918 = DIRECTION ( 'NONE',  ( 0.000000000000000000, 1.000000000000000000, -0.000000000000000000 ) ) ;
#25919 = LINE ( 'NONE', #41809, #68193 ) ;
#25920 = EDGE_CURVE ( 'NONE', #45036, #9839, #39792, .T. ) ;
#25921 = CARTESIAN_POINT ( 'NONE',  ( 7.250000000000005329, -8.249999999999998224, -23.00000000000000000 ) ) ;
#25922 = EDGE_CURVE ( 'NONE', #32175, #55318, #29545, .T. ) ;
#25923 = DIRECTION ( 'NONE',  ( 0.000000000000000000, 0.000000000000000000, 1.000000000000000000 ) ) ;
#25924 = AXIS2_PLACEMENT_3D ( 'NONE', #8534, #34349, #50282 ) ;
#25926 = CARTESIAN_POINT ( 'NONE',  ( 6.006483450353379716, -6.006483450353394815, 195.0000000000000284 ) ) ;
#25925 = DIRECTION ( 'NONE',  ( -0.7671651518153105309, -0.6414496315691445849, 0.000000000000000000 ) ) ;
#25927 = ORIENTED_EDGE ( 'NONE', *, *, #35319, .T. ) ;
#25928 = ORIENTED_EDGE ( 'NONE', *, *, #61545, .T. ) ;
#25929 = ORIENTED_EDGE ( 'NONE', *, *, #790, .T. ) ;
#25930 = DIRECTION ( 'NONE',  ( 0.000000000000000000, 0.000000000000000000, 1.000000000000000000 ) ) ;
#25931 = ADVANCED_FACE ( 'NONE', ( #61361 ), #24247, .F. ) ;
#25932 = CARTESIAN_POINT ( 'NONE',  ( -11.33351654964671162, 1.077516549646603483, 455.0000000000000568 ) ) ;
#25933 = EDGE_CURVE ( 'NONE', #49333, #35740, #41665, .T. ) ;
#25934 = FACE_OUTER_BOUND ( 'NONE', #54346, .T. ) ;
#25935 = VERTEX_POINT ( 'NONE', #34139 ) ;
#25936 = ORIENTED_EDGE ( 'NONE', *, *, #13277, .F. ) ;
#25937 = EDGE_LOOP ( 'NONE', ( #49988, #12683, #63959, #42260 ) ) ;
#25938 = DIRECTION ( 'NONE',  ( 1.000000000000000000, -0.000000000000000000, -0.000000000000000000 ) ) ;
#25939 = ORIENTED_EDGE ( 'NONE', *, *, #14644, .T. ) ;
#25940 = ORIENTED_EDGE ( 'NONE', *, *, #64230, .F. ) ;
#25941 = DIRECTION ( 'NONE',  ( -3.491481338843133355E-15, -1.000000000000000000, -1.836970198721029934E-16 ) ) ;
#25942 = EDGE_CURVE ( 'NONE', #903, #29890, #3042, .T. ) ;
#25943 = ORIENTED_EDGE ( 'NONE', *, *, #7995, .F. ) ;
#25944 = EDGE_LOOP ( 'NONE', ( #50675, #3600, #4283, #18262 ) ) ;
#25945 = CARTESIAN_POINT ( 'NONE',  ( -13.00000000000000178, -15.50000000000000000, -2.000000000000000000 ) ) ;
#25947 = VERTEX_POINT ( 'NONE', #7272 ) ;
#25946 = DIRECTION ( 'NONE',  ( -0.000000000000000000, -0.000000000000000000, -1.000000000000000000 ) ) ;
#25948 = AXIS2_PLACEMENT_3D ( 'NONE', #48679, #28147, #5548 ) ;
#25949 = ORIENTED_EDGE ( 'NONE', *, *, #37875, .T. ) ;
#25950 = AXIS2_PLACEMENT_3D ( 'NONE', #46241, #19028, #23281 ) ;
#25951 = ADVANCED_BREP_SHAPE_REPRESENTATION ( '', ( #44754, #45918 ), #48210 ) ;
#25952 = CARTESIAN_POINT ( 'NONE',  ( 11.19368345035336176, 11.99351654964661051, 195.0000000000000284 ) ) ;
#25953 = DIRECTION ( 'NONE',  ( -1.836970198721029934E-16, 1.836970198721036344E-16, -1.000000000000000000 ) ) ;
#25955 = ORIENTED_EDGE ( 'NONE', *, *, #24978, .T. ) ;
#25954 = CARTESIAN_POINT ( 'NONE',  ( -7.793516549646827940, -11.12648345035340647, 455.0000000000000568 ) ) ;
#25956 = ORIENTED_EDGE ( 'NONE', *, *, #14327, .T. ) ;
#25957 = VECTOR ( 'NONE', #30030, 1000.000000000000000 ) ;
#25958 = DIRECTION ( 'NONE',  ( -0.6414496315691494699, 0.7671651518153064231, 0.000000000000000000 ) ) ;
#25959 = CARTESIAN_POINT ( 'NONE',  ( -2.355476262117325525, -9.562023737882830332, 54.00000000000000711 ) ) ;
#25960 = DIRECTION ( 'NONE',  ( 0.000000000000000000, -1.000000000000000000, 0.000000000000000000 ) ) ;
#25961 = VECTOR ( 'NONE', #23001, 1000.000000000000114 ) ;
#25962 = DIRECTION ( 'NONE',  ( 0.000000000000000000, 1.000000000000000000, 0.000000000000000000 ) ) ;
#25963 = ORIENTED_EDGE ( 'NONE', *, *, #285, .F. ) ;
#25964 = CARTESIAN_POINT ( 'NONE',  ( 283.0000000000000568, -32.94999999999885176, 8.199999999997979572 ) ) ;
#25965 = ADVANCED_FACE ( 'NONE', ( #24606 ), #28838, .T. ) ;
#25966 = PLANE ( 'NONE',  #64875 ) ;
#25967 = DIRECTION ( 'NONE',  ( -0.4999999999999832356, 0.000000000000000000, 0.8660254037844483666 ) ) ;
#25969 = ADVANCED_FACE ( 'NONE', ( #60683 ), #1982, .T. ) ;
#25968 = LINE ( 'NONE', #42213, #12148 ) ;
#25970 = DIRECTION ( 'NONE',  ( 1.000000000000000000, 0.000000000000000000, 0.000000000000000000 ) ) ;
#25971 = VECTOR ( 'NONE', #18673, 1000.000000000000000 ) ;
#25972 = FACE_OUTER_BOUND ( 'NONE', #30769, .T. ) ;
#25973 = ADVANCED_FACE ( 'NONE', ( #50760 ), #17894, .F. ) ;
#25974 = VERTEX_POINT ( 'NONE', #19290 ) ;
#25975 = ADVANCED_FACE ( 'NONE', ( #10094 ), #26013, .T. ) ;
#25976 = CARTESIAN_POINT ( 'NONE',  ( -17.00000000000000000, -16.28999999999710369, -14.50000000000000000 ) ) ;
#25977 = DIRECTION ( 'NONE',  ( 1.000000000000000000, 0.000000000000000000, 0.000000000000000000 ) ) ;
#25978 = EDGE_LOOP ( 'NONE', ( #51042, #66559, #51308, #2835 ) ) ;
#25979 = VECTOR ( 'NONE', #2685, 1000.000000000000000 ) ;
#25980 = LINE ( 'NONE', #47537, #29302 ) ;
#25981 = CARTESIAN_POINT ( 'NONE',  ( -9.897976262117259338, 3.842976262117183683, 54.00000000000000711 ) ) ;
#25982 = CARTESIAN_POINT ( 'NONE',  ( 13.00000000000000178, -17.35230188589299871, 15.35019951917099945 ) ) ;
#25983 = CARTESIAN_POINT ( 'NONE',  ( 8.750000000000005329, -7.249999999999997335, -26.00000000000001066 ) ) ;
#25984 = CARTESIAN_POINT ( 'NONE',  ( 25.49999999999869971, -15.50000000000000000, 22.50000000000000000 ) ) ;
#25985 = VERTEX_POINT ( 'NONE', #52897 ) ;
#25986 = LINE ( 'NONE', #47202, #16303 ) ;
#25987 = FACE_OUTER_BOUND ( 'NONE', #10438, .T. ) ;
#25988 = FACE_OUTER_BOUND ( 'NONE', #50428, .T. ) ;
#25989 = EDGE_CURVE ( 'NONE', #39974, #49724, #9388, .T. ) ;
#25990 = DIRECTION ( 'NONE',  ( -1.000000000000000000, 0.000000000000000000, 0.000000000000000000 ) ) ;
#25991 =( REPRESENTATION_RELATIONSHIP ('NONE','NONE', #33057, #62481 ) REPRESENTATION_RELATIONSHIP_WITH_TRANSFORMATION ( #69228 )SHAPE_REPRESENTATION_RELATIONSHIP( ) );
#25992 = LINE ( 'NONE', #47550, #50903 ) ;
#25993 = ORIENTED_EDGE ( 'NONE', *, *, #52163, .F. ) ;
#25994 = VECTOR ( 'NONE', #30590, 1000.000000000000000 ) ;
#25996 = ORIENTED_EDGE ( 'NONE', *, *, #66614, .T. ) ;
#25995 = DIRECTION ( 'NONE',  ( 1.000000000000000000, 1.570596175624152290E-15, 5.770276737693577136E-31 ) ) ;
#25997 = AXIS2_PLACEMENT_3D ( 'NONE', #53659, #54697, #54015 ) ;
#25998 = CIRCLE ( 'NONE', #18189, 2.215251240775983899 ) ;
#25999 = CARTESIAN_POINT ( 'NONE',  ( -28.00000000000000000, -15.50000000000000000, -14.50000000000000000 ) ) ;
#26000 = LINE ( 'NONE', #47558, #68478 ) ;
#26001 = FACE_OUTER_BOUND ( 'NONE', #16612, .T. ) ;
#26002 = ORIENTED_EDGE ( 'NONE', *, *, #54153, .T. ) ;
#26003 = AXIS2_PLACEMENT_3D ( 'NONE', #36384, #57951, #9520 ) ;
#26004 = CARTESIAN_POINT ( 'NONE',  ( -7.450000000000001954, 0.000000000000000000, -23.50000000000000000 ) ) ;
#26005 = LINE ( 'NONE', #26341, #56664 ) ;
#26006 = VERTEX_POINT ( 'NONE', #31669 ) ;
#26007 = ORIENTED_EDGE ( 'NONE', *, *, #34229, .T. ) ;
#26008 = AXIS2_PLACEMENT_3D ( 'NONE', #33865, #38829, #60055 ) ;
#26009 = VERTEX_POINT ( 'NONE', #20344 ) ;
#26010 = EDGE_CURVE ( 'NONE', #31468, #53653, #41202, .T. ) ;
#26011 = DIRECTION ( 'NONE',  ( 0.000000000000000000, 0.000000000000000000, 1.000000000000000000 ) ) ;
#26012 = AXIS2_PLACEMENT_3D ( 'NONE', #1781, #18381, #12038 ) ;
#26013 = CYLINDRICAL_SURFACE ( 'NONE', #6632, 0.1999999999999996503 ) ;
#26015 = EDGE_CURVE ( 'NONE', #52878, #37597, #49545, .T. ) ;
#26014 = DIRECTION ( 'NONE',  ( 0.000000000000000000, 0.000000000000000000, 1.000000000000000000 ) ) ;
#26016 = ORIENTED_EDGE ( 'NONE', *, *, #25833, .T. ) ;
#26017 = ORIENTED_EDGE ( 'NONE', *, *, #41448, .F. ) ;
#26019 = CARTESIAN_POINT ( 'NONE',  ( -11.00000000000000000, -9.199999999999999289, 12.69999999999986073 ) ) ;
#26018 = VECTOR ( 'NONE', #29067, 1000.000000000000000 ) ;
#26020 = ORIENTED_EDGE ( 'NONE', *, *, #40487, .T. ) ;
#26021 = ORIENTED_EDGE ( 'NONE', *, *, #8792, .T. ) ;
#26022 = ORIENTED_EDGE ( 'NONE', *, *, #42659, .F. ) ;
#26023 = VERTEX_POINT ( 'NONE', #47567 ) ;
#26024 = FACE_OUTER_BOUND ( 'NONE', #36840, .T. ) ;
#26025 = UNCERTAINTY_MEASURE_WITH_UNIT (LENGTH_MEASURE( 1.000000000000000082E-05 ), #19999, 'distance_accuracy_value', 'NONE');
#26027 = ORIENTED_EDGE ( 'NONE', *, *, #11856, .T. ) ;
#26026 = CARTESIAN_POINT ( 'NONE',  ( 7.806483450353379538, -11.12648345035348996, 455.0000000000000568 ) ) ;
#26028 = DIRECTION ( 'NONE',  ( -1.000000000000000000, -0.000000000000000000, -0.000000000000000000 ) ) ;
#26029 = DIRECTION ( 'NONE',  ( 0.000000000000000000, 0.000000000000000000, 1.000000000000000000 ) ) ;
#26030 = AXIS2_PLACEMENT_3D ( 'NONE', #37592, #1728, #23302 ) ;
#26031 = DIRECTION ( 'NONE',  ( 8.673617379884051249E-15, 1.000000000000000000, 0.000000000000000000 ) ) ;
#26032 = EDGE_LOOP ( 'NONE', ( #56019, #23052, #35536, #41222 ) ) ;
#26033 = EDGE_LOOP ( 'NONE', ( #1230, #66080, #48998, #27210 ) ) ;
#26034 = DIRECTION ( 'NONE',  ( -1.836970198721029934E-16, 1.836970198721036590E-16, -1.000000000000000000 ) ) ;
#26035 = DIRECTION ( 'NONE',  ( 0.000000000000000000, 0.000000000000000000, -1.000000000000000000 ) ) ;
#26036 = CIRCLE ( 'NONE', #2296, 24.99999999998789946 ) ;
#26037 = ORIENTED_EDGE ( 'NONE', *, *, #25933, .T. ) ;
#26038 = EDGE_CURVE ( 'NONE', #22255, #58992, #37151, .T. ) ;
#26039 = VECTOR ( 'NONE', #29524, 1000.000000000000000 ) ;
#26040 = DIRECTION ( 'NONE',  ( 0.000000000000000000, 0.000000000000000000, 1.000000000000000000 ) ) ;
#26041 = CYLINDRICAL_SURFACE ( 'NONE', #18909, 1.000000000000000000 ) ;
#26042 = CARTESIAN_POINT ( 'NONE',  ( 9.804883450353379715, -10.20488345035352928, 455.0000000000000568 ) ) ;
#26043 = ORIENTED_EDGE ( 'NONE', *, *, #31157, .T. ) ;
#26044 = FACE_OUTER_BOUND ( 'NONE', #23971, .T. ) ;
#26047 = EDGE_CURVE ( 'NONE', #54166, #68564, #12264, .T. ) ;
#26046 = CARTESIAN_POINT ( 'NONE',  ( 11.08848345035334404, -11.08848345035349148, 455.0000000000000568 ) ) ;
#26045 = AXIS2_PLACEMENT_3D ( 'NONE', #11163, #28458, #54314 ) ;
#26048 = CARTESIAN_POINT ( 'NONE',  ( -25.50000000000000355, 0.000000000000000000, 24.75000000000000000 ) ) ;
#26049 = CARTESIAN_POINT ( 'NONE',  ( -11.25000000000000000, 11.18999999999999950, -5.000000000000000000 ) ) ;
#26050 = ADVANCED_FACE ( 'NONE', ( #58175 ), #2137, .T. ) ;
#26051 = EDGE_CURVE ( 'NONE', #62970, #19180, #14350, .T. ) ;
#26052 = LINE ( 'NONE', #43700, #53478 ) ;
#26054 = ORIENTED_EDGE ( 'NONE', *, *, #6473, .F. ) ;
#26053 = EDGE_CURVE ( 'NONE', #19699, #6379, #51815, .T. ) ;
#26055 = DIRECTION ( 'NONE',  ( 0.000000000000000000, 0.000000000000000000, -1.000000000000000000 ) ) ;
#26056 = EDGE_CURVE ( 'NONE', #49881, #39955, #21343, .T. ) ;
#26057 = DIRECTION ( 'NONE',  ( -0.6414496315691415873, 0.7671651518153131954, 2.309356642089130310E-17 ) ) ;
#26058 = FACE_OUTER_BOUND ( 'NONE', #28948, .T. ) ;
#26059 = CARTESIAN_POINT ( 'NONE',  ( 46.39999999999999858, 21.00000000000000000, 2.250000000000000444 ) ) ;
#26060 = ADVANCED_FACE ( 'NONE', ( #46505 ), #63129, .T. ) ;
#26061 = ORIENTED_EDGE ( 'NONE', *, *, #46348, .F. ) ;
#26062 = DIRECTION ( 'NONE',  ( 1.000000000000000000, 0.000000000000000000, 0.000000000000000000 ) ) ;
#26063 = DIRECTION ( 'NONE',  ( 0.000000000000000000, -0.6857142857147903170, 0.7278708115913530285 ) ) ;
#26064 = VECTOR ( 'NONE', #67154, 1000.000000000000000 ) ;
#26065 = CARTESIAN_POINT ( 'NONE',  ( -6.835476262117333057, -10.31452373788278543, 54.00000000000000711 ) ) ;
#26066 = CIRCLE ( 'NONE', #54280, 0.5000000000079367624 ) ;
#26067 = CARTESIAN_POINT ( 'NONE',  ( -29.50000000000000355, -11.50000000000000000, -15.00000000000000000 ) ) ;
#26068 = ORIENTED_EDGE ( 'NONE', *, *, #21117, .T. ) ;
#26069 = FACE_BOUND ( 'NONE', #36582, .T. ) ;
#26070 = DIRECTION ( 'NONE',  ( -1.000000000000000000, -1.570596175624152290E-15, 0.000000000000000000 ) ) ;
#26071 = FACE_OUTER_BOUND ( 'NONE', #66738, .T. ) ;
#26072 = DIRECTION ( 'NONE',  ( 1.836970198721029934E-16, 1.836970198721010706E-16, -1.000000000000000000 ) ) ;
#26073 = CARTESIAN_POINT ( 'NONE',  ( 6.750000000000000000, 7.750000000000000000, 0.000000000000000000 ) ) ;
#26074 = VERTEX_POINT ( 'NONE', #35910 ) ;
#26075 = EDGE_LOOP ( 'NONE', ( #56769, #35867, #25305, #30717 ) ) ;
#26076 = DIRECTION ( 'NONE',  ( 0.000000000000000000, 0.000000000000000000, 1.000000000000000000 ) ) ;
#26077 = AXIS2_PLACEMENT_3D ( 'NONE', #28518, #55407, #27838 ) ;
#26078 = CARTESIAN_POINT ( 'NONE',  ( 7.000000000000000000, -21.00000000000000000, -12.50000000000000000 ) ) ;
#26079 = EDGE_LOOP ( 'NONE', ( #28341, #3362, #10020, #68632 ) ) ;
#26080 = DIRECTION ( 'NONE',  ( 0.000000000000000000, 1.000000000000000000, 0.000000000000000000 ) ) ;
#26081 = DIRECTION ( 'NONE',  ( -1.000000000000000000, 0.000000000000000000, 0.000000000000000000 ) ) ;
#26082 = ORIENTED_EDGE ( 'NONE', *, *, #7209, .T. ) ;
#26083 = LINE ( 'NONE', #41985, #10799 ) ;
#26084 = VERTEX_POINT ( 'NONE', #14692 ) ;
#26085 = EDGE_LOOP ( 'NONE', ( #43318, #55822, #67373, #33578 ) ) ;
#26086 = FACE_OUTER_BOUND ( 'NONE', #3623, .T. ) ;
#26087 = VECTOR ( 'NONE', #24194, 1000.000000000000000 ) ;
#26088 = ORIENTED_EDGE ( 'NONE', *, *, #66371, .F. ) ;
#26089 = DIRECTION ( 'NONE',  ( -1.000000000000000000, 0.000000000000000000, 0.000000000000000000 ) ) ;
#26091 = ADVANCED_FACE ( 'NONE', ( #36978 ), #3384, .T. ) ;
#26090 = DIRECTION ( 'NONE',  ( 1.836970198721029934E-16, 1.836970198721010706E-16, -1.000000000000000000 ) ) ;
#26093 = CARTESIAN_POINT ( 'NONE',  ( 6.006483450353401921, 5.993516549646582092, 455.0000000000000568 ) ) ;
#26092 = AXIS2_PLACEMENT_3D ( 'NONE', #10290, #4984, #25513 ) ;
#26094 = ORIENTED_EDGE ( 'NONE', *, *, #54455, .T. ) ;
#26095 = EDGE_CURVE ( 'NONE', #4872, #37027, #33737, .T. ) ;
#26096 = AXIS2_PLACEMENT_3D ( 'NONE', #59450, #11014, #32588 ) ;
#26097 = LINE ( 'NONE', #25042, #56022 ) ;
#26098 = ADVANCED_FACE ( 'NONE', ( #3731 ), #52529, .F. ) ;
#26100 = CARTESIAN_POINT ( 'NONE',  ( -7.250000000000000888, -8.249999999999998224, -15.00000000000000000 ) ) ;
#26099 = LINE ( 'NONE', #6848, #36089 ) ;
#26101 = VERTEX_POINT ( 'NONE', #25304 ) ;
#26102 = ORIENTED_EDGE ( 'NONE', *, *, #17658, .T. ) ;
#26103 = ORIENTED_EDGE ( 'NONE', *, *, #43886, .F. ) ;
#26104 = ADVANCED_FACE ( 'NONE', ( #36252 ), #57818, .T. ) ;
#26105 = VECTOR ( 'NONE', #23794, 1000.000000000000000 ) ;
#26106 = VECTOR ( 'NONE', #17539, 1000.000000000000114 ) ;
#26108 = ORIENTED_EDGE ( 'NONE', *, *, #28184, .T. ) ;
#26107 = SHAPE_DEFINITION_REPRESENTATION ( #66280, #62481 ) ;
#26109 = DIRECTION ( 'NONE',  ( 0.000000000000000000, 0.000000000000000000, 1.000000000000000000 ) ) ;
#26111 = ORIENTED_EDGE ( 'NONE', *, *, #56932, .T. ) ;
#26110 = DIRECTION ( 'NONE',  ( -1.000000000000000000, 0.000000000000000000, 0.000000000000000000 ) ) ;
#26112 = CIRCLE ( 'NONE', #123, 0.8099999999999999423 ) ;
#26113 = CARTESIAN_POINT ( 'NONE',  ( -7.250000000000001776, -7.249999999999998224, -17.00000000000000000 ) ) ;
#26114 = LINE ( 'NONE', #63230, #23782 ) ;
#26115 = ORIENTED_EDGE ( 'NONE', *, *, #22713, .F. ) ;
#26116 = ORIENTED_EDGE ( 'NONE', *, *, #16029, .F. ) ;
#26117 = AXIS2_PLACEMENT_3D ( 'NONE', #2997, #55766, #24905 ) ;
#26118 = DIRECTION ( 'NONE',  ( 0.000000000000000000, 0.000000000000000000, 1.000000000000000000 ) ) ;
#26119 = ORIENTED_EDGE ( 'NONE', *, *, #20105, .T. ) ;
#26120 = CARTESIAN_POINT ( 'NONE',  ( 11.75000000000000000, -5.000000000000000000, 21.10805890929250239 ) ) ;
#26121 = CARTESIAN_POINT ( 'NONE',  ( 4.149127210878726935, -3.677663764522648204, 54.00000000000000711 ) ) ;
#26122 = CARTESIAN_POINT ( 'NONE',  ( 24.00000000000000000, -16.28999999999710369, -14.50000000000000000 ) ) ;
#26123 = VERTEX_POINT ( 'NONE', #54975 ) ;
#26124 = EDGE_CURVE ( 'NONE', #52731, #34737, #19051, .T. ) ;
#26125 = CARTESIAN_POINT ( 'NONE',  ( 9.955011587777223170, 2.752095193409229701, 455.0000000000000568 ) ) ;
#26126 = CARTESIAN_POINT ( 'NONE',  ( 41.09999999999999432, -21.00000000000000000, -13.86939075806900057 ) ) ;
#26127 = VECTOR ( 'NONE', #30972, 1000.000000000000000 ) ;
#26129 = ORIENTED_EDGE ( 'NONE', *, *, #47724, .F. ) ;
#26128 = CARTESIAN_POINT ( 'NONE',  ( 1.866219381641485375, 9.404046420174006826, 455.0000000000000568 ) ) ;
#26131 = ORIENTED_EDGE ( 'NONE', *, *, #21740, .F. ) ;
#26130 = LINE ( 'NONE', #10206, #23012 ) ;
#26132 = CARTESIAN_POINT ( 'NONE',  ( -2.406732575409666008, -8.711985858128704407, 26.00000000000000711 ) ) ;
#26133 = CARTESIAN_POINT ( 'NONE',  ( 275.0000000000000000, -38.64999999999999858, -12.69999999999999929 ) ) ;
#26134 = DIRECTION ( 'NONE',  ( 1.836970198721029934E-16, 1.836970198721010706E-16, -1.000000000000000000 ) ) ;
#26135 = LINE ( 'NONE', #4226, #52050 ) ;
#26136 = CARTESIAN_POINT ( 'NONE',  ( -25.50000000000000355, -5.578999999999999737, 22.50000000000000000 ) ) ;
#26137 = ORIENTED_EDGE ( 'NONE', *, *, #4469, .F. ) ;
#26138 = CARTESIAN_POINT ( 'NONE',  ( 11.50000000000000000, -11.50000000000100009, 15.00000000000084910 ) ) ;
#26139 = EDGE_CURVE ( 'NONE', #27517, #11827, #16438, .T. ) ;
#26140 = DIRECTION ( 'NONE',  ( -5.981805089575196197E-17, -1.000000000000000000, 0.000000000000000000 ) ) ;
#26141 = VECTOR ( 'NONE', #7485, 1000.000000000000000 ) ;
#26142 = CARTESIAN_POINT ( 'NONE',  ( 7.826483450353380000, -12.00648345035349251, 455.0000000000000568 ) ) ;
#26144 = ORIENTED_EDGE ( 'NONE', *, *, #27982, .T. ) ;
#26143 = DIRECTION ( 'NONE',  ( -0.7671651518153006499, 0.6414496315691565753, 0.000000000000000000 ) ) ;
#26145 = CARTESIAN_POINT ( 'NONE',  ( 47.00000000000000000, 0.7500000000000000000, -5.000000000000000000 ) ) ;
#26146 = EDGE_CURVE ( 'NONE', #60163, #30760, #4399, .T. ) ;
#26147 = CARTESIAN_POINT ( 'NONE',  ( -8.250000000000001776, -7.249999999999998224, -22.00000000000000000 ) ) ;
#26148 = DIRECTION ( 'NONE',  ( 0.000000000000000000, 0.000000000000000000, -1.000000000000000000 ) ) ;
#26149 = DIRECTION ( 'NONE',  ( 0.000000000000000000, 0.000000000000000000, 1.000000000000000000 ) ) ;
#26150 = ORIENTED_EDGE ( 'NONE', *, *, #54017, .F. ) ;
#26151 = DIRECTION ( 'NONE',  ( -1.836970198721029934E-16, 1.836970198721036344E-16, -1.000000000000000000 ) ) ;
#26152 = CARTESIAN_POINT ( 'NONE',  ( 7.250000000000005329, -8.249999999999998224, -11.50000000000000000 ) ) ;
#26153 = ORIENTED_EDGE ( 'NONE', *, *, #21421, .T. ) ;
#26154 = DIRECTION ( 'NONE',  ( -1.000000000000000000, 8.359604446858500663E-15, 3.071268848394972853E-30 ) ) ;
#26155 = VECTOR ( 'NONE', #43541, 1000.000000000000000 ) ;
#26156 = CLOSED_SHELL ( 'NONE', ( #69946, #42046, #3815, #63331, #19969, #25496 ) ) ;
#26157 = CARTESIAN_POINT ( 'NONE',  ( 22.90000000000000213, -14.06939075806900874, 20.80000000000001137 ) ) ;
#26158 = CARTESIAN_POINT ( 'NONE',  ( 10.05377373788278739, -8.930623737882855906, 54.00000000000000711 ) ) ;
#26159 = CYLINDRICAL_SURFACE ( 'NONE', #50753, 0.3499999999998886224 ) ;
#26161 = ADVANCED_FACE ( 'NONE', ( #6531 ), #49321, .T. ) ;
#26160 = DIRECTION ( 'NONE',  ( -1.000000000000000000, 0.000000000000000000, 0.000000000000000000 ) ) ;
#26162 = VERTEX_POINT ( 'NONE', #69834 ) ;
#26163 = EDGE_LOOP ( 'NONE', ( #57131, #46174, #52510, #69143, #47990 ) ) ;
#26164 = DIRECTION ( 'NONE',  ( 0.6414496315691367023, -0.7671651518153173033, -2.309356642089295169E-17 ) ) ;
#26165 = ORIENTED_EDGE ( 'NONE', *, *, #29151, .T. ) ;
#26166 = ORIENTED_EDGE ( 'NONE', *, *, #58486, .F. ) ;
#26167 = LINE ( 'NONE', #41359, #50606 ) ;
#26168 = AXIS2_PLACEMENT_3D ( 'NONE', #37276, #43949, #10052 ) ;
#26169 = LINE ( 'NONE', #36781, #65999 ) ;
#26170 = LINE ( 'NONE', #4947, #36680 ) ;
#26171 = ORIENTED_EDGE ( 'NONE', *, *, #51785, .F. ) ;
#26172 = ORIENTED_EDGE ( 'NONE', *, *, #25166, .F. ) ;
#26173 = DIRECTION ( 'NONE',  ( -1.000000000000000000, 0.000000000000000000, 0.000000000000000000 ) ) ;
#26174 = ORIENTED_EDGE ( 'NONE', *, *, #21988, .T. ) ;
#26175 = EDGE_LOOP ( 'NONE', ( #29797, #17537, #21247, #57734 ) ) ;
#26176 = PLANE ( 'NONE',  #13502 ) ;
#26177 = CARTESIAN_POINT ( 'NONE',  ( -4.706725378239257296, -6.358413763958960629, 54.00000000000000711 ) ) ;
#26178 = DIRECTION ( 'NONE',  ( 0.000000000000000000, 0.000000000000000000, 1.000000000000000000 ) ) ;
#26179 = VECTOR ( 'NONE', #65919, 1000.000000000000000 ) ;
#26180 = ORIENTED_EDGE ( 'NONE', *, *, #61992, .T. ) ;
#26181 = EDGE_CURVE ( 'NONE', #6839, #59936, #53933, .T. ) ;
#26182 = LINE ( 'NONE', #3562, #57177 ) ;
#26184 = DIRECTION ( 'NONE',  ( 0.000000000000000000, -0.000000000000000000, 1.000000000000000000 ) ) ;
#26183 = DIRECTION ( 'NONE',  ( 0.000000000000000000, 0.000000000000000000, -1.000000000000000000 ) ) ;
#26185 = ORIENTED_EDGE ( 'NONE', *, *, #25900, .F. ) ;
#26187 = VERTEX_POINT ( 'NONE', #58884 ) ;
#26186 = PLANE ( 'NONE',  #5941 ) ;
#26188 = ORIENTED_EDGE ( 'NONE', *, *, #51413, .T. ) ;
#26189 = EDGE_CURVE ( 'NONE', #33919, #596, #16786, .T. ) ;
#26190 = DIRECTION ( 'NONE',  ( 0.000000000000000000, 0.000000000000000000, -1.000000000000000000 ) ) ;
#26191 = AXIS2_PLACEMENT_3D ( 'NONE', #32902, #54483, #7748 ) ;
#26192 = LINE ( 'NONE', #9936, #48535 ) ;
#26193 = ORIENTED_EDGE ( 'NONE', *, *, #28125, .T. ) ;
#26194 = FACE_OUTER_BOUND ( 'NONE', #67149, .T. ) ;
#26195 = DIRECTION ( 'NONE',  ( 1.000000000000000000, -0.000000000000000000, -0.000000000000000000 ) ) ;
#26196 = ORIENTED_EDGE ( 'NONE', *, *, #40160, .F. ) ;
#26197 = VECTOR ( 'NONE', #3895, 1000.000000000000000 ) ;
#26198 = VERTEX_POINT ( 'NONE', #183 ) ;
#26199 = CARTESIAN_POINT ( 'NONE',  ( 7.450000000000003730, -7.249999999999997335, -7.000000000000000000 ) ) ;
#26200 = EDGE_CURVE ( 'NONE', #58466, #7367, #60832, .T. ) ;
#26201 = CARTESIAN_POINT ( 'NONE',  ( 283.0000000000000568, -25.50000000000000355, -14.74860679774999994 ) ) ;
#26202 = VERTEX_POINT ( 'NONE', #42954 ) ;
#26203 = CARTESIAN_POINT ( 'NONE',  ( -7.250000000000000888, 7.250000000000001776, -26.00000000000001066 ) ) ;
#26204 = DIRECTION ( 'NONE',  ( 0.000000000000000000, 0.000000000000000000, 1.000000000000000000 ) ) ;
#26206 = ORIENTED_EDGE ( 'NONE', *, *, #46201, .T. ) ;
#26205 = DIRECTION ( 'NONE',  ( 0.000000000000000000, 0.000000000000000000, 1.000000000000000000 ) ) ;
#26208 = ORIENTED_EDGE ( 'NONE', *, *, #28411, .T. ) ;
#26207 = DIRECTION ( 'NONE',  ( 1.000000000000000000, 0.000000000000000000, 0.000000000000000000 ) ) ;
#26210 = CARTESIAN_POINT ( 'NONE',  ( 75.42576880091934299, 0.000000000000000000, 330.9830310981789694 ) ) ;
#26209 = VECTOR ( 'NONE', #20565, 1000.000000000000000 ) ;
#26211 = DIRECTION ( 'NONE',  ( 0.000000000000000000, 0.000000000000000000, 1.000000000000000000 ) ) ;
#26212 = DIRECTION ( 'NONE',  ( 0.000000000000000000, -1.000000000000000000, 0.000000000000000000 ) ) ;
#26213 = CARTESIAN_POINT ( 'NONE',  ( 10.31452373788277832, 3.842976262117149044, 26.00000000000000711 ) ) ;
#26214 = CARTESIAN_POINT ( 'NONE',  ( 18.89999999999999858, 13.66939075806899240, -20.79999999999999361 ) ) ;
#26215 = DIRECTION ( 'NONE',  ( 0.000000000000000000, 0.000000000000000000, -1.000000000000000000 ) ) ;
#26216 = EDGE_LOOP ( 'NONE', ( #38094, #5653, #35452, #26611 ) ) ;
#26217 = LINE ( 'NONE', #11000, #4495 ) ;
#26218 = EDGE_CURVE ( 'NONE', #4367, #57233, #897, .T. ) ;
#26220 = ORIENTED_EDGE ( 'NONE', *, *, #31953, .F. ) ;
#26219 = CARTESIAN_POINT ( 'NONE',  ( 7.900000000000000355, 21.00000000000000000, -13.98999642601811999 ) ) ;
#26221 = DIRECTION ( 'NONE',  ( -1.836970198721029934E-16, -1.836970198721010706E-16, 1.000000000000000000 ) ) ;
#26222 = DIRECTION ( 'NONE',  ( 0.000000000000000000, 0.000000000000000000, -1.000000000000000000 ) ) ;
#26223 = EDGE_CURVE ( 'NONE', #18304, #29522, #16800, .T. ) ;
#26224 = EDGE_CURVE ( 'NONE', #44826, #14045, #26700, .T. ) ;
#26225 = LINE ( 'NONE', #37536, #52142 ) ;
#26226 = ADVANCED_FACE ( 'NONE', ( #64538 ), #37661, .F. ) ;
#26227 = ORIENTED_EDGE ( 'NONE', *, *, #5823, .T. ) ;
#26228 = CARTESIAN_POINT ( 'NONE',  ( -7.252248008019462233, -5.393625297349887049, 195.0000000000000284 ) ) ;
#26229 = LINE ( 'NONE', #64417, #13607 ) ;
#26230 = VECTOR ( 'NONE', #22572, 1000.000000000000000 ) ;
#26231 = ORIENTED_EDGE ( 'NONE', *, *, #60013, .T. ) ;
#26232 = PRODUCT_RELATED_PRODUCT_CATEGORY ( 'part', '', ( #40168 ) ) ;
#26233 = CARTESIAN_POINT ( 'NONE',  ( -11.00000000000000000, -16.28999999999999915, -14.50000000000000000 ) ) ;
#26234 = EDGE_CURVE ( 'NONE', #65595, #64473, #10040, .T. ) ;
#26235 = LINE ( 'NONE', #25891, #23493 ) ;
#26236 = ADVANCED_FACE ( 'NONE', ( #22092 ), #38356, .F. ) ;
#26237 = CIRCLE ( 'NONE', #69130, 4.000000000000000888 ) ;
#26238 = EDGE_CURVE ( 'NONE', #37936, #60008, #11177, .T. ) ;
#26239 = CARTESIAN_POINT ( 'NONE',  ( -8.250000000000001776, 0.000000000000000000, -11.00000000000000000 ) ) ;
#26240 = ORIENTED_EDGE ( 'NONE', *, *, #58609, .T. ) ;
#26241 = DIRECTION ( 'NONE',  ( -1.000000000000000000, 0.000000000000000000, 0.000000000000000000 ) ) ;
#26242 = ORIENTED_EDGE ( 'NONE', *, *, #45644, .F. ) ;
#26243 = ORIENTED_EDGE ( 'NONE', *, *, #16980, .F. ) ;
#26244 = AXIS2_PLACEMENT_3D ( 'NONE', #13110, #2848, #44581 ) ;
#26245 = LINE ( 'NONE', #46747, #48300 ) ;
#26246 = LINE ( 'NONE', #62657, #54551 ) ;
#26247 = AXIS2_PLACEMENT_3D ( 'NONE', #66248, #5485, #23105 ) ;
#26248 = DIRECTION ( 'NONE',  ( 1.000000000000000000, -0.000000000000000000, -0.000000000000000000 ) ) ;
#26249 = DIRECTION ( 'NONE',  ( -0.000000000000000000, 1.000000000000000000, -0.000000000000000000 ) ) ;
#26250 = VERTEX_POINT ( 'NONE', #21742 ) ;
#26251 = ORIENTED_EDGE ( 'NONE', *, *, #5654, .F. ) ;
#26253 = ORIENTED_EDGE ( 'NONE', *, *, #27397, .T. ) ;
#26252 = FACE_OUTER_BOUND ( 'NONE', #1316, .T. ) ;
#26254 = EDGE_LOOP ( 'NONE', ( #38868, #16971, #9924, #38461 ) ) ;
#26255 = PLANE ( 'NONE',  #49553 ) ;
#26256 = AXIS2_PLACEMENT_3D ( 'NONE', #32843, #37465, #53729 ) ;
#26257 = CARTESIAN_POINT ( 'NONE',  ( 7.250000000000005329, -7.249999999999998224, -24.00000000000000000 ) ) ;
#26258 = EDGE_CURVE ( 'NONE', #22003, #29691, #29224, .T. ) ;
#26259 = DIRECTION ( 'NONE',  ( 0.000000000000000000, 1.000000000000000000, 0.000000000000000000 ) ) ;
#26260 = CIRCLE ( 'NONE', #69158, 5.250000000000000000 ) ;
#26261 = CARTESIAN_POINT ( 'NONE',  ( -11.50000000000000000, -11.70000000000000284, 11.00000000000000000 ) ) ;
#26263 = PLANE ( 'NONE',  #58309 ) ;
#26262 = CARTESIAN_POINT ( 'NONE',  ( 7.000000000000000000, -32.95000000000000284, 14.50000000000000000 ) ) ;
#26264 = ORIENTED_EDGE ( 'NONE', *, *, #8965, .T. ) ;
#26265 = VERTEX_POINT ( 'NONE', #59915 ) ;
#26266 = ORIENTED_EDGE ( 'NONE', *, *, #21141, .T. ) ;
#26267 = ORIENTED_EDGE ( 'NONE', *, *, #20156, .F. ) ;
#26268 = FACE_OUTER_BOUND ( 'NONE', #1812, .T. ) ;
#26269 = CYLINDRICAL_SURFACE ( 'NONE', #46772, 0.5000000000001357803 ) ;
#26270 = LINE ( 'NONE', #41825, #17302 ) ;
#26271 = ORIENTED_EDGE ( 'NONE', *, *, #45537, .F. ) ;
#26272 = ORIENTED_EDGE ( 'NONE', *, *, #43802, .T. ) ;
#26273 = VERTEX_POINT ( 'NONE', #11464 ) ;
#26274 = CARTESIAN_POINT ( 'NONE',  ( -7.250000000000000000, -7.449999999999998401, -21.50000000000000000 ) ) ;
#26275 = ORIENTED_EDGE ( 'NONE', *, *, #41904, .F. ) ;
#26276 = LINE ( 'NONE', #36530, #67213 ) ;
#26277 = VECTOR ( 'NONE', #27790, 1000.000000000000000 ) ;
#26278 = ORIENTED_EDGE ( 'NONE', *, *, #13798, .F. ) ;
#26279 = VERTEX_POINT ( 'NONE', #33042 ) ;
#26280 = CARTESIAN_POINT ( 'NONE',  ( -28.00000000000000000, -15.50000000000000000, 20.05051025721700242 ) ) ;
#26281 = EDGE_CURVE ( 'NONE', #29414, #39081, #28095, .T. ) ;
#26282 = VECTOR ( 'NONE', #14731, 1000.000000000000000 ) ;
#26284 = ORIENTED_EDGE ( 'NONE', *, *, #26056, .T. ) ;
#26283 = LINE ( 'NONE', #64472, #39052 ) ;
#26285 = ORIENTED_EDGE ( 'NONE', *, *, #31499, .F. ) ;
#26286 = CARTESIAN_POINT ( 'NONE',  ( 16.75000000000000000, -2.500000000000000000, -21.77831216351300014 ) ) ;
#26287 = FACE_OUTER_BOUND ( 'NONE', #6577, .T. ) ;
#26288 = EDGE_CURVE ( 'NONE', #27857, #7713, #34060, .T. ) ;
#26290 = ORIENTED_EDGE ( 'NONE', *, *, #34216, .F. ) ;
#26289 = LINE ( 'NONE', #36541, #60568 ) ;
#26291 = ORIENTED_EDGE ( 'NONE', *, *, #30620, .T. ) ;
#26292 = DIRECTION ( 'NONE',  ( 0.000000000000000000, 3.673940397442059868E-16, -1.000000000000000000 ) ) ;
#26293 = LINE ( 'NONE', #68027, #54752 ) ;
#26294 = ADVANCED_FACE ( 'NONE', ( #34765 ), #49646, .F. ) ;
#26295 = LINE ( 'NONE', #9690, #37443 ) ;
#26296 = EDGE_CURVE ( 'NONE', #13319, #68801, #7547, .T. ) ;
#26297 = DIRECTION ( 'NONE',  ( -0.7671651518153106419, 0.6414496315691445849, 0.000000000000000000 ) ) ;
#26298 = CARTESIAN_POINT ( 'NONE',  ( 3.430747519065294071, -7.852485183456927587, 195.0000000000000284 ) ) ;
#26299 = ORIENTED_EDGE ( 'NONE', *, *, #25327, .F. ) ;
#26300 = DIRECTION ( 'NONE',  ( -1.000000000000000000, 3.491481338843133355E-15, 1.836970198721036344E-16 ) ) ;
#26301 = ORIENTED_EDGE ( 'NONE', *, *, #61274, .F. ) ;
#26302 = DIRECTION ( 'NONE',  ( -1.000000000000000000, 0.000000000000000000, 0.000000000000000000 ) ) ;
#26303 = AXIS2_PLACEMENT_3D ( 'NONE', #19282, #3723, #30250 ) ;
#26304 = EDGE_CURVE ( 'NONE', #58150, #39317, #33727, .T. ) ;
#26305 = CARTESIAN_POINT ( 'NONE',  ( -11.00000000000000000, -11.50000000000000000, -19.00000000000000000 ) ) ;
#26307 = DIRECTION ( 'NONE',  ( 1.000000000000000000, -0.000000000000000000, -0.000000000000000000 ) ) ;
#26306 = CIRCLE ( 'NONE', #47748, 4.000000000000000888 ) ;
#26308 = CIRCLE ( 'NONE', #4858, 0.5249999999999994671 ) ;
#26309 = LINE ( 'NONE', #64162, #42708 ) ;
#26310 = ORIENTED_EDGE ( 'NONE', *, *, #19563, .F. ) ;
#26311 =( LENGTH_UNIT ( ) NAMED_UNIT ( * ) SI_UNIT ( .MILLI., .METRE. ) );
#26312 = CONICAL_SURFACE ( 'NONE', #28512, 1.621000000000000885, 0.7853981633974518317 ) ;
#26313 = EDGE_CURVE ( 'NONE', #13060, #69389, #7184, .T. ) ;
#26314 = FILL_AREA_STYLE ('',( #58845 ) ) ;
#26315 = EDGE_CURVE ( 'NONE', #381, #40067, #45082, .T. ) ;
#26316 = CIRCLE ( 'NONE', #55679, 0.8128000000000145109 ) ;
#26317 = CARTESIAN_POINT ( 'NONE',  ( 40.90000000000000568, -0.1999999999911795112, 8.826273045769999343E-12 ) ) ;
#26318 = ORIENTED_EDGE ( 'NONE', *, *, #1433, .F. ) ;
#26319 = DIRECTION ( 'NONE',  ( 0.000000000000000000, 1.000000000000000000, 0.000000000000000000 ) ) ;
#26320 = DIRECTION ( 'NONE',  ( 0.000000000000000000, 3.673940397442059868E-16, -1.000000000000000000 ) ) ;
#26321 = DIRECTION ( 'NONE',  ( -0.7071067811865474617, -0.7071067811865474617, -2.597868168706479611E-16 ) ) ;
#26322 = CARTESIAN_POINT ( 'NONE',  ( -7.250000000000000888, -8.249999999999998224, -26.00000000000001066 ) ) ;
#26323 = DIRECTION ( 'NONE',  ( 0.000000000000000000, -1.000000000000000000, 0.000000000000000000 ) ) ;
#26324 = ORIENTED_EDGE ( 'NONE', *, *, #56242, .F. ) ;
#26325 = DIRECTION ( 'NONE',  ( 0.7671651518152962090, -0.6414496315691619044, -2.356647714346269254E-16 ) ) ;
#26326 = DIRECTION ( 'NONE',  ( 0.000000000000000000, 0.000000000000000000, 1.000000000000000000 ) ) ;
#26327 = VECTOR ( 'NONE', #22064, 1000.000000000000000 ) ;
#26328 = DIRECTION ( 'NONE',  ( -1.000000000000000000, 0.000000000000000000, 0.000000000000000000 ) ) ;
#26329 = DIRECTION ( 'NONE',  ( 0.000000000000000000, 0.000000000000000000, 1.000000000000000000 ) ) ;
#26330 = CARTESIAN_POINT ( 'NONE',  ( -7.450000000000001954, -7.249999999999998224, -12.50000000000000000 ) ) ;
#26331 = VECTOR ( 'NONE', #9974, 1000.000000000000000 ) ;
#26332 = ORIENTED_EDGE ( 'NONE', *, *, #50487, .F. ) ;
#26334 = VERTEX_POINT ( 'NONE', #50335 ) ;
#26333 = LINE ( 'NONE', #47891, #50910 ) ;
#26335 = CARTESIAN_POINT ( 'NONE',  ( 49.00000000000000000, 20.60000000000000142, -13.86939075806900057 ) ) ;
#26336 = CARTESIAN_POINT ( 'NONE',  ( 24.00000000000000000, -16.64230188589299786, 14.64519951917100116 ) ) ;
#26337 = DIRECTION ( 'NONE',  ( -1.000000000000000000, 0.000000000000000000, 0.000000000000000000 ) ) ;
#26338 = ORIENTED_EDGE ( 'NONE', *, *, #31964, .F. ) ;
#26339 = CIRCLE ( 'NONE', #68113, 0.2999999999998732569 ) ;
#26340 = DIRECTION ( 'NONE',  ( 0.7071067811865474617, -0.7071067811865474617, 0.000000000000000000 ) ) ;
#26341 = CARTESIAN_POINT ( 'NONE',  ( 29.25000000000000000, -5.200000000000001066, -26.25000000000000000 ) ) ;
#26342 = ORIENTED_EDGE ( 'NONE', *, *, #6872, .F. ) ;
#26343 = ORIENTED_EDGE ( 'NONE', *, *, #52442, .T. ) ;
#26344 = EDGE_CURVE ( 'NONE', #29352, #19794, #67662, .T. ) ;
#26345 = EDGE_LOOP ( 'NONE', ( #24266, #52365, #2566, #39552 ) ) ;
#26346 = LINE ( 'NONE', #3730, #55755 ) ;
#26347 = EDGE_CURVE ( 'NONE', #65501, #18999, #29122, .T. ) ;
#26348 = DIRECTION ( 'NONE',  ( -1.203165845134433242E-14, -1.000000000000000000, -1.836970198721014403E-16 ) ) ;
#26349 = DIRECTION ( 'NONE',  ( 1.000000000000000000, 0.000000000000000000, 0.000000000000000000 ) ) ;
#26350 = VECTOR ( 'NONE', #35445, 1000.000000000000000 ) ;
#26351 = VERTEX_POINT ( 'NONE', #51035 ) ;
#26352 = EDGE_LOOP ( 'NONE', ( #51379, #66670, #25041, #27841 ) ) ;
#26353 = EDGE_CURVE ( 'NONE', #41078, #41134, #34399, .T. ) ;
#26354 = AXIS2_PLACEMENT_3D ( 'NONE', #39936, #13075, #12719 ) ;
#26355 = DIRECTION ( 'NONE',  ( 0.000000000000000000, 0.000000000000000000, 1.000000000000000000 ) ) ;
#26356 = ORIENTED_EDGE ( 'NONE', *, *, #4892, .T. ) ;
#26357 = AXIS2_PLACEMENT_3D ( 'NONE', #49384, #947, #55704 ) ;
#26358 = AXIS2_PLACEMENT_3D ( 'NONE', #44588, #60859, #66173 ) ;
#26359 = EDGE_CURVE ( 'NONE', #13319, #8498, #55996, .T. ) ;
#26360 = ORIENTED_EDGE ( 'NONE', *, *, #64233, .F. ) ;
#26361 = ORIENTED_EDGE ( 'NONE', *, *, #65925, .T. ) ;
#26362 = ORIENTED_EDGE ( 'NONE', *, *, #46099, .T. ) ;
#26363 = DIRECTION ( 'NONE',  ( -1.000000000000000000, 0.000000000000000000, 0.000000000000000000 ) ) ;
#26364 = CIRCLE ( 'NONE', #4914, 1.000000000000000000 ) ;
#26365 = EDGE_CURVE ( 'NONE', #32920, #42042, #50679, .T. ) ;
#26367 = EDGE_LOOP ( 'NONE', ( #10190, #42276, #46999, #52330, #69294, #5229, #14001, #15660, #34242, #37708, #8516, #3646, #47354, #41369, #48272, #12147, #49715, #50862, #45440, #20341, #39812, #49862, #51836, #36562 ) ) ;
#26366 = CARTESIAN_POINT ( 'NONE',  ( 0.4999999999999964473, -0.4999999999999964473, 26.99999999999999645 ) ) ;
#26368 = DIRECTION ( 'NONE',  ( 1.000000000000000000, -0.000000000000000000, 0.000000000000000000 ) ) ;
#26369 = LINE ( 'NONE', #37680, #2378 ) ;
#26370 = DIRECTION ( 'NONE',  ( 1.836970198721029934E-16, 1.836970198721010706E-16, -1.000000000000000000 ) ) ;
#26371 = VERTEX_POINT ( 'NONE', #2251 ) ;
#26372 = EDGE_CURVE ( 'NONE', #65633, #40754, #6847, .T. ) ;
#26373 = ORIENTED_EDGE ( 'NONE', *, *, #36551, .T. ) ;
#26374 = EDGE_CURVE ( 'NONE', #21984, #7881, #42833, .T. ) ;
#26375 = VECTOR ( 'NONE', #21291, 1000.000000000000000 ) ;
#26376 = EDGE_CURVE ( 'NONE', #46858, #11718, #28415, .T. ) ;
#26377 = EDGE_CURVE ( 'NONE', #1302, #30390, #52421, .T. ) ;
#26378 = DIRECTION ( 'NONE',  ( 0.000000000000000000, 0.000000000000000000, -1.000000000000000000 ) ) ;
#26379 = SHAPE_REPRESENTATION ( 'SAWC-0630-60S_wagen', ( #45918 ), #34756 ) ;
#26380 = DIRECTION ( 'NONE',  ( -1.000000000000000000, 0.000000000000000000, 0.000000000000000000 ) ) ;
#26381 = VERTEX_POINT ( 'NONE', #12158 ) ;
#26382 = ADVANCED_FACE ( 'NONE', ( #59453 ), #48851, .F. ) ;
#26383 = CARTESIAN_POINT ( 'NONE',  ( -3.667976262117328190, -9.737023737882820384, 54.00000000000000711 ) ) ;
#26384 = DIRECTION ( 'NONE',  ( -0.000000000000000000, 3.673940397442059868E-16, -1.000000000000000000 ) ) ;
#26385 = CARTESIAN_POINT ( 'NONE',  ( 9.955011587777271131, 9.234937905883876752, 455.0000000000000568 ) ) ;
#26386 = ORIENTED_EDGE ( 'NONE', *, *, #12415, .T. ) ;
#26387 = FACE_OUTER_BOUND ( 'NONE', #27032, .T. ) ;
#26388 = CARTESIAN_POINT ( 'NONE',  ( 8.093267424590454340, 8.697938382363069820, 26.00000000000000711 ) ) ;
#26389 = CARTESIAN_POINT ( 'NONE',  ( -10.19191654964685156, -9.804883450353383267, 455.0000000000000568 ) ) ;
#26390 = DIRECTION ( 'NONE',  ( 1.000000000000000000, 1.301042606982605321E-16, 0.000000000000000000 ) ) ;
#26391 = PLANE ( 'NONE',  #45514 ) ;
#26392 = ORIENTED_EDGE ( 'NONE', *, *, #50225, .T. ) ;
#26393 = CARTESIAN_POINT ( 'NONE',  ( -8.821682069070780230, 2.355476262117184305, 54.00000000000000711 ) ) ;
#26394 = CARTESIAN_POINT ( 'NONE',  ( 11.90000000000000036, -0.1999999999911795112, 8.826273045769999343E-12 ) ) ;
#26395 = EDGE_CURVE ( 'NONE', #43734, #13690, #37200, .T. ) ;
#26396 = DIRECTION ( 'NONE',  ( 3.491481338843133355E-15, 1.000000000000000000, 1.836970198721029934E-16 ) ) ;
#26397 = ADVANCED_FACE ( 'NONE', ( #43875, #22664 ), #59796, .T. ) ;
#26398 = CIRCLE ( 'NONE', #35408, 0.3499999999999597877 ) ;
#26399 = CIRCLE ( 'NONE', #33144, 0.1749999999999998224 ) ;
#26400 = ORIENTED_EDGE ( 'NONE', *, *, #60739, .T. ) ;
#26401 = CARTESIAN_POINT ( 'NONE',  ( -8.916576262117260399, 8.916576262117214213, 54.00000000000000711 ) ) ;
#26402 = FACE_OUTER_BOUND ( 'NONE', #24104, .T. ) ;
#26403 = CARTESIAN_POINT ( 'NONE',  ( -22.14589803375000088, -17.50000000000000000, 21.50000000000000000 ) ) ;
#26404 = CARTESIAN_POINT ( 'NONE',  ( -15.50000000000000000, -0.2038245569916614930, 23.94337567297399971 ) ) ;
#26405 = VECTOR ( 'NONE', #11445, 1000.000000000000000 ) ;
#26406 = ORIENTED_EDGE ( 'NONE', *, *, #5539, .F. ) ;
#26407 = AXIS2_PLACEMENT_3D ( 'NONE', #61312, #28118, #49680 ) ;
#26408 = CARTESIAN_POINT ( 'NONE',  ( -7.793516549646712477, 11.11351654964660085, 195.0000000000000284 ) ) ;
#26409 = DIRECTION ( 'NONE',  ( -0.7071067811865474617, 0.7071067811865474617, -0.000000000000000000 ) ) ;
#26410 = CARTESIAN_POINT ( 'NONE',  ( 0.000000000000000000, 0.000000000000000000, 328.5239988703752942 ) ) ;
#26411 = DIRECTION ( 'NONE',  ( 0.000000000000000000, -1.000000000000000000, 0.000000000000000000 ) ) ;
#26412 = AXIS2_PLACEMENT_3D ( 'NONE', #5403, #54183, #59821 ) ;
#26414 = VECTOR ( 'NONE', #68273, 1000.000000000000000 ) ;
#26413 = FILL_AREA_STYLE_COLOUR ( '', #1458 ) ;
#26415 = CARTESIAN_POINT ( 'NONE',  ( 7.826483450353421745, 11.99351654964657499, 455.0000000000000568 ) ) ;
#26416 = ORIENTED_EDGE ( 'NONE', *, *, #65712, .T. ) ;
#26417 = ORIENTED_EDGE ( 'NONE', *, *, #30336, .F. ) ;
#26418 = CARTESIAN_POINT ( 'NONE',  ( -10.03972626211732688, -9.703773737882722017, 54.00000000000000711 ) ) ;
#26419 = FACE_OUTER_BOUND ( 'NONE', #45471, .T. ) ;
#26420 = ORIENTED_EDGE ( 'NONE', *, *, #33719, .T. ) ;
#26421 = CARTESIAN_POINT ( 'NONE',  ( -3.593516549646714520, -4.622483450353405132, 195.0000000000000284 ) ) ;
#26422 = EDGE_CURVE ( 'NONE', #17979, #26351, #32232, .T. ) ;
#26423 = LINE ( 'NONE', #58253, #58949 ) ;
#26424 = ORIENTED_EDGE ( 'NONE', *, *, #31898, .F. ) ;
#26425 = CARTESIAN_POINT ( 'NONE',  ( 8.250000000000005329, -7.249999999999998224, -26.00000000000001066 ) ) ;
#26426 = VERTEX_POINT ( 'NONE', #49190 ) ;
#26427 = VERTEX_POINT ( 'NONE', #37893 ) ;
#26428 = DIRECTION ( 'NONE',  ( -1.000000000000000000, 0.000000000000000000, 0.000000000000000000 ) ) ;
#26429 = VERTEX_POINT ( 'NONE', #16316 ) ;
#26430 = FACE_OUTER_BOUND ( 'NONE', #57549, .T. ) ;
#26431 = EDGE_CURVE ( 'NONE', #65042, #58346, #59102, .T. ) ;
#26432 = CARTESIAN_POINT ( 'NONE',  ( 39.90000000000000568, -0.2000000000000000111, 0.000000000000000000 ) ) ;
#26433 = CARTESIAN_POINT ( 'NONE',  ( -7.603567055985545942, 8.393516549646601987, 455.0000000000000568 ) ) ;
#26434 = LINE ( 'NONE', #42344, #17461 ) ;
#26435 = ORIENTED_EDGE ( 'NONE', *, *, #56282, .F. ) ;
#26436 = EDGE_LOOP ( 'NONE', ( #10481, #40534, #29807, #5581 ) ) ;
#26437 = ADVANCED_FACE ( 'NONE', ( #54159 ), #55185, .T. ) ;
#26438 = LINE ( 'NONE', #46590, #31274 ) ;
#26440 = LINE ( 'NONE', #41649, #32210 ) ;
#26439 = DIRECTION ( 'NONE',  ( -1.000000000000000000, 0.000000000000000000, 0.000000000000000000 ) ) ;
#26441 = ORIENTED_EDGE ( 'NONE', *, *, #10798, .F. ) ;
#26442 = EDGE_CURVE ( 'NONE', #49302, #9032, #58640, .T. ) ;
#26443 = AXIS2_PLACEMENT_3D ( 'NONE', #6316, #43098, #32839 ) ;
#26444 = VERTEX_POINT ( 'NONE', #65453 ) ;
#26445 = EDGE_CURVE ( 'NONE', #15780, #45972, #48498, .T. ) ;
#26447 = ORIENTED_EDGE ( 'NONE', *, *, #65869, .T. ) ;
#26446 = ITEM_DEFINED_TRANSFORMATION ( 'NONE', 'NONE', #31316,  #45918 ) ;
#26448 = EDGE_CURVE ( 'NONE', #46983, #40696, #12027, .T. ) ;
#26449 = EDGE_CURVE ( 'NONE', #64879, #32175, #34877, .T. ) ;
#26450 = PLANE ( 'NONE',  #8507 ) ;
#26452 = VERTEX_POINT ( 'NONE', #32925 ) ;
#26451 = CARTESIAN_POINT ( 'NONE',  ( -2.893516549646673930, 11.11351654964657598, 455.0000000000000568 ) ) ;
#26453 = LINE ( 'NONE', #43053, #23209 ) ;
#26454 = VECTOR ( 'NONE', #60248, 1000.000000000000000 ) ;
#26455 = CARTESIAN_POINT ( 'NONE',  ( -17.00000000000000000, -15.50000000000000000, -14.50000000000000000 ) ) ;
#26456 = EDGE_LOOP ( 'NONE', ( #48195, #56555, #7443, #14779 ) ) ;
#26457 = VERTEX_POINT ( 'NONE', #1429 ) ;
#26458 = VECTOR ( 'NONE', #36432, 1000.000000000000000 ) ;
#26459 = AXIS2_PLACEMENT_3D ( 'NONE', #20234, #19886, #25909 ) ;
#26460 = AXIS2_PLACEMENT_3D ( 'NONE', #60889, #7500, #50288 ) ;
#26461 = CARTESIAN_POINT ( 'NONE',  ( 41.09999999999999432, -0.2000000000000000111, 0.000000000000000000 ) ) ;
#26462 = ORIENTED_EDGE ( 'NONE', *, *, #14477, .F. ) ;
#26463 = DIRECTION ( 'NONE',  ( 0.000000000000000000, 0.000000000000000000, 1.000000000000000000 ) ) ;
#26464 = CARTESIAN_POINT ( 'NONE',  ( 10.90000000000000036, -0.2000000000089119934, 8.909539772616881237E-12 ) ) ;
#26465 = AXIS2_PLACEMENT_3D ( 'NONE', #61180, #12738, #61896 ) ;
#26466 = DIRECTION ( 'NONE',  ( -0.000000000000000000, 3.673940397442059868E-16, -1.000000000000000000 ) ) ;
#26467 = ORIENTED_EDGE ( 'NONE', *, *, #53453, .T. ) ;
#26468 = CONICAL_SURFACE ( 'NONE', #65965, 1732.050807568785558, 1.047197551196574761 ) ;
#26469 = DIRECTION ( 'NONE',  ( 1.836970198721029934E-16, 1.836970198721010706E-16, -1.000000000000000000 ) ) ;
#26470 = AXIS2_PLACEMENT_3D ( 'NONE', #39994, #18430, #61566 ) ;
#26471 = ORIENTED_EDGE ( 'NONE', *, *, #67229, .F. ) ;
#26472 = ORIENTED_EDGE ( 'NONE', *, *, #12125, .F. ) ;
#26473 = VECTOR ( 'NONE', #24066, 1000.000000000000000 ) ;
#26474 = DIRECTION ( 'NONE',  ( 0.000000000000000000, 0.000000000000000000, 1.000000000000000000 ) ) ;
#26475 = CARTESIAN_POINT ( 'NONE',  ( 7.450000000000006395, 7.250000000000000888, -12.50000000000000000 ) ) ;
#26476 = DIRECTION ( 'NONE',  ( -0.000000000000000000, 1.000000000000000000, -0.000000000000000000 ) ) ;
#26477 = DIRECTION ( 'NONE',  ( 0.000000000000000000, 0.000000000000000000, 1.000000000000000000 ) ) ;
#26478 = DIRECTION ( 'NONE',  ( 0.000000000000000000, -1.000000000000000000, 0.000000000000000000 ) ) ;
#26479 = VERTEX_POINT ( 'NONE', #43526 ) ;
#26480 = LINE ( 'NONE', #65007, #50448 ) ;
#26481 = DIRECTION ( 'NONE',  ( -1.000000000000000000, 1.047444401652940007E-14, 0.000000000000000000 ) ) ;
#26482 = DIRECTION ( 'NONE',  ( 0.000000000000000000, 1.000000000000000000, 0.000000000000000000 ) ) ;
#26484 = VERTEX_POINT ( 'NONE', #16679 ) ;
#26483 = DIRECTION ( 'NONE',  ( 0.000000000000000000, 0.000000000000000000, 1.000000000000000000 ) ) ;
#26485 = EDGE_CURVE ( 'NONE', #19647, #30244, #8955, .T. ) ;
#26486 = FACE_OUTER_BOUND ( 'NONE', #57847, .T. ) ;
#26487 = EDGE_CURVE ( 'NONE', #62127, #17538, #49874, .T. ) ;
#26488 = CARTESIAN_POINT ( 'NONE',  ( 7.250000000000005329, -8.249999999999998224, -26.00000000000001066 ) ) ;
#26489 = CARTESIAN_POINT ( 'NONE',  ( 0.000000000000000000, -8.249999999999998224, -19.00000000000000000 ) ) ;
#26490 = VERTEX_POINT ( 'NONE', #15973 ) ;
#26491 = CARTESIAN_POINT ( 'NONE',  ( 23.48000000000000043, -15.50000000000000000, 26.00000000000000355 ) ) ;
#26492 = PLANE ( 'NONE',  #19306 ) ;
#26493 = CIRCLE ( 'NONE', #25373, 5.000000000000004441 ) ;
#26494 = ORIENTED_EDGE ( 'NONE', *, *, #24403, .T. ) ;
#26495 = DIRECTION ( 'NONE',  ( 1.000000000000000000, -5.981805089575194965E-17, 0.000000000000000000 ) ) ;
#26496 = CARTESIAN_POINT ( 'NONE',  ( 40.90000000000000568, -16.96999999999999886, -21.00000000000000000 ) ) ;
#26497 = CYLINDRICAL_SURFACE ( 'NONE', #11781, 24.99999999998784972 ) ;
#26498 = DIRECTION ( 'NONE',  ( 1.836970198721029934E-16, 1.836970198721010706E-16, -1.000000000000000000 ) ) ;
#26499 = CARTESIAN_POINT ( 'NONE',  ( -10.19191654964681781, -11.08848345035329963, 195.0000000000000284 ) ) ;
#26500 = VECTOR ( 'NONE', #47620, 1000.000000000000000 ) ;
#26501 = CIRCLE ( 'NONE', #42284, 1.000000000000000000 ) ;
#26502 = VERTEX_POINT ( 'NONE', #38582 ) ;
#26503 = ORIENTED_EDGE ( 'NONE', *, *, #25843, .T. ) ;
#26504 = DIRECTION ( 'NONE',  ( -1.836970198721029934E-16, 1.836970198721036344E-16, -1.000000000000000000 ) ) ;
#26505 = ORIENTED_EDGE ( 'NONE', *, *, #55593, .F. ) ;
#26506 = ORIENTED_EDGE ( 'NONE', *, *, #4674, .T. ) ;
#26507 = DIRECTION ( 'NONE',  ( 0.000000000000000000, 0.000000000000000000, -1.000000000000000000 ) ) ;
#26508 = VECTOR ( 'NONE', #24049, 1000.000000000000000 ) ;
#26509 = AXIS2_PLACEMENT_3D ( 'NONE', #31702, #47601, #53272 ) ;
#26510 = LINE ( 'NONE', #52698, #28754 ) ;
#26511 = AXIS2_PLACEMENT_3D ( 'NONE', #26093, #10168, #69216 ) ;
#26512 = CARTESIAN_POINT ( 'NONE',  ( 7.000000000000000000, -20.40000000000000213, -17.60000000000000142 ) ) ;
#26513 = VERTEX_POINT ( 'NONE', #42835 ) ;
#26514 = ORIENTED_EDGE ( 'NONE', *, *, #36551, .F. ) ;
#26515 = CARTESIAN_POINT ( 'NONE',  ( 3.552713678800500929E-15, -17.79289321881343255, 20.50000000000000355 ) ) ;
#26516 = ORIENTED_EDGE ( 'NONE', *, *, #44313, .T. ) ;
#26517 = ORIENTED_EDGE ( 'NONE', *, *, #66136, .T. ) ;
#26518 = ADVANCED_FACE ( 'NONE', ( #38916 ), #27618, .T. ) ;
#26519 = CARTESIAN_POINT ( 'NONE',  ( 15.08757311576526128, -0.3152598339554911200, -23.70526090034004341 ) ) ;
#26520 = DIRECTION ( 'NONE',  ( 0.000000000000000000, -0.7071067811865474617, -0.7071067811865474617 ) ) ;
#26521 = VECTOR ( 'NONE', #60370, 1000.000000000000000 ) ;
#26522 = CARTESIAN_POINT ( 'NONE',  ( -11.00000000000000000, -16.64230188589299786, -14.64519951917100116 ) ) ;
#26523 = AXIS2_PLACEMENT_3D ( 'NONE', #17401, #50276, #38976 ) ;
#26524 = VERTEX_POINT ( 'NONE', #33274 ) ;
#26525 = AXIS2_PLACEMENT_3D ( 'NONE', #35727, #25836, #47738 ) ;
#26526 = CARTESIAN_POINT ( 'NONE',  ( 283.0000000000000568, -23.65000000000000568, 12.40000000000000213 ) ) ;
#26527 = EDGE_CURVE ( 'NONE', #19106, #46180, #54843, .T. ) ;
#26528 = DIRECTION ( 'NONE',  ( 1.000000000000000000, 0.000000000000000000, 0.000000000000000000 ) ) ;
#26529 = VERTEX_POINT ( 'NONE', #60479 ) ;
#26531 = ORIENTED_EDGE ( 'NONE', *, *, #43993, .F. ) ;
#26530 = LINE ( 'NONE', #48098, #34221 ) ;
#26532 = ORIENTED_EDGE ( 'NONE', *, *, #35131, .F. ) ;
#26533 = EDGE_CURVE ( 'NONE', #32262, #65403, #35199, .T. ) ;
#26534 = EDGE_CURVE ( 'NONE', #8859, #40018, #57507, .T. ) ;
#26535 = DIRECTION ( 'NONE',  ( -1.000000000000000000, 0.000000000000000000, 0.000000000000000000 ) ) ;
#26536 = CARTESIAN_POINT ( 'NONE',  ( 14.75000000000000178, -42.25000000000000000, -26.75000000000000000 ) ) ;
#26537 = EDGE_CURVE ( 'NONE', #53797, #6660, #51486, .T. ) ;
#26538 = ORIENTED_EDGE ( 'NONE', *, *, #26774, .F. ) ;
#26539 = VECTOR ( 'NONE', #44480, 1000.000000000000000 ) ;
#26540 = DIRECTION ( 'NONE',  ( -1.000000000000000000, 0.000000000000000000, 0.000000000000000000 ) ) ;
#26541 = DIRECTION ( 'NONE',  ( -0.000000000000000000, -0.000000000000000000, -1.000000000000000000 ) ) ;
#26542 = VECTOR ( 'NONE', #56316, 1000.000000000000000 ) ;
#26543 = ORIENTED_EDGE ( 'NONE', *, *, #53763, .T. ) ;
#26544 = ORIENTED_EDGE ( 'NONE', *, *, #69100, .T. ) ;
#26545 = DIRECTION ( 'NONE',  ( 1.047444401652939849E-14, 1.000000000000000000, 0.000000000000000000 ) ) ;
#26546 = DIRECTION ( 'NONE',  ( 0.000000000000000000, 0.000000000000000000, 1.000000000000000000 ) ) ;
#26547 = LINE ( 'NONE', #48118, #32787 ) ;
#26548 = EDGE_LOOP ( 'NONE', ( #22657, #38757, #48434, #63914 ) ) ;
#26549 = AXIS2_PLACEMENT_3D ( 'NONE', #7409, #12354, #27957 ) ;
#26550 = AXIS2_PLACEMENT_3D ( 'NONE', #25844, #40692, #67918 ) ;
#26551 = CYLINDRICAL_SURFACE ( 'NONE', #1846, 0.8099999999999999423 ) ;
#26552 = DIRECTION ( 'NONE',  ( 0.000000000000000000, 0.000000000000000000, 1.000000000000000000 ) ) ;
#26554 = ORIENTED_EDGE ( 'NONE', *, *, #40562, .F. ) ;
#26553 = DIRECTION ( 'NONE',  ( -0.000000000000000000, -0.000000000000000000, -1.000000000000000000 ) ) ;
#26556 = ORIENTED_EDGE ( 'NONE', *, *, #54668, .F. ) ;
#26555 = CARTESIAN_POINT ( 'NONE',  ( 9.562023737882805463, 8.130476262117184660, 54.00000000000000711 ) ) ;
#26557 = CARTESIAN_POINT ( 'NONE',  ( 6.749999999999996447, -7.348062532928000934, -5.000000000000000000 ) ) ;
#26558 = AXIS2_PLACEMENT_3D ( 'NONE', #39881, #19034, #68168 ) ;
#26559 = PRESENTATION_LAYER_ASSIGNMENT (  '', '', ( #57026 ) ) ;
#26560 = DIRECTION ( 'NONE',  ( -1.000000000000000000, 0.000000000000000000, 0.000000000000000000 ) ) ;
#26561 = PLANE ( 'NONE',  #44807 ) ;
#26562 = DIRECTION ( 'NONE',  ( 3.540251991789405856E-15, 1.000000000000000000, 0.000000000000000000 ) ) ;
#26563 = LINE ( 'NONE', #48136, #62171 ) ;
#26564 = VECTOR ( 'NONE', #43910, 1000.000000000000000 ) ;
#26565 = LINE ( 'NONE', #35764, #55230 ) ;
#26566 = ORIENTED_EDGE ( 'NONE', *, *, #59158, .F. ) ;
#26567 = CARTESIAN_POINT ( 'NONE',  ( 275.0000000000000000, -38.65000000000095781, -13.20000000000094253 ) ) ;
#26569 = ORIENTED_EDGE ( 'NONE', *, *, #8296, .T. ) ;
#26568 = CARTESIAN_POINT ( 'NONE',  ( 290.0000000000000000, 0.000000000000000000, 0.000000000000000000 ) ) ;
#26570 = DIRECTION ( 'NONE',  ( 0.000000000000000000, -0.000000000000000000, 1.000000000000000000 ) ) ;
#26571 = CONICAL_SURFACE ( 'NONE', #6270, 4.000000000000000000, 0.7853981633974476129 ) ;
#26572 = DIRECTION ( 'NONE',  ( 0.000000000000000000, 1.000000000000000000, 0.000000000000000000 ) ) ;
#26573 = EDGE_CURVE ( 'NONE', #38860, #19920, #34854, .T. ) ;
#26574 = CARTESIAN_POINT ( 'NONE',  ( -10.30047626211728762, -6.657023737882746595, 26.00000000000000000 ) ) ;
#26575 = EDGE_CURVE ( 'NONE', #38612, #46075, #33816, .T. ) ;
#26576 = EDGE_CURVE ( 'NONE', #66290, #14513, #12934, .T. ) ;
#26577 = ORIENTED_EDGE ( 'NONE', *, *, #32361, .T. ) ;
#26578 = CARTESIAN_POINT ( 'NONE',  ( -7.250000000000000888, 7.450000000000003730, -12.00000000000000000 ) ) ;
#26579 = DIRECTION ( 'NONE',  ( -0.000000000000000000, -0.000000000000000000, -1.000000000000000000 ) ) ;
#26581 = ORIENTED_EDGE ( 'NONE', *, *, #51785, .T. ) ;
#26580 = EDGE_CURVE ( 'NONE', #2518, #47170, #18960, .T. ) ;
#26582 = CARTESIAN_POINT ( 'NONE',  ( -23.48000000000000043, -17.50000000000000000, 26.00000000000000355 ) ) ;
#26583 = DIRECTION ( 'NONE',  ( 0.000000000000000000, 0.000000000000000000, 1.000000000000000000 ) ) ;
#26584 = ORIENTED_EDGE ( 'NONE', *, *, #47002, .T. ) ;
#26585 = DIRECTION ( 'NONE',  ( -0.000000000000000000, 3.673940397442059868E-16, -1.000000000000000000 ) ) ;
#26586 = ORIENTED_EDGE ( 'NONE', *, *, #25077, .F. ) ;
#26587 = ORIENTED_EDGE ( 'NONE', *, *, #62944, .T. ) ;
#26588 = DIRECTION ( 'NONE',  ( 0.000000000000000000, 0.000000000000000000, -1.000000000000000000 ) ) ;
#26589 = DIRECTION ( 'NONE',  ( 1.000000000000000000, -0.000000000000000000, -0.000000000000000000 ) ) ;
#26590 = VECTOR ( 'NONE', #9104, 1000.000000000000000 ) ;
#26591 = FACE_OUTER_BOUND ( 'NONE', #24542, .T. ) ;
#26592 = AXIS2_PLACEMENT_3D ( 'NONE', #48062, #32503, #53725 ) ;
#26593 = DIRECTION ( 'NONE',  ( 0.000000000000000000, 3.673940397442059868E-16, -1.000000000000000000 ) ) ;
#26594 = EDGE_LOOP ( 'NONE', ( #46152, #5536, #3917, #63252 ) ) ;
#26595 = VERTEX_POINT ( 'NONE', #3056 ) ;
#26597 = VERTEX_POINT ( 'NONE', #55402 ) ;
#26596 = CARTESIAN_POINT ( 'NONE',  ( 275.0000000000000000, -21.00000000000000000, -17.50000000000000000 ) ) ;
#26598 = ORIENTED_EDGE ( 'NONE', *, *, #12088, .F. ) ;
#26599 = VECTOR ( 'NONE', #44684, 1000.000000000000000 ) ;
#26600 = VECTOR ( 'NONE', #62204, 1000.000000000000000 ) ;
#26601 = AXIS2_PLACEMENT_3D ( 'NONE', #68366, #30531, #47833 ) ;
#26602 = FACE_OUTER_BOUND ( 'NONE', #41111, .T. ) ;
#26603 = DIRECTION ( 'NONE',  ( -1.000000000000000000, 0.000000000000000000, 0.000000000000000000 ) ) ;
#26604 = DIRECTION ( 'NONE',  ( -1.000000000000000000, 0.000000000000000000, 0.000000000000000000 ) ) ;
#26605 = DIRECTION ( 'NONE',  ( 0.000000000000000000, 1.000000000000000000, 0.000000000000000000 ) ) ;
#26606 = CIRCLE ( 'NONE', #39008, 0.4000000000000609179 ) ;
#26607 = AXIS2_PLACEMENT_3D ( 'NONE', #5826, #49311, #889 ) ;
#26609 = CARTESIAN_POINT ( 'NONE',  ( -11.00000000000000000, -11.50000000000000000, 19.00000000000000000 ) ) ;
#26608 = DIRECTION ( 'NONE',  ( 1.000000000000000000, -0.000000000000000000, 0.000000000000000000 ) ) ;
#26610 = ORIENTED_EDGE ( 'NONE', *, *, #30821, .F. ) ;
#26611 = ORIENTED_EDGE ( 'NONE', *, *, #47923, .T. ) ;
#26612 = ORIENTED_EDGE ( 'NONE', *, *, #59099, .T. ) ;
#26613 = ORIENTED_EDGE ( 'NONE', *, *, #64762, .T. ) ;
#26614 = VECTOR ( 'NONE', #35202, 1000.000000000000000 ) ;
#26615 = DIRECTION ( 'NONE',  ( 0.000000000000000000, 1.000000000000000000, 0.000000000000000000 ) ) ;
#26616 = FACE_OUTER_BOUND ( 'NONE', #29593, .T. ) ;
#26617 = EDGE_CURVE ( 'NONE', #31212, #47075, #60699, .T. ) ;
#26618 = CARTESIAN_POINT ( 'NONE',  ( -5.848397904920865642, 47.95351654964650834, 10.30076836395856077 ) ) ;
#26619 = AXIS2_PLACEMENT_3D ( 'NONE', #50300, #17428, #28053 ) ;
#26620 = DIRECTION ( 'NONE',  ( 8.659560562354963673E-17, 0.7071067811865450192, -0.7071067811865500152 ) ) ;
#26621 = EDGE_CURVE ( 'NONE', #21581, #44389, #6945, .T. ) ;
#26622 = ORIENTED_EDGE ( 'NONE', *, *, #7425, .T. ) ;
#26623 = VERTEX_POINT ( 'NONE', #19300 ) ;
#26624 = EDGE_CURVE ( 'NONE', #51641, #53480, #29908, .T. ) ;
#26625 = ORIENTED_EDGE ( 'NONE', *, *, #16689, .F. ) ;
#26626 = AXIS2_PLACEMENT_3D ( 'NONE', #69000, #27602, #5000 ) ;
#26627 = CARTESIAN_POINT ( 'NONE',  ( -6.500000000000002665, 6.500000000000002665, -1.000000000000000000 ) ) ;
#26628 = ORIENTED_EDGE ( 'NONE', *, *, #52256, .F. ) ;
#26629 = CARTESIAN_POINT ( 'NONE',  ( 4.747751991980663000, 5.380658396643107189, 455.0000000000000568 ) ) ;
#26630 = ADVANCED_FACE ( 'NONE', ( #62076 ), #46173, .T. ) ;
#26631 = LINE ( 'NONE', #48200, #1798 ) ;
#26632 = ORIENTED_EDGE ( 'NONE', *, *, #12602, .T. ) ;
#26633 = ORIENTED_EDGE ( 'NONE', *, *, #25037, .F. ) ;
#26634 = LINE ( 'NONE', #47836, #48615 ) ;
#26635 = EDGE_CURVE ( 'NONE', #21397, #46652, #20937, .T. ) ;
#26636 = LINE ( 'NONE', #69781, #40146 ) ;
#26638 = EDGE_LOOP ( 'NONE', ( #7730, #8133, #33415, #35261 ) ) ;
#26637 = EDGE_CURVE ( 'NONE', #28943, #37001, #56780, .T. ) ;
#26639 = CARTESIAN_POINT ( 'NONE',  ( -7.744988412222854279, 8.452095193409293827, 455.0000000000000568 ) ) ;
#26640 = VECTOR ( 'NONE', #57072, 1000.000000000000000 ) ;
#26642 = ORIENTED_EDGE ( 'NONE', *, *, #56804, .T. ) ;
#26641 = LINE ( 'NONE', #48212, #38550 ) ;
#26643 = ORIENTED_EDGE ( 'NONE', *, *, #49864, .F. ) ;
#26644 = LINE ( 'NONE', #27345, #49127 ) ;
#26645 = CARTESIAN_POINT ( 'NONE',  ( -8.393516549646712122, 4.383466043307770121, 455.0000000000000568 ) ) ;
#26646 = AXIS2_PLACEMENT_3D ( 'NONE', #62054, #2659, #41551 ) ;
#26647 = PLANE ( 'NONE',  #31796 ) ;
#26648 = DIRECTION ( 'NONE',  ( 1.000000000000000000, -0.000000000000000000, 0.000000000000000000 ) ) ;
#26649 = DIRECTION ( 'NONE',  ( 0.000000000000000000, -0.000000000000000000, 1.000000000000000000 ) ) ;
#26650 = VECTOR ( 'NONE', #33097, 1000.000000000000000 ) ;
#26651 = VERTEX_POINT ( 'NONE', #39468 ) ;
#26652 = LINE ( 'NONE', #20636, #30377 ) ;
#26653 = VERTEX_POINT ( 'NONE', #67038 ) ;
#26654 = AXIS2_PLACEMENT_3D ( 'NONE', #46790, #62702, #14279 ) ;
#26655 = CIRCLE ( 'NONE', #66154, 7.300000000000000711 ) ;
#26657 = CARTESIAN_POINT ( 'NONE',  ( 72.77321854994619343, 47.95351654967443977, 29.00000000000000000 ) ) ;
#26656 = CIRCLE ( 'NONE', #11930, 0.1999999999999987899 ) ;
#26658 = LINE ( 'NONE', #57775, #28934 ) ;
#26659 = FACE_OUTER_BOUND ( 'NONE', #37873, .T. ) ;
#26660 = DIRECTION ( 'NONE',  ( 0.000000000000000000, 0.000000000000000000, 1.000000000000000000 ) ) ;
#26661 = AXIS2_PLACEMENT_3D ( 'NONE', #27767, #33064, #54647 ) ;
#26662 = CIRCLE ( 'NONE', #720, 3.500000000000114131 ) ;
#26663 =( GEOMETRIC_REPRESENTATION_CONTEXT ( 3 ) GLOBAL_UNCERTAINTY_ASSIGNED_CONTEXT ( ( #62790 ) ) GLOBAL_UNIT_ASSIGNED_CONTEXT ( ( #54529, #12396, #55554 ) ) REPRESENTATION_CONTEXT ( 'NONE', 'WORKASPACE' ) );
#26664 = DIRECTION ( 'NONE',  ( 1.000000000000000000, 2.135044278125301343E-15, -0.000000000000000000 ) ) ;
#26665 = EDGE_LOOP ( 'NONE', ( #53354, #22704, #28532, #61256 ) ) ;
#26666 = VECTOR ( 'NONE', #64899, 1000.000000000000000 ) ;
#26667 = CARTESIAN_POINT ( 'NONE',  ( 7.000000000000000000, -42.50000000000000000, 7.500000000000000000 ) ) ;
#26668 = VECTOR ( 'NONE', #61589, 1000.000000000000000 ) ;
#26669 = VERTEX_POINT ( 'NONE', #8333 ) ;
#26670 = CARTESIAN_POINT ( 'NONE',  ( 4.740315990920172418, 7.798499376343941414, 455.0000000000000568 ) ) ;
#26671 = CARTESIAN_POINT ( 'NONE',  ( 83.77321854994620765, 47.95351654967443977, 15.00000000000000000 ) ) ;
#26672 = DIRECTION ( 'NONE',  ( 0.7671651518153173033, 0.6414496315691367023, 2.587583378555108576E-16 ) ) ;
#26673 = ORIENTED_EDGE ( 'NONE', *, *, #9239, .T. ) ;
#26674 = LINE ( 'NONE', #53903, #44839 ) ;
#26675 = CARTESIAN_POINT ( 'NONE',  ( 14.50000000000000000, -42.50000000000000000, 26.50000000000000000 ) ) ;
#26677 = EDGE_LOOP ( 'NONE', ( #43963, #55628 ) ) ;
#26676 = EDGE_CURVE ( 'NONE', #30300, #23148, #34156, .T. ) ;
#26678 = DIRECTION ( 'NONE',  ( 0.6414496315691619044, 0.7671651518152962090, 0.000000000000000000 ) ) ;
#26679 = CARTESIAN_POINT ( 'NONE',  ( 20.90000000000000213, -0.2000000000089119934, -8.913009219568841313E-12 ) ) ;
#26680 = PRESENTATION_STYLE_ASSIGNMENT (( #64178 ) ) ;
#26681 = ADVANCED_FACE ( 'NONE', ( #40164 ), #7286, .T. ) ;
#26682 = DIRECTION ( 'NONE',  ( 1.836970198721029934E-16, -1.836970198721036344E-16, 1.000000000000000000 ) ) ;
#26683 = VERTEX_POINT ( 'NONE', #28855 ) ;
#26685 = EDGE_LOOP ( 'NONE', ( #44640, #39441, #25558, #61370 ) ) ;
#26684 = FACE_BOUND ( 'NONE', #16706, .T. ) ;
#26686 = LINE ( 'NONE', #52155, #55353 ) ;
#26687 = CARTESIAN_POINT ( 'NONE',  ( 5.668387132715918320, -8.406483450353487541, 455.0000000000000568 ) ) ;
#26688 = DIRECTION ( 'NONE',  ( 0.000000000000000000, 0.000000000000000000, -1.000000000000000000 ) ) ;
#26689 = ORIENTED_EDGE ( 'NONE', *, *, #64567, .F. ) ;
#26690 = AXIS2_PLACEMENT_3D ( 'NONE', #24111, #18445, #29762 ) ;
#26691 = DIRECTION ( 'NONE',  ( 0.000000000000000000, 3.673940397442059868E-16, -1.000000000000000000 ) ) ;
#26692 = VECTOR ( 'NONE', #1531, 1000.000000000000000 ) ;
#26693 = ORIENTED_EDGE ( 'NONE', *, *, #31074, .F. ) ;
#26694 = ORIENTED_EDGE ( 'NONE', *, *, #30919, .T. ) ;
#26695 = ADVANCED_FACE ( 'NONE', ( #29558 ), #2686, .F. ) ;
#26696 = AXIS2_PLACEMENT_3D ( 'NONE', #9594, #36458, #4988 ) ;
#26697 = VECTOR ( 'NONE', #63424, 1000.000000000000114 ) ;
#26698 = VERTEX_POINT ( 'NONE', #67409 ) ;
#26699 = CARTESIAN_POINT ( 'NONE',  ( 29.50000000000000355, -12.00000000000000000, -10.52786404500095863 ) ) ;
#26700 = LINE ( 'NONE', #33393, #34835 ) ;
#26701 = CARTESIAN_POINT ( 'NONE',  ( 11.08848345035337424, 11.47551654964657608, 195.0000000000000284 ) ) ;
#26702 = CIRCLE ( 'NONE', #14283, 1.929199999999997139 ) ;
#26703 = AXIS2_PLACEMENT_3D ( 'NONE', #32924, #47789, #26938 ) ;
#26704 = AXIS2_PLACEMENT_3D ( 'NONE', #50866, #34945, #39222 ) ;
#26705 = EDGE_CURVE ( 'NONE', #11793, #5559, #33355, .T. ) ;
#26706 = VERTEX_POINT ( 'NONE', #8698 ) ;
#26707 = VERTEX_POINT ( 'NONE', #25317 ) ;
#26708 = CARTESIAN_POINT ( 'NONE',  ( -10.91351654964670637, 2.693516549646604030, 455.0000000000000568 ) ) ;
#26709 = AXIS2_PLACEMENT_3D ( 'NONE', #46111, #40455, #62013 ) ;
#26710 = AXIS2_PLACEMENT_3D ( 'NONE', #67114, #8054, #56849 ) ;
#26711 = ORIENTED_EDGE ( 'NONE', *, *, #37687, .F. ) ;
#26712 = ORIENTED_EDGE ( 'NONE', *, *, #23747, .F. ) ;
#26713 = VERTEX_POINT ( 'NONE', #57484 ) ;
#26714 = EDGE_LOOP ( 'NONE', ( #45145, #5733, #15752, #51147 ) ) ;
#26715 = VECTOR ( 'NONE', #10283, 1000.000000000000000 ) ;
#26716 = LINE ( 'NONE', #64549, #22584 ) ;
#26717 = UNCERTAINTY_MEASURE_WITH_UNIT (LENGTH_MEASURE( 1.000000000000000082E-05 ), #40769, 'distance_accuracy_value', 'NONE');
#26718 = EDGE_CURVE ( 'NONE', #32701, #60888, #18646, .T. ) ;
#26720 = VERTEX_POINT ( 'NONE', #35924 ) ;
#26719 = DIRECTION ( 'NONE',  ( -1.000000000000000000, 0.000000000000000000, 0.000000000000000000 ) ) ;
#26721 = EDGE_CURVE ( 'NONE', #67348, #16165, #60443, .T. ) ;
#26722 = DIRECTION ( 'NONE',  ( -1.000000000000000000, 1.047444401652940007E-14, -1.836970198721010952E-16 ) ) ;
#26723 = PRODUCT ( 'Part1', 'Part1', '', ( #57566 ) ) ;
#26724 = VECTOR ( 'NONE', #3787, 1000.000000000000000 ) ;
#26725 = DIRECTION ( 'NONE',  ( -1.000000000000000000, 0.000000000000000000, 0.000000000000000000 ) ) ;
#26726 = DIRECTION ( 'NONE',  ( 0.000000000000000000, -1.000000000000000000, 1.540434446669787085E-12 ) ) ;
#26727 = ORIENTED_EDGE ( 'NONE', *, *, #15116, .T. ) ;
#26728 = EDGE_CURVE ( 'NONE', #10205, #18896, #4801, .T. ) ;
#26729 = DIRECTION ( 'NONE',  ( 1.836970198721029934E-16, -1.836970198721036344E-16, 1.000000000000000000 ) ) ;
#26730 = CARTESIAN_POINT ( 'NONE',  ( 11.08848345035337069, 10.19191654964660998, 195.0000000000000284 ) ) ;
#26731 = ORIENTED_EDGE ( 'NONE', *, *, #55202, .T. ) ;
#26732 = CARTESIAN_POINT ( 'NONE',  ( -7.415254214038356828, -3.606483450353401121, 455.0000000000000568 ) ) ;
#26733 = DIRECTION ( 'NONE',  ( -8.339399738404101090E-15, -1.000000000000000000, -1.836970198721025990E-16 ) ) ;
#26734 = LINE ( 'NONE', #37346, #40353 ) ;
#26735 = CIRCLE ( 'NONE', #16598, 0.1749999999999989342 ) ;
#26736 = EDGE_LOOP ( 'NONE', ( #67587, #21226, #34828, #8410 ) ) ;
#26737 = DIRECTION ( 'NONE',  ( 0.6785983445458467767, 0.2810846377148228381, 0.6785983445458462215 ) ) ;
#26738 = CARTESIAN_POINT ( 'NONE',  ( 14.74999999999998934, -0.2500000000000142109, 26.75000000000000711 ) ) ;
#26739 = CIRCLE ( 'NONE', #36952, 0.1999999999999992339 ) ;
#26740 = LINE ( 'NONE', #38057, #4324 ) ;
#26741 = EDGE_CURVE ( 'NONE', #1362, #27098, #30969, .T. ) ;
#26742 = AXIS2_PLACEMENT_3D ( 'NONE', #43852, #7393, #11321 ) ;
#26743 = CARTESIAN_POINT ( 'NONE',  ( 9.737023737882816832, -3.682023737882817116, 26.00000000000000711 ) ) ;
#26744 = DIRECTION ( 'NONE',  ( 1.000000000000000000, -0.000000000000000000, 0.000000000000000000 ) ) ;
#26745 = CARTESIAN_POINT ( 'NONE',  ( 10.50702373788281641, 9.781776262117171328, 54.00000000000000711 ) ) ;
#26746 = LINE ( 'NONE', #69528, #57036 ) ;
#26747 = EDGE_CURVE ( 'NONE', #3920, #25334, #19817, .T. ) ;
#26748 = CARTESIAN_POINT ( 'NONE',  ( 7.450000000000006395, 7.250000000000000888, -14.00000000000000000 ) ) ;
#26749 = AXIS2_PLACEMENT_3D ( 'NONE', #5534, #48669, #41963 ) ;
#26750 = AXIS2_PLACEMENT_3D ( 'NONE', #58723, #22287, #43837 ) ;
#26751 = ORIENTED_EDGE ( 'NONE', *, *, #17983, .T. ) ;
#26752 = CARTESIAN_POINT ( 'NONE',  ( -4.188533722949335569, 4.727349090213398775, 195.0000000000000284 ) ) ;
#26753 = LINE ( 'NONE', #32411, #2563 ) ;
#26754 = EDGE_CURVE ( 'NONE', #17980, #39718, #20358, .T. ) ;
#26755 = VECTOR ( 'NONE', #33590, 1000.000000000000000 ) ;
#26756 = CARTESIAN_POINT ( 'NONE',  ( 7.250000000000005329, 8.250000000000001776, -26.00000000000001066 ) ) ;
#26757 = AXIS2_PLACEMENT_3D ( 'NONE', #41914, #19636, #15048 ) ;
#26758 = LINE ( 'NONE', #25355, #39772 ) ;
#26759 = EDGE_LOOP ( 'NONE', ( #47413, #61477, #64803, #31785 ) ) ;
#26760 = DIRECTION ( 'NONE',  ( 0.000000000000000000, -1.000000000000000000, 0.000000000000000000 ) ) ;
#26761 = ADVANCED_FACE ( 'NONE', ( #36618 ), #69495, .F. ) ;
#26762 = DIRECTION ( 'NONE',  ( 0.000000000000000000, 1.000000000000000000, -0.000000000000000000 ) ) ;
#26763 = CYLINDRICAL_SURFACE ( 'NONE', #50296, 24.99999999998784972 ) ;
#26764 = AXIS2_PLACEMENT_3D ( 'NONE', #49066, #33824, #12253 ) ;
#26765 = DIRECTION ( 'NONE',  ( 1.000000000000000000, -0.000000000000000000, -0.000000000000000000 ) ) ;
#26766 = DIRECTION ( 'NONE',  ( -1.000000000000000000, 0.000000000000000000, -0.000000000000000000 ) ) ;
#26767 = EDGE_CURVE ( 'NONE', #22289, #10947, #58189, .T. ) ;
#26768 = CARTESIAN_POINT ( 'NONE',  ( 49.00000000000000000, -0.1999999999911430404, -8.864436962241481021E-12 ) ) ;
#26769 = EDGE_LOOP ( 'NONE', ( #44185, #46602, #7890, #28737 ) ) ;
#26770 = CIRCLE ( 'NONE', #66281, 0.5000000000079362072 ) ;
#26771 = ORIENTED_EDGE ( 'NONE', *, *, #50260, .F. ) ;
#26772 = DIRECTION ( 'NONE',  ( 0.000000000000000000, 1.000000000000000000, 0.000000000000000000 ) ) ;
#26773 = DIRECTION ( 'NONE',  ( 0.000000000000000000, -0.7084617869615144059, 0.7057491738679528837 ) ) ;
#26775 = ORIENTED_EDGE ( 'NONE', *, *, #10328, .T. ) ;
#26774 = EDGE_CURVE ( 'NONE', #24256, #56561, #42270, .T. ) ;
#26776 = LINE ( 'NONE', #26421, #1009 ) ;
#26777 = EDGE_CURVE ( 'NONE', #17604, #31415, #9764, .T. ) ;
#26778 = CARTESIAN_POINT ( 'NONE',  ( 7.250000000000005329, -8.249999999999998224, -26.00000000000001066 ) ) ;
#26779 = EDGE_CURVE ( 'NONE', #44522, #17797, #35552, .T. ) ;
#26780 = ORIENTED_EDGE ( 'NONE', *, *, #25524, .T. ) ;
#26781 = EDGE_CURVE ( 'NONE', #16233, #40339, #57834, .T. ) ;
#26782 = EDGE_CURVE ( 'NONE', #28379, #55647, #31343, .T. ) ;
#26783 = DIRECTION ( 'NONE',  ( 1.000000000000000000, 0.000000000000000000, 0.000000000000000000 ) ) ;
#26784 = ORIENTED_EDGE ( 'NONE', *, *, #24666, .F. ) ;
#26785 = ORIENTED_EDGE ( 'NONE', *, *, #21427, .F. ) ;
#26786 = DIRECTION ( 'NONE',  ( 0.000000000000000000, 0.000000000000000000, 1.000000000000000000 ) ) ;
#26787 = EDGE_LOOP ( 'NONE', ( #61420, #57383, #55648, #38249 ) ) ;
#26788 = CARTESIAN_POINT ( 'NONE',  ( -7.394232575409645847, -6.789561617636902469, 26.00000000000000000 ) ) ;
#26789 = EDGE_CURVE ( 'NONE', #59688, #41721, #52542, .T. ) ;
#26790 = CARTESIAN_POINT ( 'NONE',  ( -7.342976262117293373, -6.665817930929262225, 54.00000000000000711 ) ) ;
#26791 = LINE ( 'NONE', #69215, #16673 ) ;
#26792 = EDGE_CURVE ( 'NONE', #54627, #21960, #52910, .T. ) ;
#26793 = AXIS2_PLACEMENT_3D ( 'NONE', #4234, #15184, #65014 ) ;
#26794 = EDGE_LOOP ( 'NONE', ( #35008, #31059, #6136, #30657 ) ) ;
#26795 = ORIENTED_EDGE ( 'NONE', *, *, #6823, .T. ) ;
#26796 = DIRECTION ( 'NONE',  ( 0.000000000000000000, 0.000000000000000000, -1.000000000000000000 ) ) ;
#26798 = DIRECTION ( 'NONE',  ( 0.000000000000000000, 1.000000000000000000, 0.000000000000000000 ) ) ;
#26797 = DIRECTION ( 'NONE',  ( 1.836970198721029934E-16, 1.836970198721010706E-16, -1.000000000000000000 ) ) ;
#26799 = ORIENTED_EDGE ( 'NONE', *, *, #45142, .F. ) ;
#26800 = ORIENTED_EDGE ( 'NONE', *, *, #12422, .F. ) ;
#26801 = VERTEX_POINT ( 'NONE', #24962 ) ;
#26802 = VECTOR ( 'NONE', #3498, 1000.000000000000000 ) ;
#26803 = VECTOR ( 'NONE', #13679, 1000.000000000000000 ) ;
#26804 = CIRCLE ( 'NONE', #68539, 0.5000000000079367624 ) ;
#26805 = CARTESIAN_POINT ( 'NONE',  ( 7.250000000000005329, -7.449999999999998401, -20.00000000000000000 ) ) ;
#26806 = ADVANCED_FACE ( 'NONE', ( #4461 ), #3398, .F. ) ;
#26808 = VERTEX_POINT ( 'NONE', #69148 ) ;
#26807 = DIRECTION ( 'NONE',  ( -1.000000000000000000, 0.000000000000000000, 0.000000000000000000 ) ) ;
#26809 = EDGE_CURVE ( 'NONE', #36688, #56607, #19646, .T. ) ;
#26810 = VECTOR ( 'NONE', #30144, 1000.000000000000000 ) ;
#26811 = VECTOR ( 'NONE', #12674, 1000.000000000000000 ) ;
#26812 = CARTESIAN_POINT ( 'NONE',  ( 8.465062094116099445, 7.744988412222715723, 455.0000000000000568 ) ) ;
#26813 = DIRECTION ( 'NONE',  ( 0.000000000000000000, 0.000000000000000000, -1.000000000000000000 ) ) ;
#26814 = PRODUCT_DEFINITION_FORMATION_WITH_SPECIFIED_SOURCE ( 'ANY', '', #38037, .NOT_KNOWN. ) ;
#26815 = EDGE_LOOP ( 'NONE', ( #57043, #65800, #61025, #21294 ) ) ;
#26816 = EDGE_LOOP ( 'NONE', ( #27667, #39223 ) ) ;
#26817 = VECTOR ( 'NONE', #216, 1000.000000000000114 ) ;
#26818 = VECTOR ( 'NONE', #27225, 1000.000000000000114 ) ;
#26819 = FACE_OUTER_BOUND ( 'NONE', #46767, .T. ) ;
#26820 = ORIENTED_EDGE ( 'NONE', *, *, #59040, .T. ) ;
#26821 = LINE ( 'NONE', #36361, #1994 ) ;
#26822 = LINE ( 'NONE', #31779, #41441 ) ;
#26823 = ORIENTED_EDGE ( 'NONE', *, *, #22436, .F. ) ;
#26824 = AXIS2_PLACEMENT_3D ( 'NONE', #5268, #49767, #16905 ) ;
#26825 = EDGE_CURVE ( 'NONE', #68679, #10522, #36989, .T. ) ;
#26826 = DIRECTION ( 'NONE',  ( 0.000000000000000000, 0.000000000000000000, 1.000000000000000000 ) ) ;
#26827 = FACE_OUTER_BOUND ( 'NONE', #19682, .T. ) ;
#26829 = ORIENTED_EDGE ( 'NONE', *, *, #64014, .F. ) ;
#26828 = DIRECTION ( 'NONE',  ( -1.000000000000000000, 0.000000000000000000, 0.000000000000000000 ) ) ;
#26830 = ORIENTED_EDGE ( 'NONE', *, *, #57426, .F. ) ;
#26831 = CARTESIAN_POINT ( 'NONE',  ( -8.697938382363103571, -2.420780051175099423, 54.00000000000000711 ) ) ;
#26832 = DIRECTION ( 'NONE',  ( -0.000000000000000000, -0.000000000000000000, -1.000000000000000000 ) ) ;
#26833 = DIRECTION ( 'NONE',  ( 0.000000000000000000, 0.000000000000000000, -1.000000000000000000 ) ) ;
#26834 = CARTESIAN_POINT ( 'NONE',  ( 15.50000000000000000, -0.4000000000005274892, 22.50000000000000000 ) ) ;
#26835 = DIRECTION ( 'NONE',  ( -1.794541526872559352E-16, -1.000000000000000000, 0.000000000000000000 ) ) ;
#26836 = ORIENTED_EDGE ( 'NONE', *, *, #48259, .T. ) ;
#26837 = PLANE ( 'NONE',  #64064 ) ;
#26838 = DIRECTION ( 'NONE',  ( 0.000000000000000000, -1.000000000000000000, 0.000000000000000000 ) ) ;
#26839 = CARTESIAN_POINT ( 'NONE',  ( -8.250000000000001776, 7.250000000000000888, -26.00000000000001066 ) ) ;
#26840 = EDGE_CURVE ( 'NONE', #47971, #48505, #29960, .T. ) ;
#26842 = ORIENTED_EDGE ( 'NONE', *, *, #22440, .T. ) ;
#26841 = DIRECTION ( 'NONE',  ( 0.000000000000000000, 1.000000000000000000, 0.000000000000000000 ) ) ;
#26843 = VECTOR ( 'NONE', #48236, 1000.000000000000000 ) ;
#26844 = DIRECTION ( 'NONE',  ( 1.000000000000000000, 0.000000000000000000, 0.000000000000000000 ) ) ;
#26845 = CARTESIAN_POINT ( 'NONE',  ( -8.250000000000001776, 0.000000000000000000, -20.50000000000000000 ) ) ;
#26846 = EDGE_CURVE ( 'NONE', #16332, #27411, #17139, .T. ) ;
#26847 = FACE_OUTER_BOUND ( 'NONE', #41989, .T. ) ;
#26848 = ORIENTED_EDGE ( 'NONE', *, *, #59136, .T. ) ;
#26849 = CARTESIAN_POINT ( 'NONE',  ( 152.0064834503532722, -16.00648345035295250, 5.000000000000000000 ) ) ;
#26850 = ADVANCED_FACE ( 'NONE', ( #65584 ), #59236, .F. ) ;
#26851 = FACE_OUTER_BOUND ( 'NONE', #49502, .T. ) ;
#26852 = EDGE_LOOP ( 'NONE', ( #26516, #44958, #2745, #51117 ) ) ;
#26853 = CARTESIAN_POINT ( 'NONE',  ( 4.456444791733522252E-16, 7.450000000000002842, -8.500000000000000000 ) ) ;
#26854 = DIRECTION ( 'NONE',  ( -0.000000000000000000, -0.000000000000000000, -1.000000000000000000 ) ) ;
#26855 = CIRCLE ( 'NONE', #61805, 24.99999999998789946 ) ;
#26856 = VECTOR ( 'NONE', #54304, 1000.000000000000000 ) ;
#26857 = FACE_OUTER_BOUND ( 'NONE', #37862, .T. ) ;
#26858 = EDGE_CURVE ( 'NONE', #50893, #6839, #31097, .T. ) ;
#26859 = CARTESIAN_POINT ( 'NONE',  ( -30.00000000000000000, 0.000000000000000000, 27.00000000000000000 ) ) ;
#26860 = VECTOR ( 'NONE', #29345, 1000.000000000000000 ) ;
#26861 = FACE_OUTER_BOUND ( 'NONE', #37602, .T. ) ;
#26862 = ORIENTED_EDGE ( 'NONE', *, *, #38573, .T. ) ;
#26863 = PRODUCT_DEFINITION_FORMATION_WITH_SPECIFIED_SOURCE ( 'ANY', '', #37447, .NOT_KNOWN. ) ;
#26864 = ORIENTED_EDGE ( 'NONE', *, *, #30037, .F. ) ;
#26865 = CARTESIAN_POINT ( 'NONE',  ( -7.259684009079930611, 4.188533722949235205, 455.0000000000000568 ) ) ;
#26866 = VERTEX_POINT ( 'NONE', #16804 ) ;
#26867 = VERTEX_POINT ( 'NONE', #15757 ) ;
#26868 = DIRECTION ( 'NONE',  ( -0.000000000000000000, 0.000000000000000000, 1.000000000000000000 ) ) ;
#26869 = VECTOR ( 'NONE', #43256, 1000.000000000000000 ) ;
#26870 = AXIS2_PLACEMENT_3D ( 'NONE', #42690, #64272, #15821 ) ;
#26871 = EDGE_CURVE ( 'NONE', #42883, #11023, #48985, .T. ) ;
#26872 = CARTESIAN_POINT ( 'NONE',  ( 7.250000000000005329, 7.250000000000000888, -9.000000000000001776 ) ) ;
#26873 = DIRECTION ( 'NONE',  ( -0.000000000000000000, -0.000000000000000000, -1.000000000000000000 ) ) ;
#26874 = ORIENTED_EDGE ( 'NONE', *, *, #19983, .T. ) ;
#26875 = VERTEX_POINT ( 'NONE', #49661 ) ;
#26876 = LINE ( 'NONE', #49118, #5907 ) ;
#26877 = ORIENTED_EDGE ( 'NONE', *, *, #22911, .F. ) ;
#26878 = EDGE_LOOP ( 'NONE', ( #46537, #31337, #19504, #41829 ) ) ;
#26879 = CIRCLE ( 'NONE', #17824, 0.1999999999999987899 ) ;
#26880 = CARTESIAN_POINT ( 'NONE',  ( 7.250000000000005329, 8.250000000000001776, -26.00000000000001066 ) ) ;
#26881 = CARTESIAN_POINT ( 'NONE',  ( 283.0000000000000568, -42.00000000000000000, -7.000000000000000000 ) ) ;
#26882 = DIRECTION ( 'NONE',  ( -1.836970198721029934E-16, 1.836970198721036590E-16, -1.000000000000000000 ) ) ;
#26883 = ORIENTED_EDGE ( 'NONE', *, *, #53665, .F. ) ;
#26884 = DIRECTION ( 'NONE',  ( 1.000000000000000000, 0.000000000000000000, 0.000000000000000000 ) ) ;
#26886 = CARTESIAN_POINT ( 'NONE',  ( 4.406483450353420928, 11.77351654964658501, 455.0000000000000568 ) ) ;
#26885 = CARTESIAN_POINT ( 'NONE',  ( 11.50000000000000000, -11.50000000000100009, 15.00000000000084910 ) ) ;
#26887 = VERTEX_POINT ( 'NONE', #11139 ) ;
#26888 = EDGE_LOOP ( 'NONE', ( #14885, #39833, #45460, #1991 ) ) ;
#26890 = ORIENTED_EDGE ( 'NONE', *, *, #12767, .F. ) ;
#26889 = DIRECTION ( 'NONE',  ( 0.000000000000000000, 0.000000000000000000, 1.000000000000000000 ) ) ;
#26891 = ORIENTED_EDGE ( 'NONE', *, *, #57492, .F. ) ;
#26892 = DIRECTION ( 'NONE',  ( 1.836970198721029934E-16, 1.836970198721010706E-16, -1.000000000000000000 ) ) ;
#26893 = EDGE_CURVE ( 'NONE', #40508, #20305, #36749, .T. ) ;
#26894 = ADVANCED_FACE ( 'NONE', ( #69846 ), #6543, .T. ) ;
#26895 = CARTESIAN_POINT ( 'NONE',  ( 30.90000000000000213, 0.000000000000000000, 0.000000000000000000 ) ) ;
#26896 = AXIS2_PLACEMENT_3D ( 'NONE', #68315, #15634, #36857 ) ;
#26897 = VERTEX_POINT ( 'NONE', #21756 ) ;
#26898 = EDGE_CURVE ( 'NONE', #7775, #40339, #9644, .T. ) ;
#26899 = LINE ( 'NONE', #47750, #49325 ) ;
#26900 = DIRECTION ( 'NONE',  ( 0.000000000000000000, 0.000000000000000000, 1.000000000000000000 ) ) ;
#26901 = VERTEX_POINT ( 'NONE', #27410 ) ;
#26902 = VERTEX_POINT ( 'NONE', #27060 ) ;
#26903 = FACE_OUTER_BOUND ( 'NONE', #40985, .T. ) ;
#26904 = DIRECTION ( 'NONE',  ( 0.000000000000000000, -1.000000000000000000, 0.000000000000000000 ) ) ;
#26905 = CARTESIAN_POINT ( 'NONE',  ( -10.49297626211724754, -3.664523737882706023, 26.00000000000000000 ) ) ;
#26906 = VERTEX_POINT ( 'NONE', #49337 ) ;
#26907 = CIRCLE ( 'NONE', #51728, 0.1999999999999987899 ) ;
#26908 = CARTESIAN_POINT ( 'NONE',  ( 7.811466277050736373, -4.740315990920255906, 455.0000000000000568 ) ) ;
#26909 = DIRECTION ( 'NONE',  ( 0.000000000000000000, 0.000000000000000000, 1.000000000000000000 ) ) ;
#26911 = ORIENTED_EDGE ( 'NONE', *, *, #27930, .T. ) ;
#26910 = DIRECTION ( 'NONE',  ( 0.000000000000000000, -0.7278708115916149302, -0.6857142857145122061 ) ) ;
#26913 = VERTEX_POINT ( 'NONE', #43317 ) ;
#26912 = DIRECTION ( 'NONE',  ( -1.000000000000000000, 0.000000000000000000, 0.000000000000000000 ) ) ;
#26914 = DIRECTION ( 'NONE',  ( 0.000000000000000000, -3.673940397442059868E-16, 1.000000000000000000 ) ) ;
#26915 = AXIS2_PLACEMENT_3D ( 'NONE', #49492, #1058, #1727 ) ;
#26916 = DIRECTION ( 'NONE',  ( 0.000000000000000000, 0.000000000000000000, -1.000000000000000000 ) ) ;
#26917 = CYLINDRICAL_SURFACE ( 'NONE', #69684, 2.204799999999997429 ) ;
#26918 = CARTESIAN_POINT ( 'NONE',  ( 40.90000000000000568, 0.000000000000000000, 0.000000000000000000 ) ) ;
#26919 = DIRECTION ( 'NONE',  ( 0.000000000000000000, 0.000000000000000000, -1.000000000000000000 ) ) ;
#26920 = CARTESIAN_POINT ( 'NONE',  ( -8.250000000000001776, -7.249999999999998224, -18.50000000000000000 ) ) ;
#26921 = ORIENTED_EDGE ( 'NONE', *, *, #49285, .T. ) ;
#26922 = PLANE ( 'NONE',  #69948 ) ;
#26924 = ORIENTED_EDGE ( 'NONE', *, *, #44387, .F. ) ;
#26923 = DIRECTION ( 'NONE',  ( 0.000000000000000000, -0.000000000000000000, -1.000000000000000000 ) ) ;
#26925 = CIRCLE ( 'NONE', #7655, 1.000000000000000888 ) ;
#26926 = ADVANCED_FACE ( 'NONE', ( #21061 ), #538, .T. ) ;
#26928 = ORIENTED_EDGE ( 'NONE', *, *, #12525, .F. ) ;
#26927 = DIRECTION ( 'NONE',  ( 1.000000000000000000, -0.000000000000000000, -0.000000000000000000 ) ) ;
#26929 = SURFACE_STYLE_USAGE ( .BOTH. , #65778 ) ;
#26930 = DIRECTION ( 'NONE',  ( 0.000000000000000000, 0.000000000000000000, -1.000000000000000000 ) ) ;
#26931 = EDGE_CURVE ( 'NONE', #5431, #46013, #16456, .T. ) ;
#26932 = ORIENTED_EDGE ( 'NONE', *, *, #27784, .F. ) ;
#26933 = FACE_OUTER_BOUND ( 'NONE', #54554, .T. ) ;
#26934 = EDGE_CURVE ( 'NONE', #37901, #22868, #65254, .T. ) ;
#26935 = CARTESIAN_POINT ( 'NONE',  ( 7.500000000000000000, -20.49999999999999645, -16.00000000000000000 ) ) ;
#26936 = EDGE_CURVE ( 'NONE', #30390, #69031, #24312, .T. ) ;
#26937 = ORIENTED_EDGE ( 'NONE', *, *, #60280, .F. ) ;
#26938 = DIRECTION ( 'NONE',  ( -1.000000000000000000, 0.000000000000000000, 0.000000000000000000 ) ) ;
#26939 = DIRECTION ( 'NONE',  ( 1.836970198721029934E-16, -1.836970198721036344E-16, 1.000000000000000000 ) ) ;
#26940 = EDGE_CURVE ( 'NONE', #68528, #3061, #33407, .T. ) ;
#26941 = EDGE_CURVE ( 'NONE', #48716, #17051, #37333, .T. ) ;
#26942 = EDGE_CURVE ( 'NONE', #26902, #48304, #51416, .T. ) ;
#26943 = ORIENTED_EDGE ( 'NONE', *, *, #23873, .T. ) ;
#26944 = CARTESIAN_POINT ( 'NONE',  ( 7.250000000000004441, 7.450000000000001954, -15.00000000000000000 ) ) ;
#26945 = ORIENTED_EDGE ( 'NONE', *, *, #39819, .F. ) ;
#26946 = EDGE_LOOP ( 'NONE', ( #51190, #5441, #29538, #48777 ) ) ;
#26947 = LINE ( 'NONE', #17710, #17800 ) ;
#26948 = CARTESIAN_POINT ( 'NONE',  ( 21.90000000000000213, -21.00000000000001421, -13.86939075806900945 ) ) ;
#26949 = DIRECTION ( 'NONE',  ( -1.000000000000000000, 0.000000000000000000, 0.000000000000000000 ) ) ;
#26950 = DIRECTION ( 'NONE',  ( -1.000000000000000000, 0.000000000000000000, 0.000000000000000000 ) ) ;
#26951 = ORIENTED_EDGE ( 'NONE', *, *, #58486, .T. ) ;
#26952 = ORIENTED_EDGE ( 'NONE', *, *, #4596, .T. ) ;
#26954 = ORIENTED_EDGE ( 'NONE', *, *, #32111, .F. ) ;
#26953 = DIRECTION ( 'NONE',  ( 0.000000000000000000, 0.000000000000000000, -1.000000000000000000 ) ) ;
#26955 = ORIENTED_EDGE ( 'NONE', *, *, #28527, .F. ) ;
#26956 = VECTOR ( 'NONE', #50323, 1000.000000000000000 ) ;
#26957 = DIRECTION ( 'NONE',  ( -1.794541526872559352E-16, -1.000000000000000000, 0.000000000000000000 ) ) ;
#26958 = DIRECTION ( 'NONE',  ( -1.678252938371784572E-14, -1.000000000000000000, -1.836970198721041520E-16 ) ) ;
#26959 = CARTESIAN_POINT ( 'NONE',  ( 15.50000000000000000, 998.9628421096749662, 22.50000000000000000 ) ) ;
#26960 = AXIS2_PLACEMENT_3D ( 'NONE', #39405, #56371, #28789 ) ;
#26961 = CARTESIAN_POINT ( 'NONE',  ( 4.456444791733522252E-16, 7.450000000000002842, -22.50000000000000000 ) ) ;
#26963 = DIRECTION ( 'NONE',  ( 1.000000000000000000, 0.000000000000000000, 0.000000000000000000 ) ) ;
#26962 = DIRECTION ( 'NONE',  ( 1.000000000000000000, -0.000000000000000000, -0.000000000000000000 ) ) ;
#26964 = ORIENTED_EDGE ( 'NONE', *, *, #20559, .F. ) ;
#26966 = ORIENTED_EDGE ( 'NONE', *, *, #15852, .F. ) ;
#26965 = LINE ( 'NONE', #38272, #57823 ) ;
#26967 = ORIENTED_EDGE ( 'NONE', *, *, #67796, .F. ) ;
#26968 = ORIENTED_EDGE ( 'NONE', *, *, #52734, .F. ) ;
#26969 = CARTESIAN_POINT ( 'NONE',  ( 0.5000000000000000000, -42.50000000000000000, 26.50000000000000000 ) ) ;
#26970 = DIRECTION ( 'NONE',  ( -0.000000000000000000, -0.000000000000000000, 1.000000000000000000 ) ) ;
#26971 = DIRECTION ( 'NONE',  ( 0.000000000000000000, 0.000000000000000000, 1.000000000000000000 ) ) ;
#26973 = AXIS2_PLACEMENT_3D ( 'NONE', #54220, #64145, #10722 ) ;
#26972 = VECTOR ( 'NONE', #35066, 1000.000000000000000 ) ;
#26974 = EDGE_CURVE ( 'NONE', #28387, #32424, #48287, .T. ) ;
#26975 = DIRECTION ( 'NONE',  ( 0.000000000000000000, 0.000000000000000000, 1.000000000000000000 ) ) ;
#26976 = EDGE_LOOP ( 'NONE', ( #21225, #8689, #46064, #12735 ) ) ;
#26977 = ORIENTED_EDGE ( 'NONE', *, *, #30336, .T. ) ;
#26978 = VERTEX_POINT ( 'NONE', #18514 ) ;
#26979 = EDGE_CURVE ( 'NONE', #29633, #11032, #29829, .T. ) ;
#26980 = EDGE_CURVE ( 'NONE', #47295, #2646, #40444, .T. ) ;
#26981 = DIRECTION ( 'NONE',  ( 0.000000000000000000, 0.000000000000000000, 1.000000000000000000 ) ) ;
#26982 = DIRECTION ( 'NONE',  ( 0.000000000000000000, 1.000000000000000000, 0.000000000000000000 ) ) ;
#26983 = CARTESIAN_POINT ( 'NONE',  ( 11.00000000000000000, -12.00000000000000000, -10.20500000000000007 ) ) ;
#26984 = EDGE_CURVE ( 'NONE', #61547, #17833, #8253, .T. ) ;
#26985 = ORIENTED_EDGE ( 'NONE', *, *, #7903, .T. ) ;
#26986 = VERTEX_POINT ( 'NONE', #2266 ) ;
#26987 = LINE ( 'NONE', #53176, #50856 ) ;
#26988 = DIRECTION ( 'NONE',  ( 1.047444401652940007E-14, 1.000000000000000000, 1.836970198721029934E-16 ) ) ;
#26989 = VERTEX_POINT ( 'NONE', #23487 ) ;
#26990 = CARTESIAN_POINT ( 'NONE',  ( 39.90000000000000568, 0.000000000000000000, 5.250000000000000000 ) ) ;
#26992 = EDGE_LOOP ( 'NONE', ( #18224, #458 ) ) ;
#26991 = DIRECTION ( 'NONE',  ( 0.000000000000000000, 0.000000000000000000, 1.000000000000000000 ) ) ;
#26993 = EDGE_LOOP ( 'NONE', ( #29361, #10263, #29383, #36174, #68074 ) ) ;
#26994 = CARTESIAN_POINT ( 'NONE',  ( 4.255011587777218551, -8.465062094116168723, 455.0000000000000568 ) ) ;
#26995 = LINE ( 'NONE', #48557, #6356 ) ;
#26996 = DIRECTION ( 'NONE',  ( 1.000000000000000000, 0.000000000000000000, 0.000000000000000000 ) ) ;
#26997 = DIRECTION ( 'NONE',  ( -1.000000000000000000, 0.000000000000000000, 0.000000000000000000 ) ) ;
#26998 = VECTOR ( 'NONE', #53580, 1000.000000000000000 ) ;
#26999 = DIRECTION ( 'NONE',  ( -1.000000000000000000, 0.000000000000000000, 0.000000000000000000 ) ) ;
#27000 = VERTEX_POINT ( 'NONE', #28776 ) ;
#27001 = DIRECTION ( 'NONE',  ( 0.000000000000000000, 0.000000000000000000, 1.000000000000000000 ) ) ;
#27002 = AXIS2_PLACEMENT_3D ( 'NONE', #46411, #61617, #57373 ) ;
#27003 = ORIENTED_EDGE ( 'NONE', *, *, #59732, .T. ) ;
#27004 = CARTESIAN_POINT ( 'NONE',  ( 7.000000000000000000, -25.00000000000299849, -9.079999998829670460 ) ) ;
#27005 = DIRECTION ( 'NONE',  ( 8.673617379884013384E-15, 1.000000000000000000, 0.000000000000000000 ) ) ;
#27006 = DIRECTION ( 'NONE',  ( 0.000000000000000000, 1.000000000000000000, 0.000000000000000000 ) ) ;
#27007 = DIRECTION ( 'NONE',  ( 0.000000000000000000, 0.000000000000000000, 1.000000000000000000 ) ) ;
#27008 = VECTOR ( 'NONE', #17414, 1000.000000000000000 ) ;
#27009 = DIRECTION ( 'NONE',  ( -1.836970198721029934E-16, -1.836970198721010706E-16, 1.000000000000000000 ) ) ;
#27010 = ORIENTED_EDGE ( 'NONE', *, *, #37891, .T. ) ;
#27011 = AXIS2_PLACEMENT_3D ( 'NONE', #29005, #66139, #1106 ) ;
#27012 = DIRECTION ( 'NONE',  ( 1.000000000000000000, 0.000000000000000000, 0.000000000000000000 ) ) ;
#27013 = EDGE_CURVE ( 'NONE', #64069, #17432, #53710, .T. ) ;
#27014 = SURFACE_STYLE_FILL_AREA ( #26314 ) ;
#27016 = AXIS2_PLACEMENT_3D ( 'NONE', #40875, #34517, #29565 ) ;
#27015 = AXIS2_PLACEMENT_3D ( 'NONE', #1344, #27188, #11586 ) ;
#27017 = EDGE_CURVE ( 'NONE', #10522, #27734, #35126, .T. ) ;
#27018 = ORIENTED_EDGE ( 'NONE', *, *, #56455, .F. ) ;
#27019 = FACE_OUTER_BOUND ( 'NONE', #21128, .T. ) ;
#27020 = DIRECTION ( 'NONE',  ( -1.000000000000000000, 0.000000000000000000, 0.000000000000000000 ) ) ;
#27021 = EDGE_LOOP ( 'NONE', ( #60468, #38687, #60463, #5547, #19863, #27311 ) ) ;
#27022 = DIRECTION ( 'NONE',  ( -9.973078850062115052E-15, -1.000000000000000000, 0.000000000000000000 ) ) ;
#27023 = VECTOR ( 'NONE', #59437, 1000.000000000000114 ) ;
#27024 = CARTESIAN_POINT ( 'NONE',  ( 29.50000000000000355, -15.97213595500069871, 14.50000000000000000 ) ) ;
#27025 = EDGE_LOOP ( 'NONE', ( #6240, #24676, #50917, #30293 ) ) ;
#27026 = FACE_OUTER_BOUND ( 'NONE', #40486, .T. ) ;
#27027 = DIRECTION ( 'NONE',  ( -1.000000000000000000, 0.000000000000000000, 0.000000000000000000 ) ) ;
#27028 = SURFACE_STYLE_USAGE ( .BOTH. , #22754 ) ;
#27029 = CARTESIAN_POINT ( 'NONE',  ( 29.50000000000000355, -11.70000000000000284, -11.00000000000000000 ) ) ;
#27030 = ORIENTED_EDGE ( 'NONE', *, *, #7066, .T. ) ;
#27032 = EDGE_LOOP ( 'NONE', ( #53906, #60824, #59929, #37517 ) ) ;
#27031 = DIRECTION ( 'NONE',  ( 0.000000000000000000, 0.000000000000000000, -1.000000000000000000 ) ) ;
#27033 = ADVANCED_FACE ( 'NONE', ( #13219 ), #66277, .F. ) ;
#27034 = LINE ( 'NONE', #882, #20325 ) ;
#27035 = FACE_OUTER_BOUND ( 'NONE', #56760, .T. ) ;
#27036 = CIRCLE ( 'NONE', #15772, 5.000000000000000000 ) ;
#27037 = CARTESIAN_POINT ( 'NONE',  ( 9.912023737882815766, -6.657023737882824754, 54.00000000000000711 ) ) ;
#27038 = ORIENTED_EDGE ( 'NONE', *, *, #67099, .T. ) ;
#27039 = CARTESIAN_POINT ( 'NONE',  ( -11.07551654964667520, 10.19191654964664018, 195.0000000000000284 ) ) ;
#27040 = FACE_OUTER_BOUND ( 'NONE', #42121, .T. ) ;
#27041 = ORIENTED_EDGE ( 'NONE', *, *, #50341, .T. ) ;
#27042 = ORIENTED_EDGE ( 'NONE', *, *, #48703, .T. ) ;
#27043 = VECTOR ( 'NONE', #67742, 1000.000000000000000 ) ;
#27044 = ORIENTED_EDGE ( 'NONE', *, *, #49810, .F. ) ;
#27045 = CARTESIAN_POINT ( 'NONE',  ( -10.30047626211724499, -3.857023737882708581, 26.00000000000000000 ) ) ;
#27046 = CIRCLE ( 'NONE', #8960, 2.285366197183106074 ) ;
#27047 = VECTOR ( 'NONE', #18665, 1000.000000000000000 ) ;
#27048 = DIRECTION ( 'NONE',  ( -1.836970198721029934E-16, 1.836970198721036344E-16, -1.000000000000000000 ) ) ;
#27049 = VERTEX_POINT ( 'NONE', #1233 ) ;
#27050 = EDGE_LOOP ( 'NONE', ( #66528, #51516, #31492, #19626, #32690, #31736 ) ) ;
#27051 = CIRCLE ( 'NONE', #16903, 0.1999999999999996503 ) ;
#27052 = CARTESIAN_POINT ( 'NONE',  ( -10.08346604330787777, 2.893516549646604208, 195.0000000000000284 ) ) ;
#27053 = ORIENTED_EDGE ( 'NONE', *, *, #29216, .T. ) ;
#27054 = ORIENTED_EDGE ( 'NONE', *, *, #62265, .F. ) ;
#27055 = EDGE_CURVE ( 'NONE', #3474, #56963, #56354, .T. ) ;
#27056 = ORIENTED_EDGE ( 'NONE', *, *, #4736, .F. ) ;
#27057 = CIRCLE ( 'NONE', #53015, 0.3999999999999993006 ) ;
#27058 = ORIENTED_EDGE ( 'NONE', *, *, #52864, .T. ) ;
#27059 = CARTESIAN_POINT ( 'NONE',  ( -11.00000000000000000, -5.599999999999999645, 27.00000000000000000 ) ) ;
#27061 = VERTEX_POINT ( 'NONE', #39730 ) ;
#27060 = CARTESIAN_POINT ( 'NONE',  ( -7.250000000000000000, -7.449999999999998401, -20.00000000000000000 ) ) ;
#27062 = VECTOR ( 'NONE', #39422, 1000.000000000000000 ) ;
#27063 = LINE ( 'NONE', #33409, #26666 ) ;
#27064 = LINE ( 'NONE', #33744, #17128 ) ;
#27065 = LINE ( 'NONE', #33745, #16666 ) ;
#27066 = ORIENTED_EDGE ( 'NONE', *, *, #4847, .T. ) ;
#27067 = AXIS2_PLACEMENT_3D ( 'NONE', #57910, #41291, #35992 ) ;
#27068 = ADVANCED_FACE ( 'NONE', ( #7207 ), #24180, .T. ) ;
#27069 = FACE_OUTER_BOUND ( 'NONE', #28028, .T. ) ;
#27070 = EDGE_CURVE ( 'NONE', #41911, #2041, #33410, .T. ) ;
#27071 = DIRECTION ( 'NONE',  ( -1.000000000000000000, 3.491481338843132961E-15, 0.000000000000000000 ) ) ;
#27072 = ORIENTED_EDGE ( 'NONE', *, *, #60505, .T. ) ;
#27073 = CARTESIAN_POINT ( 'NONE',  ( 282.8893988437589542, -25.27116123426318239, -17.22883876573683182 ) ) ;
#27074 = PLANE ( 'NONE',  #2897 ) ;
#27075 = DIRECTION ( 'NONE',  ( -1.000000000000000000, 0.000000000000000000, 0.000000000000000000 ) ) ;
#27076 = AXIS2_PLACEMENT_3D ( 'NONE', #3573, #62601, #2167 ) ;
#27077 = VERTEX_POINT ( 'NONE', #45386 ) ;
#27078 = DIRECTION ( 'NONE',  ( -0.000000000000000000, 3.673940397442059868E-16, -1.000000000000000000 ) ) ;
#27079 = CARTESIAN_POINT ( 'NONE',  ( -9.390476262117259054, 1.466476262117183627, 54.00000000000000711 ) ) ;
#27080 = FACE_OUTER_BOUND ( 'NONE', #58106, .T. ) ;
#27081 = LINE ( 'NONE', #21430, #64721 ) ;
#27082 = CARTESIAN_POINT ( 'NONE',  ( 15.50000000000000000, -1.037157890325000054, 22.50000000000000000 ) ) ;
#27083 = DIRECTION ( 'NONE',  ( -0.000000000000000000, -0.000000000000000000, -1.000000000000000000 ) ) ;
#27084 = VECTOR ( 'NONE', #10761, 1000.000000000000000 ) ;
#27085 = CARTESIAN_POINT ( 'NONE',  ( 275.5000000000000000, 0.000000000000000000, 26.50000000000000000 ) ) ;
#27086 = CIRCLE ( 'NONE', #29182, 1.224999999999997868 ) ;
#27087 = CYLINDRICAL_SURFACE ( 'NONE', #655, 0.3499999999998886224 ) ;
#27088 = ADVANCED_FACE ( 'NONE', ( #12852 ), #34417, .F. ) ;
#27089 = VECTOR ( 'NONE', #56819, 1000.000000000000000 ) ;
#27090 = EDGE_CURVE ( 'NONE', #47795, #55063, #65916, .T. ) ;
#27091 = ORIENTED_EDGE ( 'NONE', *, *, #20637, .F. ) ;
#27092 = DIRECTION ( 'NONE',  ( -1.000000000000000000, 0.000000000000000000, 0.000000000000000000 ) ) ;
#27093 = EDGE_CURVE ( 'NONE', #30530, #67203, #17479, .T. ) ;
#27094 = DIRECTION ( 'NONE',  ( -1.000000000000000000, 0.000000000000000000, 0.000000000000000000 ) ) ;
#27095 = AXIS2_PLACEMENT_3D ( 'NONE', #43422, #55434, #33514 ) ;
#27096 = CARTESIAN_POINT ( 'NONE',  ( 9.912023737882815766, -6.832023737882823688, 54.00000000000000711 ) ) ;
#27097 = PLANE ( 'NONE',  #42067 ) ;
#27098 = VERTEX_POINT ( 'NONE', #39049 ) ;
#27099 = LINE ( 'NONE', #10831, #34334 ) ;
#27100 = LINE ( 'NONE', #31723, #29393 ) ;
#27101 = ADVANCED_FACE ( 'NONE', ( #66954 ), #61650, .F. ) ;
#27102 = DIRECTION ( 'NONE',  ( -1.000000000000000000, 0.000000000000000000, 0.000000000000000000 ) ) ;
#27103 = EDGE_CURVE ( 'NONE', #1005, #56517, #29481, .T. ) ;
#27104 = AXIS2_PLACEMENT_3D ( 'NONE', #11356, #29000, #6406 ) ;
#27105 = DIRECTION ( 'NONE',  ( 1.836970198721029934E-16, 1.836970198721010706E-16, -1.000000000000000000 ) ) ;
#27106 = DIRECTION ( 'NONE',  ( 0.000000000000000000, -0.2142857142857146346, -0.9767710236555243730 ) ) ;
#27107 = EDGE_CURVE ( 'NONE', #47507, #4279, #2607, .T. ) ;
#27108 = LINE ( 'NONE', #44049, #2310 ) ;
#27109 = AXIS2_PLACEMENT_3D ( 'NONE', #49659, #23127, #18511 ) ;
#27110 = EDGE_LOOP ( 'NONE', ( #20931, #27293, #32452, #28777 ) ) ;
#27111 = ADVANCED_FACE ( 'NONE', ( #28430 ), #12511, .T. ) ;
#27112 = AXIS2_PLACEMENT_3D ( 'NONE', #7518, #51348, #23082 ) ;
#27113 = VERTEX_POINT ( 'NONE', #58481 ) ;
#27114 = DIRECTION ( 'NONE',  ( -0.000000000000000000, -0.000000000000000000, -1.000000000000000000 ) ) ;
#27115 = CARTESIAN_POINT ( 'NONE',  ( -5.242976262117259978, 5.242976262117182706, 54.00000000000000711 ) ) ;
#27116 = ORIENTED_EDGE ( 'NONE', *, *, #23874, .T. ) ;
#27117 = CARTESIAN_POINT ( 'NONE',  ( -5.993516549646711766, 5.993516549646603409, 455.0000000000000568 ) ) ;
#27118 = AXIS2_PLACEMENT_3D ( 'NONE', #35853, #9692, #19240 ) ;
#27119 = VECTOR ( 'NONE', #56085, 1000.000000000000000 ) ;
#27120 = DIRECTION ( 'NONE',  ( 0.000000000000000000, 0.000000000000000000, 1.000000000000000000 ) ) ;
#27121 = VERTEX_POINT ( 'NONE', #36534 ) ;
#27122 = FACE_OUTER_BOUND ( 'NONE', #3031, .T. ) ;
#27123 = ORIENTED_EDGE ( 'NONE', *, *, #14926, .F. ) ;
#27124 = ORIENTED_EDGE ( 'NONE', *, *, #5944, .F. ) ;
#27125 = CARTESIAN_POINT ( 'NONE',  ( 0.000000000000000000, -8.249999999999998224, -15.50000000000000000 ) ) ;
#27126 = ORIENTED_EDGE ( 'NONE', *, *, #40132, .F. ) ;
#27127 = CARTESIAN_POINT ( 'NONE',  ( -30.00000000000000000, -13.54524521594299991, 17.53999999999999915 ) ) ;
#27128 = DIRECTION ( 'NONE',  ( 1.000000000000000000, -5.981805089575194965E-17, 0.000000000000000000 ) ) ;
#27129 = LINE ( 'NONE', #68523, #52824 ) ;
#27130 = VECTOR ( 'NONE', #32710, 1000.000000000000000 ) ;
#27131 = EDGE_CURVE ( 'NONE', #37776, #62704, #67665, .T. ) ;
#27132 = VERTEX_POINT ( 'NONE', #51759 ) ;
#27133 = ORIENTED_EDGE ( 'NONE', *, *, #22521, .T. ) ;
#27134 = LINE ( 'NONE', #43383, #7505 ) ;
#27136 = DIRECTION ( 'NONE',  ( 0.000000000000000000, -5.800915303574361727E-12, 1.000000000000000000 ) ) ;
#27135 = DIRECTION ( 'NONE',  ( -0.000000000000000000, 3.673940397442059868E-16, -1.000000000000000000 ) ) ;
#27137 = ORIENTED_EDGE ( 'NONE', *, *, #12602, .F. ) ;
#27138 = ORIENTED_EDGE ( 'NONE', *, *, #49220, .F. ) ;
#27139 = EDGE_CURVE ( 'NONE', #61504, #64531, #57122, .T. ) ;
#27141 = VERTEX_POINT ( 'NONE', #19226 ) ;
#27140 = CONTEXT_DEPENDENT_SHAPE_REPRESENTATION ( #59845, #22795 ) ;
#27142 = CARTESIAN_POINT ( 'NONE',  ( 14.25000000000000000, -2.500000000000000000, -21.77831216351300014 ) ) ;
#27143 = AXIS2_PLACEMENT_3D ( 'NONE', #61920, #13478, #3231 ) ;
#27145 = ORIENTED_EDGE ( 'NONE', *, *, #55993, .F. ) ;
#27144 = PLANE ( 'NONE',  #49930 ) ;
#27146 = CARTESIAN_POINT ( 'NONE',  ( -8.697938382363098242, -2.420780051175094094, 26.00000000000000711 ) ) ;
#27147 = AXIS2_PLACEMENT_3D ( 'NONE', #7608, #3357, #19610 ) ;
#27148 = DIRECTION ( 'NONE',  ( 1.836970198721029934E-16, 1.836970198721010706E-16, -1.000000000000000000 ) ) ;
#27149 = ORIENTED_EDGE ( 'NONE', *, *, #34777, .F. ) ;
#27150 = ORIENTED_EDGE ( 'NONE', *, *, #52170, .T. ) ;
#27151 = AXIS2_PLACEMENT_3D ( 'NONE', #26394, #20732, #63878 ) ;
#27152 = DIRECTION ( 'NONE',  ( 0.000000000000000000, 1.000000000000000000, 0.000000000000000000 ) ) ;
#27153 = EDGE_LOOP ( 'NONE', ( #57884, #3531, #4309, #45280 ) ) ;
#27154 = VECTOR ( 'NONE', #26498, 1000.000000000000000 ) ;
#27155 = FACE_OUTER_BOUND ( 'NONE', #40205, .T. ) ;
#27156 = CARTESIAN_POINT ( 'NONE',  ( 13.00000000000000178, -15.50000000000000000, -20.05051025721700242 ) ) ;
#27157 = EDGE_CURVE ( 'NONE', #10558, #61792, #68729, .T. ) ;
#27158 = VECTOR ( 'NONE', #21679, 1000.000000000000000 ) ;
#27159 = ORIENTED_EDGE ( 'NONE', *, *, #16142, .T. ) ;
#27160 = CIRCLE ( 'NONE', #66028, 0.2000000000000005107 ) ;
#27161 = CARTESIAN_POINT ( 'NONE',  ( -7.250000000000000888, 7.250000000000001776, -22.50000000000000000 ) ) ;
#27162 = CARTESIAN_POINT ( 'NONE',  ( -15.50000000000000000, -0.2000000000000000111, -22.50000000000000000 ) ) ;
#27163 = EDGE_CURVE ( 'NONE', #25985, #36828, #46443, .T. ) ;
#27165 = ORIENTED_EDGE ( 'NONE', *, *, #55654, .T. ) ;
#27164 = DIRECTION ( 'NONE',  ( -1.836970198721029934E-16, 1.836970198721036344E-16, -1.000000000000000000 ) ) ;
#27166 = ORIENTED_EDGE ( 'NONE', *, *, #38008, .F. ) ;
#27167 = ADVANCED_FACE ( 'NONE', ( #2963 ), #30538, .F. ) ;
#27168 = CARTESIAN_POINT ( 'NONE',  ( -15.50000000000000000, -1.037157890325000054, 26.50000000000000000 ) ) ;
#27169 = VECTOR ( 'NONE', #67522, 1000.000000000000000 ) ;
#27170 = AXIS2_PLACEMENT_3D ( 'NONE', #18163, #55651, #45727 ) ;
#27171 = CARTESIAN_POINT ( 'NONE',  ( 15.50000000000000000, 0.000000000000000000, 22.50000000000000000 ) ) ;
#27172 = EDGE_CURVE ( 'NONE', #15713, #17105, #36183, .T. ) ;
#27173 = DIRECTION ( 'NONE',  ( 0.000000000000000000, 1.000000000000000000, 0.000000000000000000 ) ) ;
#27174 = EDGE_CURVE ( 'NONE', #4952, #19035, #59405, .T. ) ;
#27175 = EDGE_CURVE ( 'NONE', #28094, #20614, #36906, .T. ) ;
#27176 = CARTESIAN_POINT ( 'NONE',  ( 151.5599459900709860, -10.00000000000000178, 326.8892501111512843 ) ) ;
#27177 = LINE ( 'NONE', #48737, #44352 ) ;
#27178 = ORIENTED_EDGE ( 'NONE', *, *, #38805, .T. ) ;
#27179 = DIRECTION ( 'NONE',  ( -1.000000000000000000, 1.610765207321970913E-14, 1.836970198721059516E-16 ) ) ;
#27180 = DIRECTION ( 'NONE',  ( -1.000000000000000000, -5.013651664672856055E-16, 0.000000000000000000 ) ) ;
#27181 = ADVANCED_FACE ( 'NONE', ( #13917 ), #63063, .F. ) ;
#27182 = CARTESIAN_POINT ( 'NONE',  ( -9.547976262117222390, -2.369523737882729186, 54.00000000000000711 ) ) ;
#27184 = ORIENTED_EDGE ( 'NONE', *, *, #17109, .T. ) ;
#27183 = LINE ( 'NONE', #10220, #43492 ) ;
#27185 = CARTESIAN_POINT ( 'NONE',  ( -8.250000000000001776, -7.249999999999998224, -26.00000000000001066 ) ) ;
#27186 = AXIS2_PLACEMENT_3D ( 'NONE', #109, #21673, #64807 ) ;
#27187 = EDGE_CURVE ( 'NONE', #56499, #15565, #8609, .T. ) ;
#27188 = DIRECTION ( 'NONE',  ( 1.000000000000000000, -0.000000000000000000, -0.000000000000000000 ) ) ;
#27189 = CARTESIAN_POINT ( 'NONE',  ( 40.90000000000000568, 0.000000000000000000, 3.447897592003593022E-15 ) ) ;
#27190 = ADVANCED_FACE ( 'NONE', ( #41137 ), #69063, .T. ) ;
#27191 = CARTESIAN_POINT ( 'NONE',  ( -30.00000000000000000, -11.70000000000000284, -12.50000000000000000 ) ) ;
#27192 = VERTEX_POINT ( 'NONE', #57403 ) ;
#27193 = DIRECTION ( 'NONE',  ( 0.000000000000000000, -0.1249999999999996531, -0.9921567416492215186 ) ) ;
#27194 = DIRECTION ( 'NONE',  ( -1.000000000000000000, 0.000000000000000000, 0.000000000000000000 ) ) ;
#27195 = ORIENTED_EDGE ( 'NONE', *, *, #53145, .T. ) ;
#27196 = CARTESIAN_POINT ( 'NONE',  ( 7.000000000000000000, -25.50000000000000355, 17.00000000000000000 ) ) ;
#27197 = PLANE ( 'NONE',  #61538 ) ;
#27198 = CYLINDRICAL_SURFACE ( 'NONE', #26443, 0.1749999999999980738 ) ;
#27199 = EDGE_CURVE ( 'NONE', #35627, #50861, #43549, .T. ) ;
#27200 = LINE ( 'NONE', #27885, #4553 ) ;
#27201 = VECTOR ( 'NONE', #18527, 1000.000000000000000 ) ;
#27202 = EDGE_CURVE ( 'NONE', #7815, #13405, #8958, .T. ) ;
#27203 = DIRECTION ( 'NONE',  ( 8.673617379884051249E-15, 1.000000000000000000, 0.000000000000000000 ) ) ;
#27204 = AXIS2_PLACEMENT_3D ( 'NONE', #9591, #64391, #26552 ) ;
#27205 = ORIENTED_EDGE ( 'NONE', *, *, #10823, .T. ) ;
#27206 = ORIENTED_EDGE ( 'NONE', *, *, #21265, .F. ) ;
#27207 = CARTESIAN_POINT ( 'NONE',  ( 13.00000000000000178, -17.50000000000000000, -20.05051025721700242 ) ) ;
#27208 = ORIENTED_EDGE ( 'NONE', *, *, #50949, .F. ) ;
#27209 = CARTESIAN_POINT ( 'NONE',  ( -3.593516549646701197, 7.415254214038210279, 455.0000000000000568 ) ) ;
#27210 = ORIENTED_EDGE ( 'NONE', *, *, #31290, .T. ) ;
#27211 = VECTOR ( 'NONE', #57616, 1000.000000000000000 ) ;
#27212 = LINE ( 'NONE', #38175, #9951 ) ;
#27213 = EDGE_CURVE ( 'NONE', #62873, #56266, #22108, .T. ) ;
#27214 = VECTOR ( 'NONE', #7252, 1000.000000000000000 ) ;
#27215 = VECTOR ( 'NONE', #2747, 1000.000000000000000 ) ;
#27216 = PLANE ( 'NONE',  #6209 ) ;
#27217 = DIRECTION ( 'NONE',  ( 0.7671651518152939886, -0.6414496315691645689, 2.309356642088621864E-17 ) ) ;
#27218 = VERTEX_POINT ( 'NONE', #19925 ) ;
#27219 = VERTEX_POINT ( 'NONE', #25596 ) ;
#27220 = DIRECTION ( 'NONE',  ( 0.000000000000000000, 1.550842787525658429E-12, 1.000000000000000000 ) ) ;
#27221 = ORIENTED_EDGE ( 'NONE', *, *, #63028, .T. ) ;
#27222 = VECTOR ( 'NONE', #35089, 1000.000000000000000 ) ;
#27223 = VERTEX_POINT ( 'NONE', #47161 ) ;
#27224 = CARTESIAN_POINT ( 'NONE',  ( 9.562023737882759278, 2.355476262117158104, 26.00000000000000711 ) ) ;
#27225 = DIRECTION ( 'NONE',  ( 0.000000000000000000, -0.7071067811865474617, -0.7071067811865474617 ) ) ;
#27226 = CARTESIAN_POINT ( 'NONE',  ( -7.517976262117294084, -6.665817930929260449, 54.00000000000000711 ) ) ;
#27227 = ORIENTED_EDGE ( 'NONE', *, *, #40773, .F. ) ;
#27228 = CARTESIAN_POINT ( 'NONE',  ( 15.89999999999999680, -0.1999999999911795112, 8.826273045769999343E-12 ) ) ;
#27229 = CIRCLE ( 'NONE', #58827, 0.3999999999999993006 ) ;
#27231 = CARTESIAN_POINT ( 'NONE',  ( 8.689999999999999503, -8.750000000000000000, -7.000000000000000000 ) ) ;
#27230 = DIRECTION ( 'NONE',  ( 0.7071067811865527908, 0.7071067811865422437, 2.597868168706460875E-16 ) ) ;
#27232 = ORIENTED_EDGE ( 'NONE', *, *, #69213, .F. ) ;
#27233 = ORIENTED_EDGE ( 'NONE', *, *, #19800, .T. ) ;
#27235 = VERTEX_POINT ( 'NONE', #63418 ) ;
#27234 = LINE ( 'NONE', #43475, #7083 ) ;
#27236 = ORIENTED_EDGE ( 'NONE', *, *, #46229, .F. ) ;
#27237 = ADVANCED_FACE ( 'NONE', ( #14982 ), #58110, .F. ) ;
#27238 = CARTESIAN_POINT ( 'NONE',  ( 39.00000000000000000, -16.96999999999999886, -21.00000000000000000 ) ) ;
#27239 = EDGE_CURVE ( 'NONE', #8233, #20681, #9336, .T. ) ;
#27240 = ORIENTED_EDGE ( 'NONE', *, *, #42919, .F. ) ;
#27241 = ORIENTED_EDGE ( 'NONE', *, *, #9099, .T. ) ;
#27242 = ADVANCED_FACE ( 'NONE', ( #37601 ), #65170, .F. ) ;
#27243 = DIRECTION ( 'NONE',  ( -0.8660254037844358210, 0.5000000000000049960, 2.509347957447882735E-16 ) ) ;
#27244 = EDGE_CURVE ( 'NONE', #66711, #2958, #31599, .T. ) ;
#27245 = LINE ( 'NONE', #33229, #14285 ) ;
#27246 = ORIENTED_EDGE ( 'NONE', *, *, #23791, .T. ) ;
#27247 = LINE ( 'NONE', #367, #37632 ) ;
#27248 = DIRECTION ( 'NONE',  ( -1.000000000000000000, 0.000000000000000000, 0.000000000000000000 ) ) ;
#27249 = ADVANCED_FACE ( 'NONE', ( #820 ), #5769, .F. ) ;
#27250 = LINE ( 'NONE', #26905, #39529 ) ;
#27251 = AXIS2_PLACEMENT_3D ( 'NONE', #55589, #61215, #17763 ) ;
#27252 = ORIENTED_EDGE ( 'NONE', *, *, #60429, .T. ) ;
#27253 = CIRCLE ( 'NONE', #67871, 0.1999999999999987899 ) ;
#27254 = DIRECTION ( 'NONE',  ( -0.000000000000000000, 0.000000000000000000, -1.000000000000000000 ) ) ;
#27255 = DIRECTION ( 'NONE',  ( 6.508391731846280553E-15, 1.000000000000000000, 0.000000000000000000 ) ) ;
#27257 = ORIENTED_EDGE ( 'NONE', *, *, #20444, .F. ) ;
#27256 = CARTESIAN_POINT ( 'NONE',  ( 283.0000000000000568, -28.94999999999999929, 13.50000000000000000 ) ) ;
#27259 = ORIENTED_EDGE ( 'NONE', *, *, #55265, .T. ) ;
#27258 = LINE ( 'NONE', #48825, #21037 ) ;
#27260 = CIRCLE ( 'NONE', #4594, 1.000000000000001776 ) ;
#27261 = EDGE_CURVE ( 'NONE', #54344, #68712, #53177, .T. ) ;
#27262 = CARTESIAN_POINT ( 'NONE',  ( 11.00000000000000000, -17.50000000000000000, 60.00000000000000000 ) ) ;
#27263 = CARTESIAN_POINT ( 'NONE',  ( 9.955011587777223170, 2.752095193409229701, 455.0000000000000568 ) ) ;
#27264 = DIRECTION ( 'NONE',  ( 1.000000000000000000, -0.000000000000000000, -0.000000000000000000 ) ) ;
#27265 = CARTESIAN_POINT ( 'NONE',  ( 25.50000000000000355, -5.200000000000001066, -24.50000000000000000 ) ) ;
#27267 = EDGE_CURVE ( 'NONE', #50321, #69402, #10373, .T. ) ;
#27266 = VECTOR ( 'NONE', #46059, 1000.000000000000000 ) ;
#27268 = EDGE_CURVE ( 'NONE', #32145, #23467, #26636, .T. ) ;
#27269 = LINE ( 'NONE', #17325, #47508 ) ;
#27270 = DIRECTION ( 'NONE',  ( -1.000000000000000000, 0.000000000000000000, 0.000000000000000000 ) ) ;
#27271 = VERTEX_POINT ( 'NONE', #59506 ) ;
#27272 = LINE ( 'NONE', #16298, #8970 ) ;
#27273 = VECTOR ( 'NONE', #50237, 1000.000000000000000 ) ;
#27274 = EDGE_CURVE ( 'NONE', #37049, #24763, #20991, .T. ) ;
#27276 = ORIENTED_EDGE ( 'NONE', *, *, #65008, .F. ) ;
#27275 = CARTESIAN_POINT ( 'NONE',  ( -22.14589803375000088, -15.50000000000000000, 21.50000000000000000 ) ) ;
#27278 = ORIENTED_EDGE ( 'NONE', *, *, #1222, .F. ) ;
#27277 = CARTESIAN_POINT ( 'NONE',  ( -6.822336235477446387, 4.135079735113101229, 54.00000000000000711 ) ) ;
#27279 = DIRECTION ( 'NONE',  ( 1.000000000000000000, -0.000000000000000000, -0.000000000000000000 ) ) ;
#27280 = DIRECTION ( 'NONE',  ( -0.6414496315691494699, -0.7671651518153064231, -0.000000000000000000 ) ) ;
#27281 = AXIS2_PLACEMENT_3D ( 'NONE', #2546, #28724, #6805 ) ;
#27282 = ORIENTED_EDGE ( 'NONE', *, *, #4654, .T. ) ;
#27283 = DIRECTION ( 'NONE',  ( 0.000000000000000000, 0.000000000000000000, -1.000000000000000000 ) ) ;
#27284 = DIRECTION ( 'NONE',  ( -0.7671651518153006499, -0.6414496315691565753, 0.000000000000000000 ) ) ;
#27285 = ORIENTED_EDGE ( 'NONE', *, *, #53465, .T. ) ;
#27286 = CARTESIAN_POINT ( 'NONE',  ( 3.157023737882797665, 4.031976262117209053, 54.00000000000000711 ) ) ;
#27287 = DIRECTION ( 'NONE',  ( 1.000000000000000000, 0.000000000000000000, 0.000000000000000000 ) ) ;
#27288 = DIRECTION ( 'NONE',  ( 0.000000000000000000, 0.000000000000000000, -1.000000000000000000 ) ) ;
#27289 = EDGE_CURVE ( 'NONE', #26187, #54496, #21329, .T. ) ;
#27290 = EDGE_CURVE ( 'NONE', #57189, #53303, #53514, .T. ) ;
#27291 = ORIENTED_EDGE ( 'NONE', *, *, #49144, .T. ) ;
#27292 = CARTESIAN_POINT ( 'NONE',  ( -7.450000000000001954, 7.250000000000000000, -15.50000000000000000 ) ) ;
#27293 = ORIENTED_EDGE ( 'NONE', *, *, #20059, .F. ) ;
#27294 = VERTEX_POINT ( 'NONE', #42888 ) ;
#27295 = DIRECTION ( 'NONE',  ( 1.000000000000000000, 0.000000000000000000, 0.000000000000000000 ) ) ;
#27296 = CARTESIAN_POINT ( 'NONE',  ( -30.00000000000000000, -9.199999999999999289, 12.69999999999986073 ) ) ;
#27297 = CARTESIAN_POINT ( 'NONE',  ( -11.31351654964671027, 4.393516549646604652, 455.0000000000000568 ) ) ;
#27298 = LINE ( 'NONE', #48862, #40819 ) ;
#27299 = ORIENTED_EDGE ( 'NONE', *, *, #43925, .T. ) ;
#27300 = ORIENTED_EDGE ( 'NONE', *, *, #2078, .F. ) ;
#27301 = AXIS2_PLACEMENT_3D ( 'NONE', #9599, #63342, #42113 ) ;
#27303 = ORIENTED_EDGE ( 'NONE', *, *, #54718, .T. ) ;
#27302 = CARTESIAN_POINT ( 'NONE',  ( -0.9414762621172249046, 9.915476262117151052, 26.00000000000000711 ) ) ;
#27304 = ORIENTED_EDGE ( 'NONE', *, *, #39736, .T. ) ;
#27305 = CARTESIAN_POINT ( 'NONE',  ( 151.5599459900709860, -10.00000000000000178, 322.4587476295993156 ) ) ;
#27306 = CARTESIAN_POINT ( 'NONE',  ( 30.00000000000000000, -16.28999999999710369, -15.00000000000794920 ) ) ;
#27307 = CARTESIAN_POINT ( 'NONE',  ( 275.0000000000000000, -26.42999999999999972, 9.412893218813501051 ) ) ;
#27308 = CARTESIAN_POINT ( 'NONE',  ( 9.955011587777235604, -9.247904806590801385, 455.0000000000000568 ) ) ;
#27310 = DIRECTION ( 'NONE',  ( -1.000000000000000000, 0.000000000000000000, 0.000000000000000000 ) ) ;
#27309 = DIRECTION ( 'NONE',  ( 0.000000000000000000, -0.000000000000000000, -1.000000000000000000 ) ) ;
#27311 = ORIENTED_EDGE ( 'NONE', *, *, #52429, .T. ) ;
#27313 = EDGE_LOOP ( 'NONE', ( #19640, #1183, #63839, #5054 ) ) ;
#27312 = DIRECTION ( 'NONE',  ( -0.000000000000000000, -0.000000000000000000, -1.000000000000000000 ) ) ;
#27314 = ORIENTED_EDGE ( 'NONE', *, *, #50777, .F. ) ;
#27315 = ORIENTED_EDGE ( 'NONE', *, *, #41991, .T. ) ;
#27316 = AXIS2_PLACEMENT_3D ( 'NONE', #28317, #56237, #7438 ) ;
#27317 = CLOSED_SHELL ( 'NONE', ( #63890, #20155, #15045, #54069, #61868, #9197, #67186, #5025, #20596, #68628 ) ) ;
#27318 = DIRECTION ( 'NONE',  ( -0.000000000000000000, -0.000000000000000000, -1.000000000000000000 ) ) ;
#27319 = LINE ( 'NONE', #42526, #63758 ) ;
#27320 = EDGE_CURVE ( 'NONE', #69663, #32597, #11405, .T. ) ;
#27321 = CARTESIAN_POINT ( 'NONE',  ( -5.655420232009250370, 8.393516549646600211, 195.0000000000000284 ) ) ;
#27322 = VERTEX_POINT ( 'NONE', #48903 ) ;
#27323 = ORIENTED_EDGE ( 'NONE', *, *, #49866, .F. ) ;
#27324 = ORIENTED_EDGE ( 'NONE', *, *, #46603, .F. ) ;
#27325 = EDGE_CURVE ( 'NONE', #13233, #33822, #35655, .T. ) ;
#27327 = CARTESIAN_POINT ( 'NONE',  ( -7.450000000000001954, 7.250000000000000000, -24.50000000000000000 ) ) ;
#27326 = CIRCLE ( 'NONE', #54429, 1.500000000000001332 ) ;
#27328 = CYLINDRICAL_SURFACE ( 'NONE', #2669, 1.499999999997026379 ) ;
#27329 = EDGE_CURVE ( 'NONE', #40687, #27463, #22024, .T. ) ;
#27330 = LINE ( 'NONE', #49245, #58244 ) ;
#27331 = EDGE_CURVE ( 'NONE', #12520, #47907, #26283, .T. ) ;
#27332 = ORIENTED_EDGE ( 'NONE', *, *, #47050, .F. ) ;
#27333 = ORIENTED_EDGE ( 'NONE', *, *, #69494, .T. ) ;
#27334 = PLANE ( 'NONE',  #2312 ) ;
#27335 = APPLICATION_CONTEXT ( 'automotive_design' ) ;
#27336 = EDGE_CURVE ( 'NONE', #21475, #55726, #44687, .T. ) ;
#27337 = EDGE_CURVE ( 'NONE', #65968, #25985, #28887, .T. ) ;
#27338 = DIRECTION ( 'NONE',  ( 0.000000000000000000, 0.000000000000000000, -1.000000000000000000 ) ) ;
#27339 = ORIENTED_EDGE ( 'NONE', *, *, #69272, .F. ) ;
#27340 = ADVANCED_FACE ( 'NONE', ( #121 ), #16367, .T. ) ;
#27341 = CYLINDRICAL_SURFACE ( 'NONE', #18913, 0.2999999999994933941 ) ;
#27343 = ORIENTED_EDGE ( 'NONE', *, *, #28619, .T. ) ;
#27342 = CARTESIAN_POINT ( 'NONE',  ( 19.90000000000000213, -0.1999999999911795112, 8.826273045769999343E-12 ) ) ;
#27344 = EDGE_LOOP ( 'NONE', ( #26002, #51727, #63148, #39474 ) ) ;
#27345 = CARTESIAN_POINT ( 'NONE',  ( 5.668387132715918320, -8.406483450353487541, 455.0000000000000568 ) ) ;
#27346 = DIRECTION ( 'NONE',  ( -1.156482317317873342E-14, -1.000000000000000000, 0.000000000000000000 ) ) ;
#27347 = CARTESIAN_POINT ( 'NONE',  ( 7.272650909786598561, -4.201500623656122535, 455.0000000000000568 ) ) ;
#27348 = CIRCLE ( 'NONE', #66830, 0.9999999999999991118 ) ;
#27349 = CARTESIAN_POINT ( 'NONE',  ( 15.50000000000000000, -5.000000000000000000, -22.50000000000000000 ) ) ;
#27350 = DIRECTION ( 'NONE',  ( -1.053224967557348291E-14, -1.000000000000000000, 0.000000000000000000 ) ) ;
#27351 = VECTOR ( 'NONE', #8811, 1000.000000000000000 ) ;
#27352 = EDGE_LOOP ( 'NONE', ( #11755, #13821, #29596, #19088 ) ) ;
#27353 = DIRECTION ( 'NONE',  ( 0.000000000000000000, 0.000000000000000000, -1.000000000000000000 ) ) ;
#27354 = ORIENTED_EDGE ( 'NONE', *, *, #34068, .T. ) ;
#27355 = CARTESIAN_POINT ( 'NONE',  ( 9.955011587777223170, 9.234937905883922937, 195.0000000000000284 ) ) ;
#27356 = PLANE ( 'NONE',  #22195 ) ;
#27357 = CARTESIAN_POINT ( 'NONE',  ( 3.857023737882779635, -10.31452373788280141, 26.00000000000000000 ) ) ;
#27358 = AXIS2_PLACEMENT_3D ( 'NONE', #7967, #24245, #51112 ) ;
#27359 = FACE_OUTER_BOUND ( 'NONE', #38784, .T. ) ;
#27360 = CARTESIAN_POINT ( 'NONE',  ( -5.242976262117280406, -5.257023737882805747, 54.00000000000000711 ) ) ;
#27361 = EDGE_LOOP ( 'NONE', ( #30599, #65164, #15915, #20877 ) ) ;
#27362 = LINE ( 'NONE', #488, #4291 ) ;
#27363 = AXIS2_PLACEMENT_3D ( 'NONE', #16946, #60068, #11616 ) ;
#27364 = ADVANCED_FACE ( 'NONE', ( #49249 ), #7475, .T. ) ;
#27365 = VECTOR ( 'NONE', #5293, 1000.000000000000114 ) ;
#27366 = ORIENTED_EDGE ( 'NONE', *, *, #65097, .F. ) ;
#27367 = DIRECTION ( 'NONE',  ( 0.000000000000000000, 0.000000000000000000, 1.000000000000000000 ) ) ;
#27368 = DIRECTION ( 'NONE',  ( -1.000000000000000000, 0.000000000000000000, 0.000000000000000000 ) ) ;
#27369 = ADVANCED_FACE ( 'NONE', ( #18080 ), #55923, .F. ) ;
#27370 = VERTEX_POINT ( 'NONE', #45645 ) ;
#27371 = CONICAL_SURFACE ( 'NONE', #13825, 1732.050807568785558, 1.047197551196574761 ) ;
#27372 = DIRECTION ( 'NONE',  ( 0.000000000000000000, 1.000000000000000000, 0.000000000000000000 ) ) ;
#27373 = DIRECTION ( 'NONE',  ( 1.000000000000000000, -0.000000000000000000, 0.000000000000000000 ) ) ;
#27374 = ORIENTED_EDGE ( 'NONE', *, *, #38535, .T. ) ;
#27375 = DIRECTION ( 'NONE',  ( 0.000000000000000000, 0.000000000000000000, 1.000000000000000000 ) ) ;
#27376 = CARTESIAN_POINT ( 'NONE',  ( 12.90000000000000213, 13.66939075806899240, 20.79999999999999361 ) ) ;
#27377 = ADVANCED_FACE ( 'NONE', ( #12765 ), #50964, .T. ) ;
#27378 = DIRECTION ( 'NONE',  ( -0.000000000000000000, -0.000000000000000000, -1.000000000000000000 ) ) ;
#27379 = DIRECTION ( 'NONE',  ( -0.000000000000000000, 3.673940397442059868E-16, -1.000000000000000000 ) ) ;
#27380 = EDGE_LOOP ( 'NONE', ( #55537, #36597, #17530, #33871 ) ) ;
#27382 = EDGE_LOOP ( 'NONE', ( #40343, #43127, #34930, #13927 ) ) ;
#27381 = DIRECTION ( 'NONE',  ( 1.000000000000000000, -0.000000000000000000, 0.000000000000000000 ) ) ;
#27383 = CARTESIAN_POINT ( 'NONE',  ( 8.144523737882812142, 8.821682069070710952, 54.00000000000000711 ) ) ;
#27384 = PLANE ( 'NONE',  #31248 ) ;
#27385 = CARTESIAN_POINT ( 'NONE',  ( 0.000000000000000000, -7.449999999999998401, -20.00000000000000000 ) ) ;
#27386 = ORIENTED_EDGE ( 'NONE', *, *, #22919, .T. ) ;
#27387 = PLANE ( 'NONE',  #53718 ) ;
#27388 = DIRECTION ( 'NONE',  ( 1.836970198721029934E-16, 1.836970198721010706E-16, -1.000000000000000000 ) ) ;
#27389 = CIRCLE ( 'NONE', #45430, 0.1999999999999987899 ) ;
#27390 = VERTEX_POINT ( 'NONE', #22712 ) ;
#27391 = ORIENTED_EDGE ( 'NONE', *, *, #19308, .F. ) ;
#27392 = ORIENTED_EDGE ( 'NONE', *, *, #66259, .F. ) ;
#27393 = AXIS2_PLACEMENT_3D ( 'NONE', #66298, #65277, #16824 ) ;
#27394 = DIRECTION ( 'NONE',  ( 0.8660254037844401509, 0.4999999999999973910, 0.000000000000000000 ) ) ;
#27395 = CARTESIAN_POINT ( 'NONE',  ( -8.689999999999999503, 8.750000000000000000, -5.000000000000000000 ) ) ;
#27396 =( NAMED_UNIT ( * ) SI_UNIT ( $, .STERADIAN. ) SOLID_ANGLE_UNIT ( ) );
#27397 = EDGE_CURVE ( 'NONE', #17943, #67681, #29389, .T. ) ;
#27398 = VERTEX_POINT ( 'NONE', #66868 ) ;
#27399 = EDGE_LOOP ( 'NONE', ( #39024, #53183 ) ) ;
#27400 = VERTEX_POINT ( 'NONE', #49582 ) ;
#27401 = CARTESIAN_POINT ( 'NONE',  ( -2.989207322240185594, 6.858227778582772771, 26.00000000000000711 ) ) ;
#27402 = ORIENTED_EDGE ( 'NONE', *, *, #17279, .T. ) ;
#27403 = ORIENTED_EDGE ( 'NONE', *, *, #5486, .T. ) ;
#27404 = VERTEX_POINT ( 'NONE', #1148 ) ;
#27405 = VERTEX_POINT ( 'NONE', #44262 ) ;
#27406 = CARTESIAN_POINT ( 'NONE',  ( 8.835729544836338434, -2.369523737882826886, 54.00000000000000711 ) ) ;
#27407 = UNCERTAINTY_MEASURE_WITH_UNIT (LENGTH_MEASURE( 1.000000000000000082E-05 ), #64992, 'distance_accuracy_value', 'NONE');
#27408 = ADVANCED_FACE ( 'NONE', ( #34694 ), #7122, .F. ) ;
#27409 = EDGE_CURVE ( 'NONE', #15324, #59398, #66189, .T. ) ;
#27411 = VERTEX_POINT ( 'NONE', #65842 ) ;
#27410 = CARTESIAN_POINT ( 'NONE',  ( 5.393625297349901260, -4.747751991980754482, 455.0000000000000568 ) ) ;
#27412 = CARTESIAN_POINT ( 'NONE',  ( -8.566576262117358453, -9.703773737882738004, 54.00000000000000711 ) ) ;
#27413 = DIRECTION ( 'NONE',  ( 0.000000000000000000, 0.000000000000000000, -1.000000000000000000 ) ) ;
#27414 = EDGE_CURVE ( 'NONE', #27500, #33822, #24089, .T. ) ;
#27415 = DIRECTION ( 'NONE',  ( -1.000000000000000000, 3.903627567395476653E-15, 1.836970198721037083E-16 ) ) ;
#27416 = VERTEX_POINT ( 'NONE', #38968 ) ;
#27417 = VECTOR ( 'NONE', #65947, 1000.000000000000000 ) ;
#27418 = VECTOR ( 'NONE', #51665, 1000.000000000000000 ) ;
#27419 = DIRECTION ( 'NONE',  ( -1.000000000000000000, 0.000000000000000000, 0.000000000000000000 ) ) ;
#27420 = VECTOR ( 'NONE', #2455, 1000.000000000000000 ) ;
#27421 = VERTEX_POINT ( 'NONE', #28350 ) ;
#27422 = LINE ( 'NONE', #31073, #39351 ) ;
#27423 = CYLINDRICAL_SURFACE ( 'NONE', #45609, 24.99999999998794920 ) ;
#27424 = AXIS2_PLACEMENT_3D ( 'NONE', #7817, #50618, #2519 ) ;
#27425 = DIRECTION ( 'NONE',  ( 0.000000000000000000, 1.000000000000000000, 0.000000000000000000 ) ) ;
#27426 = DIRECTION ( 'NONE',  ( -0.000000000000000000, 0.000000000000000000, 1.000000000000000000 ) ) ;
#27427 = ORIENTED_EDGE ( 'NONE', *, *, #16809, .T. ) ;
#27428 = DIRECTION ( 'NONE',  ( 1.000000000000000000, -0.000000000000000000, 0.000000000000000000 ) ) ;
#27429 = CARTESIAN_POINT ( 'NONE',  ( 6.501044194225490180, -2.632023737882825287, 54.00000000000000711 ) ) ;
#27430 = CARTESIAN_POINT ( 'NONE',  ( 30.00000000000000000, -17.50000000000000000, -15.70500000000000007 ) ) ;
#27431 = VECTOR ( 'NONE', #66999, 1000.000000000000000 ) ;
#27432 = CYLINDRICAL_SURFACE ( 'NONE', #65868, 4.500000000000189182 ) ;
#27433 = DIRECTION ( 'NONE',  ( -1.000000000000000000, 0.000000000000000000, 0.000000000000000000 ) ) ;
#27434 = CARTESIAN_POINT ( 'NONE',  ( 30.00000000000000000, -16.64230188589299786, -14.64519951917100116 ) ) ;
#27435 = CIRCLE ( 'NONE', #235, 0.2000000000000000944 ) ;
#27436 = CARTESIAN_POINT ( 'NONE',  ( 8.612468434717182930, 1.466476262117163865, 54.00000000000000711 ) ) ;
#27437 = DIRECTION ( 'NONE',  ( 0.000000000000000000, 1.000000000000000000, 0.000000000000000000 ) ) ;
#27438 = VERTEX_POINT ( 'NONE', #2179 ) ;
#27439 = PLANE ( 'NONE',  #41739 ) ;
#27440 = CARTESIAN_POINT ( 'NONE',  ( 9.703773737882810835, 8.916576262117189344, 26.00000000000000711 ) ) ;
#27441 = CIRCLE ( 'NONE', #42081, 4.000000000000000888 ) ;
#27442 = EDGE_CURVE ( 'NONE', #68810, #8098, #23406, .T. ) ;
#27443 = ADVANCED_FACE ( 'NONE', ( #23744 ), #7819, .F. ) ;
#27444 = EDGE_CURVE ( 'NONE', #10558, #46985, #55657, .T. ) ;
#27445 = LINE ( 'NONE', #17171, #15446 ) ;
#27446 = DIRECTION ( 'NONE',  ( -0.000000000000000000, -0.000000000000000000, 1.000000000000000000 ) ) ;
#27447 = ORIENTED_EDGE ( 'NONE', *, *, #38108, .T. ) ;
#27448 = DIRECTION ( 'NONE',  ( 1.000000000000000000, 2.135044278125301343E-15, -0.000000000000000000 ) ) ;
#27449 = DIRECTION ( 'NONE',  ( 0.7071067811865474617, -0.7071067811865474617, 0.000000000000000000 ) ) ;
#27450 = CARTESIAN_POINT ( 'NONE',  ( 7.250000000000005329, -8.249999999999998224, -26.00000000000001066 ) ) ;
#27451 = EDGE_CURVE ( 'NONE', #42528, #12808, #24911, .T. ) ;
#27452 = DIRECTION ( 'NONE',  ( 0.000000000000000000, 0.000000000000000000, -1.000000000000000000 ) ) ;
#27453 = LINE ( 'NONE', #23178, #67017 ) ;
#27454 = PLANE ( 'NONE',  #1214 ) ;
#27455 = VERTEX_POINT ( 'NONE', #1478 ) ;
#27456 = AXIS2_PLACEMENT_3D ( 'NONE', #39622, #39961, #17036 ) ;
#27457 = ORIENTED_EDGE ( 'NONE', *, *, #44717, .F. ) ;
#27458 = FACE_OUTER_BOUND ( 'NONE', #12568, .T. ) ;
#27459 = DIRECTION ( 'NONE',  ( -1.000000000000000000, 0.000000000000000000, 0.000000000000000000 ) ) ;
#27460 = ORIENTED_EDGE ( 'NONE', *, *, #62178, .F. ) ;
#27461 = VECTOR ( 'NONE', #22337, 1000.000000000000000 ) ;
#27462 = CARTESIAN_POINT ( 'NONE',  ( 40.90000000000000568, 16.96999999999999886, -21.00000000000000000 ) ) ;
#27463 = VERTEX_POINT ( 'NONE', #23046 ) ;
#27464 = DIRECTION ( 'NONE',  ( 1.671920889371702657E-15, -1.000000000000000000, 0.000000000000000000 ) ) ;
#27466 = EDGE_LOOP ( 'NONE', ( #8815, #55228, #27354, #20353 ) ) ;
#27465 = MECHANICAL_DESIGN_GEOMETRIC_PRESENTATION_REPRESENTATION (  '', ( #7153 ), #6024 ) ;
#27467 = AXIS2_PLACEMENT_3D ( 'NONE', #61054, #18269, #12265 ) ;
#27468 = VERTEX_POINT ( 'NONE', #44600 ) ;
#27469 = DIRECTION ( 'NONE',  ( 0.000000000000000000, -0.9239212585478300266, -0.3825826812643171038 ) ) ;
#27470 = ORIENTED_EDGE ( 'NONE', *, *, #46084, .F. ) ;
#27471 = DIRECTION ( 'NONE',  ( 1.000000000000000000, 0.000000000000000000, 0.000000000000000000 ) ) ;
#27472 = LINE ( 'NONE', #49043, #32736 ) ;
#27473 = CARTESIAN_POINT ( 'NONE',  ( -9.234937905884079257, -9.955011587777201854, 195.0000000000000284 ) ) ;
#27474 = ORIENTED_EDGE ( 'NONE', *, *, #39095, .T. ) ;
#27475 = ORIENTED_EDGE ( 'NONE', *, *, #7650, .T. ) ;
#27476 = PLANE ( 'NONE',  #24482 ) ;
#27477 = DIRECTION ( 'NONE',  ( 1.836970198721029934E-16, -1.836970198721036344E-16, 1.000000000000000000 ) ) ;
#27478 = ORIENTED_EDGE ( 'NONE', *, *, #58241, .T. ) ;
#27479 = AXIS2_PLACEMENT_3D ( 'NONE', #13874, #52789, #4345 ) ;
#27480 = ORIENTED_EDGE ( 'NONE', *, *, #29222, .F. ) ;
#27481 = VERTEX_POINT ( 'NONE', #12419 ) ;
#27482 = PLANE ( 'NONE',  #52547 ) ;
#27483 = VECTOR ( 'NONE', #69234, 1000.000000000000000 ) ;
#27485 = ORIENTED_EDGE ( 'NONE', *, *, #58156, .F. ) ;
#27484 = LINE ( 'NONE', #38118, #44274 ) ;
#27486 = EDGE_CURVE ( 'NONE', #42614, #24441, #64455, .T. ) ;
#27487 = CARTESIAN_POINT ( 'NONE',  ( 8.250000000000005329, 7.250000000000000888, -12.00000000000000000 ) ) ;
#27488 = CARTESIAN_POINT ( 'NONE',  ( -2.406732575409671337, -8.711985858128709737, 54.00000000000000711 ) ) ;
#27489 = EDGE_CURVE ( 'NONE', #67902, #31344, #44962, .T. ) ;
#27490 = ORIENTED_EDGE ( 'NONE', *, *, #14800, .T. ) ;
#27491 = EDGE_CURVE ( 'NONE', #26513, #22437, #33928, .T. ) ;
#27492 = ORIENTED_EDGE ( 'NONE', *, *, #13965, .T. ) ;
#27493 = AXIS2_PLACEMENT_3D ( 'NONE', #40942, #46951, #24693 ) ;
#27494 = EDGE_CURVE ( 'NONE', #13213, #50319, #68281, .T. ) ;
#27495 = VERTEX_POINT ( 'NONE', #57669 ) ;
#27496 = CARTESIAN_POINT ( 'NONE',  ( -9.390476262117209316, -1.480523737882732060, 54.00000000000000711 ) ) ;
#27497 = DIRECTION ( 'NONE',  ( 0.7071067811865474617, -0.7071067811865474617, 0.000000000000000000 ) ) ;
#27498 = ADVANCED_FACE ( 'NONE', ( #47068 ), #35039, .T. ) ;
#27499 = EDGE_CURVE ( 'NONE', #38679, #62810, #35386, .T. ) ;
#27500 = VERTEX_POINT ( 'NONE', #51310 ) ;
#27501 = ADVANCED_FACE ( 'NONE', ( #24447 ), #56957, .F. ) ;
#27502 = CIRCLE ( 'NONE', #59155, 1.000000000000000888 ) ;
#27503 = AXIS2_PLACEMENT_3D ( 'NONE', #45449, #24246, #12918 ) ;
#27504 = DIRECTION ( 'NONE',  ( 0.000000000000000000, 0.000000000000000000, -1.000000000000000000 ) ) ;
#27505 = FACE_OUTER_BOUND ( 'NONE', #55791, .T. ) ;
#27507 = ORIENTED_EDGE ( 'NONE', *, *, #16798, .F. ) ;
#27506 = CARTESIAN_POINT ( 'NONE',  ( 3.677663764522620671, 4.135079735113112775, 54.00000000000000711 ) ) ;
#27508 = VERTEX_POINT ( 'NONE', #41403 ) ;
#27509 = CARTESIAN_POINT ( 'NONE',  ( 7.250000000000005329, 7.250000000000000888, -16.50000000000000000 ) ) ;
#27510 =( GEOMETRIC_REPRESENTATION_CONTEXT ( 3 ) GLOBAL_UNCERTAINTY_ASSIGNED_CONTEXT ( ( #36617 ) ) GLOBAL_UNIT_ASSIGNED_CONTEXT ( ( #51449, #19272, #40483 ) ) REPRESENTATION_CONTEXT ( 'NONE', 'WORKASPACE' ) );
#27512 = VECTOR ( 'NONE', #26620, 1000.000000000000000 ) ;
#27511 = CARTESIAN_POINT ( 'NONE',  ( -11.31351654964674047, -4.206483450353332820, 455.0000000000000568 ) ) ;
#27513 = PLANE ( 'NONE',  #26824 ) ;
#27514 = DIRECTION ( 'NONE',  ( 0.000000000000000000, -1.000000000000000000, 0.000000000000000000 ) ) ;
#27515 = VECTOR ( 'NONE', #23022, 1000.000000000000000 ) ;
#27516 = DIRECTION ( 'NONE',  ( -0.7071067811865401342, 0.7071067811865550112, 1.355854680848613865E-30 ) ) ;
#27517 = VERTEX_POINT ( 'NONE', #30097 ) ;
#27518 = DIRECTION ( 'NONE',  ( 0.000000000000000000, 0.000000000000000000, -1.000000000000000000 ) ) ;
#27519 = FACE_OUTER_BOUND ( 'NONE', #2598, .T. ) ;
#27520 = DIRECTION ( 'NONE',  ( -0.000000000000000000, -0.000000000000000000, -1.000000000000000000 ) ) ;
#27522 = VERTEX_POINT ( 'NONE', #46012 ) ;
#27521 = DIRECTION ( 'NONE',  ( 0.000000000000000000, -0.7071067811865475727, -0.7071067811865475727 ) ) ;
#27523 = DIRECTION ( 'NONE',  ( 1.047444401652940007E-14, 1.000000000000000000, 1.836970198721029934E-16 ) ) ;
#27524 = FACE_OUTER_BOUND ( 'NONE', #10871, .T. ) ;
#27525 = DIRECTION ( 'NONE',  ( 0.000000000000000000, 0.000000000000000000, 1.000000000000000000 ) ) ;
#27526 = DIRECTION ( 'NONE',  ( -0.000000000000000000, -0.000000000000000000, -1.000000000000000000 ) ) ;
#27527 = ORIENTED_EDGE ( 'NONE', *, *, #21505, .F. ) ;
#27528 = CYLINDRICAL_SURFACE ( 'NONE', #6108, 0.5000000000000000000 ) ;
#27529 = CARTESIAN_POINT ( 'NONE',  ( -7.250000000000000000, -7.449999999999998401, -24.50000000000000000 ) ) ;
#27530 = ORIENTED_EDGE ( 'NONE', *, *, #19469, .F. ) ;
#27531 = CARTESIAN_POINT ( 'NONE',  ( 7.606483450353380249, -11.32648345035348925, 455.0000000000000568 ) ) ;
#27532 = DIRECTION ( 'NONE',  ( 0.000000000000000000, 0.000000000000000000, -1.000000000000000000 ) ) ;
#27533 = DIRECTION ( 'NONE',  ( 0.000000000000000000, 0.000000000000000000, -1.000000000000000000 ) ) ;
#27534 = CARTESIAN_POINT ( 'NONE',  ( 176.4833316329832940, 0.000000000000000000, 324.6739988703752715 ) ) ;
#27535 = CARTESIAN_POINT ( 'NONE',  ( 41.09999999999999432, -14.06939075806900163, 20.80000000000000426 ) ) ;
#27536 = DIRECTION ( 'NONE',  ( -0.8660254037844358210, 0.5000000000000049960, 2.509347957447882735E-16 ) ) ;
#27537 = EDGE_LOOP ( 'NONE', ( #452, #25024, #29973, #9342 ) ) ;
#27538 = DIRECTION ( 'NONE',  ( 0.000000000000000000, 0.000000000000000000, 1.000000000000000000 ) ) ;
#27539 = DIRECTION ( 'NONE',  ( 0.000000000000000000, 1.000000000000000000, 0.000000000000000000 ) ) ;
#27540 = ORIENTED_EDGE ( 'NONE', *, *, #21550, .T. ) ;
#27541 = VECTOR ( 'NONE', #66311, 1000.000000000000000 ) ;
#27542 = DIRECTION ( 'NONE',  ( 1.000000000000000000, -0.000000000000000000, -0.000000000000000000 ) ) ;
#27543 = EDGE_CURVE ( 'NONE', #51391, #22759, #25858, .T. ) ;
#27544 = CARTESIAN_POINT ( 'NONE',  ( 11.00000000000000000, -9.487228132326899654, -12.50000000000000000 ) ) ;
#27545 = EDGE_CURVE ( 'NONE', #20854, #53303, #57320, .T. ) ;
#27546 = CYLINDRICAL_SURFACE ( 'NONE', #29898, 0.5249999999999994671 ) ;
#27547 = ORIENTED_EDGE ( 'NONE', *, *, #19327, .T. ) ;
#27548 = ORIENTED_EDGE ( 'NONE', *, *, #12459, .T. ) ;
#27549 = DIRECTION ( 'NONE',  ( -0.000000000000000000, 3.673940397442059868E-16, -1.000000000000000000 ) ) ;
#27550 = ORIENTED_EDGE ( 'NONE', *, *, #10878, .T. ) ;
#27551 = ORIENTED_EDGE ( 'NONE', *, *, #9925, .F. ) ;
#27552 = PLANE ( 'NONE',  #12321 ) ;
#27553 = FACE_OUTER_BOUND ( 'NONE', #21938, .T. ) ;
#27554 = AXIS2_PLACEMENT_3D ( 'NONE', #3880, #41345, #53030 ) ;
#27555 = AXIS2_PLACEMENT_3D ( 'NONE', #39376, #34058, #55994 ) ;
#27556 = CARTESIAN_POINT ( 'NONE',  ( 49.00000000000000000, 20.60000000000000142, -13.86939075806900057 ) ) ;
#27557 = EDGE_CURVE ( 'NONE', #5241, #42070, #46356, .T. ) ;
#27558 = ORIENTED_EDGE ( 'NONE', *, *, #63468, .T. ) ;
#27559 = LINE ( 'NONE', #16958, #61665 ) ;
#27561 = CARTESIAN_POINT ( 'NONE',  ( 37.90000000000000568, 20.60000000000000142, 13.86939075806899702 ) ) ;
#27560 = CARTESIAN_POINT ( 'NONE',  ( 5.257023737882801306, 5.242976262117200470, 54.00000000000000711 ) ) ;
#27562 = VERTEX_POINT ( 'NONE', #46355 ) ;
#27563 = AXIS2_PLACEMENT_3D ( 'NONE', #19185, #13528, #40403 ) ;
#27565 = EDGE_LOOP ( 'NONE', ( #14895, #1170 ) ) ;
#27564 = VECTOR ( 'NONE', #68202, 1000.000000000000000 ) ;
#27567 = ORIENTED_EDGE ( 'NONE', *, *, #1277, .T. ) ;
#27566 = CARTESIAN_POINT ( 'NONE',  ( 1.000000000000000000, -21.00000000000000000, 5.000000000000000000 ) ) ;
#27568 = ORIENTED_EDGE ( 'NONE', *, *, #24696, .T. ) ;
#27569 = ADVANCED_FACE ( 'NONE', ( #56620 ), #62979, .T. ) ;
#27570 = AXIS2_PLACEMENT_3D ( 'NONE', #35351, #3558, #9213 ) ;
#27571 = CARTESIAN_POINT ( 'NONE',  ( 25.50000000000000355, -15.50000000000000000, 22.50000000000000000 ) ) ;
#27572 = CYLINDRICAL_SURFACE ( 'NONE', #44955, 0.1999999999999996503 ) ;
#27573 = EDGE_CURVE ( 'NONE', #50027, #67161, #26036, .T. ) ;
#27574 = ORIENTED_EDGE ( 'NONE', *, *, #39676, .F. ) ;
#27575 = ORIENTED_EDGE ( 'NONE', *, *, #6484, .T. ) ;
#27576 = AXIS2_PLACEMENT_3D ( 'NONE', #53489, #19902, #63393 ) ;
#27577 = CARTESIAN_POINT ( 'NONE',  ( 2.765062094116107705, 9.942044687070449527, 455.0000000000000568 ) ) ;
#27578 = CARTESIAN_POINT ( 'NONE',  ( 283.0000000000000568, -32.95000000000000284, 7.700000000000000178 ) ) ;
#27579 = ORIENTED_EDGE ( 'NONE', *, *, #63756, .T. ) ;
#27580 = CARTESIAN_POINT ( 'NONE',  ( 4.720772854004774643, -6.358413763958961518, 26.00000000000000711 ) ) ;
#27581 = CYLINDRICAL_SURFACE ( 'NONE', #10908, 24.99999999998789946 ) ;
#27582 = EDGE_CURVE ( 'NONE', #2319, #64180, #67931, .T. ) ;
#27583 = PLANE ( 'NONE',  #35040 ) ;
#27584 = VERTEX_POINT ( 'NONE', #9237 ) ;
#27585 = EDGE_CURVE ( 'NONE', #57888, #40026, #60981, .T. ) ;
#27586 = DIRECTION ( 'NONE',  ( -0.000000000000000000, 1.000000000000000000, -0.000000000000000000 ) ) ;
#27587 = PLANE ( 'NONE',  #59939 ) ;
#27588 = CIRCLE ( 'NONE', #12872, 0.1999999999999987899 ) ;
#27589 = ORIENTED_EDGE ( 'NONE', *, *, #52193, .F. ) ;
#27591 = VERTEX_POINT ( 'NONE', #14184 ) ;
#27590 = CARTESIAN_POINT ( 'NONE',  ( -6.350872789121327244, 3.663616288756986084, 54.00000000000000711 ) ) ;
#27592 = DIRECTION ( 'NONE',  ( -0.000000000000000000, -0.000000000000000000, -1.000000000000000000 ) ) ;
#27593 = CARTESIAN_POINT ( 'NONE',  ( 30.00000000000000000, -16.64230188589299786, -14.64519951917100116 ) ) ;
#27594 = EDGE_CURVE ( 'NONE', #59384, #26720, #44087, .T. ) ;
#27595 = AXIS2_PLACEMENT_3D ( 'NONE', #23599, #44817, #34198 ) ;
#27596 = PLANE ( 'NONE',  #42565 ) ;
#27597 = DIRECTION ( 'NONE',  ( -0.000000000000000000, 3.673940397442059868E-16, -1.000000000000000000 ) ) ;
#27598 = CARTESIAN_POINT ( 'NONE',  ( 7.250000000000005329, -8.749999999999998224, -26.00000000000001066 ) ) ;
#27599 = PLANE ( 'NONE',  #59775 ) ;
#27600 = ORIENTED_EDGE ( 'NONE', *, *, #44528, .T. ) ;
#27601 = DIRECTION ( 'NONE',  ( 1.836970198721029934E-16, 1.836970198721010706E-16, -1.000000000000000000 ) ) ;
#27603 = ORIENTED_EDGE ( 'NONE', *, *, #28561, .T. ) ;
#27602 = DIRECTION ( 'NONE',  ( 0.000000000000000000, 1.000000000000000000, 0.000000000000000000 ) ) ;
#27605 = ORIENTED_EDGE ( 'NONE', *, *, #3313, .T. ) ;
#27604 = CARTESIAN_POINT ( 'NONE',  ( -10.03972626211722918, 9.689726262117183353, 54.00000000000000711 ) ) ;
#27606 = VECTOR ( 'NONE', #17174, 1000.000000000000000 ) ;
#27607 = VECTOR ( 'NONE', #62332, 1000.000000000000000 ) ;
#27608 = CARTESIAN_POINT ( 'NONE',  ( -7.250000000000000888, 8.250000000000001776, -8.000000000000000000 ) ) ;
#27609 = CARTESIAN_POINT ( 'NONE',  ( 7.000000000000000000, -32.95000000000000284, -14.50000000000000000 ) ) ;
#27610 = MECHANICAL_DESIGN_GEOMETRIC_PRESENTATION_REPRESENTATION (  '', ( #5057 ), #61447 ) ;
#27611 = VECTOR ( 'NONE', #48920, 1000.000000000000114 ) ;
#27612 = ORIENTED_EDGE ( 'NONE', *, *, #41288, .F. ) ;
#27613 = CARTESIAN_POINT ( 'NONE',  ( 30.90000000000000213, -21.00000000000001421, -13.86939075806900945 ) ) ;
#27614 = CARTESIAN_POINT ( 'NONE',  ( -8.250000000000001776, 0.000000000000000000, -22.50000000000000000 ) ) ;
#27615 = VERTEX_POINT ( 'NONE', #19834 ) ;
#27616 = ADVANCED_FACE ( 'NONE', ( #3585 ), #68639, .F. ) ;
#27617 = DIRECTION ( 'NONE',  ( 0.000000000000000000, 0.000000000000000000, 1.000000000000000000 ) ) ;
#27618 = PLANE ( 'NONE',  #48496 ) ;
#27619 = VECTOR ( 'NONE', #55813, 1000.000000000000000 ) ;
#27620 = DIRECTION ( 'NONE',  ( 1.000000000000000000, 0.000000000000000000, 0.000000000000000000 ) ) ;
#27621 = EDGE_CURVE ( 'NONE', #53055, #22100, #20189, .T. ) ;
#27622 = ORIENTED_EDGE ( 'NONE', *, *, #61633, .F. ) ;
#27623 = LINE ( 'NONE', #42498, #22565 ) ;
#27624 = VERTEX_POINT ( 'NONE', #36095 ) ;
#27625 = ADVANCED_FACE ( 'NONE', ( #3936 ), #41751, .T. ) ;
#27626 = VERTEX_POINT ( 'NONE', #42803 ) ;
#27627 = VECTOR ( 'NONE', #18767, 1000.000000000000000 ) ;
#27628 = DIRECTION ( 'NONE',  ( -2.135044278125299371E-15, -1.000000000000000000, -3.673940397442060361E-16 ) ) ;
#27629 = DIRECTION ( 'NONE',  ( 0.000000000000000000, 0.000000000000000000, -1.000000000000000000 ) ) ;
#27630 = EDGE_CURVE ( 'NONE', #45832, #6981, #65550, .T. ) ;
#27631 = CARTESIAN_POINT ( 'NONE',  ( 7.000000000000000000, -25.50000000000000355, 16.03137303340311348 ) ) ;
#27632 = EDGE_CURVE ( 'NONE', #67039, #6107, #11314, .T. ) ;
#27633 = LINE ( 'NONE', #38596, #67927 ) ;
#27634 = ORIENTED_EDGE ( 'NONE', *, *, #20152, .F. ) ;
#27635 = EDGE_LOOP ( 'NONE', ( #65390, #63594, #61958, #69021 ) ) ;
#27637 = EDGE_LOOP ( 'NONE', ( #5206, #14158, #36960, #60797, #66195, #67147 ) ) ;
#27636 = CARTESIAN_POINT ( 'NONE',  ( 30.00000000000000000, -11.70000000000000284, -11.00000000000000000 ) ) ;
#27638 = VERTEX_POINT ( 'NONE', #32889 ) ;
#27639 = CARTESIAN_POINT ( 'NONE',  ( -7.450000000000001954, 0.000000000000000000, -9.500000000000001776 ) ) ;
#27640 = DIRECTION ( 'NONE',  ( 0.000000000000000000, 1.000000000000000000, 0.000000000000000000 ) ) ;
#27641 = CARTESIAN_POINT ( 'NONE',  ( -25.50000000000000355, -15.50000000000000000, 20.49999999999999645 ) ) ;
#27642 = EDGE_CURVE ( 'NONE', #9826, #13193, #31862, .T. ) ;
#27643 = VECTOR ( 'NONE', #56580, 1000.000000000000000 ) ;
#27644 = EDGE_CURVE ( 'NONE', #20195, #22032, #69328, .T. ) ;
#27645 = FACE_OUTER_BOUND ( 'NONE', #53309, .T. ) ;
#27647 = DIRECTION ( 'NONE',  ( 0.7671651518153131954, 0.6414496315691415873, 2.587583378555109562E-16 ) ) ;
#27646 = LINE ( 'NONE', #49227, #7215 ) ;
#27648 = ORIENTED_EDGE ( 'NONE', *, *, #38493, .F. ) ;
#27650 = ORIENTED_EDGE ( 'NONE', *, *, #43928, .F. ) ;
#27649 = CARTESIAN_POINT ( 'NONE',  ( -7.250000000000000000, -7.449999999999998401, -21.50000000000000000 ) ) ;
#27651 = VECTOR ( 'NONE', #68504, 1000.000000000000227 ) ;
#27652 = VERTEX_POINT ( 'NONE', #5345 ) ;
#27653 = ORIENTED_EDGE ( 'NONE', *, *, #33208, .T. ) ;
#27654 = EDGE_CURVE ( 'NONE', #36357, #2916, #26547, .T. ) ;
#27655 = EDGE_CURVE ( 'NONE', #18488, #27508, #19253, .T. ) ;
#27656 = DIRECTION ( 'NONE',  ( 0.000000000000000000, 0.000000000000000000, 1.000000000000000000 ) ) ;
#27657 = DIRECTION ( 'NONE',  ( 0.000000000000000000, 0.000000000000000000, -1.000000000000000000 ) ) ;
#27658 = EDGE_CURVE ( 'NONE', #1406, #191, #16279, .T. ) ;
#27660 = CARTESIAN_POINT ( 'NONE',  ( 6.849523737882814878, 10.49297626211720136, 26.00000000000000711 ) ) ;
#27659 = AXIS2_PLACEMENT_3D ( 'NONE', #4970, #43478, #64707 ) ;
#27661 = ORIENTED_EDGE ( 'NONE', *, *, #16818, .F. ) ;
#27662 = ORIENTED_EDGE ( 'NONE', *, *, #40706, .F. ) ;
#27663 = VECTOR ( 'NONE', #17289, 1000.000000000000000 ) ;
#27664 = AXIS2_PLACEMENT_3D ( 'NONE', #26872, #43812, #22588 ) ;
#27665 = LINE ( 'NONE', #43577, #30906 ) ;
#27666 = DIRECTION ( 'NONE',  ( 1.000000000000000000, 0.000000000000000000, 0.000000000000000000 ) ) ;
#27667 = ORIENTED_EDGE ( 'NONE', *, *, #37514, .F. ) ;
#27668 = VERTEX_POINT ( 'NONE', #21250 ) ;
#27669 = CARTESIAN_POINT ( 'NONE',  ( 28.00000000000000000, -15.50000000000000000, 14.50000000000000000 ) ) ;
#27670 = VECTOR ( 'NONE', #27318, 1000.000000000000000 ) ;
#27671 = ADVANCED_FACE ( 'NONE', ( #38214 ), #27583, .F. ) ;
#27672 = DIRECTION ( 'NONE',  ( 0.000000000000000000, 0.000000000000000000, 1.000000000000000000 ) ) ;
#27673 = ORIENTED_EDGE ( 'NONE', *, *, #38285, .F. ) ;
#27674 = ADVANCED_FACE ( 'NONE', ( #64722 ), #49155, .F. ) ;
#27675 = AXIS2_PLACEMENT_3D ( 'NONE', #53625, #37361, #38064 ) ;
#27676 = DIRECTION ( 'NONE',  ( 0.000000000000000000, -1.000000000000000000, 0.000000000000000000 ) ) ;
#27677 = VECTOR ( 'NONE', #11747, 1000.000000000000000 ) ;
#27679 = VERTEX_POINT ( 'NONE', #59068 ) ;
#27678 = CARTESIAN_POINT ( 'NONE',  ( -4.393516549646832914, -11.32648345035344128, 455.0000000000000568 ) ) ;
#27680 = VECTOR ( 'NONE', #37347, 1000.000000000000114 ) ;
#27681 = ORIENTED_EDGE ( 'NONE', *, *, #63650, .T. ) ;
#27682 = DIRECTION ( 'NONE',  ( 0.000000000000000000, -0.1249999999999996531, -0.9921567416492215186 ) ) ;
#27683 = DIRECTION ( 'NONE',  ( 0.000000000000000000, 1.000000000000000000, 0.000000000000000000 ) ) ;
#27684 = DIRECTION ( 'NONE',  ( 0.7671651518153006499, 0.6414496315691565753, 0.000000000000000000 ) ) ;
#27685 = DIRECTION ( 'NONE',  ( 1.000000000000000000, 0.000000000000000000, 0.000000000000000000 ) ) ;
#27686 = DIRECTION ( 'NONE',  ( -1.000000000000000000, 0.000000000000000000, 0.000000000000000000 ) ) ;
#27687 = ORIENTED_EDGE ( 'NONE', *, *, #18257, .F. ) ;
#27688 = LINE ( 'NONE', #60549, #27008 ) ;
#27690 = ORIENTED_EDGE ( 'NONE', *, *, #31980, .F. ) ;
#27689 = LINE ( 'NONE', #49267, #59323 ) ;
#27691 = DIRECTION ( 'NONE',  ( 1.000000000000000000, -0.000000000000000000, -0.000000000000000000 ) ) ;
#27692 = EDGE_CURVE ( 'NONE', #29909, #41212, #58389, .T. ) ;
#27693 = DIRECTION ( 'NONE',  ( -0.000000000000000000, 3.673940397442059868E-16, -1.000000000000000000 ) ) ;
#27694 = DIRECTION ( 'NONE',  ( 1.000000000000000000, 0.000000000000000000, 0.000000000000000000 ) ) ;
#27695 = CARTESIAN_POINT ( 'NONE',  ( 2.706483450353419862, 10.91351654964658735, 455.0000000000000568 ) ) ;
#27696 = FACE_OUTER_BOUND ( 'NONE', #21640, .T. ) ;
#27697 = CIRCLE ( 'NONE', #67206, 3.499999999999041655 ) ;
#27698 = VERTEX_POINT ( 'NONE', #31516 ) ;
#27699 = ORIENTED_EDGE ( 'NONE', *, *, #11643, .F. ) ;
#27700 = VECTOR ( 'NONE', #16226, 1000.000000000000000 ) ;
#27701 = CARTESIAN_POINT ( 'NONE',  ( -13.00000000000000178, -16.64230188589300141, 14.64519951917099583 ) ) ;
#27702 = EDGE_CURVE ( 'NONE', #17331, #3096, #15244, .T. ) ;
#27703 = CIRCLE ( 'NONE', #6252, 3.499999999999999556 ) ;
#27704 = VECTOR ( 'NONE', #52827, 1000.000000000000000 ) ;
#27705 = VERTEX_POINT ( 'NONE', #15606 ) ;
#27706 = DIRECTION ( 'NONE',  ( 1.053224967557347660E-14, 1.000000000000000000, 0.000000000000000000 ) ) ;
#27707 = DIRECTION ( 'NONE',  ( 0.000000000000000000, 0.000000000000000000, 1.000000000000000000 ) ) ;
#27708 = EDGE_CURVE ( 'NONE', #44931, #65973, #27250, .T. ) ;
#27709 = ORIENTED_EDGE ( 'NONE', *, *, #36256, .T. ) ;
#27710 = CARTESIAN_POINT ( 'NONE',  ( 0.000000000000000000, -7.449999999999998401, -12.50000000000000000 ) ) ;
#27711 = LINE ( 'NONE', #65209, #1473 ) ;
#27712 = VECTOR ( 'NONE', #265, 1000.000000000000000 ) ;
#27713 = AXIS2_PLACEMENT_3D ( 'NONE', #29454, #55986, #61622 ) ;
#27714 = VERTEX_POINT ( 'NONE', #33 ) ;
#27715 = LINE ( 'NONE', #21370, #60433 ) ;
#27716 = ADVANCED_FACE ( 'NONE', ( #10624 ), #58730, .F. ) ;
#27717 = DIRECTION ( 'NONE',  ( -0.7071067811865401342, 0.7071067811865550112, 1.367410260514937456E-30 ) ) ;
#27718 = CIRCLE ( 'NONE', #41227, 1.000000000000000000 ) ;
#27719 = CARTESIAN_POINT ( 'NONE',  ( -11.75000000000000000, -5.200000000000001066, -26.25000000000000000 ) ) ;
#27720 = EDGE_CURVE ( 'NONE', #24719, #27819, #51971, .T. ) ;
#27721 = CARTESIAN_POINT ( 'NONE',  ( -1.853252480934758584, 9.404046420173985510, 455.0000000000000568 ) ) ;
#27722 = ORIENTED_EDGE ( 'NONE', *, *, #4654, .F. ) ;
#27724 = VERTEX_POINT ( 'NONE', #37855 ) ;
#27723 = LINE ( 'NONE', #48948, #20443 ) ;
#27725 = AXIS2_PLACEMENT_3D ( 'NONE', #53544, #147, #42918 ) ;
#27726 = DIRECTION ( 'NONE',  ( 0.000000000000000000, -0.7075494706728322480, 0.7066638143775262337 ) ) ;
#27727 = CARTESIAN_POINT ( 'NONE',  ( -25.50000000000000355, -15.50000000000000000, -22.50000000000000000 ) ) ;
#27728 = FACE_OUTER_BOUND ( 'NONE', #7792, .T. ) ;
#27729 = VERTEX_POINT ( 'NONE', #54123 ) ;
#27730 = AXIS2_PLACEMENT_3D ( 'NONE', #58410, #4322, #14913 ) ;
#27731 = FACE_OUTER_BOUND ( 'NONE', #48971, .T. ) ;
#27732 = CARTESIAN_POINT ( 'NONE',  ( 6.832023737882818359, -9.912023737882819319, 54.00000000000000711 ) ) ;
#27733 = EDGE_LOOP ( 'NONE', ( #20693, #24819, #65274, #23608 ) ) ;
#27734 = VERTEX_POINT ( 'NONE', #5683 ) ;
#27735 = EDGE_CURVE ( 'NONE', #49662, #62779, #372, .T. ) ;
#27736 = ORIENTED_EDGE ( 'NONE', *, *, #43282, .F. ) ;
#27737 = CARTESIAN_POINT ( 'NONE',  ( 7.899999999999999467, 21.00000000000000000, 13.98999642601811999 ) ) ;
#27738 = CYLINDRICAL_SURFACE ( 'NONE', #11742, 0.1749999999999998224 ) ;
#27739 = CARTESIAN_POINT ( 'NONE',  ( 11.18999999999999950, 11.18999999999999950, -5.000000000000000000 ) ) ;
#27740 = ORIENTED_EDGE ( 'NONE', *, *, #52482, .F. ) ;
#27741 = ORIENTED_EDGE ( 'NONE', *, *, #69128, .T. ) ;
#27742 = ORIENTED_EDGE ( 'NONE', *, *, #11180, .F. ) ;
#27743 = DIRECTION ( 'NONE',  ( -0.000000000000000000, -0.000000000000000000, -1.000000000000000000 ) ) ;
#27744 = ORIENTED_EDGE ( 'NONE', *, *, #65703, .T. ) ;
#27745 = VECTOR ( 'NONE', #43805, 1000.000000000000227 ) ;
#27746 = ORIENTED_EDGE ( 'NONE', *, *, #30090, .F. ) ;
#27747 = ORIENTED_EDGE ( 'NONE', *, *, #51590, .F. ) ;
#27748 = ORIENTED_EDGE ( 'NONE', *, *, #6103, .F. ) ;
#27749 = AXIS2_PLACEMENT_3D ( 'NONE', #61338, #12896, #51800 ) ;
#27750 = LINE ( 'NONE', #50693, #44050 ) ;
#27751 = EDGE_CURVE ( 'NONE', #18134, #7863, #1399, .T. ) ;
#27753 = ORIENTED_EDGE ( 'NONE', *, *, #41780, .F. ) ;
#27752 = DIRECTION ( 'NONE',  ( 0.000000000000000000, 0.000000000000000000, -1.000000000000000000 ) ) ;
#27754 = DIRECTION ( 'NONE',  ( 0.000000000000000000, -0.7071067811865474617, -0.7071067811865474617 ) ) ;
#27755 = ADVANCED_FACE ( 'NONE', ( #61472, #50181 ), #23315, .T. ) ;
#27756 = VECTOR ( 'NONE', #42187, 1000.000000000000000 ) ;
#27757 = VECTOR ( 'NONE', #38399, 1000.000000000000000 ) ;
#27758 = AXIS2_PLACEMENT_3D ( 'NONE', #43919, #27666, #54899 ) ;
#27759 = CARTESIAN_POINT ( 'NONE',  ( 14.50000000000000000, 0.000000000000000000, 26.50000000000000000 ) ) ;
#27760 = CYLINDRICAL_SURFACE ( 'NONE', #48256, 24.99999999998789946 ) ;
#27761 = ADVANCED_FACE ( 'NONE', ( #11651 ), #22966, .F. ) ;
#27762 = VERTEX_POINT ( 'NONE', #38879 ) ;
#27763 = VECTOR ( 'NONE', #68104, 1000.000000000000000 ) ;
#27764 = AXIS2_PLACEMENT_3D ( 'NONE', #38763, #49036, #69902 ) ;
#27765 = VECTOR ( 'NONE', #5037, 1000.000000000000114 ) ;
#27766 = DIRECTION ( 'NONE',  ( 1.349135440953254805E-14, 1.000000000000000000, 1.836970198721035604E-16 ) ) ;
#27767 = CARTESIAN_POINT ( 'NONE',  ( -7.250000000000000888, 7.250000000000001776, -8.500000000000000000 ) ) ;
#27768 = AXIS2_PLACEMENT_3D ( 'NONE', #38122, #59673, #65334 ) ;
#27769 = ORIENTED_EDGE ( 'NONE', *, *, #53122, .F. ) ;
#27770 = DIRECTION ( 'NONE',  ( -1.000000000000000000, 0.000000000000000000, 0.000000000000000000 ) ) ;
#27771 = VECTOR ( 'NONE', #2554, 1000.000000000000114 ) ;
#27772 = DIRECTION ( 'NONE',  ( 0.000000000000000000, 0.000000000000000000, 1.000000000000000000 ) ) ;
#27773 = CARTESIAN_POINT ( 'NONE',  ( 0.000000000000000000, 0.000000000000000000, 276.7801873289890295 ) ) ;
#27774 = DIRECTION ( 'NONE',  ( -1.000000000000000000, 0.000000000000000000, 0.000000000000000000 ) ) ;
#27775 = ORIENTED_EDGE ( 'NONE', *, *, #45765, .F. ) ;
#27776 = DIRECTION ( 'NONE',  ( -0.8660254037844358210, 0.5000000000000049960, 2.509347957447882735E-16 ) ) ;
#27777 = DIRECTION ( 'NONE',  ( 0.000000000000000000, -1.000000000000000000, 0.000000000000000000 ) ) ;
#27778 = DIRECTION ( 'NONE',  ( 1.836970198721029934E-16, 1.836970198721010706E-16, -1.000000000000000000 ) ) ;
#27779 = CARTESIAN_POINT ( 'NONE',  ( 10.50702373788281996, -3.664523737882826815, 54.00000000000000711 ) ) ;
#27780 = DIRECTION ( 'NONE',  ( 0.000000000000000000, -1.000000000000000000, 0.000000000000000000 ) ) ;
#27781 = PLANE ( 'NONE',  #23754 ) ;
#27782 = DIRECTION ( 'NONE',  ( 0.000000000000000000, 0.000000000000000000, -1.000000000000000000 ) ) ;
#27783 = DIRECTION ( 'NONE',  ( 0.000000000000000000, -1.000000000000000000, 0.000000000000000000 ) ) ;
#27784 = EDGE_CURVE ( 'NONE', #61917, #43744, #62143, .T. ) ;
#27785 = ORIENTED_EDGE ( 'NONE', *, *, #65686, .F. ) ;
#27786 = LINE ( 'NONE', #28132, #38373 ) ;
#27787 = VECTOR ( 'NONE', #6203, 1000.000000000000000 ) ;
#27788 = CARTESIAN_POINT ( 'NONE',  ( -7.793516549646712477, 11.11351654964660085, 195.0000000000000284 ) ) ;
#27789 = CARTESIAN_POINT ( 'NONE',  ( 282.6457513110646005, -20.49999999999999645, -17.00000000000000000 ) ) ;
#27790 = DIRECTION ( 'NONE',  ( 1.836970198721029934E-16, 1.836970198721010706E-16, -1.000000000000000000 ) ) ;
#27791 = VERTEX_POINT ( 'NONE', #17999 ) ;
#27792 = CARTESIAN_POINT ( 'NONE',  ( -5.538810540050059572, -7.357023737882796510, 26.00000000000000711 ) ) ;
#27793 = CARTESIAN_POINT ( 'NONE',  ( -8.916576262117258622, 9.689726262117185129, 54.00000000000000711 ) ) ;
#27794 = AXIS2_PLACEMENT_3D ( 'NONE', #15473, #37042, #58602 ) ;
#27795 = EDGE_CURVE ( 'NONE', #38364, #19298, #28963, .T. ) ;
#27796 = EDGE_CURVE ( 'NONE', #47032, #30962, #1201, .T. ) ;
#27797 = DIRECTION ( 'NONE',  ( 1.000000000000000000, -0.000000000000000000, 0.000000000000000000 ) ) ;
#27798 = CIRCLE ( 'NONE', #69603, 0.3500000000002722600 ) ;
#27799 = CARTESIAN_POINT ( 'NONE',  ( -7.450000000000001954, -7.249999999999998224, -14.50000000000000000 ) ) ;
#27800 = EDGE_CURVE ( 'NONE', #25525, #68528, #49501, .T. ) ;
#27801 = CARTESIAN_POINT ( 'NONE',  ( 275.0000000000000000, -25.50000000000000355, -17.00000000000000000 ) ) ;
#27802 = EDGE_CURVE ( 'NONE', #35620, #20264, #68936, .T. ) ;
#27803 = ORIENTED_EDGE ( 'NONE', *, *, #48435, .F. ) ;
#27804 = AXIS2_PLACEMENT_3D ( 'NONE', #55530, #41251, #17698 ) ;
#27805 = CIRCLE ( 'NONE', #8615, 3.499999999999040323 ) ;
#27806 = VECTOR ( 'NONE', #2436, 1000.000000000000000 ) ;
#27807 = ORIENTED_EDGE ( 'NONE', *, *, #34234, .T. ) ;
#27808 = EDGE_CURVE ( 'NONE', #7626, #65138, #39562, .T. ) ;
#27809 = LINE ( 'NONE', #65302, #66549 ) ;
#27810 = CARTESIAN_POINT ( 'NONE',  ( 10.31452373788281562, -6.657023737882825642, 54.00000000000000711 ) ) ;
#27811 = VERTEX_POINT ( 'NONE', #65421 ) ;
#27812 = VECTOR ( 'NONE', #19940, 1000.000000000000114 ) ;
#27813 = AXIS2_PLACEMENT_3D ( 'NONE', #14955, #44746, #61009 ) ;
#27814 = AXIS2_PLACEMENT_3D ( 'NONE', #17287, #32539, #53751 ) ;
#27815 = LINE ( 'NONE', #6919, #12628 ) ;
#27816 = ORIENTED_EDGE ( 'NONE', *, *, #8840, .T. ) ;
#27817 = AXIS2_PLACEMENT_3D ( 'NONE', #3401, #13648, #56782 ) ;
#27818 = CARTESIAN_POINT ( 'NONE',  ( 7.250000000000005329, -7.249999999999998224, -9.500000000000001776 ) ) ;
#27819 = VERTEX_POINT ( 'NONE', #55153 ) ;
#27820 = EDGE_LOOP ( 'NONE', ( #59735, #32868, #37501, #30445 ) ) ;
#27821 = LINE ( 'NONE', #1619, #61086 ) ;
#27822 = ORIENTED_EDGE ( 'NONE', *, *, #68278, .F. ) ;
#27823 = CARTESIAN_POINT ( 'NONE',  ( 283.0000000000000568, -42.50000000000000000, 9.700000000000002842 ) ) ;
#27824 = DIRECTION ( 'NONE',  ( 0.000000000000000000, 0.000000000000000000, -1.000000000000000000 ) ) ;
#27825 = DIRECTION ( 'NONE',  ( -0.000000000000000000, -0.000000000000000000, -1.000000000000000000 ) ) ;
#27826 = CIRCLE ( 'NONE', #13116, 3.999999999999993339 ) ;
#27827 = ORIENTED_EDGE ( 'NONE', *, *, #445, .T. ) ;
#27828 = ORIENTED_EDGE ( 'NONE', *, *, #9919, .F. ) ;
#27829 = CARTESIAN_POINT ( 'NONE',  ( 11.50000000000000000, -11.50000000000100009, -10.50000000000065903 ) ) ;
#27830 = CARTESIAN_POINT ( 'NONE',  ( 7.749999999999998224, -7.348062532928000934, -5.000000000000000000 ) ) ;
#27831 = ORIENTED_EDGE ( 'NONE', *, *, #39946, .T. ) ;
#27832 = ORIENTED_EDGE ( 'NONE', *, *, #48521, .F. ) ;
#27833 = ORIENTED_EDGE ( 'NONE', *, *, #28232, .T. ) ;
#27834 = PLANE ( 'NONE',  #40093 ) ;
#27836 = EDGE_LOOP ( 'NONE', ( #36235, #66653, #35855, #45018 ) ) ;
#27835 = DIRECTION ( 'NONE',  ( 0.000000000000000000, 0.000000000000000000, 1.000000000000000000 ) ) ;
#27837 = CARTESIAN_POINT ( 'NONE',  ( 9.690000000000001279, 9.690000000000001279, -5.000000000000000000 ) ) ;
#27838 = DIRECTION ( 'NONE',  ( -1.000000000000000000, 0.000000000000000000, 0.000000000000000000 ) ) ;
#27839 = VERTEX_POINT ( 'NONE', #28269 ) ;
#27840 = CIRCLE ( 'NONE', #62808, 0.2000000000005261458 ) ;
#27841 = ORIENTED_EDGE ( 'NONE', *, *, #34777, .T. ) ;
#27842 = EDGE_CURVE ( 'NONE', #52180, #42854, #11996, .T. ) ;
#27843 = ADVANCED_FACE ( 'NONE', ( #66783, #54807, #66091, #50537, #33577 ), #6371, .F. ) ;
#27844 = VECTOR ( 'NONE', #9373, 1000.000000000000000 ) ;
#27845 = ORIENTED_EDGE ( 'NONE', *, *, #54995, .F. ) ;
#27846 = EDGE_CURVE ( 'NONE', #31741, #45978, #61123, .T. ) ;
#27847 = CARTESIAN_POINT ( 'NONE',  ( -15.50000000000000000, -1.037157890325000054, -22.50000000000000000 ) ) ;
#27848 = DIRECTION ( 'NONE',  ( 0.000000000000000000, 0.000000000000000000, 1.000000000000000000 ) ) ;
#27849 = AXIS2_PLACEMENT_3D ( 'NONE', #39921, #61140, #12701 ) ;
#27850 = VECTOR ( 'NONE', #5348, 1000.000000000000000 ) ;
#27851 = ORIENTED_EDGE ( 'NONE', *, *, #20499, .T. ) ;
#27852 = VECTOR ( 'NONE', #54670, 1000.000000000000000 ) ;
#27853 = AXIS2_PLACEMENT_3D ( 'NONE', #61878, #46304, #35328 ) ;
#27854 = CARTESIAN_POINT ( 'NONE',  ( 30.00000000000000000, -11.70000000000012008, -10.70000000000011831 ) ) ;
#27855 = DIRECTION ( 'NONE',  ( 0.000000000000000000, 0.000000000000000000, 1.000000000000000000 ) ) ;
#27857 = VERTEX_POINT ( 'NONE', #55498 ) ;
#27856 = CARTESIAN_POINT ( 'NONE',  ( 41.09999999999999432, -14.06939075806901940, -20.80000000000000426 ) ) ;
#27858 = VERTEX_POINT ( 'NONE', #44874 ) ;
#27859 = DIRECTION ( 'NONE',  ( -1.000000000000000000, 0.000000000000000000, 0.000000000000000000 ) ) ;
#27860 = CIRCLE ( 'NONE', #38072, 24.99999999998784972 ) ;
#27861 = CIRCLE ( 'NONE', #68495, 24.99999999998784972 ) ;
#27862 = CARTESIAN_POINT ( 'NONE',  ( 7.000000000000000000, -23.29603921945599865, 12.50000000000000000 ) ) ;
#27863 = CYLINDRICAL_SURFACE ( 'NONE', #55083, 1.000000000000000000 ) ;
#27864 = CARTESIAN_POINT ( 'NONE',  ( 5.257023737882803083, 7.172176262117205603, 26.00000000000000711 ) ) ;
#27865 = VECTOR ( 'NONE', #41312, 1000.000000000000000 ) ;
#27866 = FACE_OUTER_BOUND ( 'NONE', #45328, .T. ) ;
#27867 = ORIENTED_EDGE ( 'NONE', *, *, #24149, .F. ) ;
#27868 = LINE ( 'NONE', #65689, #9844 ) ;
#27869 = PLANE ( 'NONE',  #49700 ) ;
#27870 = PLANE ( 'NONE',  #69422 ) ;
#27871 = CARTESIAN_POINT ( 'NONE',  ( -30.00000000000000000, -12.00000000000000000, -12.20000000000000107 ) ) ;
#27872 = VECTOR ( 'NONE', #13845, 1000.000000000000000 ) ;
#27873 = DIRECTION ( 'NONE',  ( 1.000000000000000000, 0.000000000000000000, 0.000000000000000000 ) ) ;
#27874 = DIRECTION ( 'NONE',  ( -0.5000000000000004441, 0.8660254037844383745, 3.181725716174720005E-16 ) ) ;
#27875 = DIRECTION ( 'NONE',  ( 0.000000000000000000, 0.000000000000000000, 1.000000000000000000 ) ) ;
#27876 = CARTESIAN_POINT ( 'NONE',  ( 11.78648345035335865, 7.593516549646607494, 195.0000000000000284 ) ) ;
#27877 = VERTEX_POINT ( 'NONE', #7040 ) ;
#27878 = CARTESIAN_POINT ( 'NONE',  ( 2.369523737882817116, 9.547976262117204627, 54.00000000000000711 ) ) ;
#27879 = CARTESIAN_POINT ( 'NONE',  ( -7.450000000000001954, -7.249999999999998224, -15.50000000000000000 ) ) ;
#27880 = ORIENTED_EDGE ( 'NONE', *, *, #64378, .T. ) ;
#27881 = DIRECTION ( 'NONE',  ( -0.6414496315691473605, -0.7671651518153083105, -2.309356642089130002E-17 ) ) ;
#27882 = DIRECTION ( 'NONE',  ( -1.836970198721029934E-16, -1.836970198721010706E-16, 1.000000000000000000 ) ) ;
#27883 = CARTESIAN_POINT ( 'NONE',  ( -9.390476262117200434, -0.9555237378827314831, 54.00000000000000711 ) ) ;
#27884 = DIRECTION ( 'NONE',  ( 1.000000000000000000, 0.000000000000000000, 0.000000000000000000 ) ) ;
#27885 = CARTESIAN_POINT ( 'NONE',  ( -10.73351654964671020, 1.677516549646603794, 455.0000000000000568 ) ) ;
#27886 = ADVANCED_FACE ( 'NONE', ( #1068 ), #66447, .F. ) ;
#27887 = EDGE_CURVE ( 'NONE', #27714, #5641, #49792, .T. ) ;
#27888 = CARTESIAN_POINT ( 'NONE',  ( -30.00000000000000000, -14.04000000000000092, -14.80000000000000071 ) ) ;
#27889 = ORIENTED_EDGE ( 'NONE', *, *, #26372, .F. ) ;
#27890 = EDGE_CURVE ( 'NONE', #28088, #16593, #45565, .T. ) ;
#27891 = DIRECTION ( 'NONE',  ( -0.000000000000000000, 3.673940397442059868E-16, -1.000000000000000000 ) ) ;
#27892 = ADVANCED_FACE ( 'NONE', ( #29652 ), #41668, .T. ) ;
#27893 = VECTOR ( 'NONE', #30472, 1000.000000000000000 ) ;
#27894 = ORIENTED_EDGE ( 'NONE', *, *, #68644, .T. ) ;
#27895 = CYLINDRICAL_SURFACE ( 'NONE', #20129, 0.1749999999999998224 ) ;
#27896 = CIRCLE ( 'NONE', #44772, 2.250000000000001776 ) ;
#27897 = PRODUCT_RELATED_PRODUCT_CATEGORY ( 'part', '', ( #26723 ) ) ;
#27898 = DIRECTION ( 'NONE',  ( 0.000000000000000000, -1.000000000000000000, 0.000000000000000000 ) ) ;
#27899 = AXIS2_PLACEMENT_3D ( 'NONE', #29584, #13328, #2374 ) ;
#27900 = CARTESIAN_POINT ( 'NONE',  ( -15.50000000000000000, -5.000000000000000000, 19.00000000000000000 ) ) ;
#27901 = ORIENTED_EDGE ( 'NONE', *, *, #34275, .F. ) ;
#27902 = EDGE_CURVE ( 'NONE', #40018, #42074, #8080, .T. ) ;
#27903 = ORIENTED_EDGE ( 'NONE', *, *, #584, .F. ) ;
#27904 = LINE ( 'NONE', #1041, #9135 ) ;
#27906 = ORIENTED_EDGE ( 'NONE', *, *, #34233, .F. ) ;
#27905 = EDGE_CURVE ( 'NONE', #19992, #60323, #24001, .T. ) ;
#27907 = EDGE_LOOP ( 'NONE', ( #14103, #58623, #29007, #69811 ) ) ;
#27908 = CIRCLE ( 'NONE', #64073, 1.000000000000000000 ) ;
#27909 = CARTESIAN_POINT ( 'NONE',  ( 11.50000000000000000, -11.50000000000000000, 15.00000000000000000 ) ) ;
#27910 = CARTESIAN_POINT ( 'NONE',  ( -10.08346604330787777, 2.693516549646604918, 455.0000000000000568 ) ) ;
#27911 = DIRECTION ( 'NONE',  ( 0.000000000000000000, 0.000000000000000000, -1.000000000000000000 ) ) ;
#27912 = ORIENTED_EDGE ( 'NONE', *, *, #7346, .T. ) ;
#27913 = CARTESIAN_POINT ( 'NONE',  ( 6.832023737882818359, -9.737023737882811503, 26.00000000000000000 ) ) ;
#27914 = VECTOR ( 'NONE', #52930, 1000.000000000000000 ) ;
#27915 = CIRCLE ( 'NONE', #51638, 0.1999999999999996503 ) ;
#27917 = CARTESIAN_POINT ( 'NONE',  ( 10.09643294401457858, 9.293516549646566816, 455.0000000000000568 ) ) ;
#27916 = LINE ( 'NONE', #1049, #5075 ) ;
#27918 = ORIENTED_EDGE ( 'NONE', *, *, #22007, .T. ) ;
#27920 = ORIENTED_EDGE ( 'NONE', *, *, #10163, .F. ) ;
#27919 = PLANE ( 'NONE',  #44374 ) ;
#27921 = EDGE_LOOP ( 'NONE', ( #39614, #1656, #62533, #18242 ) ) ;
#27922 = DIRECTION ( 'NONE',  ( 0.6414496315691484707, -0.7671651518153074223, 0.000000000000000000 ) ) ;
#27923 = AXIS2_PLACEMENT_3D ( 'NONE', #69259, #3861, #20123 ) ;
#27924 = FACE_OUTER_BOUND ( 'NONE', #16961, .T. ) ;
#27925 = VERTEX_POINT ( 'NONE', #51228 ) ;
#27926 = ORIENTED_EDGE ( 'NONE', *, *, #55732, .T. ) ;
#27927 = DIRECTION ( 'NONE',  ( -1.000000000000000000, 0.000000000000000000, 0.000000000000000000 ) ) ;
#27928 = CYLINDRICAL_SURFACE ( 'NONE', #59458, 0.5000000000009459100 ) ;
#27929 = VERTEX_POINT ( 'NONE', #19054 ) ;
#27930 = EDGE_CURVE ( 'NONE', #43298, #37385, #59935, .T. ) ;
#27931 = DIRECTION ( 'NONE',  ( 0.000000000000000000, 0.000000000000000000, -1.000000000000000000 ) ) ;
#27932 = FACE_OUTER_BOUND ( 'NONE', #5896, .T. ) ;
#27933 = DIRECTION ( 'NONE',  ( 7.808916176531286882E-15, 1.000000000000000000, 0.000000000000000000 ) ) ;
#27934 = ORIENTED_EDGE ( 'NONE', *, *, #16869, .T. ) ;
#27935 = CARTESIAN_POINT ( 'NONE',  ( -8.250000000000001776, 0.000000000000000000, -13.00000000000000178 ) ) ;
#27936 = CARTESIAN_POINT ( 'NONE',  ( 29.50000000000000355, -12.00000000000000000, 11.00000000000000000 ) ) ;
#27937 = CIRCLE ( 'NONE', #36994, 1.929199999999997139 ) ;
#27939 = VERTEX_POINT ( 'NONE', #35293 ) ;
#27938 = DIRECTION ( 'NONE',  ( 1.000000000000000000, 0.000000000000000000, 0.000000000000000000 ) ) ;
#27941 = EDGE_LOOP ( 'NONE', ( #19749, #32626, #7041, #18707 ) ) ;
#27940 = DIRECTION ( 'NONE',  ( -1.000000000000000000, 0.000000000000000000, 0.000000000000000000 ) ) ;
#27942 = CARTESIAN_POINT ( 'NONE',  ( -8.250000000000001776, 0.000000000000000000, -24.50000000000000000 ) ) ;
#27943 = EDGE_CURVE ( 'NONE', #45109, #114, #57670, .T. ) ;
#27944 = DIRECTION ( 'NONE',  ( -1.000000000000000000, 0.000000000000000000, 0.000000000000000000 ) ) ;
#27945 = LINE ( 'NONE', #49513, #1925 ) ;
#27946 = CARTESIAN_POINT ( 'NONE',  ( 9.690000000000001279, 9.690000000000001279, 0.000000000000000000 ) ) ;
#27947 = PLANE ( 'NONE',  #50863 ) ;
#27948 = VECTOR ( 'NONE', #40389, 1000.000000000000000 ) ;
#27949 = CIRCLE ( 'NONE', #34692, 24.99999999998784972 ) ;
#27950 = EDGE_CURVE ( 'NONE', #7833, #40446, #51589, .T. ) ;
#27951 = CARTESIAN_POINT ( 'NONE',  ( -8.250000000000001776, 0.000000000000000000, -17.50000000000000000 ) ) ;
#27952 = ORIENTED_EDGE ( 'NONE', *, *, #33129, .F. ) ;
#27953 = DIRECTION ( 'NONE',  ( -0.8660254037844482555, 0.000000000000000000, -0.4999999999999831801 ) ) ;
#27954 = ORIENTED_EDGE ( 'NONE', *, *, #21739, .F. ) ;
#27955 = VECTOR ( 'NONE', #12727, 1000.000000000000114 ) ;
#27958 = ORIENTED_EDGE ( 'NONE', *, *, #64960, .T. ) ;
#27957 = DIRECTION ( 'NONE',  ( 0.000000000000000000, 0.000000000000000000, 1.000000000000000000 ) ) ;
#27956 = VECTOR ( 'NONE', #8966, 1000.000000000000000 ) ;
#27959 = CARTESIAN_POINT ( 'NONE',  ( 48.50000000000000000, 0.7500000000000000000, 3.418698582794335028 ) ) ;
#27960 = DIRECTION ( 'NONE',  ( 1.836970198721029934E-16, -1.836970198721036344E-16, 1.000000000000000000 ) ) ;
#27961 = AXIS2_PLACEMENT_3D ( 'NONE', #64494, #16049, #37621 ) ;
#27962 = ORIENTED_EDGE ( 'NONE', *, *, #60350, .T. ) ;
#27963 = LINE ( 'NONE', #48493, #42191 ) ;
#27964 = DIRECTION ( 'NONE',  ( -1.000000000000000000, 0.000000000000000000, 0.000000000000000000 ) ) ;
#27965 = ADVANCED_FACE ( 'NONE', ( #13396 ), #61845, .F. ) ;
#27966 = VERTEX_POINT ( 'NONE', #34951 ) ;
#27967 = PLANE ( 'NONE',  #66210 ) ;
#27968 = DIRECTION ( 'NONE',  ( 0.000000000000000000, 0.000000000000000000, -1.000000000000000000 ) ) ;
#27969 = FACE_OUTER_BOUND ( 'NONE', #15133, .T. ) ;
#27970 = DIRECTION ( 'NONE',  ( 0.5000000000000068834, 0.8660254037844345998, 6.723777587268309839E-17 ) ) ;
#27971 = EDGE_CURVE ( 'NONE', #37432, #16302, #61027, .T. ) ;
#27972 = AXIS2_PLACEMENT_3D ( 'NONE', #48735, #59342, #28201 ) ;
#27973 = DIRECTION ( 'NONE',  ( 0.000000000000000000, -0.5625376724249369076, 0.8267716535433071723 ) ) ;
#27974 = ORIENTED_EDGE ( 'NONE', *, *, #57435, .T. ) ;
#27975 = EDGE_CURVE ( 'NONE', #29308, #6488, #8431, .T. ) ;
#27976 = FACE_OUTER_BOUND ( 'NONE', #40576, .T. ) ;
#27977 = EDGE_LOOP ( 'NONE', ( #1221, #53217 ) ) ;
#27978 = EDGE_CURVE ( 'NONE', #10363, #21898, #57237, .T. ) ;
#27979 = ORIENTED_EDGE ( 'NONE', *, *, #28002, .T. ) ;
#27980 = CARTESIAN_POINT ( 'NONE',  ( 8.250000000000005329, 7.250000000000000888, -26.00000000000001066 ) ) ;
#27981 = CARTESIAN_POINT ( 'NONE',  ( 7.000000000000000000, -20.40000000000000213, -16.03137303340311348 ) ) ;
#27982 = EDGE_CURVE ( 'NONE', #60071, #11614, #36363, .T. ) ;
#27983 = LINE ( 'NONE', #23013, #43402 ) ;
#27984 = DIRECTION ( 'NONE',  ( -0.000000000000000000, 3.673940397442059868E-16, -1.000000000000000000 ) ) ;
#27985 = VERTEX_POINT ( 'NONE', #52283 ) ;
#27986 = ADVANCED_FACE ( 'NONE', ( #40962 ), #51936, .F. ) ;
#27987 = ORIENTED_EDGE ( 'NONE', *, *, #53763, .F. ) ;
#27989 = VERTEX_POINT ( 'NONE', #57931 ) ;
#27988 = DIRECTION ( 'NONE',  ( -1.000000000000000000, 0.000000000000000000, 0.000000000000000000 ) ) ;
#27991 = ORIENTED_EDGE ( 'NONE', *, *, #32612, .F. ) ;
#27990 = EDGE_CURVE ( 'NONE', #18063, #37646, #3847, .T. ) ;
#27992 = DIRECTION ( 'NONE',  ( 0.000000000000000000, -1.000000000000000000, -3.673940397442059868E-16 ) ) ;
#27993 = DIRECTION ( 'NONE',  ( 0.000000000000000000, 0.000000000000000000, 1.000000000000000000 ) ) ;
#27994 = DIRECTION ( 'NONE',  ( -1.000000000000000000, 0.000000000000000000, 0.000000000000000000 ) ) ;
#27995 = VECTOR ( 'NONE', #21003, 1000.000000000000000 ) ;
#27996 = LINE ( 'NONE', #27308, #60508 ) ;
#27998 = DIRECTION ( 'NONE',  ( -0.000000000000000000, -0.000000000000000000, -1.000000000000000000 ) ) ;
#27997 = DIRECTION ( 'NONE',  ( -1.000000000000000000, 0.000000000000000000, 0.000000000000000000 ) ) ;
#27999 = ORIENTED_EDGE ( 'NONE', *, *, #27055, .F. ) ;
#28001 = ORIENTED_EDGE ( 'NONE', *, *, #50884, .T. ) ;
#28000 = CARTESIAN_POINT ( 'NONE',  ( 23.48000000000000043, -17.50000000000000000, -26.00000000000000355 ) ) ;
#28002 = EDGE_CURVE ( 'NONE', #6350, #59597, #41314, .T. ) ;
#28003 = VERTEX_POINT ( 'NONE', #14461 ) ;
#28004 = EDGE_LOOP ( 'NONE', ( #49156, #7720, #48883, #44748, #42774, #44913 ) ) ;
#28005 = DIRECTION ( 'NONE',  ( 0.000000000000000000, -1.000000000000000000, 0.000000000000000000 ) ) ;
#28006 = CARTESIAN_POINT ( 'NONE',  ( 15.50000000000000000, -2.500000000000000000, 21.05662432702600029 ) ) ;
#28007 = VECTOR ( 'NONE', #60396, 1000.000000000000000 ) ;
#28008 = CARTESIAN_POINT ( 'NONE',  ( -10.19191654964686933, -11.48848345035334795, 455.0000000000000568 ) ) ;
#28009 = DIRECTION ( 'NONE',  ( -0.000000000000000000, -0.000000000000000000, 1.000000000000000000 ) ) ;
#28010 = EDGE_CURVE ( 'NONE', #48863, #50286, #10285, .T. ) ;
#28011 = ORIENTED_EDGE ( 'NONE', *, *, #23641, .F. ) ;
#28012 = ORIENTED_EDGE ( 'NONE', *, *, #19477, .T. ) ;
#28013 = AXIS2_PLACEMENT_3D ( 'NONE', #39672, #24479, #12793 ) ;
#28014 = CIRCLE ( 'NONE', #3180, 0.1999999999999996503 ) ;
#28015 = DIRECTION ( 'NONE',  ( 0.000000000000000000, 0.000000000000000000, -1.000000000000000000 ) ) ;
#28016 = CARTESIAN_POINT ( 'NONE',  ( -9.897976262117287760, -6.832023737882751746, 26.00000000000000000 ) ) ;
#28017 = ORIENTED_EDGE ( 'NONE', *, *, #35850, .F. ) ;
#28018 = ADVANCED_FACE ( 'NONE', ( #25413 ), #46974, .F. ) ;
#28019 = EDGE_LOOP ( 'NONE', ( #52469, #6334, #17374, #34587, #49647, #61573, #29094, #18491, #2852, #20873, #667, #48547, #54200, #40208, #21686, #63283, #328, #44968 ) ) ;
#28020 = DIRECTION ( 'NONE',  ( 0.000000000000000000, 3.989863994748342081E-13, 1.000000000000000000 ) ) ;
#28021 = CARTESIAN_POINT ( 'NONE',  ( -8.250000000000001776, -8.249999999999998224, -26.00000000000001066 ) ) ;
#28022 = ORIENTED_EDGE ( 'NONE', *, *, #18413, .F. ) ;
#28023 = ADVANCED_FACE ( 'NONE', ( #1241, #4215 ), #6550, .T. ) ;
#28024 = AXIS2_PLACEMENT_3D ( 'NONE', #5178, #27778, #930 ) ;
#28025 = LINE ( 'NONE', #59157, #60702 ) ;
#28026 = EDGE_CURVE ( 'NONE', #9595, #41334, #25779, .T. ) ;
#28028 = EDGE_LOOP ( 'NONE', ( #64192, #16163, #22256, #55641 ) ) ;
#28027 = CARTESIAN_POINT ( 'NONE',  ( -7.450000000000001954, -7.249999999999998224, -22.50000000000000000 ) ) ;
#28029 = VERTEX_POINT ( 'NONE', #20800 ) ;
#28030 = PLANE ( 'NONE',  #28721 ) ;
#28031 = CARTESIAN_POINT ( 'NONE',  ( 2.906483450353343656, -10.92648345035346402, 455.0000000000000568 ) ) ;
#28032 = CARTESIAN_POINT ( 'NONE',  ( 6.006483450353401921, 5.993516549646582092, 455.0000000000000568 ) ) ;
#28033 = CARTESIAN_POINT ( 'NONE',  ( -2.277516549646816379, -9.841277389592805847, 455.0000000000000568 ) ) ;
#28034 = LINE ( 'NONE', #22724, #47453 ) ;
#28035 = EDGE_CURVE ( 'NONE', #35740, #43050, #42718, .T. ) ;
#28036 = ORIENTED_EDGE ( 'NONE', *, *, #60407, .F. ) ;
#28037 = DIRECTION ( 'NONE',  ( 1.000000000000000000, 0.000000000000000000, 0.000000000000000000 ) ) ;
#28039 = ORIENTED_EDGE ( 'NONE', *, *, #37741, .F. ) ;
#28038 = CARTESIAN_POINT ( 'NONE',  ( -4.135079735113167843, 6.822336235477362010, 26.00000000000000711 ) ) ;
#28040 = CARTESIAN_POINT ( 'NONE',  ( -30.00000000000000000, -5.000000000000000000, 27.00000000000000000 ) ) ;
#28041 = DIRECTION ( 'NONE',  ( 1.000000000000000000, -0.000000000000000000, 0.000000000000000000 ) ) ;
#28042 = EDGE_CURVE ( 'NONE', #31900, #12490, #31780, .T. ) ;
#28043 = DIRECTION ( 'NONE',  ( 0.000000000000000000, 0.000000000000000000, -1.000000000000000000 ) ) ;
#28044 = EDGE_CURVE ( 'NONE', #15054, #14428, #4556, .T. ) ;
#28045 = FACE_OUTER_BOUND ( 'NONE', #42455, .T. ) ;
#28046 = CARTESIAN_POINT ( 'NONE',  ( 11.32648345035337734, -7.606483450353492159, 455.0000000000000568 ) ) ;
#28047 = ADVANCED_FACE ( 'NONE', ( #53690 ), #37084, .T. ) ;
#28048 = VERTEX_POINT ( 'NONE', #4898 ) ;
#28049 = EDGE_CURVE ( 'NONE', #52876, #57882, #47676, .T. ) ;
#28050 = ADVANCED_FACE ( 'NONE', ( #15161 ), #5253, .F. ) ;
#28051 = EDGE_LOOP ( 'NONE', ( #16362, #23284, #34690, #53078 ) ) ;
#28052 = DIRECTION ( 'NONE',  ( 0.000000000000000000, -1.000000000000000000, 0.000000000000000000 ) ) ;
#28053 = DIRECTION ( 'NONE',  ( 0.000000000000000000, 0.000000000000000000, -1.000000000000000000 ) ) ;
#28054 = EDGE_CURVE ( 'NONE', #34099, #64234, #60271, .T. ) ;
#28055 = VECTOR ( 'NONE', #14418, 1000.000000000000114 ) ;
#28056 = ORIENTED_EDGE ( 'NONE', *, *, #53222, .T. ) ;
#28057 = EDGE_CURVE ( 'NONE', #50773, #48157, #11829, .T. ) ;
#28058 = DIRECTION ( 'NONE',  ( -0.000000000000000000, 0.000000000000000000, 1.000000000000000000 ) ) ;
#28059 = CARTESIAN_POINT ( 'NONE',  ( -4.383466043307858939, 8.593516549646588842, 455.0000000000000568 ) ) ;
#28060 = ORIENTED_EDGE ( 'NONE', *, *, #63443, .F. ) ;
#28061 = ADVANCED_FACE ( 'NONE', ( #22800 ), #58985, .F. ) ;
#28062 = VECTOR ( 'NONE', #550, 1000.000000000000000 ) ;
#28063 = FACE_OUTER_BOUND ( 'NONE', #69778, .T. ) ;
#28064 = DIRECTION ( 'NONE',  ( -1.000000000000000000, 0.000000000000000000, 0.000000000000000000 ) ) ;
#28065 = VERTEX_POINT ( 'NONE', #917 ) ;
#28066 = CARTESIAN_POINT ( 'NONE',  ( 28.90000000000000213, 13.66939075806899240, 20.79999999999999361 ) ) ;
#28067 = DIRECTION ( 'NONE',  ( 0.000000000000000000, -0.9921567416492215186, 0.1249999999999996531 ) ) ;
#28068 = FACE_OUTER_BOUND ( 'NONE', #53314, .T. ) ;
#28069 = EDGE_CURVE ( 'NONE', #67816, #16876, #63600, .T. ) ;
#28070 = VERTEX_POINT ( 'NONE', #42022 ) ;
#28072 = ORIENTED_EDGE ( 'NONE', *, *, #25632, .F. ) ;
#28071 = DIRECTION ( 'NONE',  ( -0.5000000000000129896, -0.8660254037844311581, -2.509347957447868930E-16 ) ) ;
#28073 = EDGE_CURVE ( 'NONE', #7006, #10852, #67866, .T. ) ;
#28074 = CIRCLE ( 'NONE', #50667, 0.5540281690140901327 ) ;
#28075 = CARTESIAN_POINT ( 'NONE',  ( 4.206483450353422526, 11.31351654964658415, 455.0000000000000568 ) ) ;
#28076 = DIRECTION ( 'NONE',  ( 1.000000000000000000, 0.000000000000000000, 0.000000000000000000 ) ) ;
#28077 = DIRECTION ( 'NONE',  ( -1.000000000000000000, 0.000000000000000000, 0.000000000000000000 ) ) ;
#28078 = ORIENTED_EDGE ( 'NONE', *, *, #49984, .T. ) ;
#28079 = DIRECTION ( 'NONE',  ( -0.4999999999999755196, 0.8660254037844526964, 2.509347957447861534E-16 ) ) ;
#28080 = DIRECTION ( 'NONE',  ( -1.000000000000000000, 0.000000000000000000, 0.000000000000000000 ) ) ;
#28081 = ORIENTED_EDGE ( 'NONE', *, *, #46969, .F. ) ;
#28082 = EDGE_CURVE ( 'NONE', #2943, #11562, #17487, .T. ) ;
#28083 = ORIENTED_EDGE ( 'NONE', *, *, #39777, .F. ) ;
#28084 = VERTEX_POINT ( 'NONE', #21165 ) ;
#28085 = CARTESIAN_POINT ( 'NONE',  ( 8.900000000000005684, -21.00000000000000000, -13.86939075806900057 ) ) ;
#28086 = DIRECTION ( 'NONE',  ( 1.836970198721029934E-16, 1.836970198721010706E-16, -1.000000000000000000 ) ) ;
#28087 = DIRECTION ( 'NONE',  ( 0.000000000000000000, 0.000000000000000000, 1.000000000000000000 ) ) ;
#28088 = VERTEX_POINT ( 'NONE', #15853 ) ;
#28089 = ORIENTED_EDGE ( 'NONE', *, *, #3371, .T. ) ;
#28090 = ORIENTED_EDGE ( 'NONE', *, *, #63334, .T. ) ;
#28091 = DIRECTION ( 'NONE',  ( 1.000000000000000000, -0.000000000000000000, 0.000000000000000000 ) ) ;
#28092 = ORIENTED_EDGE ( 'NONE', *, *, #44525, .F. ) ;
#28093 = ORIENTED_EDGE ( 'NONE', *, *, #6603, .F. ) ;
#28094 = VERTEX_POINT ( 'NONE', #44013 ) ;
#28095 = CIRCLE ( 'NONE', #64294, 0.3000000000005387246 ) ;
#28096 = ADVANCED_FACE ( 'NONE', ( #52648 ), #65591, .F. ) ;
#28097 = ORIENTED_EDGE ( 'NONE', *, *, #8756, .T. ) ;
#28098 = DIRECTION ( 'NONE',  ( 0.000000000000000000, 0.000000000000000000, 1.000000000000000000 ) ) ;
#28100 = ORIENTED_EDGE ( 'NONE', *, *, #5693, .F. ) ;
#28099 = CARTESIAN_POINT ( 'NONE',  ( 14.50000000000000000, -42.50000000000000000, 30.00000000000000000 ) ) ;
#28101 = VECTOR ( 'NONE', #54182, 1000.000000000000000 ) ;
#28102 = EDGE_CURVE ( 'NONE', #9312, #2345, #62361, .T. ) ;
#28103 = LINE ( 'NONE', #43319, #58317 ) ;
#28104 = CARTESIAN_POINT ( 'NONE',  ( 7.450000000000003730, -7.249999999999997335, -14.00000000000000000 ) ) ;
#28105 = CYLINDRICAL_SURFACE ( 'NONE', #42596, 5.000000000000000000 ) ;
#28106 = EDGE_CURVE ( 'NONE', #50851, #24869, #66287, .T. ) ;
#28107 = ORIENTED_EDGE ( 'NONE', *, *, #20801, .T. ) ;
#28108 = AXIS2_PLACEMENT_3D ( 'NONE', #56029, #66630, #18183 ) ;
#28109 = EDGE_CURVE ( 'NONE', #19877, #33774, #47531, .T. ) ;
#28110 = CARTESIAN_POINT ( 'NONE',  ( -8.916576262117345664, -8.580623737882765667, 54.00000000000000711 ) ) ;
#28111 = CARTESIAN_POINT ( 'NONE',  ( 8.250000000000005329, 7.250000000000000888, -9.000000000000001776 ) ) ;
#28112 = CARTESIAN_POINT ( 'NONE',  ( 30.00000000000000000, -9.199999999999999289, 12.69999999999986073 ) ) ;
#28113 = EDGE_CURVE ( 'NONE', #49641, #63752, #51410, .T. ) ;
#28114 = VERTEX_POINT ( 'NONE', #18893 ) ;
#28115 = PLANE ( 'NONE',  #54065 ) ;
#28117 = VECTOR ( 'NONE', #69073, 1000.000000000000000 ) ;
#28116 = VECTOR ( 'NONE', #44119, 999.9999999999998863 ) ;
#28118 = DIRECTION ( 'NONE',  ( 0.000000000000000000, 1.000000000000000000, -0.000000000000000000 ) ) ;
#28119 = FACE_OUTER_BOUND ( 'NONE', #52797, .T. ) ;
#28120 = ORIENTED_EDGE ( 'NONE', *, *, #37631, .T. ) ;
#28121 = FACE_OUTER_BOUND ( 'NONE', #39914, .T. ) ;
#28122 = CIRCLE ( 'NONE', #30396, 0.3499999999999285905 ) ;
#28123 = FACE_BOUND ( 'NONE', #9574, .T. ) ;
#28124 = DIRECTION ( 'NONE',  ( 1.000000000000000000, -0.000000000000000000, -0.000000000000000000 ) ) ;
#28125 = EDGE_CURVE ( 'NONE', #55190, #28029, #45232, .T. ) ;
#28126 = DIRECTION ( 'NONE',  ( 0.000000000000000000, 0.000000000000000000, -1.000000000000000000 ) ) ;
#28127 = DIRECTION ( 'NONE',  ( 0.000000000000000000, 0.000000000000000000, 1.000000000000000000 ) ) ;
#28128 = DIRECTION ( 'NONE',  ( -1.000000000000000000, 0.000000000000000000, 0.000000000000000000 ) ) ;
#28129 =( NAMED_UNIT ( * ) SI_UNIT ( $, .STERADIAN. ) SOLID_ANGLE_UNIT ( ) );
#28130 = DIRECTION ( 'NONE',  ( -8.540177112501197482E-15, -1.000000000000000000, -3.673940397442059868E-16 ) ) ;
#28131 = VERTEX_POINT ( 'NONE', #7917 ) ;
#28132 = CARTESIAN_POINT ( 'NONE',  ( 11.78648345035337819, -4.186483450353492231, 455.0000000000000568 ) ) ;
#28133 = DIRECTION ( 'NONE',  ( 1.000000000000000000, 2.135044278125301343E-15, -0.000000000000000000 ) ) ;
#28134 = DIRECTION ( 'NONE',  ( 0.000000000000000000, 0.7057491738665943037, 0.7084617869628675457 ) ) ;
#28135 = DIRECTION ( 'NONE',  ( 0.000000000000000000, 1.000000000000000000, 1.880440247955334083E-12 ) ) ;
#28136 = EDGE_LOOP ( 'NONE', ( #68774, #61604, #43915, #36397 ) ) ;
#28137 = DIRECTION ( 'NONE',  ( -1.000000000000000000, 9.050731179009442381E-15, 3.325184690495119758E-30 ) ) ;
#28138 = DIRECTION ( 'NONE',  ( 0.000000000000000000, -0.000000000000000000, 1.000000000000000000 ) ) ;
#28139 = DIRECTION ( 'NONE',  ( -1.000000000000000000, 0.000000000000000000, 0.000000000000000000 ) ) ;
#28140 = AXIS2_PLACEMENT_3D ( 'NONE', #1219, #1905, #23112 ) ;
#28141 = LINE ( 'NONE', #1965, #21854 ) ;
#28142 = CARTESIAN_POINT ( 'NONE',  ( 11.75000000000000000, -5.200000000000001066, -11.75000000000000000 ) ) ;
#28143 = ADVANCED_FACE ( 'NONE', ( #61666 ), #51061, .F. ) ;
#28144 = ORIENTED_EDGE ( 'NONE', *, *, #51500, .T. ) ;
#28145 = VECTOR ( 'NONE', #42428, 1000.000000000000000 ) ;
#28146 = ADVANCED_FACE ( 'NONE', ( #1570 ), #23137, .F. ) ;
#28147 = DIRECTION ( 'NONE',  ( 1.000000000000000000, -0.000000000000000000, -0.000000000000000000 ) ) ;
#28148 = LINE ( 'NONE', #44388, #66145 ) ;
#28149 = ORIENTED_EDGE ( 'NONE', *, *, #65958, .T. ) ;
#28150 = CIRCLE ( 'NONE', #67675, 24.99999999998794920 ) ;
#28151 = DIRECTION ( 'NONE',  ( 3.491481338843132961E-15, 1.000000000000000000, 1.836970198721029934E-16 ) ) ;
#28152 = ORIENTED_EDGE ( 'NONE', *, *, #9944, .F. ) ;
#28153 = AXIS2_PLACEMENT_3D ( 'NONE', #34865, #66005, #45126 ) ;
#28154 = PLANE ( 'NONE',  #46928 ) ;
#28155 = ORIENTED_EDGE ( 'NONE', *, *, #54678, .T. ) ;
#28156 = ORIENTED_EDGE ( 'NONE', *, *, #18490, .T. ) ;
#28157 = CARTESIAN_POINT ( 'NONE',  ( 25.57999999999999829, 0.000000000000000000, 2.458500000000000796 ) ) ;
#28158 = ORIENTED_EDGE ( 'NONE', *, *, #60896, .F. ) ;
#28159 = DIRECTION ( 'NONE',  ( 2.478176394252584099E-15, 1.000000000000000000, 0.000000000000000000 ) ) ;
#28160 = AXIS2_PLACEMENT_3D ( 'NONE', #1264, #22493, #12202 ) ;
#28161 = DIRECTION ( 'NONE',  ( -1.062075597536822467E-14, -1.000000000000000000, 0.000000000000000000 ) ) ;
#28162 = CARTESIAN_POINT ( 'NONE',  ( -25.50000000000000355, -15.50000000000000000, -22.50000000000000000 ) ) ;
#28163 = EDGE_LOOP ( 'NONE', ( #14995, #17898, #35838, #20254 ) ) ;
#28164 = ORIENTED_EDGE ( 'NONE', *, *, #69097, .F. ) ;
#28165 = CARTESIAN_POINT ( 'NONE',  ( -7.750000000000001776, 7.750000000000001776, 0.000000000000000000 ) ) ;
#28167 = LINE ( 'NONE', #44758, #58199 ) ;
#28166 = VECTOR ( 'NONE', #52119, 1000.000000000000000 ) ;
#28168 = VERTEX_POINT ( 'NONE', #24550 ) ;
#28169 = ORIENTED_EDGE ( 'NONE', *, *, #12994, .F. ) ;
#28170 = ORIENTED_EDGE ( 'NONE', *, *, #64966, .F. ) ;
#28171 = FACE_OUTER_BOUND ( 'NONE', #632, .T. ) ;
#28172 = DIRECTION ( 'NONE',  ( -0.7071067811865451302, 0.7071067811865500152, 0.000000000000000000 ) ) ;
#28174 = ORIENTED_EDGE ( 'NONE', *, *, #66967, .T. ) ;
#28173 = DIRECTION ( 'NONE',  ( 0.000000000000000000, 0.000000000000000000, -1.000000000000000000 ) ) ;
#28175 = EDGE_CURVE ( 'NONE', #68454, #31689, #2620, .T. ) ;
#28176 = FACE_OUTER_BOUND ( 'NONE', #9026, .T. ) ;
#28177 = CARTESIAN_POINT ( 'NONE',  ( 10.00000000000000000, 18.00000000000000355, 21.00000000000000000 ) ) ;
#28178 = VECTOR ( 'NONE', #8866, 1000.000000000000000 ) ;
#28179 = ORIENTED_EDGE ( 'NONE', *, *, #4849, .T. ) ;
#28180 = ORIENTED_EDGE ( 'NONE', *, *, #23226, .F. ) ;
#28181 = ADVANCED_FACE ( 'NONE', ( #39400 ), #7576, .T. ) ;
#28182 = ORIENTED_EDGE ( 'NONE', *, *, #5113, .F. ) ;
#28183 = EDGE_CURVE ( 'NONE', #27705, #43873, #45048, .T. ) ;
#28184 = EDGE_CURVE ( 'NONE', #56406, #43147, #39741, .T. ) ;
#28185 = CARTESIAN_POINT ( 'NONE',  ( 7.000000000000000000, -30.45000000000094786, 14.49999999999906031 ) ) ;
#28186 = LINE ( 'NONE', #44774, #57235 ) ;
#28187 = ADVANCED_FACE ( 'NONE', ( #12862 ), #45396, .F. ) ;
#28188 = EDGE_CURVE ( 'NONE', #5949, #19358, #22696, .T. ) ;
#28189 = CARTESIAN_POINT ( 'NONE',  ( 10.14575131106459160, -20.49999999999999645, -17.00000000000000000 ) ) ;
#28190 = AXIS2_PLACEMENT_3D ( 'NONE', #15472, #5207, #30673 ) ;
#28191 = AXIS2_PLACEMENT_3D ( 'NONE', #12736, #66842, #35348 ) ;
#28192 = EDGE_CURVE ( 'NONE', #36247, #50834, #4637, .T. ) ;
#28193 = LINE ( 'NONE', #49759, #38056 ) ;
#28194 = CARTESIAN_POINT ( 'NONE',  ( 40.90000000000000568, -14.48845687959340012, -21.00000000000000000 ) ) ;
#28196 = ORIENTED_EDGE ( 'NONE', *, *, #21040, .F. ) ;
#28195 = CARTESIAN_POINT ( 'NONE',  ( 25.50000000000000355, -15.50000000000000000, -22.50000000000000000 ) ) ;
#28197 = VERTEX_POINT ( 'NONE', #34427 ) ;
#28198 = DIRECTION ( 'NONE',  ( 0.000000000000000000, 0.000000000000000000, -1.000000000000000000 ) ) ;
#28199 = VECTOR ( 'NONE', #12702, 1000.000000000000000 ) ;
#28200 = DIRECTION ( 'NONE',  ( 1.000000000000000000, -0.000000000000000000, 0.000000000000000000 ) ) ;
#28201 = DIRECTION ( 'NONE',  ( 0.000000000000000000, -0.1249999999999996531, -0.9921567416492215186 ) ) ;
#28202 = CARTESIAN_POINT ( 'NONE',  ( 6.006483450353377940, 7.393516549646579783, 455.0000000000000568 ) ) ;
#28203 = AXIS2_PLACEMENT_3D ( 'NONE', #26317, #41168, #65119 ) ;
#28204 = DIRECTION ( 'NONE',  ( 0.000000000000000000, -1.000000000000000000, -3.673940397442059868E-16 ) ) ;
#28205 = ORIENTED_EDGE ( 'NONE', *, *, #10262, .T. ) ;
#28206 = CARTESIAN_POINT ( 'NONE',  ( 30.00000000000000000, -10.85999999999999943, -9.350000000000269651 ) ) ;
#28207 = DIRECTION ( 'NONE',  ( 0.7071067811865550112, 0.7071067811865401342, 0.000000000000000000 ) ) ;
#28208 = DIRECTION ( 'NONE',  ( 0.000000000000000000, 1.000000000000000000, 0.000000000000000000 ) ) ;
#28209 = AXIS2_PLACEMENT_3D ( 'NONE', #46742, #40745, #57707 ) ;
#28210 = DIRECTION ( 'NONE',  ( 0.000000000000000000, 1.000000000000000000, 0.000000000000000000 ) ) ;
#28211 = CARTESIAN_POINT ( 'NONE',  ( -29.50000000000000355, -11.70000000000012008, 10.70000000000011831 ) ) ;
#28212 = CARTESIAN_POINT ( 'NONE',  ( -2.693516549646827851, -10.92648345035345692, 455.0000000000000568 ) ) ;
#28213 = AXIS2_PLACEMENT_3D ( 'NONE', #64484, #21692, #37265 ) ;
#28214 = DIRECTION ( 'NONE',  ( -0.000000000000000000, 3.673940397442059868E-16, -1.000000000000000000 ) ) ;
#28215 = ORIENTED_EDGE ( 'NONE', *, *, #691, .T. ) ;
#28216 = CARTESIAN_POINT ( 'NONE',  ( 30.00000000000000000, -11.70000000000000284, -12.50000000000000000 ) ) ;
#28217 = CARTESIAN_POINT ( 'NONE',  ( 11.19368345035336709, -12.00648345035349251, 455.0000000000000568 ) ) ;
#28218 = VERTEX_POINT ( 'NONE', #50707 ) ;
#28219 = DIRECTION ( 'NONE',  ( 0.7071067811865490160, 0.000000000000000000, 0.7071067811865461294 ) ) ;
#28220 = DIRECTION ( 'NONE',  ( 0.000000000000000000, 0.000000000000000000, 1.000000000000000000 ) ) ;
#28221 = CYLINDRICAL_SURFACE ( 'NONE', #49052, 1.399999999999998579 ) ;
#28222 = FACE_OUTER_BOUND ( 'NONE', #82, .T. ) ;
#28223 = LINE ( 'NONE', #5632, #20340 ) ;
#28224 = CARTESIAN_POINT ( 'NONE',  ( -7.250000000000000888, 7.250000000000001776, -26.00000000000001066 ) ) ;
#28225 = EDGE_CURVE ( 'NONE', #55626, #5311, #2277, .T. ) ;
#28226 = ORIENTED_EDGE ( 'NONE', *, *, #49690, .T. ) ;
#28227 = CARTESIAN_POINT ( 'NONE',  ( -7.250000000000000888, -8.249999999999998224, -13.00000000000000178 ) ) ;
#28228 = ORIENTED_EDGE ( 'NONE', *, *, #16602, .T. ) ;
#28229 = EDGE_CURVE ( 'NONE', #48332, #4626, #46457, .T. ) ;
#28230 = CARTESIAN_POINT ( 'NONE',  ( -16.75000000000000000, -2.500000000000000000, 21.77831216351300014 ) ) ;
#28231 = EDGE_CURVE ( 'NONE', #22594, #60163, #13583, .T. ) ;
#28232 = EDGE_CURVE ( 'NONE', #38683, #18160, #24894, .T. ) ;
#28233 = PLANE ( 'NONE',  #32188 ) ;
#28234 = ORIENTED_EDGE ( 'NONE', *, *, #20458, .F. ) ;
#28235 = ORIENTED_EDGE ( 'NONE', *, *, #67556, .F. ) ;
#28236 = CARTESIAN_POINT ( 'NONE',  ( 4.720772854004774643, -6.358413763958971288, 54.00000000000000711 ) ) ;
#28237 = VECTOR ( 'NONE', #66668, 1000.000000000000000 ) ;
#28238 = ORIENTED_EDGE ( 'NONE', *, *, #3490, .F. ) ;
#28239 = ORIENTED_EDGE ( 'NONE', *, *, #2901, .T. ) ;
#28240 = CARTESIAN_POINT ( 'NONE',  ( 8.241237374594303944, -1.634292677759888068, 54.00000000000000711 ) ) ;
#28241 = CARTESIAN_POINT ( 'NONE',  ( 2.544523737882812053, 9.547976262117211732, 26.00000000000000711 ) ) ;
#28243 = LINE ( 'NONE', #33884, #30994 ) ;
#28242 = AXIS2_PLACEMENT_3D ( 'NONE', #39771, #1963, #18214 ) ;
#28244 = VERTEX_POINT ( 'NONE', #69431 ) ;
#28245 = AXIS2_PLACEMENT_3D ( 'NONE', #23584, #12964, #67072 ) ;
#28246 = CARTESIAN_POINT ( 'NONE',  ( -8.750000000000001776, 0.000000000000000000, -30.00000000000001066 ) ) ;
#28248 = DIRECTION ( 'NONE',  ( -1.000000000000000000, 0.000000000000000000, 0.000000000000000000 ) ) ;
#28247 = CARTESIAN_POINT ( 'NONE',  ( 7.450000000000006395, 7.250000000000000888, -11.50000000000000000 ) ) ;
#28249 = ORIENTED_EDGE ( 'NONE', *, *, #10920, .F. ) ;
#28251 = ORIENTED_EDGE ( 'NONE', *, *, #61148, .T. ) ;
#28250 = DIRECTION ( 'NONE',  ( 1.000000000000000000, 0.000000000000000000, 0.000000000000000000 ) ) ;
#28252 = VERTEX_POINT ( 'NONE', #35851 ) ;
#28253 = VECTOR ( 'NONE', #57972, 1000.000000000000000 ) ;
#28254 = CARTESIAN_POINT ( 'NONE',  ( -69.91216426482253610, 38.49351654963848546, 318.8237994620739073 ) ) ;
#28256 = AXIS2_PLACEMENT_3D ( 'NONE', #12170, #45384, #28775 ) ;
#28255 = CARTESIAN_POINT ( 'NONE',  ( 7.000000000000000000, -26.50000000000000000, 0.5000000000000000000 ) ) ;
#28257 = VECTOR ( 'NONE', #69369, 1000.000000000000000 ) ;
#28258 = EDGE_CURVE ( 'NONE', #66768, #32863, #28382, .T. ) ;
#28259 = CARTESIAN_POINT ( 'NONE',  ( 283.0000000000000568, -32.95000000000000284, 14.50000000000000000 ) ) ;
#28260 = ORIENTED_EDGE ( 'NONE', *, *, #69723, .F. ) ;
#28261 = ORIENTED_EDGE ( 'NONE', *, *, #60476, .T. ) ;
#28262 = AXIS2_PLACEMENT_3D ( 'NONE', #48, #42116, #21611 ) ;
#28263 = VECTOR ( 'NONE', #58547, 1000.000000000000000 ) ;
#28264 = DIRECTION ( 'NONE',  ( -1.836970198721029934E-16, 1.836970198721036344E-16, -1.000000000000000000 ) ) ;
#28265 = CARTESIAN_POINT ( 'NONE',  ( 46.39999999999999858, 21.00000000000000000, -2.250000000000000444 ) ) ;
#28266 = ORIENTED_EDGE ( 'NONE', *, *, #43767, .F. ) ;
#28267 = DIRECTION ( 'NONE',  ( -1.836970198721029934E-16, 1.836970198721036590E-16, -1.000000000000000000 ) ) ;
#28268 = DIRECTION ( 'NONE',  ( 0.000000000000000000, -1.000000000000000000, 0.000000000000000000 ) ) ;
#28269 = CARTESIAN_POINT ( 'NONE',  ( 6.619341603356846626, 4.734785091273825408, 455.0000000000000568 ) ) ;
#28270 = ADVANCED_FACE ( 'NONE', ( #68028 ), #4038, .F. ) ;
#28271 = ORIENTED_EDGE ( 'NONE', *, *, #34680, .F. ) ;
#28272 = ADVANCED_FACE ( 'NONE', ( #63430 ), #36196, .F. ) ;
#28273 = PLANE ( 'NONE',  #14372 ) ;
#28274 = CIRCLE ( 'NONE', #63269, 25.39999999999999858 ) ;
#28275 = DIRECTION ( 'NONE',  ( -0.000000000000000000, -0.000000000000000000, -1.000000000000000000 ) ) ;
#28277 = VERTEX_POINT ( 'NONE', #68380 ) ;
#28276 = SURFACE_SIDE_STYLE ('',( #39567 ) ) ;
#28279 = ORIENTED_EDGE ( 'NONE', *, *, #1934, .F. ) ;
#28278 = DIRECTION ( 'NONE',  ( -1.836970198721029934E-16, -1.836970198721010706E-16, 1.000000000000000000 ) ) ;
#28280 = LINE ( 'NONE', #49849, #29110 ) ;
#28281 = PLANE ( 'NONE',  #55547 ) ;
#28282 = CARTESIAN_POINT ( 'NONE',  ( 39.00000000000000000, 21.00000000000000000, -13.98999642601811999 ) ) ;
#28283 = CARTESIAN_POINT ( 'NONE',  ( 4.961189459950039904, -7.357023737882821379, 54.00000000000000711 ) ) ;
#28284 = PLANE ( 'NONE',  #64427 ) ;
#28285 = DIRECTION ( 'NONE',  ( 0.000000000000000000, 0.000000000000000000, -1.000000000000000000 ) ) ;
#28286 = ORIENTED_EDGE ( 'NONE', *, *, #33255, .F. ) ;
#28287 = CARTESIAN_POINT ( 'NONE',  ( 9.404523737882753309, 1.466476262117160312, 26.00000000000000711 ) ) ;
#28288 = AXIS2_PLACEMENT_3D ( 'NONE', #22629, #29299, #60099 ) ;
#28289 = DIRECTION ( 'NONE',  ( -1.000000000000000000, 0.000000000000000000, 0.000000000000000000 ) ) ;
#28291 = ORIENTED_EDGE ( 'NONE', *, *, #67802, .F. ) ;
#28290 = CARTESIAN_POINT ( 'NONE',  ( 283.0000000000000568, -25.14575131106457917, 17.35424868893542438 ) ) ;
#28292 = VECTOR ( 'NONE', #67233, 1000.000000000000000 ) ;
#28293 = PLANE ( 'NONE',  #53857 ) ;
#28294 = FACE_OUTER_BOUND ( 'NONE', #41757, .T. ) ;
#28295 = AXIS2_PLACEMENT_3D ( 'NONE', #48847, #15969, #69361 ) ;
#28296 = ORIENTED_EDGE ( 'NONE', *, *, #26789, .F. ) ;
#28297 = CARTESIAN_POINT ( 'NONE',  ( 7.250000000000005329, -7.249999999999998224, -22.00000000000000000 ) ) ;
#28298 = DIRECTION ( 'NONE',  ( 1.836970198721029934E-16, -1.836970198721036344E-16, 1.000000000000000000 ) ) ;
#28299 = VERTEX_POINT ( 'NONE', #14992 ) ;
#28300 = AXIS2_PLACEMENT_3D ( 'NONE', #15379, #46838, #20322 ) ;
#28301 = CARTESIAN_POINT ( 'NONE',  ( 69.92576880110368620, 0.000000000000000000, 281.4830310981151911 ) ) ;
#28302 = CARTESIAN_POINT ( 'NONE',  ( -8.393516549646745872, -4.396432944014549093, 455.0000000000000568 ) ) ;
#28303 = FACE_OUTER_BOUND ( 'NONE', #1739, .T. ) ;
#28304 = CARTESIAN_POINT ( 'NONE',  ( -7.259684009080030975, -7.811466277050769236, 455.0000000000000568 ) ) ;
#28305 = VECTOR ( 'NONE', #54957, 1000.000000000000000 ) ;
#28306 = LINE ( 'NONE', #12035, #7145 ) ;
#28307 = ORIENTED_EDGE ( 'NONE', *, *, #18596, .F. ) ;
#28308 = CARTESIAN_POINT ( 'NONE',  ( 30.00000000000000000, -8.959999999999999076, 17.04524521594300523 ) ) ;
#28309 = ORIENTED_EDGE ( 'NONE', *, *, #23393, .F. ) ;
#28310 = ORIENTED_EDGE ( 'NONE', *, *, #48734, .T. ) ;
#28311 = EDGE_CURVE ( 'NONE', #26875, #34775, #51770, .T. ) ;
#28312 = CARTESIAN_POINT ( 'NONE',  ( 10.50000000000000000, -9.690000000000001279, -5.000000000000000000 ) ) ;
#28313 = AXIS2_PLACEMENT_3D ( 'NONE', #4912, #68568, #4570 ) ;
#28314 = DIRECTION ( 'NONE',  ( 1.000000000000000000, -3.491481338843133750E-15, -1.836970198721036590E-16 ) ) ;
#28315 = EDGE_CURVE ( 'NONE', #41475, #55991, #15339, .T. ) ;
#28316 = CARTESIAN_POINT ( 'NONE',  ( 30.00000000000000000, -17.00000000000000000, 15.70499999999969809 ) ) ;
#28317 = CARTESIAN_POINT ( 'NONE',  ( -10.08346604330792751, -9.106483450353335840, 195.0000000000000284 ) ) ;
#28318 = ORIENTED_EDGE ( 'NONE', *, *, #47440, .T. ) ;
#28319 = ORIENTED_EDGE ( 'NONE', *, *, #35341, .F. ) ;
#28320 = LINE ( 'NONE', #23371, #17106 ) ;
#28321 = ORIENTED_EDGE ( 'NONE', *, *, #58646, .F. ) ;
#28322 = FACE_OUTER_BOUND ( 'NONE', #894, .T. ) ;
#28323 = PLANE ( 'NONE',  #45610 ) ;
#28324 = CIRCLE ( 'NONE', #14812, 24.99999999998794920 ) ;
#28325 = DIRECTION ( 'NONE',  ( 1.000000000000000000, -0.000000000000000000, 0.000000000000000000 ) ) ;
#28327 = CARTESIAN_POINT ( 'NONE',  ( 7.428221114745003462, -3.606483450353394016, 195.0000000000000284 ) ) ;
#28326 = CYLINDRICAL_SURFACE ( 'NONE', #59181, 2.204799999999997429 ) ;
#28328 = ORIENTED_EDGE ( 'NONE', *, *, #56768, .T. ) ;
#28330 = ORIENTED_EDGE ( 'NONE', *, *, #61218, .T. ) ;
#28329 = FACE_OUTER_BOUND ( 'NONE', #27025, .T. ) ;
#28331 = ORIENTED_EDGE ( 'NONE', *, *, #18420, .T. ) ;
#28332 = ORIENTED_EDGE ( 'NONE', *, *, #56284, .T. ) ;
#28333 = EDGE_CURVE ( 'NONE', #33655, #51399, #58895, .T. ) ;
#28334 = CARTESIAN_POINT ( 'NONE',  ( -7.813516549646711162, 11.99351654964660341, 455.0000000000000568 ) ) ;
#28335 = VECTOR ( 'NONE', #36725, 1000.000000000000000 ) ;
#28336 = CIRCLE ( 'NONE', #64501, 0.2000000000000005107 ) ;
#28337 = CYLINDRICAL_SURFACE ( 'NONE', #64769, 0.8128000000000145109 ) ;
#28338 = CIRCLE ( 'NONE', #54354, 0.2000000000000005107 ) ;
#28339 = PLANE ( 'NONE',  #29688 ) ;
#28340 = VERTEX_POINT ( 'NONE', #8972 ) ;
#28341 = ORIENTED_EDGE ( 'NONE', *, *, #64372, .T. ) ;
#28342 = VECTOR ( 'NONE', #36853, 1000.000000000000000 ) ;
#28343 = DIRECTION ( 'NONE',  ( 0.4999999999999827360, 0.000000000000000000, 0.8660254037844485886 ) ) ;
#28344 = CARTESIAN_POINT ( 'NONE',  ( 16.54633693294649888, -0.2717122460102533998, -21.66072723692568402 ) ) ;
#28345 = EDGE_LOOP ( 'NONE', ( #58390, #28732, #15861, #52990 ) ) ;
#28346 = CIRCLE ( 'NONE', #5811, 4.500000000000190958 ) ;
#28347 = AXIS2_PLACEMENT_3D ( 'NONE', #1980, #33800, #6597 ) ;
#28348 = ORIENTED_EDGE ( 'NONE', *, *, #25082, .T. ) ;
#28349 = CARTESIAN_POINT ( 'NONE',  ( 3.857023737882817827, 10.30047626211720413, 54.00000000000000711 ) ) ;
#28350 = CARTESIAN_POINT ( 'NONE',  ( 7.357023737882817827, -5.552858015815577808, 26.00000000000000711 ) ) ;
#28351 = ORIENTED_EDGE ( 'NONE', *, *, #22135, .F. ) ;
#28352 = EDGE_CURVE ( 'NONE', #47619, #51803, #57767, .T. ) ;
#28353 = VECTOR ( 'NONE', #14104, 1000.000000000000000 ) ;
#28354 = EDGE_CURVE ( 'NONE', #25494, #14048, #68738, .T. ) ;
#28355 = CARTESIAN_POINT ( 'NONE',  ( 275.0000000000000000, -25.69999999999924967, 14.52500000000000213 ) ) ;
#28356 = EDGE_CURVE ( 'NONE', #5469, #16596, #26295, .T. ) ;
#28358 = ORIENTED_EDGE ( 'NONE', *, *, #57933, .T. ) ;
#28357 = DIRECTION ( 'NONE',  ( -1.000000000000000000, 0.000000000000000000, 0.000000000000000000 ) ) ;
#28359 = ORIENTED_EDGE ( 'NONE', *, *, #65638, .F. ) ;
#28361 = FACE_OUTER_BOUND ( 'NONE', #41046, .T. ) ;
#28360 = AXIS2_PLACEMENT_3D ( 'NONE', #69799, #21355, #6133 ) ;
#28362 = DIRECTION ( 'NONE',  ( 0.000000000000000000, 0.000000000000000000, 1.000000000000000000 ) ) ;
#28363 = ADVANCED_FACE ( 'NONE', ( #10038 ), #30551, .F. ) ;
#28364 = DIRECTION ( 'NONE',  ( 1.000000000000000000, -0.000000000000000000, -0.000000000000000000 ) ) ;
#28365 = DIRECTION ( 'NONE',  ( 0.000000000000000000, -1.000000000000000000, 0.000000000000000000 ) ) ;
#28366 = LINE ( 'NONE', #66201, #22163 ) ;
#28367 = CARTESIAN_POINT ( 'NONE',  ( -6.817976262117261044, 9.722976262117182245, 54.00000000000000711 ) ) ;
#28368 = EDGE_CURVE ( 'NONE', #5395, #32193, #63382, .T. ) ;
#28369 = ORIENTED_EDGE ( 'NONE', *, *, #54669, .F. ) ;
#28370 = CARTESIAN_POINT ( 'NONE',  ( 15.00000000000000000, -21.00000000000000000, -5.000000000000000000 ) ) ;
#28371 = EDGE_CURVE ( 'NONE', #35366, #64273, #19939, .T. ) ;
#28373 = ORIENTED_EDGE ( 'NONE', *, *, #65943, .F. ) ;
#28372 = LINE ( 'NONE', #1174, #18618 ) ;
#28374 = LINE ( 'NONE', #23768, #21959 ) ;
#28375 = DIRECTION ( 'NONE',  ( 1.000000000000000000, 0.000000000000000000, 0.000000000000000000 ) ) ;
#28376 = CARTESIAN_POINT ( 'NONE',  ( -18.85410196625000268, -17.50000000000000000, -21.50000000000000000 ) ) ;
#28377 = CARTESIAN_POINT ( 'NONE',  ( 30.00000000000000000, -9.199999999999999289, -12.34999999999989839 ) ) ;
#28378 = CARTESIAN_POINT ( 'NONE',  ( -15.50000000000000000, -5.000000000000000000, -22.50000000000000000 ) ) ;
#28379 = VERTEX_POINT ( 'NONE', #31275 ) ;
#28380 = EDGE_LOOP ( 'NONE', ( #21970, #8470, #44946, #8065 ) ) ;
#28381 = CARTESIAN_POINT ( 'NONE',  ( 283.0000000000000568, -23.65000000000000568, 12.40000000000000213 ) ) ;
#28382 = CIRCLE ( 'NONE', #55500, 2.204799999999997429 ) ;
#28383 = DIRECTION ( 'NONE',  ( 1.000000000000000000, -7.304098846218132892E-15, -2.683482381803073952E-30 ) ) ;
#28384 = STYLED_ITEM ( 'NONE', ( #1746 ), #42807 ) ;
#28385 = ORIENTED_EDGE ( 'NONE', *, *, #52482, .T. ) ;
#28386 = LINE ( 'NONE', #23440, #64369 ) ;
#28387 = VERTEX_POINT ( 'NONE', #63784 ) ;
#28388 = ORIENTED_EDGE ( 'NONE', *, *, #36622, .T. ) ;
#28389 = LINE ( 'NONE', #49620, #47145 ) ;
#28390 = DIRECTION ( 'NONE',  ( 0.000000000000000000, 0.000000000000000000, 1.000000000000000000 ) ) ;
#28391 = EDGE_LOOP ( 'NONE', ( #27072, #33026, #69957, #52102 ) ) ;
#28392 = DIRECTION ( 'NONE',  ( -3.491481338843133355E-15, -1.000000000000000000, -1.836970198721029934E-16 ) ) ;
#28393 = FACE_OUTER_BOUND ( 'NONE', #64956, .T. ) ;
#28394 = VECTOR ( 'NONE', #34301, 1000.000000000000000 ) ;
#28395 = CARTESIAN_POINT ( 'NONE',  ( 1.000000000000000000, -21.00000000000000000, 0.000000000000000000 ) ) ;
#28396 = ORIENTED_EDGE ( 'NONE', *, *, #32117, .F. ) ;
#28398 = EDGE_LOOP ( 'NONE', ( #21493, #26264, #10112, #47914, #36918, #30773, #27126, #48002 ) ) ;
#28397 = CARTESIAN_POINT ( 'NONE',  ( 41.09999999999999432, -21.00000000000000000, -13.86939075806900057 ) ) ;
#28399 = CARTESIAN_POINT ( 'NONE',  ( -7.593516549646838421, -11.78648345035340839, 455.0000000000000568 ) ) ;
#28400 = PLANE ( 'NONE',  #19206 ) ;
#28401 = DIRECTION ( 'NONE',  ( -1.000000000000000000, 0.000000000000000000, 0.000000000000000000 ) ) ;
#28402 = CARTESIAN_POINT ( 'NONE',  ( -25.50000000000000355, -15.50000000000000000, -22.50000000000000000 ) ) ;
#28403 = ORIENTED_EDGE ( 'NONE', *, *, #63608, .F. ) ;
#28404 = AXIS2_PLACEMENT_3D ( 'NONE', #16671, #9975, #37195 ) ;
#28405 = DIRECTION ( 'NONE',  ( 1.047444401652940007E-14, 1.000000000000000000, 0.000000000000000000 ) ) ;
#28406 = EDGE_CURVE ( 'NONE', #47490, #3732, #47512, .T. ) ;
#28407 = CARTESIAN_POINT ( 'NONE',  ( 4.406483450353420928, 11.77351654964658501, 455.0000000000000568 ) ) ;
#28408 = ORIENTED_EDGE ( 'NONE', *, *, #55649, .T. ) ;
#28409 = ORIENTED_EDGE ( 'NONE', *, *, #64737, .F. ) ;
#28410 = ORIENTED_EDGE ( 'NONE', *, *, #27157, .T. ) ;
#28411 = EDGE_CURVE ( 'NONE', #29645, #37690, #4397, .T. ) ;
#28412 = CARTESIAN_POINT ( 'NONE',  ( -7.252248008019455128, 5.380658396643134722, 195.0000000000000284 ) ) ;
#28413 = CARTESIAN_POINT ( 'NONE',  ( 8.406483450353334774, 4.383466043307768345, 195.0000000000000284 ) ) ;
#28414 = ADVANCED_BREP_SHAPE_REPRESENTATION ( '', ( #19304, #45918 ), #69670 ) ;
#28415 = LINE ( 'NONE', #13203, #49594 ) ;
#28416 = VECTOR ( 'NONE', #14986, 1000.000000000000000 ) ;
#28417 = DIRECTION ( 'NONE',  ( 1.836970198721029934E-16, 1.836970198721010706E-16, -1.000000000000000000 ) ) ;
#28418 = ORIENTED_EDGE ( 'NONE', *, *, #64919, .T. ) ;
#28420 = EDGE_CURVE ( 'NONE', #54414, #18330, #69029, .T. ) ;
#28419 = ORIENTED_EDGE ( 'NONE', *, *, #31386, .F. ) ;
#28421 = ORIENTED_EDGE ( 'NONE', *, *, #47053, .T. ) ;
#28422 = LINE ( 'NONE', #22782, #45209 ) ;
#28423 = ORIENTED_EDGE ( 'NONE', *, *, #27268, .F. ) ;
#28424 = ORIENTED_EDGE ( 'NONE', *, *, #9200, .T. ) ;
#28425 = ADVANCED_FACE ( 'NONE', ( #35486 ), #13930, .F. ) ;
#28426 = VERTEX_POINT ( 'NONE', #38641 ) ;
#28427 = ORIENTED_EDGE ( 'NONE', *, *, #3176, .F. ) ;
#28428 = CARTESIAN_POINT ( 'NONE',  ( 283.0000000000000568, -42.50000000000000000, -15.10000000000000142 ) ) ;
#28429 = CIRCLE ( 'NONE', #41973, 3.999999999999993339 ) ;
#28431 = ORIENTED_EDGE ( 'NONE', *, *, #3055, .T. ) ;
#28430 = FACE_OUTER_BOUND ( 'NONE', #36624, .T. ) ;
#28432 = DIRECTION ( 'NONE',  ( 1.000000000000000000, -3.491481338843132961E-15, -1.836970198721036344E-16 ) ) ;
#28433 = PRODUCT_DEFINITION_SHAPE ( 'NONE', 'NONE',  #34822 ) ;
#28434 = PLANE ( 'NONE',  #8068 ) ;
#28435 = EDGE_CURVE ( 'NONE', #8968, #20434, #38304, .T. ) ;
#28436 = FACE_OUTER_BOUND ( 'NONE', #24028, .T. ) ;
#28438 = VERTEX_POINT ( 'NONE', #49259 ) ;
#28437 = CARTESIAN_POINT ( 'NONE',  ( 39.90000000000000568, -21.00000000000000000, 13.86939075806900057 ) ) ;
#28439 = DIRECTION ( 'NONE',  ( 0.000000000000000000, -1.000000000000000000, 0.000000000000000000 ) ) ;
#28440 = VECTOR ( 'NONE', #14765, 1000.000000000000000 ) ;
#28441 = CARTESIAN_POINT ( 'NONE',  ( 7.250000000000005329, -8.249999999999998224, -14.00000000000000000 ) ) ;
#28442 = CARTESIAN_POINT ( 'NONE',  ( 25.57999999999999829, 0.000000000000000000, 0.000000000000000000 ) ) ;
#28443 = ADVANCED_FACE ( 'NONE', ( #54916 ), #835, .F. ) ;
#28444 = ORIENTED_EDGE ( 'NONE', *, *, #46788, .F. ) ;
#28445 = VECTOR ( 'NONE', #21223, 1000.000000000000114 ) ;
#28446 = CARTESIAN_POINT ( 'NONE',  ( 9.689999999999999503, -10.50000000000000178, -5.000000000000000000 ) ) ;
#28447 = EDGE_CURVE ( 'NONE', #53340, #47124, #32985, .T. ) ;
#28448 = LINE ( 'NONE', #1576, #12845 ) ;
#28449 = DIRECTION ( 'NONE',  ( 0.000000000000000000, 0.000000000000000000, -1.000000000000000000 ) ) ;
#28450 = VERTEX_POINT ( 'NONE', #64482 ) ;
#28451 = LINE ( 'NONE', #60284, #66316 ) ;
#28452 = VECTOR ( 'NONE', #24823, 1000.000000000000000 ) ;
#28453 = CARTESIAN_POINT ( 'NONE',  ( 7.000000000000000000, -38.10000000000000142, -8.400000000000000355 ) ) ;
#28454 = DIRECTION ( 'NONE',  ( -1.047444401652940007E-14, -1.000000000000000000, 0.000000000000000000 ) ) ;
#28455 = EDGE_CURVE ( 'NONE', #34056, #60969, #49591, .T. ) ;
#28456 = ORIENTED_EDGE ( 'NONE', *, *, #21207, .F. ) ;
#28457 = DIRECTION ( 'NONE',  ( 0.7071067811865470176, 0.7071067811865480168, 0.000000000000000000 ) ) ;
#28458 = DIRECTION ( 'NONE',  ( 1.836970198721029934E-16, 1.836970198721010706E-16, -1.000000000000000000 ) ) ;
#28459 = PLANE ( 'NONE',  #18611 ) ;
#28460 = DIRECTION ( 'NONE',  ( -1.000000000000000000, 0.000000000000000000, 0.000000000000000000 ) ) ;
#28461 = ORIENTED_EDGE ( 'NONE', *, *, #22755, .T. ) ;
#28462 = CARTESIAN_POINT ( 'NONE',  ( 9.703773737882785966, -8.580623737882856261, 54.00000000000000711 ) ) ;
#28463 = CARTESIAN_POINT ( 'NONE',  ( -2.893516549646828473, -10.92648345035345514, 455.0000000000000568 ) ) ;
#28464 = CARTESIAN_POINT ( 'NONE',  ( -7.415254214038336400, 3.593516549646602609, 455.0000000000000568 ) ) ;
#28465 = DIRECTION ( 'NONE',  ( 1.836970198721029934E-16, 1.836970198721010706E-16, -1.000000000000000000 ) ) ;
#28466 = CYLINDRICAL_SURFACE ( 'NONE', #13895, 0.1999999999999987899 ) ;
#28467 = ORIENTED_EDGE ( 'NONE', *, *, #43925, .F. ) ;
#28468 = CARTESIAN_POINT ( 'NONE',  ( -14.25000000000000000, -0.2038245569916330158, -21.77831216351300014 ) ) ;
#28469 = LINE ( 'NONE', #44728, #3411 ) ;
#28470 = CIRCLE ( 'NONE', #60084, 3.500000000000003109 ) ;
#28471 = CARTESIAN_POINT ( 'NONE',  ( -8.250000000000001776, -7.249999999999998224, -19.00000000000000000 ) ) ;
#28472 = EDGE_CURVE ( 'NONE', #7472, #17145, #21689, .T. ) ;
#28473 = DIRECTION ( 'NONE',  ( -1.000000000000000000, 0.000000000000000000, 0.000000000000000000 ) ) ;
#28474 = FACE_OUTER_BOUND ( 'NONE', #18525, .T. ) ;
#28475 = AXIS2_PLACEMENT_3D ( 'NONE', #1332, #39830, #6629 ) ;
#28476 = EDGE_LOOP ( 'NONE', ( #34911, #3932, #68013, #16635 ) ) ;
#28477 = VERTEX_POINT ( 'NONE', #48220 ) ;
#28478 = EDGE_CURVE ( 'NONE', #26351, #41781, #38548, .T. ) ;
#28479 = CARTESIAN_POINT ( 'NONE',  ( -7.450000000000001954, 7.250000000000000000, -7.500000000000000000 ) ) ;
#28480 = CARTESIAN_POINT ( 'NONE',  ( 25.57999999999999829, 0.000000000000000000, 0.000000000000000000 ) ) ;
#28481 = EDGE_LOOP ( 'NONE', ( #67658, #15729, #52001, #52309 ) ) ;
#28482 = EDGE_CURVE ( 'NONE', #45353, #39173, #45283, .T. ) ;
#28483 = AXIS2_PLACEMENT_3D ( 'NONE', #35021, #51294, #7798 ) ;
#28484 = CARTESIAN_POINT ( 'NONE',  ( 12.00648345035340903, 7.813516549646560172, 455.0000000000000568 ) ) ;
#28485 = EDGE_CURVE ( 'NONE', #4816, #32597, #473, .T. ) ;
#28486 = ORIENTED_EDGE ( 'NONE', *, *, #6927, .F. ) ;
#28487 = AXIS2_PLACEMENT_3D ( 'NONE', #52888, #69124, #20678 ) ;
#28488 = DIRECTION ( 'NONE',  ( 0.000000000000000000, 0.000000000000000000, -1.000000000000000000 ) ) ;
#28489 = VERTEX_POINT ( 'NONE', #22035 ) ;
#28490 = ADVANCED_FACE ( 'NONE', ( #6471 ), #10383, .T. ) ;
#28491 = ORIENTED_EDGE ( 'NONE', *, *, #58145, .T. ) ;
#28492 = CARTESIAN_POINT ( 'NONE',  ( 8.250000000000005329, -7.249999999999998224, -26.00000000000001066 ) ) ;
#28493 = CARTESIAN_POINT ( 'NONE',  ( -8.689999999999999503, -9.750000000000001776, -7.000000000000000000 ) ) ;
#28494 = DIRECTION ( 'NONE',  ( -1.000000000000000000, 0.000000000000000000, 0.000000000000000000 ) ) ;
#28496 =( BOUNDED_CURVE ( )  B_SPLINE_CURVE ( 3, ( #22605, #5327, #54099, #69674 ),
 .UNSPECIFIED., .F., .F. ) 
 B_SPLINE_CURVE_WITH_KNOTS ( ( 4, 4 ),
 ( 2.245927859731928322, 2.418858405776365572 ),
 .UNSPECIFIED. ) 
 CURVE ( )  GEOMETRIC_REPRESENTATION_ITEM ( )  RATIONAL_B_SPLINE_CURVE ( ( 1.000000000000000000, 0.9975094710839678136, 0.9975094710839678136, 1.000000000000000000 ) ) 
 REPRESENTATION_ITEM ( '' )  );
#28495 = DIRECTION ( 'NONE',  ( 0.000000000000000000, -1.000000000000000000, 0.000000000000000000 ) ) ;
#28497 = AXIS2_PLACEMENT_3D ( 'NONE', #46845, #25286, #9731 ) ;
#28498 = ORIENTED_EDGE ( 'NONE', *, *, #48835, .T. ) ;
#28499 = ADVANCED_FACE ( 'NONE', ( #64148 ), #60193, .F. ) ;
#28500 = ORIENTED_EDGE ( 'NONE', *, *, #25862, .F. ) ;
#28501 = PLANE ( 'NONE',  #25609 ) ;
#28502 = EDGE_CURVE ( 'NONE', #21801, #1690, #50948, .T. ) ;
#28503 = AXIS2_PLACEMENT_3D ( 'NONE', #60375, #5959, #11932 ) ;
#28504 = LINE ( 'NONE', #11545, #31675 ) ;
#28505 = EDGE_LOOP ( 'NONE', ( #36356, #4174, #59005, #49668 ) ) ;
#28506 = VECTOR ( 'NONE', #3578, 1000.000000000000000 ) ;
#28507 = ORIENTED_EDGE ( 'NONE', *, *, #33302, .F. ) ;
#28508 = EDGE_CURVE ( 'NONE', #7626, #4514, #64550, .T. ) ;
#28509 = EDGE_CURVE ( 'NONE', #42130, #38006, #33336, .T. ) ;
#28510 = VERTEX_POINT ( 'NONE', #11751 ) ;
#28511 = CARTESIAN_POINT ( 'NONE',  ( -8.079219948824906794, 8.697938382363059162, 26.00000000000000711 ) ) ;
#28512 = AXIS2_PLACEMENT_3D ( 'NONE', #26136, #25791, #57250 ) ;
#28513 = DIRECTION ( 'NONE',  ( -1.000000000000000000, 8.540177112501197482E-15, 3.137610169492823463E-30 ) ) ;
#28515 = VERTEX_POINT ( 'NONE', #1164 ) ;
#28514 = CARTESIAN_POINT ( 'NONE',  ( -11.31351654964670850, 4.193516549646605363, 455.0000000000000568 ) ) ;
#28516 = ADVANCED_FACE ( 'NONE', ( #37262 ), #26647, .F. ) ;
#28517 = DIRECTION ( 'NONE',  ( 1.000000000000000000, 0.000000000000000000, 0.000000000000000000 ) ) ;
#28518 = CARTESIAN_POINT ( 'NONE',  ( -7.250000000000001776, -7.249999999999998224, -19.00000000000000000 ) ) ;
#28519 = EDGE_LOOP ( 'NONE', ( #69390, #59321, #67559, #2255, #1898, #51568 ) ) ;
#28520 = VERTEX_POINT ( 'NONE', #32299 ) ;
#28521 = AXIS2_PLACEMENT_3D ( 'NONE', #66319, #35163, #7243 ) ;
#28522 = DIRECTION ( 'NONE',  ( -8.673617379884087537E-15, -1.000000000000000000, 0.000000000000000000 ) ) ;
#28523 = DIRECTION ( 'NONE',  ( -1.000000000000000000, 0.000000000000000000, 0.000000000000000000 ) ) ;
#28524 = VECTOR ( 'NONE', #56454, 1000.000000000000000 ) ;
#28525 = EDGE_CURVE ( 'NONE', #4544, #19912, #59167, .T. ) ;
#28526 = DIRECTION ( 'NONE',  ( 1.000000000000000000, -0.000000000000000000, -0.000000000000000000 ) ) ;
#28527 = EDGE_CURVE ( 'NONE', #10161, #29039, #2529, .T. ) ;
#28528 = LINE ( 'NONE', #23224, #35756 ) ;
#28529 = CARTESIAN_POINT ( 'NONE',  ( 49.00000000000000000, -0.2000000000089119934, -8.913009219568841313E-12 ) ) ;
#28531 = ORIENTED_EDGE ( 'NONE', *, *, #44012, .T. ) ;
#28530 = CARTESIAN_POINT ( 'NONE',  ( -27.50000000000000000, -5.200000000000001066, -22.50000000000000000 ) ) ;
#28532 = ORIENTED_EDGE ( 'NONE', *, *, #25327, .T. ) ;
#28533 = VECTOR ( 'NONE', #46688, 1000.000000000000000 ) ;
#28534 = CARTESIAN_POINT ( 'NONE',  ( 28.90000000000000213, -14.06939075806902117, -20.80000000000000426 ) ) ;
#28535 = FACE_OUTER_BOUND ( 'NONE', #58567, .T. ) ;
#28536 = CARTESIAN_POINT ( 'NONE',  ( -8.250000000000001776, -7.249999999999998224, -11.00000000000000000 ) ) ;
#28537 = DIRECTION ( 'NONE',  ( 1.000000000000000000, 0.000000000000000000, 0.000000000000000000 ) ) ;
#28538 = DIRECTION ( 'NONE',  ( -0.5773502691896257311, 0.5773502691896257311, 0.5773502691896257311 ) ) ;
#28539 = ORIENTED_EDGE ( 'NONE', *, *, #51281, .F. ) ;
#28540 = DIRECTION ( 'NONE',  ( 0.000000000000000000, 0.000000000000000000, 1.000000000000000000 ) ) ;
#28541 = DIRECTION ( 'NONE',  ( 0.000000000000000000, 1.000000000000000000, 0.000000000000000000 ) ) ;
#28542 = FACE_OUTER_BOUND ( 'NONE', #9932, .T. ) ;
#28543 = PLANE ( 'NONE',  #31098 ) ;
#28544 = LINE ( 'NONE', #59356, #20243 ) ;
#28545 = PLANE ( 'NONE',  #3643 ) ;
#28546 = AXIS2_PLACEMENT_3D ( 'NONE', #46553, #68131, #19675 ) ;
#28547 = CARTESIAN_POINT ( 'NONE',  ( 28.00000000000000000, -17.00000000000000000, -15.70499999999969809 ) ) ;
#28548 = AXIS2_PLACEMENT_3D ( 'NONE', #51886, #57187, #45513 ) ;
#28549 = ADVANCED_FACE ( 'NONE', ( #23418 ), #66199, .F. ) ;
#28550 = EDGE_LOOP ( 'NONE', ( #14972, #29916, #40848, #4975 ) ) ;
#28551 = CARTESIAN_POINT ( 'NONE',  ( 2.906483450353417375, 10.08346604330775875, 455.0000000000000568 ) ) ;
#28552 = CARTESIAN_POINT ( 'NONE',  ( 7.000000000000000000, -25.93000000000544958, -9.412893218815410634 ) ) ;
#28553 = ORIENTED_EDGE ( 'NONE', *, *, #11730, .T. ) ;
#28554 = LINE ( 'NONE', #19000, #13061 ) ;
#28555 = LINE ( 'NONE', #50129, #40255 ) ;
#28556 = LINE ( 'NONE', #50130, #11732 ) ;
#28558 = CIRCLE ( 'NONE', #48932, 1.000000000000000000 ) ;
#28557 = CARTESIAN_POINT ( 'NONE',  ( 16.75000000000000000, -0.2038245569916320166, -21.77831216351300014 ) ) ;
#28559 = LINE ( 'NONE', #55449, #42950 ) ;
#28560 = EDGE_LOOP ( 'NONE', ( #3925, #66336, #49180, #63566, #41516, #48804 ) ) ;
#28561 = EDGE_CURVE ( 'NONE', #50939, #65427, #60542, .T. ) ;
#28562 = DIRECTION ( 'NONE',  ( 0.000000000000000000, -0.7071067811865496822, 0.7071067811865454633 ) ) ;
#28563 = VECTOR ( 'NONE', #25857, 1000.000000000000000 ) ;
#28564 = EDGE_LOOP ( 'NONE', ( #14368, #68249, #27474, #5295 ) ) ;
#28565 = CARTESIAN_POINT ( 'NONE',  ( -3.667976262117227382, 9.897976262117168744, 54.00000000000000711 ) ) ;
#28566 = ORIENTED_EDGE ( 'NONE', *, *, #52154, .F. ) ;
#28567 = EDGE_CURVE ( 'NONE', #46469, #46340, #8180, .T. ) ;
#28568 = DIRECTION ( 'NONE',  ( 1.836970198721029934E-16, 1.836970198721010706E-16, -1.000000000000000000 ) ) ;
#28569 = EDGE_CURVE ( 'NONE', #55707, #41932, #44610, .T. ) ;
#28570 = VECTOR ( 'NONE', #54249, 1000.000000000000000 ) ;
#28571 = EDGE_CURVE ( 'NONE', #44549, #68445, #146, .T. ) ;
#28572 = DIRECTION ( 'NONE',  ( 1.000000000000000000, 0.000000000000000000, 0.000000000000000000 ) ) ;
#28573 = FACE_OUTER_BOUND ( 'NONE', #34024, .T. ) ;
#28574 = ORIENTED_EDGE ( 'NONE', *, *, #15756, .T. ) ;
#28575 = ADVANCED_FACE ( 'NONE', ( #39326 ), #35050, .F. ) ;
#28576 = VERTEX_POINT ( 'NONE', #18091 ) ;
#28577 = EDGE_CURVE ( 'NONE', #27584, #60914, #12777, .T. ) ;
#28578 = VECTOR ( 'NONE', #6613, 1000.000000000000000 ) ;
#28579 = DIRECTION ( 'NONE',  ( -1.000000000000000000, 0.000000000000000000, 0.000000000000000000 ) ) ;
#28580 = ORIENTED_EDGE ( 'NONE', *, *, #19213, .F. ) ;
#28581 = VERTEX_POINT ( 'NONE', #61930 ) ;
#28582 = CARTESIAN_POINT ( 'NONE',  ( 283.0000000000000568, -26.06132420600899735, 10.13999572156699891 ) ) ;
#28583 = LINE ( 'NONE', #28932, #32469 ) ;
#28584 = DIRECTION ( 'NONE',  ( -1.000000000000000000, 0.000000000000000000, 0.000000000000000000 ) ) ;
#28585 = VERTEX_POINT ( 'NONE', #38978 ) ;
#28586 = VECTOR ( 'NONE', #353, 1000.000000000000000 ) ;
#28587 = DIRECTION ( 'NONE',  ( -1.000000000000000000, 0.000000000000000000, 0.000000000000000000 ) ) ;
#28589 = DIRECTION ( 'NONE',  ( -1.000000000000000000, 0.000000000000000000, -0.000000000000000000 ) ) ;
#28588 = DIRECTION ( 'NONE',  ( 0.000000000000000000, 0.7096009616570518874, 0.7046037717862339012 ) ) ;
#28590 = EDGE_LOOP ( 'NONE', ( #55195, #38387, #45006, #40335 ) ) ;
#28592 = VERTEX_POINT ( 'NONE', #45308 ) ;
#28591 = CARTESIAN_POINT ( 'NONE',  ( -30.00000000000000000, -12.00000000000000000, -12.20000000000000107 ) ) ;
#28593 = ORIENTED_EDGE ( 'NONE', *, *, #14971, .T. ) ;
#28594 = DIRECTION ( 'NONE',  ( 0.000000000000000000, 0.000000000000000000, 1.000000000000000000 ) ) ;
#28595 = LINE ( 'NONE', #28255, #24264 ) ;
#28596 = VERTEX_POINT ( 'NONE', #29062 ) ;
#28597 = DIRECTION ( 'NONE',  ( 1.000000000000000000, -0.000000000000000000, 0.000000000000000000 ) ) ;
#28598 = AXIS2_PLACEMENT_3D ( 'NONE', #48148, #69722, #52776 ) ;
#28599 = AXIS2_PLACEMENT_3D ( 'NONE', #13803, #40334, #61897 ) ;
#28600 = DIRECTION ( 'NONE',  ( 0.8660254037844563602, 0.4999999999999695244, 2.509347957447842799E-16 ) ) ;
#28601 = ORIENTED_EDGE ( 'NONE', *, *, #25759, .F. ) ;
#28602 = ORIENTED_EDGE ( 'NONE', *, *, #44237, .F. ) ;
#28603 = VECTOR ( 'NONE', #37286, 1000.000000000000000 ) ;
#28605 = CARTESIAN_POINT ( 'NONE',  ( -8.250000000000001776, 0.000000000000000000, -17.00000000000000000 ) ) ;
#28604 = AXIS2_PLACEMENT_3D ( 'NONE', #2651, #24230, #67369 ) ;
#28606 = CIRCLE ( 'NONE', #54631, 25.39999999999999858 ) ;
#28607 = CARTESIAN_POINT ( 'NONE',  ( 41.09999999999999432, 13.66939075806899950, 20.80000000000000426 ) ) ;
#28608 = EDGE_LOOP ( 'NONE', ( #32466, #35041, #10271, #26968 ) ) ;
#28609 = FACE_OUTER_BOUND ( 'NONE', #63057, .T. ) ;
#28610 = DIRECTION ( 'NONE',  ( 0.000000000000000000, -1.000000000000000000, 0.000000000000000000 ) ) ;
#28611 = AXIS2_PLACEMENT_3D ( 'NONE', #45934, #35660, #67514 ) ;
#28612 = AXIS2_PLACEMENT_3D ( 'NONE', #65834, #22705, #5429 ) ;
#28613 = DIRECTION ( 'NONE',  ( 1.000000000000000000, -5.981805089575194965E-17, 0.000000000000000000 ) ) ;
#28614 = ORIENTED_EDGE ( 'NONE', *, *, #19816, .F. ) ;
#28615 = ADVANCED_FACE ( 'NONE', ( #29748 ), #51322, .F. ) ;
#28616 = FACE_OUTER_BOUND ( 'NONE', #16610, .T. ) ;
#28617 = DIRECTION ( 'NONE',  ( -1.000000000000000000, 0.000000000000000000, 0.000000000000000000 ) ) ;
#28620 = VERTEX_POINT ( 'NONE', #56631 ) ;
#28619 = EDGE_CURVE ( 'NONE', #66569, #13296, #12431, .T. ) ;
#28618 = CARTESIAN_POINT ( 'NONE',  ( 7.250000000000005329, -7.249999999999998224, -26.00000000000001066 ) ) ;
#28622 = VERTEX_POINT ( 'NONE', #34708 ) ;
#28621 = FACE_OUTER_BOUND ( 'NONE', #42905, .T. ) ;
#28623 = DIRECTION ( 'NONE',  ( 0.000000000000000000, 0.000000000000000000, 1.000000000000000000 ) ) ;
#28624 = DIRECTION ( 'NONE',  ( 0.7071067811865474617, 0.7071067811865474617, 0.000000000000000000 ) ) ;
#28625 = PLANE ( 'NONE',  #7570 ) ;
#28626 = FACE_OUTER_BOUND ( 'NONE', #25053, .T. ) ;
#28627 = DIRECTION ( 'NONE',  ( 1.000000000000000000, 0.000000000000000000, 0.000000000000000000 ) ) ;
#28628 = ORIENTED_EDGE ( 'NONE', *, *, #25314, .F. ) ;
#28629 = CARTESIAN_POINT ( 'NONE',  ( -3.663616288757086004, -4.149127210878724270, 26.00000000000000711 ) ) ;
#28630 = LINE ( 'NONE', #1417, #31610 ) ;
#28631 = DIRECTION ( 'NONE',  ( -1.000000000000000000, 0.000000000000000000, 0.000000000000000000 ) ) ;
#28633 = ORIENTED_EDGE ( 'NONE', *, *, #49984, .F. ) ;
#28632 = CARTESIAN_POINT ( 'NONE',  ( 7.272650909786598561, -4.201500623656027500, 195.0000000000000284 ) ) ;
#28634 = FACE_OUTER_BOUND ( 'NONE', #37392, .T. ) ;
#28635 = CARTESIAN_POINT ( 'NONE',  ( -15.50000000000000000, -0.4000000000000000222, 22.50000000000000000 ) ) ;
#28636 = ORIENTED_EDGE ( 'NONE', *, *, #12768, .F. ) ;
#28637 = DIRECTION ( 'NONE',  ( 0.000000000000000000, 0.000000000000000000, -1.000000000000000000 ) ) ;
#28638 = DIRECTION ( 'NONE',  ( 0.000000000000000000, -3.673940397442059868E-16, 1.000000000000000000 ) ) ;
#28639 = ORIENTED_EDGE ( 'NONE', *, *, #40166, .T. ) ;
#28640 = DIRECTION ( 'NONE',  ( -0.000000000000000000, 1.000000000000000000, -0.000000000000000000 ) ) ;
#28641 = PLANE ( 'NONE',  #45857 ) ;
#28642 = FACE_BOUND ( 'NONE', #39114, .T. ) ;
#28643 = APPLICATION_CONTEXT ( 'automotive_design' ) ;
#28644 = DIRECTION ( 'NONE',  ( 0.000000000000000000, 0.000000000000000000, 1.000000000000000000 ) ) ;
#28645 = EDGE_CURVE ( 'NONE', #39887, #15366, #57717, .T. ) ;
#28646 = DIRECTION ( 'NONE',  ( 0.000000000000000000, -3.673940397442059868E-16, 1.000000000000000000 ) ) ;
#28647 = VECTOR ( 'NONE', #4240, 1000.000000000000000 ) ;
#28648 = VERTEX_POINT ( 'NONE', #50630 ) ;
#28649 = DIRECTION ( 'NONE',  ( -0.000000000000000000, -0.000000000000000000, -1.000000000000000000 ) ) ;
#28650 = ORIENTED_EDGE ( 'NONE', *, *, #41942, .T. ) ;
#28651 = VERTEX_POINT ( 'NONE', #2190 ) ;
#28652 = DIRECTION ( 'NONE',  ( 0.000000000000000000, -0.6801302850037772574, -0.7330912599538208507 ) ) ;
#28653 = LINE ( 'NONE', #30323, #51870 ) ;
#28654 = ADVANCED_FACE ( 'NONE', ( #6790 ), #23757, .F. ) ;
#28655 =( GEOMETRIC_REPRESENTATION_CONTEXT ( 3 ) GLOBAL_UNCERTAINTY_ASSIGNED_CONTEXT ( ( #54287 ) ) GLOBAL_UNIT_ASSIGNED_CONTEXT ( ( #43281, #37993, #54953 ) ) REPRESENTATION_CONTEXT ( 'NONE', 'WORKASPACE' ) );
#28656 = CIRCLE ( 'NONE', #47853, 0.3499999999999285905 ) ;
#28657 = EDGE_CURVE ( 'NONE', #55692, #51462, #39998, .T. ) ;
#28658 = EDGE_CURVE ( 'NONE', #52522, #31415, #56281, .T. ) ;
#28659 = CIRCLE ( 'NONE', #68192, 24.99999999998784972 ) ;
#28660 = FILL_AREA_STYLE_COLOUR ( '', #44497 ) ;
#28661 = VECTOR ( 'NONE', #37568, 1000.000000000000000 ) ;
#28662 = VECTOR ( 'NONE', #56040, 1000.000000000000000 ) ;
#28663 = CARTESIAN_POINT ( 'NONE',  ( 7.250000000000005329, 7.250000000000000888, -30.00000000000001066 ) ) ;
#28664 = VERTEX_POINT ( 'NONE', #49929 ) ;
#28665 = EDGE_CURVE ( 'NONE', #64711, #66347, #1490, .T. ) ;
#28666 = ORIENTED_EDGE ( 'NONE', *, *, #12214, .F. ) ;
#28667 = EDGE_CURVE ( 'NONE', #38006, #60907, #40372, .T. ) ;
#28668 = CARTESIAN_POINT ( 'NONE',  ( 7.450000000000006395, 7.250000000000000888, -12.00000000000000000 ) ) ;
#28669 = ORIENTED_EDGE ( 'NONE', *, *, #69008, .T. ) ;
#28670 = DIRECTION ( 'NONE',  ( -1.836970198721029934E-16, -1.836970198721010706E-16, 1.000000000000000000 ) ) ;
#28671 = CARTESIAN_POINT ( 'NONE',  ( 19.90000000000000213, -14.06939075806900874, 20.80000000000001137 ) ) ;
#28672 = EDGE_CURVE ( 'NONE', #35542, #868, #4314, .T. ) ;
#28673 = LINE ( 'NONE', #34670, #2612 ) ;
#28674 = VECTOR ( 'NONE', #13192, 1000.000000000000000 ) ;
#28675 = FACE_BOUND ( 'NONE', #58881, .T. ) ;
#28677 = DIRECTION ( 'NONE',  ( -0.000000000000000000, -0.000000000000000000, 1.000000000000000000 ) ) ;
#28676 = DIRECTION ( 'NONE',  ( 0.000000000000000000, 0.000000000000000000, -1.000000000000000000 ) ) ;
#28678 = ORIENTED_EDGE ( 'NONE', *, *, #47042, .T. ) ;
#28680 = EDGE_LOOP ( 'NONE', ( #16962, #65572, #38556, #43548 ) ) ;
#28679 = DIRECTION ( 'NONE',  ( 0.000000000000000000, 0.000000000000000000, -1.000000000000000000 ) ) ;
#28681 = VERTEX_POINT ( 'NONE', #58400 ) ;
#28682 = ORIENTED_EDGE ( 'NONE', *, *, #26754, .T. ) ;
#28683 = CARTESIAN_POINT ( 'NONE',  ( -2.530476262117229425, 9.547976262117158441, 26.00000000000000711 ) ) ;
#28684 = DIRECTION ( 'NONE',  ( -1.000000000000000000, 0.000000000000000000, 0.000000000000000000 ) ) ;
#28685 = LINE ( 'NONE', #12409, #62435 ) ;
#28686 = ORIENTED_EDGE ( 'NONE', *, *, #2593, .T. ) ;
#28687 = ORIENTED_EDGE ( 'NONE', *, *, #14387, .T. ) ;
#28688 = CARTESIAN_POINT ( 'NONE',  ( 7.250000000000005329, 7.250000000000000888, -30.00000000000001066 ) ) ;
#28689 = CARTESIAN_POINT ( 'NONE',  ( 16.75000000000000000, -0.2038245569916320166, -21.77831216351300014 ) ) ;
#28690 = CIRCLE ( 'NONE', #30978, 1.000000000000000000 ) ;
#28691 = ORIENTED_EDGE ( 'NONE', *, *, #39420, .T. ) ;
#28692 = ORIENTED_EDGE ( 'NONE', *, *, #48130, .T. ) ;
#28693 = DIRECTION ( 'NONE',  ( -1.000000000000000000, 0.000000000000000000, 0.000000000000000000 ) ) ;
#28694 = DIRECTION ( 'NONE',  ( 1.000000000000000000, -0.000000000000000000, -0.000000000000000000 ) ) ;
#28695 = EDGE_LOOP ( 'NONE', ( #22710, #48618, #63593, #37254 ) ) ;
#28696 = VECTOR ( 'NONE', #50813, 1000.000000000000114 ) ;
#28697 = AXIS2_PLACEMENT_3D ( 'NONE', #5753, #48888, #43911 ) ;
#28698 = LINE ( 'NONE', #61560, #69658 ) ;
#28701 = ORIENTED_EDGE ( 'NONE', *, *, #1893, .T. ) ;
#28700 = ADVANCED_FACE ( 'NONE', ( #19493 ), #30460, .F. ) ;
#28699 = LINE ( 'NONE', #44604, #2394 ) ;
#28702 = ORIENTED_EDGE ( 'NONE', *, *, #18591, .F. ) ;
#28703 = EDGE_CURVE ( 'NONE', #8535, #46756, #43133, .T. ) ;
#28704 = EDGE_CURVE ( 'NONE', #59416, #48640, #68991, .T. ) ;
#28705 = CYLINDRICAL_SURFACE ( 'NONE', #11806, 1.000000000000002665 ) ;
#28706 = LINE ( 'NONE', #7483, #713 ) ;
#28707 = AXIS2_PLACEMENT_3D ( 'NONE', #41457, #58069, #42507 ) ;
#28708 = AXIS2_PLACEMENT_3D ( 'NONE', #24582, #58151, #57795 ) ;
#28709 = DIRECTION ( 'NONE',  ( 0.000000000000000000, 0.000000000000000000, 1.000000000000000000 ) ) ;
#28710 = CARTESIAN_POINT ( 'NONE',  ( 16.75000000000000000, -2.500000000000000000, 23.22168783648699986 ) ) ;
#28711 = CARTESIAN_POINT ( 'NONE',  ( 9.899999999999998579, -21.00000000000000000, 13.86939075806900057 ) ) ;
#28712 = EDGE_CURVE ( 'NONE', #6107, #67217, #35397, .T. ) ;
#28713 = DIRECTION ( 'NONE',  ( 0.000000000000000000, 0.8320000000000478124, 0.5547756303226741847 ) ) ;
#28714 = AXIS2_PLACEMENT_3D ( 'NONE', #49125, #21562, #16252 ) ;
#28715 = ORIENTED_EDGE ( 'NONE', *, *, #7024, .F. ) ;
#28716 = CARTESIAN_POINT ( 'NONE',  ( -24.00000000000000000, -17.00000000000000000, -15.70499999999969809 ) ) ;
#28718 = VERTEX_POINT ( 'NONE', #62626 ) ;
#28717 = DIRECTION ( 'NONE',  ( 0.7071067811865474617, 0.7071067811865474617, 0.000000000000000000 ) ) ;
#28719 = CYLINDRICAL_SURFACE ( 'NONE', #23057, 0.1999999999999987899 ) ;
#28720 = LINE ( 'NONE', #35410, #6393 ) ;
#28721 = AXIS2_PLACEMENT_3D ( 'NONE', #66874, #50628, #2188 ) ;
#28722 = CARTESIAN_POINT ( 'NONE',  ( -5.242976262117280406, -5.257023737882805747, 54.00000000000000711 ) ) ;
#28723 = AXIS2_PLACEMENT_3D ( 'NONE', #36077, #30076, #20869 ) ;
#28724 = DIRECTION ( 'NONE',  ( 0.000000000000000000, 0.000000000000000000, 1.000000000000000000 ) ) ;
#28725 = VERTEX_POINT ( 'NONE', #9960 ) ;
#28726 = ORIENTED_EDGE ( 'NONE', *, *, #9436, .F. ) ;
#28727 = DIRECTION ( 'NONE',  ( -1.000000000000000000, 0.000000000000000000, 0.000000000000000000 ) ) ;
#28728 = SURFACE_STYLE_USAGE ( .BOTH. , #43621 ) ;
#28729 = PLANE ( 'NONE',  #313 ) ;
#28730 = ORIENTED_EDGE ( 'NONE', *, *, #41838, .F. ) ;
#28731 = LINE ( 'NONE', #49951, #18053 ) ;
#28732 = ORIENTED_EDGE ( 'NONE', *, *, #14307, .T. ) ;
#28733 = CONICAL_SURFACE ( 'NONE', #44520, 1.621000000000000885, 0.7853981633974518317 ) ;
#28734 = VERTEX_POINT ( 'NONE', #3947 ) ;
#28735 = FACE_OUTER_BOUND ( 'NONE', #45960, .T. ) ;
#28736 = CARTESIAN_POINT ( 'NONE',  ( 0.000000000000000000, 0.000000000000000000, 0.000000000000000000 ) ) ;
#28737 = ORIENTED_EDGE ( 'NONE', *, *, #6606, .T. ) ;
#28738 = CARTESIAN_POINT ( 'NONE',  ( 49.00000000000000000, -21.00000000000000000, 13.86939075806900057 ) ) ;
#28739 = CIRCLE ( 'NONE', #63796, 1.000000000000000000 ) ;
#28740 = DIRECTION ( 'NONE',  ( -0.000000000000000000, 3.673940397442059868E-16, -1.000000000000000000 ) ) ;
#28741 = CARTESIAN_POINT ( 'NONE',  ( 283.0000000000000568, -31.99999999999889866, -7.899999999997660893 ) ) ;
#28742 = EDGE_LOOP ( 'NONE', ( #53306, #63571, #39451, #66418 ) ) ;
#28744 = VERTEX_POINT ( 'NONE', #63699 ) ;
#28743 = DIRECTION ( 'NONE',  ( -0.000000000000000000, 3.673940397442059868E-16, -1.000000000000000000 ) ) ;
#28745 = ADVANCED_FACE ( 'NONE', ( #52382 ), #20199, .T. ) ;
#28746 = VECTOR ( 'NONE', #7247, 1000.000000000000000 ) ;
#28747 = CARTESIAN_POINT ( 'NONE',  ( 30.00000000000000000, -5.599999999999999645, 9.000000000000001776 ) ) ;
#28748 = CARTESIAN_POINT ( 'NONE',  ( 4.406483450353340103, -11.32648345035347681, 455.0000000000000568 ) ) ;
#28749 = EDGE_CURVE ( 'NONE', #34855, #23968, #25159, .T. ) ;
#28750 = DIRECTION ( 'NONE',  ( -1.836970198721029934E-16, 1.836970198721036344E-16, -1.000000000000000000 ) ) ;
#28751 = DIRECTION ( 'NONE',  ( -1.000000000000000000, -1.671920889371702854E-15, 0.000000000000000000 ) ) ;
#28752 = ADVANCED_FACE ( 'NONE', ( #14194 ), #9250, .F. ) ;
#28753 = FACE_OUTER_BOUND ( 'NONE', #68649, .T. ) ;
#28754 = VECTOR ( 'NONE', #57632, 1000.000000000000000 ) ;
#28755 = CARTESIAN_POINT ( 'NONE',  ( -3.593516549646762481, -4.622483450353452206, 455.0000000000000568 ) ) ;
#28756 = EDGE_CURVE ( 'NONE', #57627, #25429, #31528, .T. ) ;
#28757 = VERTEX_POINT ( 'NONE', #30107 ) ;
#28758 = ORIENTED_EDGE ( 'NONE', *, *, #4204, .T. ) ;
#28759 = PRODUCT_DEFINITION ( 'UNKNOWN', '', #26863, #2065 ) ;
#28760 = ORIENTED_EDGE ( 'NONE', *, *, #34480, .F. ) ;
#28761 = CARTESIAN_POINT ( 'NONE',  ( 28.90000000000000213, 0.000000000000000000, 0.000000000000000000 ) ) ;
#28762 = ADVANCED_FACE ( 'NONE', ( #41414 ), #68293, .F. ) ;
#28763 = LINE ( 'NONE', #50334, #33205 ) ;
#28764 = ADVANCED_FACE ( 'NONE', ( #3241 ), #57332, .F. ) ;
#28765 = DIRECTION ( 'NONE',  ( 0.7671651518153006499, 0.6414496315691565753, 0.000000000000000000 ) ) ;
#28766 = AXIS2_PLACEMENT_3D ( 'NONE', #31374, #52939, #4488 ) ;
#28767 = ORIENTED_EDGE ( 'NONE', *, *, #44448, .F. ) ;
#28768 = ORIENTED_EDGE ( 'NONE', *, *, #57344, .T. ) ;
#28769 = ORIENTED_EDGE ( 'NONE', *, *, #36596, .F. ) ;
#28770 = DIRECTION ( 'NONE',  ( 0.000000000000000000, -0.7096009616570518874, -0.7046037717862339012 ) ) ;
#28771 = ORIENTED_EDGE ( 'NONE', *, *, #69401, .F. ) ;
#28772 = ORIENTED_EDGE ( 'NONE', *, *, #14307, .F. ) ;
#28773 = EDGE_LOOP ( 'NONE', ( #7375, #37507, #32528, #26727 ) ) ;
#28774 = ORIENTED_EDGE ( 'NONE', *, *, #52760, .F. ) ;
#28775 = DIRECTION ( 'NONE',  ( -1.000000000000000000, 0.000000000000000000, -0.000000000000000000 ) ) ;
#28777 = ORIENTED_EDGE ( 'NONE', *, *, #30226, .T. ) ;
#28776 = CARTESIAN_POINT ( 'NONE',  ( -4.383466043307859827, 8.393516549646591329, 455.0000000000000568 ) ) ;
#28778 = CARTESIAN_POINT ( 'NONE',  ( 10.92648345035337343, -9.306483450353395526, 195.0000000000000284 ) ) ;
#28779 = DIRECTION ( 'NONE',  ( 0.000000000000000000, -1.000000000000000000, 0.000000000000000000 ) ) ;
#28780 = CARTESIAN_POINT ( 'NONE',  ( 2.005523737882808355, 8.598420958951638937, 26.00000000000000711 ) ) ;
#28782 = ORIENTED_EDGE ( 'NONE', *, *, #33651, .F. ) ;
#28781 = CARTESIAN_POINT ( 'NONE',  ( 15.50000000000129852, -17.50000000000000000, 22.50000000000000000 ) ) ;
#28783 = AXIS2_PLACEMENT_3D ( 'NONE', #1879, #23790, #61605 ) ;
#28784 = CARTESIAN_POINT ( 'NONE',  ( -30.00000000000000000, -14.04000000000000092, 14.80000000000000071 ) ) ;
#28785 = LINE ( 'NONE', #56024, #32314 ) ;
#28786 = EDGE_CURVE ( 'NONE', #16582, #21729, #53097, .T. ) ;
#28787 = DIRECTION ( 'NONE',  ( -1.836970198721029934E-16, 1.836970198721036344E-16, -1.000000000000000000 ) ) ;
#28788 = VERTEX_POINT ( 'NONE', #25869 ) ;
#28789 = DIRECTION ( 'NONE',  ( -0.8660254037844510311, -0.4999999999999786282, 0.000000000000000000 ) ) ;
#28790 = AXIS2_PLACEMENT_3D ( 'NONE', #14554, #8539, #52395 ) ;
#28792 = LINE ( 'NONE', #34797, #49020 ) ;
#28791 = AXIS2_PLACEMENT_3D ( 'NONE', #64977, #20440, #58969 ) ;
#28793 = CARTESIAN_POINT ( 'NONE',  ( 176.4833316329832940, 0.000000000000000000, 282.8454385697650082 ) ) ;
#28794 = ORIENTED_EDGE ( 'NONE', *, *, #27720, .F. ) ;
#28795 = CARTESIAN_POINT ( 'NONE',  ( 6.849523737882817542, -10.50702373788282529, 54.00000000000000711 ) ) ;
#28796 = CIRCLE ( 'NONE', #15303, 0.5000000000079367624 ) ;
#28797 = EDGE_CURVE ( 'NONE', #41567, #2486, #58030, .T. ) ;
#28798 = DIRECTION ( 'NONE',  ( 0.000000000000000000, 0.000000000000000000, 1.000000000000000000 ) ) ;
#28799 = DIRECTION ( 'NONE',  ( 1.079558018506126625E-14, 1.000000000000000000, 1.836970198721016622E-16 ) ) ;
#28800 = EDGE_LOOP ( 'NONE', ( #28678, #14874, #37565, #24944 ) ) ;
#28801 = VECTOR ( 'NONE', #65152, 1000.000000000000000 ) ;
#28802 = EDGE_CURVE ( 'NONE', #61047, #68976, #20550, .T. ) ;
#28803 = DIRECTION ( 'NONE',  ( -1.000000000000000000, 0.000000000000000000, 0.000000000000000000 ) ) ;
#28804 = FACE_OUTER_BOUND ( 'NONE', #63818, .T. ) ;
#28805 = DIRECTION ( 'NONE',  ( 1.000000000000000000, 0.000000000000000000, 0.000000000000000000 ) ) ;
#28806 = CARTESIAN_POINT ( 'NONE',  ( 78.77321854994620765, 47.95351654967443977, 39.00000000000000000 ) ) ;
#28807 = ORIENTED_EDGE ( 'NONE', *, *, #49667, .F. ) ;
#28808 = FACE_OUTER_BOUND ( 'NONE', #63365, .T. ) ;
#28809 = DIRECTION ( 'NONE',  ( 0.000000000000000000, 0.6857142857142843884, 0.7278708115918295363 ) ) ;
#28810 = DIRECTION ( 'NONE',  ( -1.000000000000000000, 0.000000000000000000, 0.000000000000000000 ) ) ;
#28811 = CARTESIAN_POINT ( 'NONE',  ( 7.250000000000005329, -7.249999999999998224, -20.50000000000000000 ) ) ;
#28812 = DIRECTION ( 'NONE',  ( 0.000000000000000000, 0.000000000000000000, -1.000000000000000000 ) ) ;
#28813 = ORIENTED_EDGE ( 'NONE', *, *, #1657, .F. ) ;
#28814 = FACE_OUTER_BOUND ( 'NONE', #23381, .T. ) ;
#28815 = LINE ( 'NONE', #45080, #66644 ) ;
#28816 = EDGE_CURVE ( 'NONE', #63729, #59026, #19147, .T. ) ;
#28817 = DIRECTION ( 'NONE',  ( 0.000000000000000000, 0.000000000000000000, -1.000000000000000000 ) ) ;
#28818 = DIRECTION ( 'NONE',  ( -1.000000000000000000, 0.000000000000000000, 0.000000000000000000 ) ) ;
#28819 = LINE ( 'NONE', #51450, #53174 ) ;
#28820 = ORIENTED_EDGE ( 'NONE', *, *, #58057, .T. ) ;
#28822 = ORIENTED_EDGE ( 'NONE', *, *, #25209, .T. ) ;
#28821 = PLANE ( 'NONE',  #6987 ) ;
#28823 = FACE_OUTER_BOUND ( 'NONE', #1780, .T. ) ;
#28824 = EDGE_CURVE ( 'NONE', #69842, #24526, #21606, .T. ) ;
#28825 = DIRECTION ( 'NONE',  ( 1.000000000000000000, -0.000000000000000000, -0.000000000000000000 ) ) ;
#28826 = ORIENTED_EDGE ( 'NONE', *, *, #62996, .T. ) ;
#28827 = CARTESIAN_POINT ( 'NONE',  ( 276.8775010008008053, -53.81370849898476649, -17.50000000000000000 ) ) ;
#28828 = VECTOR ( 'NONE', #44135, 1000.000000000000000 ) ;
#28829 = ORIENTED_EDGE ( 'NONE', *, *, #60198, .T. ) ;
#28830 = AXIS2_PLACEMENT_3D ( 'NONE', #47974, #10834, #36669 ) ;
#28831 = FACE_OUTER_BOUND ( 'NONE', #20296, .T. ) ;
#28832 = ORIENTED_EDGE ( 'NONE', *, *, #55719, .F. ) ;
#28833 = ORIENTED_EDGE ( 'NONE', *, *, #8713, .F. ) ;
#28835 = EDGE_CURVE ( 'NONE', #58770, #52725, #20524, .T. ) ;
#28834 = DIRECTION ( 'NONE',  ( 1.000000000000000000, 3.469446951953611033E-15, 0.000000000000000000 ) ) ;
#28836 = LINE ( 'NONE', #56764, #20736 ) ;
#28837 = EDGE_CURVE ( 'NONE', #23447, #11691, #19398, .T. ) ;
#28838 = PLANE ( 'NONE',  #65351 ) ;
#28839 = DIRECTION ( 'NONE',  ( -1.000000000000000000, 0.000000000000000000, 0.000000000000000000 ) ) ;
#28840 = AXIS2_PLACEMENT_3D ( 'NONE', #14708, #20011, #10107 ) ;
#28841 = AXIS2_PLACEMENT_3D ( 'NONE', #31095, #47698, #26143 ) ;
#28842 = VECTOR ( 'NONE', #36445, 1000.000000000000000 ) ;
#28843 = EDGE_LOOP ( 'NONE', ( #18417, #34125, #38422, #12249 ) ) ;
#28844 = ORIENTED_EDGE ( 'NONE', *, *, #15039, .T. ) ;
#28845 = CARTESIAN_POINT ( 'NONE',  ( 283.0000000000000568, -20.40000000000000213, 12.40000000000000213 ) ) ;
#28846 = CARTESIAN_POINT ( 'NONE',  ( 0.000000000000000000, 8.250000000000001776, -20.50000000000000000 ) ) ;
#28847 = CIRCLE ( 'NONE', #43611, 0.1749999999999998224 ) ;
#28848 = VECTOR ( 'NONE', #55465, 1000.000000000000000 ) ;
#28849 = VECTOR ( 'NONE', #49223, 1000.000000000000000 ) ;
#28850 = VERTEX_POINT ( 'NONE', #43856 ) ;
#28851 = ORIENTED_EDGE ( 'NONE', *, *, #10801, .F. ) ;
#28852 = ORIENTED_EDGE ( 'NONE', *, *, #68475, .T. ) ;
#28853 = AXIS2_PLACEMENT_3D ( 'NONE', #4886, #48370, #37416 ) ;
#28854 = CARTESIAN_POINT ( 'NONE',  ( -11.00000000000000000, -11.50000000000000000, -15.00000000000000000 ) ) ;
#28856 = ORIENTED_EDGE ( 'NONE', *, *, #29196, .F. ) ;
#28855 = CARTESIAN_POINT ( 'NONE',  ( 7.000000000000000000, -31.30000000000000071, -12.69999999999999929 ) ) ;
#28857 = CARTESIAN_POINT ( 'NONE',  ( -11.00000000000000000, -16.28999999999999915, -14.50000000000000000 ) ) ;
#28858 = VECTOR ( 'NONE', #10232, 1000.000000000000000 ) ;
#28859 = CARTESIAN_POINT ( 'NONE',  ( -8.249999999999996447, 8.250000000000001776, -5.000000000000000000 ) ) ;
#28860 = EDGE_CURVE ( 'NONE', #19296, #6839, #47769, .T. ) ;
#28861 = EDGE_LOOP ( 'NONE', ( #41982, #66273, #14763, #2134 ) ) ;
#28862 = CIRCLE ( 'NONE', #26626, 3.500000000000114131 ) ;
#28863 = ORIENTED_EDGE ( 'NONE', *, *, #37555, .F. ) ;
#28864 = EDGE_CURVE ( 'NONE', #60150, #47415, #63434, .T. ) ;
#28865 = LINE ( 'NONE', #45124, #41690 ) ;
#28866 = LINE ( 'NONE', #23221, #48224 ) ;
#28867 = CARTESIAN_POINT ( 'NONE',  ( -7.798499376344111056, -7.272650909786579909, 195.0000000000000284 ) ) ;
#28868 = ADVANCED_FACE ( 'NONE', ( #60111 ), #69338, .T. ) ;
#28869 = DIRECTION ( 'NONE',  ( 0.000000000000000000, 0.000000000000000000, -1.000000000000000000 ) ) ;
#28870 = FACE_OUTER_BOUND ( 'NONE', #61675, .T. ) ;
#28872 = EDGE_LOOP ( 'NONE', ( #7801, #56627 ) ) ;
#28871 = CARTESIAN_POINT ( 'NONE',  ( -6.822336235477441946, -4.149127210878692296, 26.00000000000000711 ) ) ;
#28873 = VERTEX_POINT ( 'NONE', #59433 ) ;
#28874 = EDGE_CURVE ( 'NONE', #60123, #43073, #5844, .T. ) ;
#28875 = PLANE ( 'NONE',  #47912 ) ;
#28876 = LINE ( 'NONE', #50105, #64633 ) ;
#28877 = EDGE_CURVE ( 'NONE', #59188, #26479, #38599, .T. ) ;
#28878 = CIRCLE ( 'NONE', #14212, 0.5000000000009441337 ) ;
#28879 = DIRECTION ( 'NONE',  ( 0.000000000000000000, 0.000000000000000000, -1.000000000000000000 ) ) ;
#28880 = VECTOR ( 'NONE', #5112, 1000.000000000000000 ) ;
#28881 = EDGE_CURVE ( 'NONE', #28664, #67299, #11324, .T. ) ;
#28882 = LINE ( 'NONE', #17929, #19589 ) ;
#28883 = ORIENTED_EDGE ( 'NONE', *, *, #67756, .T. ) ;
#28884 = CARTESIAN_POINT ( 'NONE',  ( 6.006483450353379716, -6.006483450353490738, 455.0000000000000568 ) ) ;
#28885 = DIRECTION ( 'NONE',  ( -1.000000000000000000, 0.000000000000000000, -0.000000000000000000 ) ) ;
#28886 = DIRECTION ( 'NONE',  ( 1.836970198721029934E-16, 1.836970198721010706E-16, -1.000000000000000000 ) ) ;
#28887 = CIRCLE ( 'NONE', #53765, 2.215251240775983899 ) ;
#28888 = VECTOR ( 'NONE', #16131, 1000.000000000000000 ) ;
#28889 = AXIS2_PLACEMENT_3D ( 'NONE', #4295, #25501, #47063 ) ;
#28890 = CARTESIAN_POINT ( 'NONE',  ( 34.89999999999999858, 20.60000000000000142, 13.86939075806900057 ) ) ;
#28891 = EDGE_CURVE ( 'NONE', #41558, #41898, #16654, .T. ) ;
#28892 = CARTESIAN_POINT ( 'NONE',  ( 15.00000000000000000, -20.40000000000000213, 17.60000000000000142 ) ) ;
#28893 = EDGE_CURVE ( 'NONE', #86, #30798, #43159, .T. ) ;
#28894 = AXIS2_PLACEMENT_3D ( 'NONE', #5854, #44350, #66288 ) ;
#28895 = VECTOR ( 'NONE', #23721, 1000.000000000000000 ) ;
#28896 = VECTOR ( 'NONE', #62153, 1000.000000000000000 ) ;
#28897 = CARTESIAN_POINT ( 'NONE',  ( -15.50000000000000000, -5.000000000000000000, -26.50000000000000000 ) ) ;
#28898 = EDGE_LOOP ( 'NONE', ( #33164, #34302, #5209, #41131 ) ) ;
#28899 = CARTESIAN_POINT ( 'NONE',  ( 8.250000000000005329, 0.000000000000000000, -25.50000000000000355 ) ) ;
#28900 = CARTESIAN_POINT ( 'NONE',  ( 41.09999999999999432, -21.00000000000000000, 13.86939075806900057 ) ) ;
#28901 = EDGE_CURVE ( 'NONE', #68940, #11281, #64058, .T. ) ;
#28902 = VERTEX_POINT ( 'NONE', #10633 ) ;
#28903 = CARTESIAN_POINT ( 'NONE',  ( -3.650476262117223314, 10.30047626211716683, 54.00000000000000711 ) ) ;
#28904 = EDGE_CURVE ( 'NONE', #26250, #40700, #28429, .T. ) ;
#28905 = EDGE_CURVE ( 'NONE', #38001, #54143, #31874, .T. ) ;
#28906 = DIRECTION ( 'NONE',  ( 0.7071067811865474617, 0.7071067811865474617, 0.000000000000000000 ) ) ;
#28907 = AXIS2_PLACEMENT_3D ( 'NONE', #51762, #12854, #67669 ) ;
#28908 = CARTESIAN_POINT ( 'NONE',  ( -23.75054448485400016, -15.50000000000000000, 25.53140320652400064 ) ) ;
#28909 = DIRECTION ( 'NONE',  ( 0.7071067811865474617, -0.7071067811865474617, -2.597868168706479611E-16 ) ) ;
#28910 = CARTESIAN_POINT ( 'NONE',  ( 7.450000000000006395, 7.250000000000000888, -15.50000000000000000 ) ) ;
#28911 = ORIENTED_EDGE ( 'NONE', *, *, #8896, .T. ) ;
#28912 = EDGE_CURVE ( 'NONE', #6104, #64750, #37867, .T. ) ;
#28913 = DIRECTION ( 'NONE',  ( 0.000000000000000000, -1.000000000000000000, 0.000000000000000000 ) ) ;
#28914 = AXIS2_PLACEMENT_3D ( 'NONE', #63070, #15689, #53182 ) ;
#28915 = ORIENTED_EDGE ( 'NONE', *, *, #8154, .F. ) ;
#28916 = EDGE_CURVE ( 'NONE', #23540, #12421, #64397, .T. ) ;
#28917 = CARTESIAN_POINT ( 'NONE',  ( 29.50000000000000355, -11.50000000000000000, 19.00000000000000000 ) ) ;
#28918 = VERTEX_POINT ( 'NONE', #37522 ) ;
#28919 = PLANE ( 'NONE',  #22459 ) ;
#28920 = EDGE_CURVE ( 'NONE', #50899, #22396, #32212, .T. ) ;
#28921 = FACE_OUTER_BOUND ( 'NONE', #52138, .T. ) ;
#28922 = CARTESIAN_POINT ( 'NONE',  ( 30.00000000000000000, -13.79999999999979998, 17.30000000000000071 ) ) ;
#28923 = ORIENTED_EDGE ( 'NONE', *, *, #32903, .T. ) ;
#28924 = ORIENTED_EDGE ( 'NONE', *, *, #37530, .F. ) ;
#28926 = EDGE_CURVE ( 'NONE', #9481, #48587, #56652, .T. ) ;
#28925 = CARTESIAN_POINT ( 'NONE',  ( -4.141586236041100655, 4.706725378239165813, 54.00000000000000711 ) ) ;
#28927 = VERTEX_POINT ( 'NONE', #383 ) ;
#28928 = VERTEX_POINT ( 'NONE', #59776 ) ;
#28929 = EDGE_CURVE ( 'NONE', #6044, #56509, #14881, .T. ) ;
#28930 = PRODUCT_DEFINITION_CONTEXT ( 'detailed design', #62502, 'design' ) ;
#28931 = FACE_OUTER_BOUND ( 'NONE', #67876, .T. ) ;
#28932 = CARTESIAN_POINT ( 'NONE',  ( -9.390476262117259054, 1.466476262117183182, 26.00000000000000711 ) ) ;
#28933 = FACE_OUTER_BOUND ( 'NONE', #15808, .T. ) ;
#28934 = VECTOR ( 'NONE', #30910, 1000.000000000000000 ) ;
#28935 = VERTEX_POINT ( 'NONE', #1411 ) ;
#28936 = DIRECTION ( 'NONE',  ( 0.000000000000000000, -3.673940397442059868E-16, 1.000000000000000000 ) ) ;
#28938 = DIRECTION ( 'NONE',  ( 1.000000000000000000, 0.000000000000000000, 0.000000000000000000 ) ) ;
#28937 = CARTESIAN_POINT ( 'NONE',  ( 49.00000000000000000, -0.2000000000089119934, 8.909539772616881237E-12 ) ) ;
#28939 = ORIENTED_EDGE ( 'NONE', *, *, #13665, .F. ) ;
#28941 = EDGE_LOOP ( 'NONE', ( #57676, #58520, #32169, #16861 ) ) ;
#28940 = FACE_OUTER_BOUND ( 'NONE', #55876, .T. ) ;
#28942 = AXIS2_PLACEMENT_3D ( 'NONE', #35444, #52077, #57375 ) ;
#28943 = VERTEX_POINT ( 'NONE', #38891 ) ;
#28944 = DIRECTION ( 'NONE',  ( 0.000000000000000000, 0.000000000000000000, 1.000000000000000000 ) ) ;
#28945 = CIRCLE ( 'NONE', #61695, 0.5999999999999998668 ) ;
#28946 = CIRCLE ( 'NONE', #42542, 0.1749999999999989342 ) ;
#28947 = DIRECTION ( 'NONE',  ( 3.491481338843134144E-15, 1.000000000000000000, 1.836970198721030181E-16 ) ) ;
#28948 = EDGE_LOOP ( 'NONE', ( #56256, #47201, #46419, #5012 ) ) ;
#28949 = AXIS2_PLACEMENT_3D ( 'NONE', #16737, #32984, #10382 ) ;
#28950 = CIRCLE ( 'NONE', #10895, 4.000000000000000888 ) ;
#28951 = VECTOR ( 'NONE', #14457, 1000.000000000000000 ) ;
#28952 = DIRECTION ( 'NONE',  ( 0.000000000000000000, 0.000000000000000000, -1.000000000000000000 ) ) ;
#28953 = DIRECTION ( 'NONE',  ( 0.000000000000000000, 1.000000000000000000, 0.000000000000000000 ) ) ;
#28954 = VERTEX_POINT ( 'NONE', #18712 ) ;
#28955 = ORIENTED_EDGE ( 'NONE', *, *, #20152, .T. ) ;
#28956 = VECTOR ( 'NONE', #18435, 1000.000000000000000 ) ;
#28957 = CYLINDRICAL_SURFACE ( 'NONE', #40256, 0.3000000000005393908 ) ;
#28958 = CARTESIAN_POINT ( 'NONE',  ( -9.690000000000001279, -8.750000000000000000, -7.000000000000000000 ) ) ;
#28959 = ORIENTED_EDGE ( 'NONE', *, *, #10308, .T. ) ;
#28960 = CARTESIAN_POINT ( 'NONE',  ( -7.250000000000000888, 7.450000000000003730, -16.00000000000000000 ) ) ;
#28962 = CARTESIAN_POINT ( 'NONE',  ( 1.000000000000000000, -21.00000000000000000, 0.000000000000000000 ) ) ;
#28961 = VECTOR ( 'NONE', #63241, 1000.000000000000000 ) ;
#28963 = LINE ( 'NONE', #45215, #12420 ) ;
#28964 = EDGE_LOOP ( 'NONE', ( #35678, #2868, #8695, #28424, #21374, #54783 ) ) ;
#28965 = EDGE_CURVE ( 'NONE', #15138, #53340, #197, .T. ) ;
#28966 = CIRCLE ( 'NONE', #36932, 0.1749999999999998224 ) ;
#28967 = LINE ( 'NONE', #7389, #34644 ) ;
#28968 = FACE_OUTER_BOUND ( 'NONE', #67371, .T. ) ;
#28970 = EDGE_LOOP ( 'NONE', ( #39466, #51931, #46925, #34759, #13653, #42249, #25231, #62920 ) ) ;
#28969 = LINE ( 'NONE', #39911, #8084 ) ;
#28972 = EDGE_LOOP ( 'NONE', ( #36939, #34860, #25834, #61465 ) ) ;
#28971 = LINE ( 'NONE', #22299, #58353 ) ;
#28973 = EDGE_CURVE ( 'NONE', #4514, #48863, #28974, .T. ) ;
#28974 = LINE ( 'NONE', #61481, #65691 ) ;
#28975 = EDGE_CURVE ( 'NONE', #33710, #55788, #44527, .T. ) ;
#28976 = CARTESIAN_POINT ( 'NONE',  ( 8.690000000000001279, -9.750000000000001776, -5.000000000000000000 ) ) ;
#28977 = DIRECTION ( 'NONE',  ( -1.000000000000000000, 0.000000000000000000, 0.000000000000000000 ) ) ;
#28978 = ADVANCED_FACE ( 'NONE', ( #7051 ), #28281, .T. ) ;
#28979 = CARTESIAN_POINT ( 'NONE',  ( -8.250000000000001776, 0.000000000000000000, -18.50000000000000000 ) ) ;
#28980 = ORIENTED_EDGE ( 'NONE', *, *, #36219, .F. ) ;
#28981 = LINE ( 'NONE', #51606, #6402 ) ;
#28982 = CYLINDRICAL_SURFACE ( 'NONE', #7843, 1.000000000000000000 ) ;
#28983 = DIRECTION ( 'NONE',  ( 1.836970198721029934E-16, 1.836970198721010706E-16, -1.000000000000000000 ) ) ;
#28985 = ORIENTED_EDGE ( 'NONE', *, *, #28994, .T. ) ;
#28984 = LINE ( 'NONE', #25434, #11834 ) ;
#28986 = DIRECTION ( 'NONE',  ( -0.000000000000000000, 3.673940397442059868E-16, -1.000000000000000000 ) ) ;
#28987 = VECTOR ( 'NONE', #25175, 1000.000000000000000 ) ;
#28988 = CARTESIAN_POINT ( 'NONE',  ( -15.50000000000000000, -2.500000000000000000, -21.05662432702600029 ) ) ;
#28989 = VECTOR ( 'NONE', #14251, 1000.000000000000114 ) ;
#28990 = VERTEX_POINT ( 'NONE', #17320 ) ;
#28991 = LINE ( 'NONE', #45242, #60250 ) ;
#28992 = DIRECTION ( 'NONE',  ( -0.000000000000000000, 0.000000000000000000, 1.000000000000000000 ) ) ;
#28993 = ORIENTED_EDGE ( 'NONE', *, *, #22186, .T. ) ;
#28994 = EDGE_CURVE ( 'NONE', #9220, #44308, #54822, .T. ) ;
#28995 = LINE ( 'NONE', #33945, #30066 ) ;
#28996 = LINE ( 'NONE', #66478, #4144 ) ;
#28997 = AXIS2_PLACEMENT_3D ( 'NONE', #12267, #18625, #34180 ) ;
#28998 = VECTOR ( 'NONE', #16898, 1000.000000000000000 ) ;
#28999 = LINE ( 'NONE', #66817, #22400 ) ;
#29000 = DIRECTION ( 'NONE',  ( -0.000000000000000000, -0.000000000000000000, -1.000000000000000000 ) ) ;
#29001 = AXIS2_PLACEMENT_3D ( 'NONE', #40115, #29520, #3352 ) ;
#29002 = CARTESIAN_POINT ( 'NONE',  ( 41.09999999999999432, -0.2000000000000000111, 0.000000000000000000 ) ) ;
#29003 = ORIENTED_EDGE ( 'NONE', *, *, #10623, .F. ) ;
#29004 = AXIS2_PLACEMENT_3D ( 'NONE', #53499, #9665, #41482 ) ;
#29005 = CARTESIAN_POINT ( 'NONE',  ( 7.606483450353380249, -11.78648345035349010, 455.0000000000000568 ) ) ;
#29006 = ORIENTED_EDGE ( 'NONE', *, *, #69006, .T. ) ;
#29007 = ORIENTED_EDGE ( 'NONE', *, *, #11189, .F. ) ;
#29008 = CARTESIAN_POINT ( 'NONE',  ( -15.50000000000000000, -2.500000000000000000, 21.05662432702600029 ) ) ;
#29009 = VECTOR ( 'NONE', #19664, 1000.000000000000000 ) ;
#29010 = CIRCLE ( 'NONE', #68551, 0.5000000000000000000 ) ;
#29011 = AXIS2_PLACEMENT_3D ( 'NONE', #13743, #35291, #14808 ) ;
#29012 = CARTESIAN_POINT ( 'NONE',  ( 26.90000000000000213, -0.2000000000089119934, 8.909539772616881237E-12 ) ) ;
#29014 = LINE ( 'NONE', #3550, #24250 ) ;
#29013 = LINE ( 'NONE', #46931, #56614 ) ;
#29015 = EDGE_LOOP ( 'NONE', ( #2580, #32183, #37934, #31799 ) ) ;
#29016 = ORIENTED_EDGE ( 'NONE', *, *, #60901, .T. ) ;
#29018 = ADVANCED_FACE ( 'NONE', ( #24013 ), #22638, .F. ) ;
#29017 = CYLINDRICAL_SURFACE ( 'NONE', #32963, 0.5000000000079367624 ) ;
#29019 = ORIENTED_EDGE ( 'NONE', *, *, #37631, .F. ) ;
#29020 = PRODUCT_DEFINITION_SHAPE ( 'NONE', 'NONE',  #29636 ) ;
#29021 = ADVANCED_FACE ( 'NONE', ( #13409 ), #55510, .F. ) ;
#29022 = AXIS2_PLACEMENT_3D ( 'NONE', #5605, #54392, #54050 ) ;
#29023 = CARTESIAN_POINT ( 'NONE',  ( -7.250000000000001776, -7.249999999999998224, -17.50000000000000000 ) ) ;
#29024 = LINE ( 'NONE', #55552, #19627 ) ;
#29025 = DIRECTION ( 'NONE',  ( 0.7071067811865474617, 0.7071067811865474617, 0.000000000000000000 ) ) ;
#29026 = EDGE_CURVE ( 'NONE', #22338, #27411, #39238, .T. ) ;
#29027 = DIRECTION ( 'NONE',  ( -1.000000000000000000, 0.000000000000000000, 0.000000000000000000 ) ) ;
#29029 = LINE ( 'NONE', #32953, #32315 ) ;
#29028 = DIRECTION ( 'NONE',  ( 0.000000000000000000, 1.000000000000000000, 1.880440247955360336E-12 ) ) ;
#29030 = EDGE_LOOP ( 'NONE', ( #58085, #22180, #35574, #61289, #11391, #28388, #16562, #27832, #50432 ) ) ;
#29032 = ORIENTED_EDGE ( 'NONE', *, *, #1190, .F. ) ;
#29031 = PLANE ( 'NONE',  #44286 ) ;
#29033 = ORIENTED_EDGE ( 'NONE', *, *, #5937, .T. ) ;
#29034 = VERTEX_POINT ( 'NONE', #44189 ) ;
#29035 = LINE ( 'NONE', #60519, #20839 ) ;
#29036 = CARTESIAN_POINT ( 'NONE',  ( 7.357023737882817827, -3.848229544836346605, 54.00000000000000711 ) ) ;
#29037 = ORIENTED_EDGE ( 'NONE', *, *, #1696, .T. ) ;
#29038 = PRESENTATION_LAYER_ASSIGNMENT (  '', '', ( #44825 ) ) ;
#29039 = VERTEX_POINT ( 'NONE', #12345 ) ;
#29040 = FACE_OUTER_BOUND ( 'NONE', #42165, .T. ) ;
#29041 = DIRECTION ( 'NONE',  ( 1.000000000000000000, 0.000000000000000000, 0.000000000000000000 ) ) ;
#29042 = ORIENTED_EDGE ( 'NONE', *, *, #68272, .T. ) ;
#29043 = ORIENTED_EDGE ( 'NONE', *, *, #41885, .T. ) ;
#29044 = CIRCLE ( 'NONE', #68588, 0.3499999999999996447 ) ;
#29045 = AXIS2_PLACEMENT_3D ( 'NONE', #5181, #26744, #48313 ) ;
#29047 = DIRECTION ( 'NONE',  ( 0.7071067811865602293, 0.7071067811865348052, 2.597868168706466792E-16 ) ) ;
#29046 = VECTOR ( 'NONE', #19660, 1000.000000000000000 ) ;
#29048 = DIRECTION ( 'NONE',  ( 0.000000000000000000, -0.000000000000000000, 1.000000000000000000 ) ) ;
#29049 = VERTEX_POINT ( 'NONE', #65766 ) ;
#29050 = VECTOR ( 'NONE', #2218, 1000.000000000000000 ) ;
#29051 = EDGE_CURVE ( 'NONE', #68865, #12955, #6709, .T. ) ;
#29052 = VECTOR ( 'NONE', #26370, 1000.000000000000000 ) ;
#29053 = PLANE ( 'NONE',  #66357 ) ;
#29055 = ORIENTED_EDGE ( 'NONE', *, *, #5524, .F. ) ;
#29054 = CARTESIAN_POINT ( 'NONE',  ( 49.00000000000000000, -0.2000000000089119934, 8.909539772616881237E-12 ) ) ;
#29056 = VERTEX_POINT ( 'NONE', #50191 ) ;
#29057 = EDGE_CURVE ( 'NONE', #9204, #8160, #46503, .T. ) ;
#29058 = CARTESIAN_POINT ( 'NONE',  ( -7.250000000000000888, 8.250000000000001776, -21.00000000000000000 ) ) ;
#29059 = VECTOR ( 'NONE', #65275, 1000.000000000000000 ) ;
#29060 = FACE_OUTER_BOUND ( 'NONE', #53523, .T. ) ;
#29061 = AXIS2_PLACEMENT_3D ( 'NONE', #64610, #43032, #32444 ) ;
#29062 = CARTESIAN_POINT ( 'NONE',  ( 30.00000000000000000, -5.599999999999999645, -9.000000000000001776 ) ) ;
#29063 = EDGE_CURVE ( 'NONE', #67323, #59830, #10387, .T. ) ;
#29064 = DIRECTION ( 'NONE',  ( 0.000000000000000000, 0.000000000000000000, 1.000000000000000000 ) ) ;
#29065 = ADVANCED_FACE ( 'NONE', ( #1753 ), #23327, .T. ) ;
#29066 = FACE_OUTER_BOUND ( 'NONE', #24769, .T. ) ;
#29067 = DIRECTION ( 'NONE',  ( -0.000000000000000000, -0.000000000000000000, -1.000000000000000000 ) ) ;
#29068 = EDGE_CURVE ( 'NONE', #8035, #3393, #34263, .T. ) ;
#29069 = EDGE_CURVE ( 'NONE', #42896, #22077, #45225, .T. ) ;
#29070 = CARTESIAN_POINT ( 'NONE',  ( 49.00000000000000000, -0.1999999999911795112, 8.826273045769999343E-12 ) ) ;
#29071 = VERTEX_POINT ( 'NONE', #39916 ) ;
#29072 = DIRECTION ( 'NONE',  ( 0.000000000000000000, -0.7096009616570518874, 0.7046037717862339012 ) ) ;
#29074 = EDGE_LOOP ( 'NONE', ( #8781, #32806, #56137, #12634 ) ) ;
#29073 = DIRECTION ( 'NONE',  ( -0.000000000000000000, 3.673940397442059868E-16, -1.000000000000000000 ) ) ;
#29075 = VECTOR ( 'NONE', #47605, 1000.000000000000000 ) ;
#29076 = DIRECTION ( 'NONE',  ( 1.000000000000000000, -5.120954910632640039E-15, 0.000000000000000000 ) ) ;
#29077 = DIRECTION ( 'NONE',  ( 0.000000000000000000, 0.000000000000000000, -1.000000000000000000 ) ) ;
#29078 = ADVANCED_FACE ( 'NONE', ( #13050 ), #34620, .T. ) ;
#29079 = CARTESIAN_POINT ( 'NONE',  ( -5.538810540050023157, 7.342976262117183239, 26.00000000000000711 ) ) ;
#29080 = LINE ( 'NONE', #60893, #18209 ) ;
#29081 = DIRECTION ( 'NONE',  ( 0.000000000000000000, 0.000000000000000000, 1.000000000000000000 ) ) ;
#29082 = VERTEX_POINT ( 'NONE', #4224 ) ;
#29083 = VERTEX_POINT ( 'NONE', #30729 ) ;
#29084 = CYLINDRICAL_SURFACE ( 'NONE', #21188, 0.5249999999999999112 ) ;
#29085 = DIRECTION ( 'NONE',  ( -0.000000000000000000, 3.673940397442059868E-16, -1.000000000000000000 ) ) ;
#29086 = FACE_OUTER_BOUND ( 'NONE', #37752, .T. ) ;
#29087 = ORIENTED_EDGE ( 'NONE', *, *, #66315, .F. ) ;
#29088 = CARTESIAN_POINT ( 'NONE',  ( 4.740315990920143108, 4.188533722949256521, 195.0000000000000284 ) ) ;
#29089 = ORIENTED_EDGE ( 'NONE', *, *, #68656, .F. ) ;
#29090 = VECTOR ( 'NONE', #34025, 1000.000000000000000 ) ;
#29091 = VERTEX_POINT ( 'NONE', #51601 ) ;
#29092 = CARTESIAN_POINT ( 'NONE',  ( -7.250000000000000888, -8.249999999999998224, -26.00000000000001066 ) ) ;
#29093 = FACE_OUTER_BOUND ( 'NONE', #46053, .T. ) ;
#29094 = ORIENTED_EDGE ( 'NONE', *, *, #54552, .T. ) ;
#29095 = DIRECTION ( 'NONE',  ( 0.000000000000000000, 1.000000000000000000, 0.000000000000000000 ) ) ;
#29096 = DIRECTION ( 'NONE',  ( 9.973078850062115052E-15, 1.000000000000000000, 1.836970198721028948E-16 ) ) ;
#29097 = DIRECTION ( 'NONE',  ( 0.000000000000000000, 1.000000000000000000, 0.000000000000000000 ) ) ;
#29098 = ORIENTED_EDGE ( 'NONE', *, *, #44269, .F. ) ;
#29099 = ORIENTED_EDGE ( 'NONE', *, *, #47160, .T. ) ;
#29101 = ORIENTED_EDGE ( 'NONE', *, *, #29374, .F. ) ;
#29100 = DIRECTION ( 'NONE',  ( 0.7071067811865602293, 0.7071067811865348052, 2.597868168706465806E-16 ) ) ;
#29102 = VERTEX_POINT ( 'NONE', #46629 ) ;
#29103 = CIRCLE ( 'NONE', #30227, 4.000000000000000888 ) ;
#29104 = AXIS2_PLACEMENT_3D ( 'NONE', #44264, #17397, #69784 ) ;
#29105 = EDGE_CURVE ( 'NONE', #35311, #26457, #30022, .T. ) ;
#29106 = LINE ( 'NONE', #25203, #12270 ) ;
#29107 = CYLINDRICAL_SURFACE ( 'NONE', #33160, 24.99999999998794920 ) ;
#29108 = FACE_OUTER_BOUND ( 'NONE', #23276, .T. ) ;
#29109 = CARTESIAN_POINT ( 'NONE',  ( -7.250000000000000888, 8.250000000000001776, -18.00000000000000000 ) ) ;
#29110 = VECTOR ( 'NONE', #59774, 1000.000000000000000 ) ;
#29111 = EDGE_CURVE ( 'NONE', #32973, #7937, #40631, .T. ) ;
#29112 = EDGE_CURVE ( 'NONE', #520, #12942, #3163, .T. ) ;
#29114 = CARTESIAN_POINT ( 'NONE',  ( 290.0000000000000000, 0.000000000000000000, 0.000000000000000000 ) ) ;
#29113 = AXIS2_PLACEMENT_3D ( 'NONE', #57469, #29546, #19291 ) ;
#29115 = LINE ( 'NONE', #55637, #58997 ) ;
#29116 = ORIENTED_EDGE ( 'NONE', *, *, #6814, .F. ) ;
#29117 = VERTEX_POINT ( 'NONE', #52664 ) ;
#29118 = EDGE_CURVE ( 'NONE', #32857, #18730, #36027, .T. ) ;
#29119 = VERTEX_POINT ( 'NONE', #45939 ) ;
#29120 = DIRECTION ( 'NONE',  ( -0.7071067811865474617, -0.7071067811865474617, -2.597868168706479611E-16 ) ) ;
#29121 = LINE ( 'NONE', #55307, #15150 ) ;
#29122 = LINE ( 'NONE', #61275, #39434 ) ;
#29123 = CARTESIAN_POINT ( 'NONE',  ( 283.0000000000000568, -38.64999999999999858, 15.00000000000000000 ) ) ;
#29124 = ORIENTED_EDGE ( 'NONE', *, *, #14967, .T. ) ;
#29125 = VERTEX_POINT ( 'NONE', #14471 ) ;
#29126 = VERTEX_POINT ( 'NONE', #67857 ) ;
#29127 = CARTESIAN_POINT ( 'NONE',  ( -6.467976262117258734, 5.242976262117182706, 26.00000000000000711 ) ) ;
#29128 = EDGE_LOOP ( 'NONE', ( #68459, #38047, #31757, #14574 ) ) ;
#29129 = VERTEX_POINT ( 'NONE', #29664 ) ;
#29130 = ORIENTED_EDGE ( 'NONE', *, *, #51813, .F. ) ;
#29131 = ORIENTED_EDGE ( 'NONE', *, *, #22399, .T. ) ;
#29132 = DIRECTION ( 'NONE',  ( -0.000000000000000000, -0.000000000000000000, -1.000000000000000000 ) ) ;
#29134 = EDGE_LOOP ( 'NONE', ( #67783, #47870, #57720, #20960, #21911, #34783, #63012, #5587 ) ) ;
#29133 = DIRECTION ( 'NONE',  ( -0.000000000000000000, -0.000000000000000000, -1.000000000000000000 ) ) ;
#29135 = DIRECTION ( 'NONE',  ( 0.000000000000000000, 0.000000000000000000, 1.000000000000000000 ) ) ;
#29136 = DIRECTION ( 'NONE',  ( -8.359604446858500663E-15, -1.000000000000000000, 0.000000000000000000 ) ) ;
#29137 = CARTESIAN_POINT ( 'NONE',  ( 7.000000000000000000, -42.50000000000000000, -14.50000000000000000 ) ) ;
#29138 = AXIS2_PLACEMENT_3D ( 'NONE', #4335, #53463, #26583 ) ;
#29140 = EDGE_LOOP ( 'NONE', ( #68347, #11129, #7778, #3203, #7574, #39653 ) ) ;
#29139 = CARTESIAN_POINT ( 'NONE',  ( 106.4257688009193430, 0.000000000000000000, 330.9830310981789694 ) ) ;
#29141 = ORIENTED_EDGE ( 'NONE', *, *, #67550, .T. ) ;
#29142 = CARTESIAN_POINT ( 'NONE',  ( 7.250000000000005329, 7.250000000000000888, -26.00000000000001066 ) ) ;
#29143 = DIRECTION ( 'NONE',  ( 0.000000000000000000, 0.000000000000000000, 1.000000000000000000 ) ) ;
#29144 = LINE ( 'NONE', #55003, #10114 ) ;
#29145 = EDGE_CURVE ( 'NONE', #55686, #16950, #40974, .T. ) ;
#29146 = ORIENTED_EDGE ( 'NONE', *, *, #42251, .F. ) ;
#29147 = CARTESIAN_POINT ( 'NONE',  ( -4.173516549646666185, 11.99351654964658920, 455.0000000000000568 ) ) ;
#29148 = AXIS2_PLACEMENT_3D ( 'NONE', #7694, #8036, #23963 ) ;
#29149 = LINE ( 'NONE', #60634, #64826 ) ;
#29150 = CARTESIAN_POINT ( 'NONE',  ( 48.99818419603327868, 0.7500000000000000000, -3.928730293367447501 ) ) ;
#29151 = EDGE_CURVE ( 'NONE', #66059, #46437, #19751, .T. ) ;
#29152 = ORIENTED_EDGE ( 'NONE', *, *, #17224, .T. ) ;
#29153 = FACE_OUTER_BOUND ( 'NONE', #27820, .T. ) ;
#29154 = AXIS2_PLACEMENT_3D ( 'NONE', #51578, #24701, #62507 ) ;
#29155 = LINE ( 'NONE', #52771, #26331 ) ;
#29156 = CARTESIAN_POINT ( 'NONE',  ( -6.486996718459908884, -3.157023737882779013, 26.00000000000000711 ) ) ;
#29157 = EDGE_LOOP ( 'NONE', ( #66487, #30727, #49199, #45621 ) ) ;
#29158 = DIRECTION ( 'NONE',  ( 0.000000000000000000, 1.000000000000000000, 0.000000000000000000 ) ) ;
#29159 = DIRECTION ( 'NONE',  ( 0.000000000000000000, 0.000000000000000000, -1.000000000000000000 ) ) ;
#29160 = FACE_OUTER_BOUND ( 'NONE', #14769, .T. ) ;
#29161 = VECTOR ( 'NONE', #55099, 1000.000000000000000 ) ;
#29162 = ORIENTED_EDGE ( 'NONE', *, *, #37157, .F. ) ;
#29163 = CARTESIAN_POINT ( 'NONE',  ( 10.31452373788281562, -6.849523737882814878, 26.00000000000000000 ) ) ;
#29164 = PLANE ( 'NONE',  #60238 ) ;
#29165 = DIRECTION ( 'NONE',  ( 0.000000000000000000, 1.000000000000000000, 0.000000000000000000 ) ) ;
#29166 = PLANE ( 'NONE',  #64018 ) ;
#29167 = CYLINDRICAL_SURFACE ( 'NONE', #51091, 3.499999999999850342 ) ;
#29168 = VERTEX_POINT ( 'NONE', #3859 ) ;
#29169 = DIRECTION ( 'NONE',  ( 0.000000000000000000, -1.000000000000000000, 0.000000000000000000 ) ) ;
#29170 = DIRECTION ( 'NONE',  ( -1.836970198721029934E-16, 1.836970198721036590E-16, -1.000000000000000000 ) ) ;
#29171 = FACE_OUTER_BOUND ( 'NONE', #51059, .T. ) ;
#29172 = CARTESIAN_POINT ( 'NONE',  ( 283.0000000000000568, -40.30000000000000426, -12.20000000000000107 ) ) ;
#29173 = VERTEX_POINT ( 'NONE', #25787 ) ;
#29175 = ORIENTED_EDGE ( 'NONE', *, *, #33293, .F. ) ;
#29174 = DIRECTION ( 'NONE',  ( 1.000000000000000000, 0.000000000000000000, 0.000000000000000000 ) ) ;
#29176 = DIRECTION ( 'NONE',  ( 0.000000000000000000, 1.000000000000000000, 0.000000000000000000 ) ) ;
#29177 = CARTESIAN_POINT ( 'NONE',  ( -17.00000000000000000, -16.64230188589299786, 14.64519951917100116 ) ) ;
#29178 = ORIENTED_EDGE ( 'NONE', *, *, #46630, .T. ) ;
#29179 = PLANE ( 'NONE',  #31857 ) ;
#29180 = ORIENTED_EDGE ( 'NONE', *, *, #33939, .F. ) ;
#29181 = EDGE_CURVE ( 'NONE', #46347, #1592, #25424, .T. ) ;
#29182 = AXIS2_PLACEMENT_3D ( 'NONE', #32775, #38099, #28161 ) ;
#29183 = DIRECTION ( 'NONE',  ( 0.000000000000000000, 0.000000000000000000, 1.000000000000000000 ) ) ;
#29184 = ORIENTED_EDGE ( 'NONE', *, *, #13662, .F. ) ;
#29185 = ORIENTED_EDGE ( 'NONE', *, *, #51832, .F. ) ;
#29186 = CARTESIAN_POINT ( 'NONE',  ( 25.50000000000000355, -5.578999999999999737, -22.50000000000000000 ) ) ;
#29187 = DIRECTION ( 'NONE',  ( 0.000000000000000000, 1.000000000000000000, 0.000000000000000000 ) ) ;
#29188 = CIRCLE ( 'NONE', #25846, 0.2999999999994933386 ) ;
#29189 = CARTESIAN_POINT ( 'NONE',  ( 30.00000000000000000, -17.14999999999999858, 27.00000000000000000 ) ) ;
#29190 = CARTESIAN_POINT ( 'NONE',  ( -7.603567055985545942, 8.593516549646603053, 455.0000000000000568 ) ) ;
#29191 = EDGE_LOOP ( 'NONE', ( #37995, #45875, #69264, #62869, #15812, #9518, #61596, #2964, #49857, #61521, #33732, #2336, #3739, #21076, #15416, #7661 ) ) ;
#29192 = VERTEX_POINT ( 'NONE', #68912 ) ;
#29193 = CARTESIAN_POINT ( 'NONE',  ( 15.50000000000129852, -15.50000000000000000, 22.50000000000000000 ) ) ;
#29194 = VECTOR ( 'NONE', #59251, 999.9999999999998863 ) ;
#29195 = DIRECTION ( 'NONE',  ( 0.000000000000000000, 0.000000000000000000, 1.000000000000000000 ) ) ;
#29196 = EDGE_CURVE ( 'NONE', #33331, #69428, #39729, .T. ) ;
#29197 = ORIENTED_EDGE ( 'NONE', *, *, #27990, .T. ) ;
#29198 = ORIENTED_EDGE ( 'NONE', *, *, #36367, .F. ) ;
#29199 = ORIENTED_EDGE ( 'NONE', *, *, #48811, .T. ) ;
#29200 = EDGE_CURVE ( 'NONE', #44134, #29889, #31081, .T. ) ;
#29201 = FACE_OUTER_BOUND ( 'NONE', #37591, .T. ) ;
#29203 = EDGE_LOOP ( 'NONE', ( #16202, #51128, #24367, #2678 ) ) ;
#29202 = CARTESIAN_POINT ( 'NONE',  ( -4.727349090213463612, 7.798499376343949407, 455.0000000000000568 ) ) ;
#29204 = CIRCLE ( 'NONE', #39406, 0.3499999999999996447 ) ;
#29205 = CARTESIAN_POINT ( 'NONE',  ( 30.00000000000000000, -8.959999999999999076, -12.95475478405700009 ) ) ;
#29206 = CARTESIAN_POINT ( 'NONE',  ( -2.752095193409373586, 9.942044687070435316, 455.0000000000000568 ) ) ;
#29207 = ORIENTED_EDGE ( 'NONE', *, *, #42420, .T. ) ;
#29208 = VERTEX_POINT ( 'NONE', #30378 ) ;
#29209 = DIRECTION ( 'NONE',  ( 0.000000000000000000, 0.000000000000000000, 1.000000000000000000 ) ) ;
#29210 = CARTESIAN_POINT ( 'NONE',  ( 7.606483450353380249, -11.32648345035339155, 195.0000000000000284 ) ) ;
#29211 = FACE_OUTER_BOUND ( 'NONE', #5835, .T. ) ;
#29212 = ADVANCED_FACE ( 'NONE', ( #62906 ), #51951, .F. ) ;
#29213 = DIRECTION ( 'NONE',  ( 1.000000000000000000, 0.000000000000000000, 0.000000000000000000 ) ) ;
#29214 = CARTESIAN_POINT ( 'NONE',  ( -11.00000000000000000, -9.487228132326899654, -12.50000000000000000 ) ) ;
#29215 = EDGE_CURVE ( 'NONE', #868, #16845, #63258, .T. ) ;
#29216 = EDGE_CURVE ( 'NONE', #46451, #51473, #20122, .T. ) ;
#29218 = ORIENTED_EDGE ( 'NONE', *, *, #34405, .T. ) ;
#29217 = DIRECTION ( 'NONE',  ( 0.000000000000000000, 1.000000000000000000, 0.000000000000000000 ) ) ;
#29219 = EDGE_LOOP ( 'NONE', ( #54723, #1642, #2941, #6167 ) ) ;
#29220 = CARTESIAN_POINT ( 'NONE',  ( 276.8000000000000682, -25.60000000000000142, 17.60000000000000142 ) ) ;
#29221 = DIRECTION ( 'NONE',  ( 1.000000000000000000, -0.000000000000000000, 0.000000000000000000 ) ) ;
#29222 = EDGE_CURVE ( 'NONE', #61067, #13213, #63615, .T. ) ;
#29223 = FACE_OUTER_BOUND ( 'NONE', #25060, .T. ) ;
#29224 = CIRCLE ( 'NONE', #58594, 5.000000000000000000 ) ;
#29225 = CYLINDRICAL_SURFACE ( 'NONE', #50014, 4.000000000000000000 ) ;
#29226 = EDGE_CURVE ( 'NONE', #46315, #9955, #26237, .T. ) ;
#29227 = ORIENTED_EDGE ( 'NONE', *, *, #55078, .T. ) ;
#29228 = LINE ( 'NONE', #50802, #25641 ) ;
#29229 = CARTESIAN_POINT ( 'NONE',  ( -7.250000000000000888, 7.450000000000003730, -22.50000000000000000 ) ) ;
#29231 = ADVANCED_FACE ( 'NONE', ( #67520 ), #19065, .T. ) ;
#29230 = DIRECTION ( 'NONE',  ( 0.000000000000000000, 0.000000000000000000, 1.000000000000000000 ) ) ;
#29232 = VECTOR ( 'NONE', #44933, 1000.000000000000000 ) ;
#29233 = CARTESIAN_POINT ( 'NONE',  ( -8.697938382363185283, -8.093267424590415260, 54.00000000000000711 ) ) ;
#29234 = CARTESIAN_POINT ( 'NONE',  ( -8.916576262117260399, 8.566576262117216345, 54.00000000000000711 ) ) ;
#29235 = CARTESIAN_POINT ( 'NONE',  ( 6.836383711243005479, -6.364920264886896994, 26.00000000000000711 ) ) ;
#29236 = VECTOR ( 'NONE', #18100, 1000.000000000000000 ) ;
#29237 = CARTESIAN_POINT ( 'NONE',  ( 14.50000000000000000, -42.50000000000000000, 30.00000000000000000 ) ) ;
#29238 = ORIENTED_EDGE ( 'NONE', *, *, #52986, .T. ) ;
#29239 = DIRECTION ( 'NONE',  ( 1.011922027653137735E-14, 1.000000000000000000, 0.000000000000000000 ) ) ;
#29240 = LINE ( 'NONE', #8374, #50789 ) ;
#29241 = VERTEX_POINT ( 'NONE', #56885 ) ;
#29242 = DIRECTION ( 'NONE',  ( 1.000000000000000000, 0.000000000000000000, 0.000000000000000000 ) ) ;
#29243 = DIRECTION ( 'NONE',  ( 0.000000000000000000, 0.000000000000000000, 1.000000000000000000 ) ) ;
#29244 = VECTOR ( 'NONE', #64561, 1000.000000000000000 ) ;
#29245 = CARTESIAN_POINT ( 'NONE',  ( -15.50000000000000000, -0.4000000000000000222, 19.00000000000000355 ) ) ;
#29246 = DIRECTION ( 'NONE',  ( 0.000000000000000000, 0.000000000000000000, -1.000000000000000000 ) ) ;
#29247 = ORIENTED_EDGE ( 'NONE', *, *, #42317, .F. ) ;
#29249 = VECTOR ( 'NONE', #2008, 1000.000000000000000 ) ;
#29248 = CIRCLE ( 'NONE', #37173, 0.8099999999999999423 ) ;
#29250 = DIRECTION ( 'NONE',  ( 0.000000000000000000, 0.000000000000000000, 1.000000000000000000 ) ) ;
#29251 = EDGE_LOOP ( 'NONE', ( #54641, #9287, #65855, #48033 ) ) ;
#29252 = CARTESIAN_POINT ( 'NONE',  ( -30.00000000000000000, -5.200000000000001066, -26.59999999999999787 ) ) ;
#29253 = EDGE_CURVE ( 'NONE', #12885, #39877, #66838, .T. ) ;
#29254 = VERTEX_POINT ( 'NONE', #54390 ) ;
#29255 = CARTESIAN_POINT ( 'NONE',  ( 15.50000000000000000, -0.4000000000005274892, -25.79999999999946780 ) ) ;
#29256 = VECTOR ( 'NONE', #12011, 1000.000000000000000 ) ;
#29257 = ORIENTED_EDGE ( 'NONE', *, *, #26353, .F. ) ;
#29258 = ADVANCED_FACE ( 'NONE', ( #5603 ), #5943, .T. ) ;
#29259 = DIRECTION ( 'NONE',  ( 1.088659024508174415E-14, 1.000000000000000000, 1.836970198721030674E-16 ) ) ;
#29260 = ORIENTED_EDGE ( 'NONE', *, *, #62478, .T. ) ;
#29261 = ORIENTED_EDGE ( 'NONE', *, *, #25167, .F. ) ;
#29262 = CARTESIAN_POINT ( 'NONE',  ( 8.250000000000005329, -8.249999999999998224, -26.00000000000001066 ) ) ;
#29263 = ORIENTED_EDGE ( 'NONE', *, *, #65300, .F. ) ;
#29264 = ORIENTED_EDGE ( 'NONE', *, *, #55596, .F. ) ;
#29265 = CARTESIAN_POINT ( 'NONE',  ( 7.450000000000006395, 7.250000000000000888, -11.50000000000000000 ) ) ;
#29266 = CARTESIAN_POINT ( 'NONE',  ( 7.250000000000005329, -8.249999999999998224, -20.50000000000000000 ) ) ;
#29267 = DIRECTION ( 'NONE',  ( -0.9583148474998867128, 0.000000000000000000, 0.2857142857143631365 ) ) ;
#29268 = VECTOR ( 'NONE', #39467, 1000.000000000000000 ) ;
#29269 = EDGE_LOOP ( 'NONE', ( #2060, #38184, #47303, #48262 ) ) ;
#29270 = CARTESIAN_POINT ( 'NONE',  ( 8.250000000000005329, -8.249999999999998224, -26.00000000000001066 ) ) ;
#29272 = LINE ( 'NONE', #24691, #40099 ) ;
#29271 = DIRECTION ( 'NONE',  ( 1.000000000000000000, 0.000000000000000000, 0.000000000000000000 ) ) ;
#29273 = ORIENTED_EDGE ( 'NONE', *, *, #38205, .T. ) ;
#29275 = ORIENTED_EDGE ( 'NONE', *, *, #45909, .T. ) ;
#29274 = LINE ( 'NONE', #50849, #64748 ) ;
#29276 = ORIENTED_EDGE ( 'NONE', *, *, #36883, .F. ) ;
#29277 =( LENGTH_UNIT ( ) NAMED_UNIT ( * ) SI_UNIT ( .MILLI., .METRE. ) );
#29278 = EDGE_CURVE ( 'NONE', #57470, #997, #69257, .T. ) ;
#29279 = DIRECTION ( 'NONE',  ( 0.000000000000000000, 1.000000000000000000, 0.000000000000000000 ) ) ;
#29280 = AXIS2_PLACEMENT_3D ( 'NONE', #46145, #8309, #8673 ) ;
#29281 = CIRCLE ( 'NONE', #63173, 0.3999999999999993006 ) ;
#29282 = ORIENTED_EDGE ( 'NONE', *, *, #18582, .F. ) ;
#29283 = CARTESIAN_POINT ( 'NONE',  ( 7.250000000000005329, 7.250000000000000888, -26.00000000000001066 ) ) ;
#29284 = DIRECTION ( 'NONE',  ( -1.000000000000000000, 1.088659024508174257E-14, 0.000000000000000000 ) ) ;
#29285 = ORIENTED_EDGE ( 'NONE', *, *, #15540, .T. ) ;
#29286 = ADVANCED_FACE ( 'NONE', ( #5267 ), #53011, .F. ) ;
#29287 = VERTEX_POINT ( 'NONE', #53356 ) ;
#29288 = EDGE_CURVE ( 'NONE', #59582, #61023, #43416, .T. ) ;
#29289 = VECTOR ( 'NONE', #4657, 1000.000000000000000 ) ;
#29290 = CARTESIAN_POINT ( 'NONE',  ( 16.75000000000000000, -2.500000000000000000, 23.22168783648699986 ) ) ;
#29291 = CARTESIAN_POINT ( 'NONE',  ( -3.842976262117324016, -9.912023737882812213, 26.00000000000000000 ) ) ;
#29292 = EDGE_CURVE ( 'NONE', #51111, #54102, #44278, .T. ) ;
#29293 = ADVANCED_FACE ( 'NONE', ( #36736 ), #15173, .F. ) ;
#29294 = EDGE_CURVE ( 'NONE', #24330, #10503, #32812, .T. ) ;
#29295 = ORIENTED_EDGE ( 'NONE', *, *, #10560, .T. ) ;
#29296 = VECTOR ( 'NONE', #10060, 1000.000000000000000 ) ;
#29297 = PLANE ( 'NONE',  #9897 ) ;
#29298 = DIRECTION ( 'NONE',  ( -1.000000000000000000, 3.491481338843133355E-15, 1.836970198721036344E-16 ) ) ;
#29299 = DIRECTION ( 'NONE',  ( 0.000000000000000000, 0.000000000000000000, -1.000000000000000000 ) ) ;
#29300 = ORIENTED_EDGE ( 'NONE', *, *, #21733, .T. ) ;
#29301 = EDGE_CURVE ( 'NONE', #35322, #12465, #9875, .T. ) ;
#29302 = VECTOR ( 'NONE', #69103, 1000.000000000000000 ) ;
#29303 = DIRECTION ( 'NONE',  ( 0.000000000000000000, 0.000000000000000000, 1.000000000000000000 ) ) ;
#29304 = EDGE_CURVE ( 'NONE', #52054, #63857, #15866, .T. ) ;
#29305 = LINE ( 'NONE', #56879, #58517 ) ;
#29306 = EDGE_LOOP ( 'NONE', ( #25911, #38029, #12929, #35469 ) ) ;
#29308 = VERTEX_POINT ( 'NONE', #32126 ) ;
#29307 = DIRECTION ( 'NONE',  ( -1.073876437509453175E-14, -1.000000000000000000, 0.000000000000000000 ) ) ;
#29309 = ADVANCED_FACE ( 'NONE', ( #31448 ), #48388, .F. ) ;
#29310 = CARTESIAN_POINT ( 'NONE',  ( 3.848229544836330174, 7.517976262117205266, 54.00000000000000711 ) ) ;
#29311 = AXIS2_PLACEMENT_3D ( 'NONE', #9836, #25388, #63578 ) ;
#29312 = DIRECTION ( 'NONE',  ( -9.050731179009442381E-15, -1.000000000000000000, 0.000000000000000000 ) ) ;
#29313 = DIRECTION ( 'NONE',  ( 1.000000000000000000, -1.203165845134433084E-14, -1.836970198721051874E-16 ) ) ;
#29314 = DIRECTION ( 'NONE',  ( -1.000000000000000000, 1.794541526872559352E-16, 0.000000000000000000 ) ) ;
#29315 = DIRECTION ( 'NONE',  ( 0.000000000000000000, -1.000000000000000000, 0.000000000000000000 ) ) ;
#29316 = EDGE_CURVE ( 'NONE', #17328, #32965, #45385, .T. ) ;
#29317 = VERTEX_POINT ( 'NONE', #37094 ) ;
#29318 = CARTESIAN_POINT ( 'NONE',  ( -28.00000000000000000, -17.35230188589299871, 15.35019951917099945 ) ) ;
#29319 = CARTESIAN_POINT ( 'NONE',  ( 11.00000000000000000, -11.50000000000082068, -10.20500000000000007 ) ) ;
#29321 = EDGE_CURVE ( 'NONE', #35101, #22946, #2488, .T. ) ;
#29320 = PRESENTATION_STYLE_ASSIGNMENT (( #7758 ) ) ;
#29323 = ORIENTED_EDGE ( 'NONE', *, *, #16480, .T. ) ;
#29322 = CARTESIAN_POINT ( 'NONE',  ( 10.50702373788281285, 9.781776262117176657, 26.00000000000000711 ) ) ;
#29324 = DIRECTION ( 'NONE',  ( 1.000000000000000000, 0.000000000000000000, 0.000000000000000000 ) ) ;
#29325 = AXIS2_PLACEMENT_3D ( 'NONE', #10786, #65252, #63847 ) ;
#29326 = DIRECTION ( 'NONE',  ( 0.000000000000000000, 0.000000000000000000, 1.000000000000000000 ) ) ;
#29327 = ORIENTED_EDGE ( 'NONE', *, *, #41287, .T. ) ;
#29328 = CARTESIAN_POINT ( 'NONE',  ( 11.50000000000000000, -12.00000000000000000, -10.52786404500095863 ) ) ;
#29329 = CARTESIAN_POINT ( 'NONE',  ( 8.144523737882815695, 9.547976262117185087, 54.00000000000000711 ) ) ;
#29330 = EDGE_CURVE ( 'NONE', #20601, #49081, #69949, .T. ) ;
#29331 = ORIENTED_EDGE ( 'NONE', *, *, #62930, .F. ) ;
#29332 = DIRECTION ( 'NONE',  ( -1.047444401652940007E-14, -1.000000000000000000, -1.836970198721029934E-16 ) ) ;
#29333 = CARTESIAN_POINT ( 'NONE',  ( 19.90000000000000213, -0.000000000000000000, -20.80000000000000426 ) ) ;
#29334 =( NAMED_UNIT ( * ) PLANE_ANGLE_UNIT ( ) SI_UNIT ( $, .RADIAN. ) );
#29335 = DIRECTION ( 'NONE',  ( -0.000000000000000000, -0.000000000000000000, 1.000000000000000000 ) ) ;
#29336 = VECTOR ( 'NONE', #4080, 1000.000000000000000 ) ;
#29337 = AXIS2_PLACEMENT_3D ( 'NONE', #43031, #64609, #16522 ) ;
#29338 = DIRECTION ( 'NONE',  ( 0.000000000000000000, 1.000000000000000000, 0.000000000000000000 ) ) ;
#29339 = AXIS2_PLACEMENT_3D ( 'NONE', #52222, #25358, #63546 ) ;
#29340 = ORIENTED_EDGE ( 'NONE', *, *, #25397, .T. ) ;
#29341 = PLANE ( 'NONE',  #49566 ) ;
#29342 = ORIENTED_EDGE ( 'NONE', *, *, #29710, .F. ) ;
#29343 = ORIENTED_EDGE ( 'NONE', *, *, #13749, .F. ) ;
#29344 = AXIS2_PLACEMENT_3D ( 'NONE', #11926, #6638, #28207 ) ;
#29345 = DIRECTION ( 'NONE',  ( 0.000000000000000000, 0.000000000000000000, 1.000000000000000000 ) ) ;
#29346 = VECTOR ( 'NONE', #6991, 1000.000000000000000 ) ;
#29347 = EDGE_CURVE ( 'NONE', #35347, #39629, #10552, .T. ) ;
#29348 = DIRECTION ( 'NONE',  ( 0.000000000000000000, 0.000000000000000000, -1.000000000000000000 ) ) ;
#29350 = LINE ( 'NONE', #64344, #50185 ) ;
#29349 = CARTESIAN_POINT ( 'NONE',  ( 22.90000000000000213, -0.1999999999911430404, -8.864436962241481021E-12 ) ) ;
#29351 = ORIENTED_EDGE ( 'NONE', *, *, #47815, .T. ) ;
#29352 = VERTEX_POINT ( 'NONE', #32484 ) ;
#29353 = CARTESIAN_POINT ( 'NONE',  ( 27.00000000000000000, 0.000000000000000000, 0.000000000000000000 ) ) ;
#29354 = ORIENTED_EDGE ( 'NONE', *, *, #56331, .F. ) ;
#29355 = VECTOR ( 'NONE', #59108, 1000.000000000000000 ) ;
#29356 = EDGE_CURVE ( 'NONE', #8058, #49494, #54049, .T. ) ;
#29357 = LINE ( 'NONE', #7447, #66550 ) ;
#29358 = DIRECTION ( 'NONE',  ( 1.000000000000000000, -0.000000000000000000, 0.000000000000000000 ) ) ;
#29359 = DIRECTION ( 'NONE',  ( -0.000000000000000000, -0.000000000000000000, -1.000000000000000000 ) ) ;
#29360 = LINE ( 'NONE', #65813, #36486 ) ;
#29361 = ORIENTED_EDGE ( 'NONE', *, *, #12840, .F. ) ;
#29362 = EDGE_CURVE ( 'NONE', #26162, #9194, #38139, .T. ) ;
#29363 = LINE ( 'NONE', #18397, #39061 ) ;
#29364 = AXIS2_PLACEMENT_3D ( 'NONE', #3951, #41063, #52040 ) ;
#29365 = VECTOR ( 'NONE', #58180, 1000.000000000000000 ) ;
#29367 = CARTESIAN_POINT ( 'NONE',  ( 7.900000000000000355, 21.00000000000000000, 18.00000000000000355 ) ) ;
#29366 = LINE ( 'NONE', #50937, #50175 ) ;
#29368 = ORIENTED_EDGE ( 'NONE', *, *, #64844, .F. ) ;
#29369 = EDGE_CURVE ( 'NONE', #6930, #45407, #44442, .T. ) ;
#29371 = ORIENTED_EDGE ( 'NONE', *, *, #15423, .T. ) ;
#29370 = DIRECTION ( 'NONE',  ( -1.000000000000000000, 0.000000000000000000, 0.000000000000000000 ) ) ;
#29372 = ORIENTED_EDGE ( 'NONE', *, *, #57417, .T. ) ;
#29373 = VERTEX_POINT ( 'NONE', #17924 ) ;
#29374 = EDGE_CURVE ( 'NONE', #4410, #6935, #55428, .T. ) ;
#29375 = DIRECTION ( 'NONE',  ( 0.7071067811865500152, 0.7071067811865451302, 0.000000000000000000 ) ) ;
#29376 = CARTESIAN_POINT ( 'NONE',  ( 275.0000000000000000, -42.00000000000000000, 26.50000000000000000 ) ) ;
#29377 = ORIENTED_EDGE ( 'NONE', *, *, #60779, .F. ) ;
#29378 = ORIENTED_EDGE ( 'NONE', *, *, #48773, .T. ) ;
#29379 = EDGE_CURVE ( 'NONE', #51438, #31236, #17578, .T. ) ;
#29380 = ADVANCED_FACE ( 'NONE', ( #12609 ), #11571, .F. ) ;
#29381 = CARTESIAN_POINT ( 'NONE',  ( -11.18999999999999950, 12.00000000000000178, 0.000000000000000000 ) ) ;
#29382 = CARTESIAN_POINT ( 'NONE',  ( 275.0000000000000000, -38.64999999999999858, 15.00000000000000000 ) ) ;
#29383 = ORIENTED_EDGE ( 'NONE', *, *, #22895, .F. ) ;
#29384 = ADVANCED_FACE ( 'NONE', ( #22555 ), #33506, .T. ) ;
#29385 = EDGE_CURVE ( 'NONE', #11645, #6322, #28876, .T. ) ;
#29386 = ORIENTED_EDGE ( 'NONE', *, *, #25150, .T. ) ;
#29387 = DIRECTION ( 'NONE',  ( -0.000000000000000000, 3.673940397442059868E-16, -1.000000000000000000 ) ) ;
#29388 = VECTOR ( 'NONE', #19491, 1000.000000000000000 ) ;
#29389 = LINE ( 'NONE', #12089, #19869 ) ;
#29390 = AXIS2_PLACEMENT_3D ( 'NONE', #7384, #7735, #38547 ) ;
#29391 = ORIENTED_EDGE ( 'NONE', *, *, #41424, .T. ) ;
#29392 = EDGE_CURVE ( 'NONE', #28928, #37936, #65683, .T. ) ;
#29393 = VECTOR ( 'NONE', #37034, 1000.000000000000000 ) ;
#29394 = DIRECTION ( 'NONE',  ( -0.000000000000000000, -0.000000000000000000, -1.000000000000000000 ) ) ;
#29395 = LINE ( 'NONE', #13837, #52025 ) ;
#29397 = ORIENTED_EDGE ( 'NONE', *, *, #68240, .F. ) ;
#29396 = DIRECTION ( 'NONE',  ( -0.000000000000000000, -0.000000000000000000, -1.000000000000000000 ) ) ;
#29398 = ORIENTED_EDGE ( 'NONE', *, *, #44980, .T. ) ;
#29399 = VECTOR ( 'NONE', #4831, 1000.000000000000000 ) ;
#29400 = LINE ( 'NONE', #20197, #11328 ) ;
#29401 = CARTESIAN_POINT ( 'NONE',  ( 23.90000000000000213, -0.000000000000000000, 20.80000000000000426 ) ) ;
#29402 = CARTESIAN_POINT ( 'NONE',  ( 4.201500623656004407, 4.727349090213387228, 195.0000000000000284 ) ) ;
#29403 = DIRECTION ( 'NONE',  ( 1.000000000000000000, 0.000000000000000000, 0.000000000000000000 ) ) ;
#29404 = LINE ( 'NONE', #46028, #38023 ) ;
#29405 = AXIS2_PLACEMENT_3D ( 'NONE', #64941, #54681, #39099 ) ;
#29406 = LINE ( 'NONE', #68296, #40683 ) ;
#29408 = CIRCLE ( 'NONE', #7953, 25.39999999999999858 ) ;
#29407 = LINE ( 'NONE', #66882, #62927 ) ;
#29409 = EDGE_CURVE ( 'NONE', #5287, #56170, #12261, .T. ) ;
#29410 = VERTEX_POINT ( 'NONE', #39490 ) ;
#29411 = DIRECTION ( 'NONE',  ( -1.000000000000000000, 0.000000000000000000, 0.000000000000000000 ) ) ;
#29414 = VERTEX_POINT ( 'NONE', #27862 ) ;
#29413 = ADVANCED_FACE ( 'NONE', ( #33154 ), #34175, .T. ) ;
#29412 = CARTESIAN_POINT ( 'NONE',  ( 25.50000000000000355, -5.200000000000001066, 22.50000000000000000 ) ) ;
#29415 = DIRECTION ( 'NONE',  ( 0.000000000000000000, 3.673940397442059868E-16, -1.000000000000000000 ) ) ;
#29416 = DIRECTION ( 'NONE',  ( -1.000000000000000000, 1.047444401652940007E-14, -1.836970198721010706E-16 ) ) ;
#29417 = DIRECTION ( 'NONE',  ( -1.062075597536821205E-14, -1.000000000000000000, 0.000000000000000000 ) ) ;
#29418 = PLANE ( 'NONE',  #36293 ) ;
#29419 = VECTOR ( 'NONE', #35401, 1000.000000000000000 ) ;
#29420 = VECTOR ( 'NONE', #50342, 1000.000000000000000 ) ;
#29421 = DIRECTION ( 'NONE',  ( -1.000000000000000000, 0.000000000000000000, 0.000000000000000000 ) ) ;
#29422 = ORIENTED_EDGE ( 'NONE', *, *, #65869, .F. ) ;
#29423 = DIRECTION ( 'NONE',  ( -0.000000000000000000, -0.7071067811865474617, 0.7071067811865474617 ) ) ;
#29424 = ORIENTED_EDGE ( 'NONE', *, *, #67643, .T. ) ;
#29425 = DIRECTION ( 'NONE',  ( 0.000000000000000000, 0.000000000000000000, 1.000000000000000000 ) ) ;
#29426 = PLANE ( 'NONE',  #52411 ) ;
#29427 = VERTEX_POINT ( 'NONE', #2022 ) ;
#29428 = AXIS2_PLACEMENT_3D ( 'NONE', #40953, #67837, #62510 ) ;
#29429 = DIRECTION ( 'NONE',  ( -1.000000000000000000, 0.000000000000000000, 0.000000000000000000 ) ) ;
#29430 = ORIENTED_EDGE ( 'NONE', *, *, #8976, .F. ) ;
#29431 = ORIENTED_EDGE ( 'NONE', *, *, #56752, .F. ) ;
#29432 = CARTESIAN_POINT ( 'NONE',  ( -7.342976262117259623, 4.947141984184421304, 54.00000000000000711 ) ) ;
#29433 = CARTESIAN_POINT ( 'NONE',  ( -7.250000000000000888, 7.450000000000003730, -7.500000000000000000 ) ) ;
#29434 = EDGE_LOOP ( 'NONE', ( #3199, #19993, #25680, #65301 ) ) ;
#29435 = FACE_OUTER_BOUND ( 'NONE', #44165, .T. ) ;
#29436 = CARTESIAN_POINT ( 'NONE',  ( 10.31452373788281562, -6.657023737882825642, 54.00000000000000711 ) ) ;
#29437 = CARTESIAN_POINT ( 'NONE',  ( 7.500000000000000000, -53.81370849898476649, -16.00000000000000000 ) ) ;
#29438 = ORIENTED_EDGE ( 'NONE', *, *, #16355, .T. ) ;
#29439 = ORIENTED_EDGE ( 'NONE', *, *, #47143, .F. ) ;
#29440 = VECTOR ( 'NONE', #2440, 1000.000000000000000 ) ;
#29442 = ORIENTED_EDGE ( 'NONE', *, *, #19126, .T. ) ;
#29441 = LINE ( 'NONE', #51017, #7998 ) ;
#29443 = ORIENTED_EDGE ( 'NONE', *, *, #63492, .T. ) ;
#29444 = EDGE_CURVE ( 'NONE', #61792, #46863, #3668, .T. ) ;
#29445 = PRODUCT_DEFINITION_SHAPE ( 'NONE', 'NONE',  #38746 ) ;
#29446 = VECTOR ( 'NONE', #54389, 1000.000000000000114 ) ;
#29447 = VECTOR ( 'NONE', #52027, 1000.000000000000000 ) ;
#29448 = CARTESIAN_POINT ( 'NONE',  ( 14.50000000000000000, -42.00000000000000000, 27.00000000000000000 ) ) ;
#29449 = CARTESIAN_POINT ( 'NONE',  ( 11.90000000000000036, 20.60000000000000142, 13.86939075806899702 ) ) ;
#29450 = DIRECTION ( 'NONE',  ( 1.836970198721029934E-16, 1.836970198721010706E-16, -1.000000000000000000 ) ) ;
#29451 = FACE_OUTER_BOUND ( 'NONE', #69612, .T. ) ;
#29453 = ADVANCED_FACE ( 'NONE', ( #55090 ), #11918, .F. ) ;
#29452 = VECTOR ( 'NONE', #2817, 1000.000000000000000 ) ;
#29454 = CARTESIAN_POINT ( 'NONE',  ( -9.828310488886053520, 2.277516549646603661, 455.0000000000000568 ) ) ;
#29455 = DIRECTION ( 'NONE',  ( -1.000000000000000000, 0.000000000000000000, 0.000000000000000000 ) ) ;
#29456 = EDGE_CURVE ( 'NONE', #47564, #63930, #7663, .T. ) ;
#29457 = VERTEX_POINT ( 'NONE', #33837 ) ;
#29458 = ORIENTED_EDGE ( 'NONE', *, *, #46045, .F. ) ;
#29459 = EDGE_CURVE ( 'NONE', #46212, #8276, #7027, .T. ) ;
#29460 = ORIENTED_EDGE ( 'NONE', *, *, #48965, .F. ) ;
#29461 = VECTOR ( 'NONE', #43283, 1000.000000000000000 ) ;
#29462 = CIRCLE ( 'NONE', #61193, 0.5000000000079362072 ) ;
#29463 = ORIENTED_EDGE ( 'NONE', *, *, #23873, .F. ) ;
#29464 = DIRECTION ( 'NONE',  ( 1.000000000000000000, -0.000000000000000000, -0.000000000000000000 ) ) ;
#29465 = EDGE_CURVE ( 'NONE', #52164, #60151, #25113, .T. ) ;
#29466 = ADVANCED_FACE ( 'NONE', ( #28535 ), #1660, .F. ) ;
#29467 = CARTESIAN_POINT ( 'NONE',  ( 83.97321854994621049, 47.95351654967443977, 15.00000000000000000 ) ) ;
#29468 = AXIS2_PLACEMENT_3D ( 'NONE', #43287, #27381, #65551 ) ;
#29469 = CARTESIAN_POINT ( 'NONE',  ( -7.450000000000001954, 0.000000000000000000, -14.00000000000000000 ) ) ;
#29470 = DIRECTION ( 'NONE',  ( 1.000000000000000000, -0.000000000000000000, -0.000000000000000000 ) ) ;
#29471 = ORIENTED_EDGE ( 'NONE', *, *, #27090, .F. ) ;
#29472 = ORIENTED_EDGE ( 'NONE', *, *, #29301, .T. ) ;
#29473 = EDGE_LOOP ( 'NONE', ( #14420, #40568, #74, #13170 ) ) ;
#29475 = LINE ( 'NONE', #8245, #61006 ) ;
#29474 = AXIS2_PLACEMENT_3D ( 'NONE', #9345, #57778, #30217 ) ;
#29476 = ORIENTED_EDGE ( 'NONE', *, *, #5303, .T. ) ;
#29477 = ORIENTED_EDGE ( 'NONE', *, *, #35031, .T. ) ;
#29478 = VERTEX_POINT ( 'NONE', #50797 ) ;
#29479 = VERTEX_POINT ( 'NONE', #2369 ) ;
#29480 = LINE ( 'NONE', #34780, #10199 ) ;
#29482 = ORIENTED_EDGE ( 'NONE', *, *, #48028, .T. ) ;
#29481 = LINE ( 'NONE', #12172, #31151 ) ;
#29483 = ORIENTED_EDGE ( 'NONE', *, *, #51048, .F. ) ;
#29484 = FACE_OUTER_BOUND ( 'NONE', #13076, .T. ) ;
#29485 = LINE ( 'NONE', #51054, #4724 ) ;
#29486 = CIRCLE ( 'NONE', #31783, 0.2000000000000005107 ) ;
#29487 = CARTESIAN_POINT ( 'NONE',  ( 9.804883450353456098, 11.07551654964653132, 455.0000000000000568 ) ) ;
#29489 = VERTEX_POINT ( 'NONE', #65348 ) ;
#29488 = DIRECTION ( 'NONE',  ( 0.000000000000000000, 0.000000000000000000, 1.000000000000000000 ) ) ;
#29490 = ORIENTED_EDGE ( 'NONE', *, *, #23037, .F. ) ;
#29491 = DIRECTION ( 'NONE',  ( 0.000000000000000000, 0.000000000000000000, 1.000000000000000000 ) ) ;
#29492 = CARTESIAN_POINT ( 'NONE',  ( -10.08346604330787777, 2.893516549646604208, 455.0000000000000568 ) ) ;
#29493 = PLANE ( 'NONE',  #68860 ) ;
#29494 = AXIS2_PLACEMENT_3D ( 'NONE', #34791, #56365, #62012 ) ;
#29495 = ORIENTED_EDGE ( 'NONE', *, *, #10433, .F. ) ;
#29496 = DIRECTION ( 'NONE',  ( -1.836970198721029934E-16, 1.836970198721036590E-16, -1.000000000000000000 ) ) ;
#29497 = EDGE_CURVE ( 'NONE', #62940, #68694, #16904, .T. ) ;
#29498 = CARTESIAN_POINT ( 'NONE',  ( 6.849523737882817542, -10.31452373788281207, 26.00000000000000000 ) ) ;
#29499 = CIRCLE ( 'NONE', #56606, 1.620999999999997332 ) ;
#29500 = CARTESIAN_POINT ( 'NONE',  ( 283.0000000000000568, -38.64999999999999858, 15.00000000000000000 ) ) ;
#29501 = ORIENTED_EDGE ( 'NONE', *, *, #60910, .T. ) ;
#29502 = EDGE_CURVE ( 'NONE', #29645, #4880, #36294, .T. ) ;
#29503 = FACE_OUTER_BOUND ( 'NONE', #53642, .T. ) ;
#29504 = CARTESIAN_POINT ( 'NONE',  ( 9.106483450353373144, 11.11351654964661329, 195.0000000000000284 ) ) ;
#29505 = CARTESIAN_POINT ( 'NONE',  ( -10.73351654964663915, -1.090483450353293415, 195.0000000000000284 ) ) ;
#29506 = EDGE_CURVE ( 'NONE', #6091, #30940, #3765, .T. ) ;
#29508 = EDGE_CURVE ( 'NONE', #25597, #32858, #29931, .T. ) ;
#29507 = CIRCLE ( 'NONE', #46467, 1.500000000000000444 ) ;
#29509 = CIRCLE ( 'NONE', #21610, 0.1999999999999987899 ) ;
#29510 = EDGE_LOOP ( 'NONE', ( #11277, #9675, #36074, #63843 ) ) ;
#29511 = CARTESIAN_POINT ( 'NONE',  ( -6.486996718459931088, 3.142976262117182173, 26.00000000000000711 ) ) ;
#29512 = LINE ( 'NONE', #19954, #19780 ) ;
#29513 = AXIS2_PLACEMENT_3D ( 'NONE', #84, #65136, #53482 ) ;
#29514 = CARTESIAN_POINT ( 'NONE',  ( 280.0000000000000000, -20.49999999999999645, -16.00000000000000711 ) ) ;
#29515 = ORIENTED_EDGE ( 'NONE', *, *, #3386, .F. ) ;
#29516 = FACE_OUTER_BOUND ( 'NONE', #5374, .T. ) ;
#29517 = CARTESIAN_POINT ( 'NONE',  ( 10.20488345035338185, -10.20488345035343336, 195.0000000000000284 ) ) ;
#29518 = CARTESIAN_POINT ( 'NONE',  ( 7.000000000000000000, -21.00000000000000000, -4.000000000000000000 ) ) ;
#29519 = VECTOR ( 'NONE', #33347, 1000.000000000000114 ) ;
#29520 = DIRECTION ( 'NONE',  ( -0.000000000000000000, -0.000000000000000000, 1.000000000000000000 ) ) ;
#29521 = DIRECTION ( 'NONE',  ( 0.000000000000000000, 0.7046037717862339012, 0.7096009616570518874 ) ) ;
#29522 = VERTEX_POINT ( 'NONE', #57854 ) ;
#29523 = DIRECTION ( 'NONE',  ( 4.121462285523435444E-16, 1.000000000000000000, 0.000000000000000000 ) ) ;
#29524 = DIRECTION ( 'NONE',  ( -0.000000000000000000, -0.000000000000000000, -1.000000000000000000 ) ) ;
#29525 = LINE ( 'NONE', #41179, #67265 ) ;
#29526 = DIRECTION ( 'NONE',  ( 0.000000000000000000, 1.000000000000000000, 0.000000000000000000 ) ) ;
#29527 = CARTESIAN_POINT ( 'NONE',  ( 3.606483450353369147, -7.428221114745098497, 455.0000000000000568 ) ) ;
#29528 = VERTEX_POINT ( 'NONE', #3420 ) ;
#29530 = ORIENTED_EDGE ( 'NONE', *, *, #16742, .T. ) ;
#29529 = DIRECTION ( 'NONE',  ( -1.000000000000000000, 0.000000000000000000, 0.000000000000000000 ) ) ;
#29531 = EDGE_CURVE ( 'NONE', #66948, #19393, #19325, .T. ) ;
#29532 = DIRECTION ( 'NONE',  ( -1.000000000000000000, 0.000000000000000000, 0.000000000000000000 ) ) ;
#29533 = FACE_OUTER_BOUND ( 'NONE', #50049, .T. ) ;
#29534 = VERTEX_POINT ( 'NONE', #30297 ) ;
#29535 = DIRECTION ( 'NONE',  ( 0.000000000000000000, 0.000000000000000000, -1.000000000000000000 ) ) ;
#29536 = VERTEX_POINT ( 'NONE', #30641 ) ;
#29537 = LINE ( 'NONE', #3998, #59412 ) ;
#29538 = ORIENTED_EDGE ( 'NONE', *, *, #45368, .F. ) ;
#29539 = VERTEX_POINT ( 'NONE', #8007 ) ;
#29540 = DIRECTION ( 'NONE',  ( 1.000000000000000000, 0.000000000000000000, 0.000000000000000000 ) ) ;
#29541 = EDGE_CURVE ( 'NONE', #24182, #51206, #62445, .T. ) ;
#29542 = EDGE_CURVE ( 'NONE', #61891, #15754, #62394, .T. ) ;
#29543 = VECTOR ( 'NONE', #38225, 1000.000000000000000 ) ;
#29544 = LINE ( 'NONE', #55387, #8307 ) ;
#29545 = LINE ( 'NONE', #51114, #7731 ) ;
#29546 = DIRECTION ( 'NONE',  ( -1.000000000000000000, 0.000000000000000000, 0.000000000000000000 ) ) ;
#29547 = PRESENTATION_LAYER_ASSIGNMENT (  '', '', ( #43086 ) ) ;
#29548 = EDGE_CURVE ( 'NONE', #3375, #62137, #61765, .T. ) ;
#29549 = ORIENTED_EDGE ( 'NONE', *, *, #61652, .T. ) ;
#29550 = EDGE_LOOP ( 'NONE', ( #66268, #14275, #16020, #61646 ) ) ;
#29551 = DIRECTION ( 'NONE',  ( 0.000000000000000000, 0.000000000000000000, 1.000000000000000000 ) ) ;
#29552 = DIRECTION ( 'NONE',  ( 0.000000000000000000, -1.000000000000000000, 0.000000000000000000 ) ) ;
#29553 = VERTEX_POINT ( 'NONE', #24988 ) ;
#29554 = ORIENTED_EDGE ( 'NONE', *, *, #25922, .F. ) ;
#29555 = VECTOR ( 'NONE', #56409, 1000.000000000000000 ) ;
#29556 = ORIENTED_EDGE ( 'NONE', *, *, #60975, .T. ) ;
#29557 = DIRECTION ( 'NONE',  ( -1.000000000000000000, 0.000000000000000000, 0.000000000000000000 ) ) ;
#29559 = ORIENTED_EDGE ( 'NONE', *, *, #33224, .F. ) ;
#29558 = FACE_OUTER_BOUND ( 'NONE', #15121, .T. ) ;
#29560 = PLANE ( 'NONE',  #36818 ) ;
#29561 = CARTESIAN_POINT ( 'NONE',  ( 2.706483450353343478, -10.92648345035346225, 455.0000000000000568 ) ) ;
#29562 = ORIENTED_EDGE ( 'NONE', *, *, #23954, .T. ) ;
#29563 = ORIENTED_EDGE ( 'NONE', *, *, #5490, .F. ) ;
#29564 = AXIS2_PLACEMENT_3D ( 'NONE', #42828, #20914, #59790 ) ;
#29565 = DIRECTION ( 'NONE',  ( -0.9375000000000006661, 0.000000000000000000, 0.3479852726768744020 ) ) ;
#29566 = DIRECTION ( 'NONE',  ( 0.000000000000000000, -1.000000000000000000, -0.000000000000000000 ) ) ;
#29567 = CARTESIAN_POINT ( 'NONE',  ( 10.62249899919925866, -21.00000000000000000, -17.50000000000000000 ) ) ;
#29568 = CARTESIAN_POINT ( 'NONE',  ( -8.130476262117259267, 9.547976262117177981, 26.00000000000000711 ) ) ;
#29569 = CARTESIAN_POINT ( 'NONE',  ( -7.250000000000000888, 8.250000000000001776, -20.50000000000000000 ) ) ;
#29571 = EDGE_LOOP ( 'NONE', ( #40795, #44761, #30264, #41459 ) ) ;
#29570 = DIRECTION ( 'NONE',  ( 1.836970198721029934E-16, 1.836970198721010706E-16, -1.000000000000000000 ) ) ;
#29572 = ORIENTED_EDGE ( 'NONE', *, *, #5347, .T. ) ;
#29573 = EDGE_CURVE ( 'NONE', #12180, #6660, #19665, .T. ) ;
#29574 = DIRECTION ( 'NONE',  ( -1.836970198721029934E-16, 1.836970198721036344E-16, -1.000000000000000000 ) ) ;
#29575 = FACE_OUTER_BOUND ( 'NONE', #48553, .T. ) ;
#29576 = EDGE_CURVE ( 'NONE', #54885, #34850, #25338, .T. ) ;
#29577 = EDGE_CURVE ( 'NONE', #43129, #7082, #2706, .T. ) ;
#29578 = CARTESIAN_POINT ( 'NONE',  ( 55.00000000000000000, -16.96999999999999886, 21.00000000000000000 ) ) ;
#29579 = CARTESIAN_POINT ( 'NONE',  ( -4.188533722949421723, -7.272650909786664286, 455.0000000000000568 ) ) ;
#29580 = CIRCLE ( 'NONE', #42018, 2.000000000000000000 ) ;
#29581 = ADVANCED_FACE ( 'NONE', ( #45487 ), #14385, .T. ) ;
#29582 = CARTESIAN_POINT ( 'NONE',  ( 181.4833316329832940, 0.000000000000000000, 328.5239988703752942 ) ) ;
#29583 = ORIENTED_EDGE ( 'NONE', *, *, #57339, .T. ) ;
#29584 = CARTESIAN_POINT ( 'NONE',  ( 10.50702373788280752, 6.835476262117182067, 54.00000000000000711 ) ) ;
#29585 = DIRECTION ( 'NONE',  ( 0.000000000000000000, 1.000000000000000000, 0.000000000000000000 ) ) ;
#29586 = AXIS2_PLACEMENT_3D ( 'NONE', #54736, #39158, #12959 ) ;
#29587 =( LENGTH_UNIT ( ) NAMED_UNIT ( * ) SI_UNIT ( .MILLI., .METRE. ) );
#29588 = CARTESIAN_POINT ( 'NONE',  ( -7.259684009079930611, 4.188533722949235205, 195.0000000000000284 ) ) ;
#29589 = LINE ( 'NONE', #23941, #6656 ) ;
#29590 = CARTESIAN_POINT ( 'NONE',  ( -2.993516549646791258, -7.428221114745081621, 455.0000000000000568 ) ) ;
#29591 = AXIS2_PLACEMENT_3D ( 'NONE', #46502, #62406, #2671 ) ;
#29592 = DIRECTION ( 'NONE',  ( -1.000000000000000000, 0.000000000000000000, 0.000000000000000000 ) ) ;
#29593 = EDGE_LOOP ( 'NONE', ( #38963, #69691, #69852, #55058 ) ) ;
#29594 = DIRECTION ( 'NONE',  ( 1.836970198721029934E-16, 1.836970198721010706E-16, -1.000000000000000000 ) ) ;
#29595 = DIRECTION ( 'NONE',  ( 0.000000000000000000, -5.800915303574361727E-12, 1.000000000000000000 ) ) ;
#29596 = ORIENTED_EDGE ( 'NONE', *, *, #7726, .F. ) ;
#29597 = CARTESIAN_POINT ( 'NONE',  ( 4.456444791733522252E-16, 7.450000000000002842, -20.00000000000000000 ) ) ;
#29598 = VECTOR ( 'NONE', #46849, 1000.000000000000000 ) ;
#29599 = DIRECTION ( 'NONE',  ( 0.000000000000000000, -1.000000000000000000, 0.000000000000000000 ) ) ;
#29600 = LINE ( 'NONE', #45873, #18592 ) ;
#29601 = LINE ( 'NONE', #50820, #21808 ) ;
#29602 = FACE_OUTER_BOUND ( 'NONE', #69767, .T. ) ;
#29603 = ORIENTED_EDGE ( 'NONE', *, *, #63437, .F. ) ;
#29604 = CARTESIAN_POINT ( 'NONE',  ( -7.450000000000001954, 0.000000000000000000, -11.50000000000000000 ) ) ;
#29605 = VECTOR ( 'NONE', #54759, 1000.000000000000000 ) ;
#29606 = ORIENTED_EDGE ( 'NONE', *, *, #24866, .F. ) ;
#29607 = CARTESIAN_POINT ( 'NONE',  ( 83.77321854994620765, 47.95351654967443977, 20.00000000000000000 ) ) ;
#29608 = ORIENTED_EDGE ( 'NONE', *, *, #66040, .F. ) ;
#29609 = CARTESIAN_POINT ( 'NONE',  ( 14.25000000000000000, -2.500000000000000000, 21.77831216351300014 ) ) ;
#29610 = AXIS2_PLACEMENT_3D ( 'NONE', #62549, #30743, #61867 ) ;
#29611 = ORIENTED_EDGE ( 'NONE', *, *, #22736, .T. ) ;
#29612 = PLANE ( 'NONE',  #67167 ) ;
#29613 = DIRECTION ( 'NONE',  ( -1.836970198721029934E-16, 1.836970198721036344E-16, -1.000000000000000000 ) ) ;
#29614 = ORIENTED_EDGE ( 'NONE', *, *, #29782, .F. ) ;
#29615 = ORIENTED_EDGE ( 'NONE', *, *, #32157, .T. ) ;
#29616 = LINE ( 'NONE', #36333, #66703 ) ;
#29617 = ORIENTED_EDGE ( 'NONE', *, *, #28371, .T. ) ;
#29618 = ORIENTED_EDGE ( 'NONE', *, *, #44879, .T. ) ;
#29619 = EDGE_CURVE ( 'NONE', #14148, #56608, #9423, .T. ) ;
#29620 = PRODUCT_DEFINITION_CONTEXT ( 'detailed design', #45367, 'design' ) ;
#29621 = CARTESIAN_POINT ( 'NONE',  ( -7.605476262117257136, 9.722976262117180468, 54.00000000000000711 ) ) ;
#29622 = CARTESIAN_POINT ( 'NONE',  ( -6.606374702650169795, 4.734785091273855606, 195.0000000000000284 ) ) ;
#29623 = LINE ( 'NONE', #61097, #27619 ) ;
#29624 = EDGE_CURVE ( 'NONE', #45669, #53184, #39821, .T. ) ;
#29625 = EDGE_CURVE ( 'NONE', #25422, #10709, #46894, .T. ) ;
#29626 = EDGE_LOOP ( 'NONE', ( #20442, #17740, #29482, #61537, #20205, #44885, #60233, #50309 ) ) ;
#29627 = DIRECTION ( 'NONE',  ( 1.836970198721029934E-16, 1.836970198721010706E-16, -1.000000000000000000 ) ) ;
#29629 = DIRECTION ( 'NONE',  ( -0.7071067811865475727, 0.000000000000000000, 0.7071067811865475727 ) ) ;
#29628 = LINE ( 'NONE', #23979, #62641 ) ;
#29630 = EDGE_LOOP ( 'NONE', ( #48185, #44945, #23948, #34927 ) ) ;
#29633 = VERTEX_POINT ( 'NONE', #8727 ) ;
#29632 = EDGE_CURVE ( 'NONE', #11295, #54217, #34874, .T. ) ;
#29631 = FACE_OUTER_BOUND ( 'NONE', #18567, .T. ) ;
#29634 = AXIS2_PLACEMENT_3D ( 'NONE', #44041, #5882, #33093 ) ;
#29635 = ORIENTED_EDGE ( 'NONE', *, *, #39732, .T. ) ;
#29636 = PRODUCT_DEFINITION ( 'UNKNOWN', '', #42640, #48782 ) ;
#29637 = SHAPE_DEFINITION_REPRESENTATION ( #67870, #4299 ) ;
#29638 = ADVANCED_FACE ( 'NONE', ( #30990 ), #66883, .F. ) ;
#29639 = LINE ( 'NONE', #45548, #69447 ) ;
#29640 = VECTOR ( 'NONE', #7227, 1000.000000000000000 ) ;
#29641 = ADVANCED_FACE ( 'NONE', ( #18621 ), #18980, .F. ) ;
#29642 = EDGE_LOOP ( 'NONE', ( #12466, #35189, #59695, #38591 ) ) ;
#29643 = CYLINDRICAL_SURFACE ( 'NONE', #13360, 4.500000000000189182 ) ;
#29644 = CARTESIAN_POINT ( 'NONE',  ( 0.000000000000000000, -7.449999999999998401, -8.500000000000000000 ) ) ;
#29645 = VERTEX_POINT ( 'NONE', #10127 ) ;
#29646 = ORIENTED_EDGE ( 'NONE', *, *, #59378, .T. ) ;
#29647 = CARTESIAN_POINT ( 'NONE',  ( -9.547976262117256141, 7.955476262117183062, 54.00000000000000711 ) ) ;
#29648 = FACE_OUTER_BOUND ( 'NONE', #27313, .T. ) ;
#29649 = ORIENTED_EDGE ( 'NONE', *, *, #41935, .T. ) ;
#29650 = CARTESIAN_POINT ( 'NONE',  ( 6.006483450353379716, -6.006483450353394815, 195.0000000000000284 ) ) ;
#29651 = DIRECTION ( 'NONE',  ( 0.000000000000000000, -1.000000000000000000, 0.000000000000000000 ) ) ;
#29652 = FACE_OUTER_BOUND ( 'NONE', #6414, .T. ) ;
#29653 = VERTEX_POINT ( 'NONE', #52932 ) ;
#29654 = AXIS2_PLACEMENT_3D ( 'NONE', #21379, #48261, #33029 ) ;
#29655 = DIRECTION ( 'NONE',  ( 1.000000000000000000, 0.000000000000000000, 0.000000000000000000 ) ) ;
#29656 = FACE_OUTER_BOUND ( 'NONE', #16152, .T. ) ;
#29658 = ORIENTED_EDGE ( 'NONE', *, *, #66621, .F. ) ;
#29657 =( NAMED_UNIT ( * ) SI_UNIT ( $, .STERADIAN. ) SOLID_ANGLE_UNIT ( ) );
#29660 = ORIENTED_EDGE ( 'NONE', *, *, #41775, .T. ) ;
#29659 = CARTESIAN_POINT ( 'NONE',  ( 78.77321854994620765, 47.95351654967443977, 39.00000000000000000 ) ) ;
#29662 = CARTESIAN_POINT ( 'NONE',  ( -8.566576262117358453, -9.703773737882738004, 54.00000000000000711 ) ) ;
#29661 = VECTOR ( 'NONE', #3008, 1000.000000000000000 ) ;
#29663 = AXIS2_PLACEMENT_3D ( 'NONE', #63682, #15238, #24792 ) ;
#29664 = CARTESIAN_POINT ( 'NONE',  ( 8.250000000000005329, 7.250000000000000888, -26.00000000000001066 ) ) ;
#29665 = CARTESIAN_POINT ( 'NONE',  ( -11.75000000000000000, -5.000000000000000000, -21.10805890929250950 ) ) ;
#29666 = PLANE ( 'NONE',  #3435 ) ;
#29667 = VECTOR ( 'NONE', #26835, 1000.000000000000000 ) ;
#29668 = DIRECTION ( 'NONE',  ( -0.000000000000000000, 0.000000000000000000, 1.000000000000000000 ) ) ;
#29669 = ORIENTED_EDGE ( 'NONE', *, *, #56076, .T. ) ;
#29670 = CARTESIAN_POINT ( 'NONE',  ( 275.0000000000000000, -37.14999999999894698, 8.200000000002349410 ) ) ;
#29671 = LINE ( 'NONE', #19420, #24776 ) ;
#29672 = CARTESIAN_POINT ( 'NONE',  ( 289.4999999999998863, -42.00000000000004263, 26.99999999999991829 ) ) ;
#29674 = VERTEX_POINT ( 'NONE', #31368 ) ;
#29673 = CARTESIAN_POINT ( 'NONE',  ( 7.000000000000000000, -39.79999999999954952, 8.900000000000419575 ) ) ;
#29675 = LINE ( 'NONE', #50895, #54963 ) ;
#29676 = VECTOR ( 'NONE', #4977, 1000.000000000000114 ) ;
#29677 = CARTESIAN_POINT ( 'NONE',  ( -11.00000000000000000, -12.00000000000000000, 10.52786404500095863 ) ) ;
#29678 = ORIENTED_EDGE ( 'NONE', *, *, #8467, .T. ) ;
#29679 = EDGE_CURVE ( 'NONE', #22100, #64136, #32397, .T. ) ;
#29680 = EDGE_LOOP ( 'NONE', ( #23981, #48712, #3023, #3954 ) ) ;
#29681 = CARTESIAN_POINT ( 'NONE',  ( 49.00000000000000000, -0.7500000000000000000, 4.943429983321300014 ) ) ;
#29682 = CARTESIAN_POINT ( 'NONE',  ( 7.000000000000000000, -21.00000000000000000, 0.000000000000000000 ) ) ;
#29683 = AXIS2_PLACEMENT_3D ( 'NONE', #51796, #15372, #3353 ) ;
#29684 = VERTEX_POINT ( 'NONE', #27079 ) ;
#29685 = LINE ( 'NONE', #25448, #1855 ) ;
#29686 = DIRECTION ( 'NONE',  ( -1.000000000000000000, 0.000000000000000000, 0.000000000000000000 ) ) ;
#29687 = ADVANCED_FACE ( 'NONE', ( #4481 ), #58576, .T. ) ;
#29688 = AXIS2_PLACEMENT_3D ( 'NONE', #55569, #7111, #12755 ) ;
#29689 = DIRECTION ( 'NONE',  ( -1.000000000000000000, 0.000000000000000000, 0.000000000000000000 ) ) ;
#29690 = CARTESIAN_POINT ( 'NONE',  ( 7.250000000000005329, -7.449999999999998401, -16.50000000000000000 ) ) ;
#29691 = VERTEX_POINT ( 'NONE', #15777 ) ;
#29692 = DIRECTION ( 'NONE',  ( 1.000000000000000000, -1.671920889371702854E-15, 0.000000000000000000 ) ) ;
#29693 = VERTEX_POINT ( 'NONE', #53276 ) ;
#29694 = EDGE_CURVE ( 'NONE', #38093, #20252, #69521, .T. ) ;
#29695 = ORIENTED_EDGE ( 'NONE', *, *, #41483, .T. ) ;
#29696 = AXIS2_PLACEMENT_3D ( 'NONE', #67828, #62498, #46594 ) ;
#29697 = CARTESIAN_POINT ( 'NONE',  ( -11.00000000000000000, -12.00000000000000000, 12.20000000000000107 ) ) ;
#29698 = EDGE_CURVE ( 'NONE', #65774, #26484, #48853, .T. ) ;
#29699 = DIRECTION ( 'NONE',  ( 0.000000000000000000, -0.7071067811865496822, 0.7071067811865454633 ) ) ;
#29700 = DIRECTION ( 'NONE',  ( -1.000000000000000000, 3.491481338843133355E-15, 1.836970198721036344E-16 ) ) ;
#29701 = ORIENTED_EDGE ( 'NONE', *, *, #16406, .T. ) ;
#29702 = ORIENTED_EDGE ( 'NONE', *, *, #19313, .F. ) ;
#29703 = FACE_OUTER_BOUND ( 'NONE', #31665, .T. ) ;
#29704 = ORIENTED_EDGE ( 'NONE', *, *, #44932, .T. ) ;
#29705 = EDGE_LOOP ( 'NONE', ( #45099, #13562, #45800, #63934 ) ) ;
#29706 = CARTESIAN_POINT ( 'NONE',  ( -8.250000000000001776, -7.249999999999998224, -14.00000000000000000 ) ) ;
#29707 = CARTESIAN_POINT ( 'NONE',  ( -9.690000000000001279, -8.750000000000000000, -5.000000000000000000 ) ) ;
#29708 = VECTOR ( 'NONE', #31571, 1000.000000000000000 ) ;
#29709 = CARTESIAN_POINT ( 'NONE',  ( 6.619341603356837744, -4.747751991980742936, 455.0000000000000568 ) ) ;
#29710 = EDGE_CURVE ( 'NONE', #46512, #31832, #33040, .T. ) ;
#29711 = CARTESIAN_POINT ( 'NONE',  ( 11.00000000000000000, -12.00000000000000000, -12.20000000000000107 ) ) ;
#29712 = ORIENTED_EDGE ( 'NONE', *, *, #63293, .F. ) ;
#29713 = VECTOR ( 'NONE', #41352, 1000.000000000000000 ) ;
#29714 = DIRECTION ( 'NONE',  ( 1.000000000000000000, 0.000000000000000000, 0.000000000000000000 ) ) ;
#29716 = CARTESIAN_POINT ( 'NONE',  ( -11.00000000000000000, -10.85999999999999943, 9.350000000000269651 ) ) ;
#29715 = CARTESIAN_POINT ( 'NONE',  ( 30.00000000000000000, -14.04000000000000092, -17.04524521594300523 ) ) ;
#29717 = AXIS2_PLACEMENT_3D ( 'NONE', #32753, #33450, #65297 ) ;
#29719 = EDGE_LOOP ( 'NONE', ( #24629, #56613, #53750, #4329 ) ) ;
#29718 = CIRCLE ( 'NONE', #24119, 0.5000000000009302559 ) ;
#29721 = EDGE_LOOP ( 'NONE', ( #8873, #5568, #56481, #64153 ) ) ;
#29720 = CARTESIAN_POINT ( 'NONE',  ( 17.00000000000000000, -15.50000000000000000, 2.000000000000000000 ) ) ;
#29722 = VERTEX_POINT ( 'NONE', #26048 ) ;
#29723 = EDGE_LOOP ( 'NONE', ( #59577, #34339, #52443, #12194 ) ) ;
#29724 = CIRCLE ( 'NONE', #38764, 0.5999999999999998668 ) ;
#29725 = AXIS2_PLACEMENT_3D ( 'NONE', #932, #15779, #16126 ) ;
#29726 = ADVANCED_FACE ( 'NONE', ( #42990 ), #59258, .T. ) ;
#29727 = CARTESIAN_POINT ( 'NONE',  ( -29.50000000000000355, -11.50000000000100009, 15.00000000000084910 ) ) ;
#29728 = EDGE_CURVE ( 'NONE', #21380, #67902, #47953, .T. ) ;
#29729 = CARTESIAN_POINT ( 'NONE',  ( 31.89999999999999858, 13.66939075806899240, -20.79999999999999361 ) ) ;
#29730 = ORIENTED_EDGE ( 'NONE', *, *, #32991, .T. ) ;
#29731 = VERTEX_POINT ( 'NONE', #42647 ) ;
#29732 = LINE ( 'NONE', #29381, #21861 ) ;
#29733 = FACE_OUTER_BOUND ( 'NONE', #54956, .T. ) ;
#29734 = VECTOR ( 'NONE', #19009, 1000.000000000000000 ) ;
#29735 = ADVANCED_FACE ( 'NONE', ( #37353 ), #36642, .F. ) ;
#29736 = ORIENTED_EDGE ( 'NONE', *, *, #33545, .F. ) ;
#29737 = VERTEX_POINT ( 'NONE', #58916 ) ;
#29738 = CARTESIAN_POINT ( 'NONE',  ( 7.806483450353379538, -11.12648345035348996, 455.0000000000000568 ) ) ;
#29739 = CARTESIAN_POINT ( 'NONE',  ( 24.00000000000000000, -17.50000000000000000, -15.70500000000000007 ) ) ;
#29740 = ORIENTED_EDGE ( 'NONE', *, *, #17921, .T. ) ;
#29741 = CARTESIAN_POINT ( 'NONE',  ( 11.50000000000000000, -12.00000000000000000, 11.03137303340310282 ) ) ;
#29742 = CARTESIAN_POINT ( 'NONE',  ( -11.00000000000000000, -15.97213595500069871, 14.50000000000000000 ) ) ;
#29744 = EDGE_LOOP ( 'NONE', ( #23398, #33289, #50414, #50385, #2403, #4684, #57665, #15543, #27206, #65318, #21907, #37135 ) ) ;
#29743 = CARTESIAN_POINT ( 'NONE',  ( 9.804883450353379715, -10.20488345035352928, 455.0000000000000568 ) ) ;
#29745 = EDGE_LOOP ( 'NONE', ( #51838, #21972, #85, #63974 ) ) ;
#29746 = DIRECTION ( 'NONE',  ( 1.156482317317870187E-14, 1.000000000000000000, 0.000000000000000000 ) ) ;
#29747 = DIRECTION ( 'NONE',  ( -1.000000000000000000, 0.000000000000000000, 0.000000000000000000 ) ) ;
#29748 = FACE_OUTER_BOUND ( 'NONE', #40141, .T. ) ;
#29749 = CARTESIAN_POINT ( 'NONE',  ( 0.000000000000000000, 20.50000000000000000, 17.79289321881345032 ) ) ;
#29750 = DIRECTION ( 'NONE',  ( 0.5773502691896216232, 0.5773502691896359451, 0.5773502691896197359 ) ) ;
#29751 = EDGE_CURVE ( 'NONE', #37106, #47930, #64229, .T. ) ;
#29752 = CARTESIAN_POINT ( 'NONE',  ( 7.450000000000006395, 7.250000000000000888, -10.50000000000000000 ) ) ;
#29753 = DIRECTION ( 'NONE',  ( 0.000000000000000000, 0.000000000000000000, -1.000000000000000000 ) ) ;
#29754 = ORIENTED_EDGE ( 'NONE', *, *, #42258, .F. ) ;
#29755 = DIRECTION ( 'NONE',  ( 0.000000000000000000, 0.000000000000000000, -1.000000000000000000 ) ) ;
#29756 = EDGE_CURVE ( 'NONE', #29819, #26009, #51098, .T. ) ;
#29758 = ORIENTED_EDGE ( 'NONE', *, *, #61674, .F. ) ;
#29757 = CARTESIAN_POINT ( 'NONE',  ( 26.90000000000000213, -0.1999999999911430404, -8.864436962241481021E-12 ) ) ;
#29759 = CARTESIAN_POINT ( 'NONE',  ( -11.50000000000000000, -12.00000000000000000, -11.00000000000000000 ) ) ;
#29760 = AXIS2_PLACEMENT_3D ( 'NONE', #37888, #11680, #32587 ) ;
#29761 = VECTOR ( 'NONE', #63127, 1000.000000000000000 ) ;
#29762 = DIRECTION ( 'NONE',  ( -1.000000000000000000, 0.000000000000000000, 0.000000000000000000 ) ) ;
#29764 = EDGE_CURVE ( 'NONE', #54988, #19639, #20726, .T. ) ;
#29763 = DIRECTION ( 'NONE',  ( 0.000000000000000000, 0.000000000000000000, 1.000000000000000000 ) ) ;
#29765 = DIRECTION ( 'NONE',  ( 0.000000000000000000, 1.000000000000000000, 0.000000000000000000 ) ) ;
#29766 = CARTESIAN_POINT ( 'NONE',  ( 2.664535259100375697E-15, 20.50000000000000355, 17.79289321881343611 ) ) ;
#29767 = AXIS2_PLACEMENT_3D ( 'NONE', #16819, #38382, #11490 ) ;
#29768 = ADVANCED_FACE ( 'NONE', ( #15081 ), #48651, .T. ) ;
#29769 = EDGE_LOOP ( 'NONE', ( #44464, #56290, #12024, #55207 ) ) ;
#29770 = CARTESIAN_POINT ( 'NONE',  ( 11.18999999999999950, -11.18999999999999950, -4.250000000000000000 ) ) ;
#29771 = VERTEX_POINT ( 'NONE', #48309 ) ;
#29772 = VECTOR ( 'NONE', #52431, 1000.000000000000000 ) ;
#29773 = FACE_OUTER_BOUND ( 'NONE', #16287, .T. ) ;
#29774 = VECTOR ( 'NONE', #16024, 1000.000000000000000 ) ;
#29775 = ADVANCED_FACE ( 'NONE', ( #69865 ), #53968, .F. ) ;
#29776 = LINE ( 'NONE', #2913, #39801 ) ;
#29777 = ORIENTED_EDGE ( 'NONE', *, *, #34416, .T. ) ;
#29778 = DIRECTION ( 'NONE',  ( 1.836970198721029934E-16, 1.836970198721010706E-16, -1.000000000000000000 ) ) ;
#29779 = VERTEX_POINT ( 'NONE', #5522 ) ;
#29780 = ADVANCED_FACE ( 'NONE', ( #16478 ), #11158, .F. ) ;
#29781 = ORIENTED_EDGE ( 'NONE', *, *, #17259, .F. ) ;
#29782 = EDGE_CURVE ( 'NONE', #24541, #24415, #16129, .T. ) ;
#29783 = CARTESIAN_POINT ( 'NONE',  ( 11.00000000000000000, -8.959999999999999076, -17.04524521594300523 ) ) ;
#29784 = CARTESIAN_POINT ( 'NONE',  ( -11.33351654964668676, -1.090483450353329165, 455.0000000000000568 ) ) ;
#29785 = EDGE_LOOP ( 'NONE', ( #30680, #34360, #28296, #10702, #47180, #23482 ) ) ;
#29786 = CARTESIAN_POINT ( 'NONE',  ( 25.57999999999999829, 0.000000000000000000, 0.000000000000000000 ) ) ;
#29787 = EDGE_CURVE ( 'NONE', #58661, #25681, #50023, .T. ) ;
#29788 = ADVANCED_FACE ( 'NONE', ( #28123, #44361, #43694, #61319, #34442 ), #11841, .F. ) ;
#29789 = ADVANCED_FACE ( 'NONE', ( #39755 ), #5867, .F. ) ;
#29790 = CARTESIAN_POINT ( 'NONE',  ( -4.242044687070659847, -8.465062094116134972, 455.0000000000000568 ) ) ;
#29791 = LINE ( 'NONE', #17796, #56567 ) ;
#29792 = VERTEX_POINT ( 'NONE', #49002 ) ;
#29793 = ORIENTED_EDGE ( 'NONE', *, *, #50771, .T. ) ;
#29795 = VERTEX_POINT ( 'NONE', #66636 ) ;
#29794 = LINE ( 'NONE', #60920, #69049 ) ;
#29796 = EDGE_CURVE ( 'NONE', #245, #26524, #22128, .T. ) ;
#29797 = ORIENTED_EDGE ( 'NONE', *, *, #51092, .F. ) ;
#29798 = CARTESIAN_POINT ( 'NONE',  ( 8.900000000000005684, 21.00000000000000000, 13.98999642601811999 ) ) ;
#29799 = CARTESIAN_POINT ( 'NONE',  ( -11.07551654964681731, -9.804883450353372609, 455.0000000000000568 ) ) ;
#29800 = CARTESIAN_POINT ( 'NONE',  ( 16.89999999999999858, -0.2000000000089119934, 8.909539772616881237E-12 ) ) ;
#29801 = LINE ( 'NONE', #8932, #62410 ) ;
#29802 = AXIS2_PLACEMENT_3D ( 'NONE', #64851, #64168, #42577 ) ;
#29803 = CARTESIAN_POINT ( 'NONE',  ( -5.242976262117259978, 5.242976262117182706, 26.00000000000000711 ) ) ;
#29804 = CARTESIAN_POINT ( 'NONE',  ( -11.00000000000000000, -9.200000000000120082, 17.30000000000000071 ) ) ;
#29805 = ORIENTED_EDGE ( 'NONE', *, *, #879, .T. ) ;
#29806 = CIRCLE ( 'NONE', #65935, 0.5000000000000000000 ) ;
#29807 = ORIENTED_EDGE ( 'NONE', *, *, #17552, .F. ) ;
#29808 = ORIENTED_EDGE ( 'NONE', *, *, #13275, .F. ) ;
#29809 = ORIENTED_EDGE ( 'NONE', *, *, #31690, .F. ) ;
#29810 = LINE ( 'NONE', #19549, #22023 ) ;
#29811 = EDGE_CURVE ( 'NONE', #50286, #20807, #1254, .T. ) ;
#29812 = PLANE ( 'NONE',  #29815 ) ;
#29813 = ADVANCED_FACE ( 'NONE', ( #23152 ), #44711, .T. ) ;
#29814 = VECTOR ( 'NONE', #20136, 1000.000000000000000 ) ;
#29816 = CARTESIAN_POINT ( 'NONE',  ( 7.826483450353421745, 11.99351654964657499, 455.0000000000000568 ) ) ;
#29815 = AXIS2_PLACEMENT_3D ( 'NONE', #63403, #53161, #68715 ) ;
#29817 = VERTEX_POINT ( 'NONE', #22483 ) ;
#29818 = ORIENTED_EDGE ( 'NONE', *, *, #21992, .T. ) ;
#29819 = VERTEX_POINT ( 'NONE', #59945 ) ;
#29820 = LINE ( 'NONE', #60945, #47510 ) ;
#29821 = ORIENTED_EDGE ( 'NONE', *, *, #7910, .T. ) ;
#29822 = AXIS2_PLACEMENT_3D ( 'NONE', #52047, #62637, #24820 ) ;
#29823 = ORIENTED_EDGE ( 'NONE', *, *, #30706, .T. ) ;
#29824 = DIRECTION ( 'NONE',  ( 0.000000000000000000, 0.7071067811865495711, -0.7071067811865455743 ) ) ;
#29825 = ORIENTED_EDGE ( 'NONE', *, *, #61458, .F. ) ;
#29826 = VERTEX_POINT ( 'NONE', #22814 ) ;
#29827 = DIRECTION ( 'NONE',  ( 0.000000000000000000, -1.000000000000000000, 0.000000000000000000 ) ) ;
#29828 = CIRCLE ( 'NONE', #63721, 2.250000000000001776 ) ;
#29830 = ORIENTED_EDGE ( 'NONE', *, *, #12216, .F. ) ;
#29829 = LINE ( 'NONE', #55659, #26599 ) ;
#29831 = ORIENTED_EDGE ( 'NONE', *, *, #987, .T. ) ;
#29832 = CARTESIAN_POINT ( 'NONE',  ( -8.250000000000001776, 0.000000000000000000, -19.00000000000000000 ) ) ;
#29833 = DIRECTION ( 'NONE',  ( -1.836970198721029934E-16, 1.836970198721036344E-16, -1.000000000000000000 ) ) ;
#29834 = AXIS2_PLACEMENT_3D ( 'NONE', #44108, #60360, #44789 ) ;
#29835 = PLANE ( 'NONE',  #66204 ) ;
#29837 = ORIENTED_EDGE ( 'NONE', *, *, #13894, .F. ) ;
#29836 = CARTESIAN_POINT ( 'NONE',  ( -5.993516549646728642, -6.006483450353378828, 195.0000000000000284 ) ) ;
#29838 = AXIS2_PLACEMENT_3D ( 'NONE', #13107, #50598, #55898 ) ;
#29839 = ORIENTED_EDGE ( 'NONE', *, *, #57743, .F. ) ;
#29840 = DIRECTION ( 'NONE',  ( -0.000000000000000000, -0.000000000000000000, 1.000000000000000000 ) ) ;
#29841 = LINE ( 'NONE', #45049, #51477 ) ;
#29842 = CARTESIAN_POINT ( 'NONE',  ( -2.500000000000000000, 0.000000000000000000, -30.00000000000001066 ) ) ;
#29843 = EDGE_LOOP ( 'NONE', ( #8447, #39323, #39667, #69223, #35440, #1516, #12313, #68855 ) ) ;
#29844 = DIRECTION ( 'NONE',  ( 0.000000000000000000, -1.000000000000000000, -3.673940397442059868E-16 ) ) ;
#29845 = EDGE_CURVE ( 'NONE', #29817, #50067, #65933, .T. ) ;
#29846 = CARTESIAN_POINT ( 'NONE',  ( -9.750000000000001776, 9.690000000000001279, -4.250000000000000000 ) ) ;
#29847 = LINE ( 'NONE', #51420, #15388 ) ;
#29848 = VERTEX_POINT ( 'NONE', #60641 ) ;
#29849 = VECTOR ( 'NONE', #25110, 1000.000000000000000 ) ;
#29851 = EDGE_CURVE ( 'NONE', #61234, #18742, #12192, .T. ) ;
#29850 = PLANE ( 'NONE',  #49423 ) ;
#29852 = DIRECTION ( 'NONE',  ( 0.000000000000000000, 1.000000000000000000, 0.000000000000000000 ) ) ;
#29853 = CARTESIAN_POINT ( 'NONE',  ( -7.603567055985545942, 8.393516549646601987, 455.0000000000000568 ) ) ;
#29854 = DIRECTION ( 'NONE',  ( 1.836970198721029934E-16, 1.836970198721010706E-16, -1.000000000000000000 ) ) ;
#29855 = ADVANCED_FACE ( 'NONE', ( #17504 ), #39073, .F. ) ;
#29856 = AXIS2_PLACEMENT_3D ( 'NONE', #63428, #20629, #20981 ) ;
#29857 = ORIENTED_EDGE ( 'NONE', *, *, #60280, .T. ) ;
#29858 =( LENGTH_UNIT ( ) NAMED_UNIT ( * ) SI_UNIT ( .MILLI., .METRE. ) );
#29859 = ADVANCED_FACE ( 'NONE', ( #50376 ), #6210, .F. ) ;
#29860 = DIRECTION ( 'NONE',  ( 0.000000000000000000, 0.000000000000000000, 1.000000000000000000 ) ) ;
#29861 = VECTOR ( 'NONE', #29169, 1000.000000000000000 ) ;
#29862 = VECTOR ( 'NONE', #33979, 1000.000000000000000 ) ;
#29863 = EDGE_LOOP ( 'NONE', ( #53760, #478, #58173, #58731, #20988, #54093 ) ) ;
#29864 = CARTESIAN_POINT ( 'NONE',  ( 11.18999999999999950, -11.18999999999999950, -5.000000000000000000 ) ) ;
#29865 = PLANE ( 'NONE',  #68165 ) ;
#29866 = CARTESIAN_POINT ( 'NONE',  ( 9.306483450353379538, -10.92648345035339119, 195.0000000000000284 ) ) ;
#29867 = LINE ( 'NONE', #46132, #7548 ) ;
#29868 = DIRECTION ( 'NONE',  ( -1.000000000000000000, 0.000000000000000000, 0.000000000000000000 ) ) ;
#29869 = VECTOR ( 'NONE', #64429, 1000.000000000000000 ) ;
#29870 = VERTEX_POINT ( 'NONE', #65604 ) ;
#29871 = CIRCLE ( 'NONE', #5058, 0.2000000000000005107 ) ;
#29872 = CARTESIAN_POINT ( 'NONE',  ( 7.250000000000004441, 7.450000000000001954, -24.00000000000000000 ) ) ;
#29873 = DIRECTION ( 'NONE',  ( 0.000000000000000000, 0.000000000000000000, 1.000000000000000000 ) ) ;
#29874 = CARTESIAN_POINT ( 'NONE',  ( 4.456444791733522252E-16, 7.450000000000002842, -17.50000000000000000 ) ) ;
#29875 = EDGE_CURVE ( 'NONE', #42019, #15647, #55683, .T. ) ;
#29876 = CIRCLE ( 'NONE', #46836, 2.000000000000000000 ) ;
#29877 = DIRECTION ( 'NONE',  ( 1.000000000000000000, 1.301042606982605321E-16, 0.000000000000000000 ) ) ;
#29878 = DIRECTION ( 'NONE',  ( -1.000000000000000000, 3.491481338843133355E-15, 1.836970198721036344E-16 ) ) ;
#29879 = ORIENTED_EDGE ( 'NONE', *, *, #35478, .F. ) ;
#29881 = ORIENTED_EDGE ( 'NONE', *, *, #46867, .T. ) ;
#29880 = CARTESIAN_POINT ( 'NONE',  ( 0.000000000000000000, 8.250000000000001776, -22.00000000000000000 ) ) ;
#29882 = STYLED_ITEM ( 'NONE', ( #47346 ), #43959 ) ;
#29883 = LINE ( 'NONE', #55711, #49644 ) ;
#29884 = DIRECTION ( 'NONE',  ( -1.000000000000000000, 0.000000000000000000, 0.000000000000000000 ) ) ;
#29885 = ORIENTED_EDGE ( 'NONE', *, *, #40798, .F. ) ;
#29886 = AXIS2_PLACEMENT_3D ( 'NONE', #55136, #17634, #56172 ) ;
#29887 = DIRECTION ( 'NONE',  ( 1.000000000000000000, -0.000000000000000000, -0.000000000000000000 ) ) ;
#29888 = ORIENTED_EDGE ( 'NONE', *, *, #38200, .T. ) ;
#29889 = VERTEX_POINT ( 'NONE', #28453 ) ;
#29890 = VERTEX_POINT ( 'NONE', #23507 ) ;
#29891 = CARTESIAN_POINT ( 'NONE',  ( 277.3542486889354564, -25.50000000000000355, -17.00000000000000000 ) ) ;
#29892 = ADVANCED_FACE ( 'NONE', ( #49355 ), #38723, .T. ) ;
#29893 = DIRECTION ( 'NONE',  ( -0.7671651518153105309, 0.6414496315691445849, 0.000000000000000000 ) ) ;
#29894 = DIRECTION ( 'NONE',  ( -4.956352788505168198E-15, -1.000000000000000000, 0.000000000000000000 ) ) ;
#29896 = ADVANCED_FACE ( 'NONE', ( #36476 ), #4327, .F. ) ;
#29895 = CARTESIAN_POINT ( 'NONE',  ( -4.727349090213463612, 7.798499376343949407, 195.0000000000000284 ) ) ;
#29897 = ORIENTED_EDGE ( 'NONE', *, *, #3537, .T. ) ;
#29898 = AXIS2_PLACEMENT_3D ( 'NONE', #49115, #22929, #23275 ) ;
#29900 = EDGE_CURVE ( 'NONE', #66278, #46124, #35147, .T. ) ;
#29899 = ORIENTED_EDGE ( 'NONE', *, *, #5356, .T. ) ;
#29901 = DIRECTION ( 'NONE',  ( 1.000000000000000000, 0.000000000000000000, 0.000000000000000000 ) ) ;
#29902 = CARTESIAN_POINT ( 'NONE',  ( 49.00000000000000000, -0.1999999999911795112, 8.826273045769999343E-12 ) ) ;
#29903 = ORIENTED_EDGE ( 'NONE', *, *, #12770, .T. ) ;
#29904 = AXIS2_PLACEMENT_3D ( 'NONE', #64857, #37639, #32672 ) ;
#29905 = ORIENTED_EDGE ( 'NONE', *, *, #37699, .T. ) ;
#29906 = ORIENTED_EDGE ( 'NONE', *, *, #47501, .F. ) ;
#29907 = CARTESIAN_POINT ( 'NONE',  ( 41.09999999999999432, -21.00000000000000000, 13.86939075806900057 ) ) ;
#29909 = VERTEX_POINT ( 'NONE', #69005 ) ;
#29908 = LINE ( 'NONE', #51127, #13442 ) ;
#29910 = CARTESIAN_POINT ( 'NONE',  ( 7.250000000000005329, -7.449999999999998401, -15.50000000000000000 ) ) ;
#29911 = VECTOR ( 'NONE', #42825, 1000.000000000000000 ) ;
#29912 = AXIS2_PLACEMENT_3D ( 'NONE', #62163, #57917, #13729 ) ;
#29913 = CARTESIAN_POINT ( 'NONE',  ( 7.250000000000005329, 7.250000000000000888, -20.00000000000000000 ) ) ;
#29914 = VECTOR ( 'NONE', #20172, 999.9999999999998863 ) ;
#29915 = ORIENTED_EDGE ( 'NONE', *, *, #28994, .F. ) ;
#29916 = ORIENTED_EDGE ( 'NONE', *, *, #10705, .F. ) ;
#29917 = CIRCLE ( 'NONE', #69456, 0.2000000000000005107 ) ;
#29918 = LINE ( 'NONE', #51498, #33755 ) ;
#29919 = DIRECTION ( 'NONE',  ( -1.836970198721029934E-16, 1.836970198721036344E-16, -1.000000000000000000 ) ) ;
#29920 = VECTOR ( 'NONE', #33308, 1000.000000000000000 ) ;
#29921 = DIRECTION ( 'NONE',  ( 1.000000000000000000, 0.000000000000000000, 0.000000000000000000 ) ) ;
#29922 = ADVANCED_FACE ( 'NONE', ( #2289, #47094 ), #40101, .T. ) ;
#29923 = AXIS2_PLACEMENT_3D ( 'NONE', #9796, #46900, #14740 ) ;
#29924 = DIRECTION ( 'NONE',  ( 0.000000000000000000, 1.000000000000000000, 0.000000000000000000 ) ) ;
#29925 = DIRECTION ( 'NONE',  ( 1.000000000000000000, -0.000000000000000000, 0.000000000000000000 ) ) ;
#29927 = ORIENTED_EDGE ( 'NONE', *, *, #34944, .F. ) ;
#29926 = FILL_AREA_STYLE ('',( #14726 ) ) ;
#29928 = VERTEX_POINT ( 'NONE', #29504 ) ;
#29929 = PLANE ( 'NONE',  #5017 ) ;
#29930 = CARTESIAN_POINT ( 'NONE',  ( 7.500000000000000000, -20.40000000000000213, -16.00000000000000000 ) ) ;
#29931 = LINE ( 'NONE', #35220, #49981 ) ;
#29932 = CARTESIAN_POINT ( 'NONE',  ( 181.4833316329832940, 9.000000000000001776, 328.5239988703752942 ) ) ;
#29933 = EDGE_CURVE ( 'NONE', #18545, #33868, #41776, .T. ) ;
#29934 = EDGE_CURVE ( 'NONE', #1047, #34676, #8239, .T. ) ;
#29935 = LINE ( 'NONE', #69174, #47804 ) ;
#29937 = VERTEX_POINT ( 'NONE', #18904 ) ;
#29936 = EDGE_CURVE ( 'NONE', #69235, #190, #14918, .T. ) ;
#29938 = DIRECTION ( 'NONE',  ( 0.000000000000000000, 0.000000000000000000, 1.000000000000000000 ) ) ;
#29939 = EDGE_CURVE ( 'NONE', #21386, #34404, #11615, .T. ) ;
#29940 = FACE_BOUND ( 'NONE', #7334, .T. ) ;
#29941 = FACE_OUTER_BOUND ( 'NONE', #46764, .T. ) ;
#29942 = LINE ( 'NONE', #56809, #31152 ) ;
#29943 = EDGE_CURVE ( 'NONE', #30449, #11172, #56729, .T. ) ;
#29944 = DIRECTION ( 'NONE',  ( 0.000000000000000000, 0.000000000000000000, 1.000000000000000000 ) ) ;
#29945 = CARTESIAN_POINT ( 'NONE',  ( 283.0000000000000568, -38.15000000000000568, -14.50000000000000000 ) ) ;
#29946 = CARTESIAN_POINT ( 'NONE',  ( 8.406483450353379183, -6.344579767990839336, 195.0000000000000284 ) ) ;
#29947 = EDGE_LOOP ( 'NONE', ( #55432, #62337, #294, #18659 ) ) ;
#29948 = DIRECTION ( 'NONE',  ( -0.000000000000000000, -0.000000000000000000, -1.000000000000000000 ) ) ;
#29949 = CARTESIAN_POINT ( 'NONE',  ( -10.19191654964682137, -11.48848345035329821, 195.0000000000000284 ) ) ;
#29950 = VECTOR ( 'NONE', #45694, 1000.000000000000000 ) ;
#29951 = ORIENTED_EDGE ( 'NONE', *, *, #54297, .F. ) ;
#29952 = CARTESIAN_POINT ( 'NONE',  ( 280.0000000000000000, -20.40000000000000213, -20.00000000000000000 ) ) ;
#29953 = DIRECTION ( 'NONE',  ( -1.062171939662868407E-14, -1.000000000000000000, 0.000000000000000000 ) ) ;
#29954 = CARTESIAN_POINT ( 'NONE',  ( -9.942044687070568543, 9.234937905883914055, 455.0000000000000568 ) ) ;
#29955 = AXIS2_PLACEMENT_3D ( 'NONE', #8744, #30315, #45511 ) ;
#29956 = DIRECTION ( 'NONE',  ( 0.000000000000000000, 0.000000000000000000, -1.000000000000000000 ) ) ;
#29957 = DIRECTION ( 'NONE',  ( 0.000000000000000000, 1.000000000000000000, 0.000000000000000000 ) ) ;
#29958 = VERTEX_POINT ( 'NONE', #24563 ) ;
#29959 = CARTESIAN_POINT ( 'NONE',  ( 106.4257688009193998, 10.00000000000000000, 289.4830310981789125 ) ) ;
#29960 = CIRCLE ( 'NONE', #68386, 0.3499999999999295341 ) ;
#29961 = AXIS2_PLACEMENT_3D ( 'NONE', #45855, #46550, #56466 ) ;
#29962 = AXIS2_PLACEMENT_3D ( 'NONE', #51207, #14449, #35999 ) ;
#29963 = ORIENTED_EDGE ( 'NONE', *, *, #45715, .T. ) ;
#29964 = FACE_OUTER_BOUND ( 'NONE', #14525, .T. ) ;
#29965 = DIRECTION ( 'NONE',  ( -0.000000000000000000, 3.673940397442059868E-16, -1.000000000000000000 ) ) ;
#29966 = VERTEX_POINT ( 'NONE', #8279 ) ;
#29967 = CYLINDRICAL_SURFACE ( 'NONE', #48398, 0.1999999999999987899 ) ;
#29968 = VECTOR ( 'NONE', #67826, 1000.000000000000000 ) ;
#29969 = PRESENTATION_LAYER_ASSIGNMENT (  '', '', ( #60455 ) ) ;
#29970 = EDGE_LOOP ( 'NONE', ( #61927, #26556, #24069, #50352 ) ) ;
#29971 = AXIS2_PLACEMENT_3D ( 'NONE', #54035, #64625, #16185 ) ;
#29972 = DIRECTION ( 'NONE',  ( -1.000000000000000000, 0.000000000000000000, 0.000000000000000000 ) ) ;
#29973 = ORIENTED_EDGE ( 'NONE', *, *, #61442, .T. ) ;
#29974 = ORIENTED_EDGE ( 'NONE', *, *, #10796, .F. ) ;
#29975 = CARTESIAN_POINT ( 'NONE',  ( 283.0000000000000568, -32.45000000000000995, -15.00000000000000000 ) ) ;
#29976 = ORIENTED_EDGE ( 'NONE', *, *, #63006, .F. ) ;
#29977 = ORIENTED_EDGE ( 'NONE', *, *, #8300, .T. ) ;
#29978 = CARTESIAN_POINT ( 'NONE',  ( -6.822336235477446387, 6.350872789121265072, 26.00000000000000711 ) ) ;
#29979 = CARTESIAN_POINT ( 'NONE',  ( -8.697938382363179954, -8.093267424590409931, 26.00000000000000000 ) ) ;
#29980 = VECTOR ( 'NONE', #2639, 999.9999999999998863 ) ;
#29981 = CARTESIAN_POINT ( 'NONE',  ( 105.8309041053263257, 5.657408540445008960, 2.000000000000000000 ) ) ;
#29982 = VERTEX_POINT ( 'NONE', #67350 ) ;
#29983 = EDGE_CURVE ( 'NONE', #33386, #60663, #29155, .T. ) ;
#29984 = VECTOR ( 'NONE', #63707, 1000.000000000000000 ) ;
#29985 = CARTESIAN_POINT ( 'NONE',  ( -11.00000000000000000, -10.85999999999999943, -9.000000000000001776 ) ) ;
#29986 = EDGE_CURVE ( 'NONE', #11455, #6920, #47775, .T. ) ;
#29988 = CARTESIAN_POINT ( 'NONE',  ( -8.079219948824956532, -8.711985858128644011, 26.00000000000000000 ) ) ;
#29987 = FACE_OUTER_BOUND ( 'NONE', #31627, .T. ) ;
#29989 = VERTEX_POINT ( 'NONE', #29853 ) ;
#29991 = ORIENTED_EDGE ( 'NONE', *, *, #55268, .T. ) ;
#29990 = CARTESIAN_POINT ( 'NONE',  ( 4.186483450353335023, -12.00648345035338238, 195.0000000000000284 ) ) ;
#29992 = ORIENTED_EDGE ( 'NONE', *, *, #56224, .T. ) ;
#29993 = EDGE_CURVE ( 'NONE', #28935, #39720, #68105, .T. ) ;
#29994 =( NAMED_UNIT ( * ) SI_UNIT ( $, .STERADIAN. ) SOLID_ANGLE_UNIT ( ) );
#29995 = DIRECTION ( 'NONE',  ( 0.000000000000000000, 1.000000000000000000, 0.000000000000000000 ) ) ;
#29997 = VERTEX_POINT ( 'NONE', #23852 ) ;
#29996 = DIRECTION ( 'NONE',  ( -1.836970198721029934E-16, 1.836970198721036590E-16, -1.000000000000000000 ) ) ;
#29998 = DIRECTION ( 'NONE',  ( 0.000000000000000000, -0.1111111111108840643, -0.9938079899999319178 ) ) ;
#29999 = DIRECTION ( 'NONE',  ( -0.000000000000000000, -1.000000000000000000, -0.000000000000000000 ) ) ;
#30000 = ORIENTED_EDGE ( 'NONE', *, *, #9600, .F. ) ;
#30001 = AXIS2_PLACEMENT_3D ( 'NONE', #38720, #11837, #59254 ) ;
#30002 = ORIENTED_EDGE ( 'NONE', *, *, #31690, .T. ) ;
#30003 = PLANE ( 'NONE',  #7446 ) ;
#30004 = CIRCLE ( 'NONE', #66085, 3.300000002979700753 ) ;
#30005 = ORIENTED_EDGE ( 'NONE', *, *, #11901, .T. ) ;
#30006 = CARTESIAN_POINT ( 'NONE',  ( -9.828310488885993124, -1.690483450353310158, 195.0000000000000284 ) ) ;
#30007 = CARTESIAN_POINT ( 'NONE',  ( 1.634292677759874746, 8.227189898828697778, 54.00000000000000711 ) ) ;
#30008 = VECTOR ( 'NONE', #19684, 1000.000000000000114 ) ;
#30009 = DIRECTION ( 'NONE',  ( 0.000000000000000000, 0.000000000000000000, -1.000000000000000000 ) ) ;
#30010 = ORIENTED_EDGE ( 'NONE', *, *, #29292, .F. ) ;
#30011 = AXIS2_PLACEMENT_3D ( 'NONE', #30833, #2298, #15277 ) ;
#30012 = VECTOR ( 'NONE', #16361, 1000.000000000000000 ) ;
#30013 = LINE ( 'NONE', #51594, #35815 ) ;
#30014 = CARTESIAN_POINT ( 'NONE',  ( 282.8893988437589542, -20.72883876573682826, 17.22883876573683182 ) ) ;
#30016 = ORIENTED_EDGE ( 'NONE', *, *, #55335, .T. ) ;
#30015 = DIRECTION ( 'NONE',  ( -1.000000000000000000, 0.000000000000000000, 0.000000000000000000 ) ) ;
#30018 = ORIENTED_EDGE ( 'NONE', *, *, #30137, .T. ) ;
#30017 = CYLINDRICAL_SURFACE ( 'NONE', #55764, 5.000000000000000000 ) ;
#30019 = DIRECTION ( 'NONE',  ( 1.000000000000000000, 0.000000000000000000, 0.000000000000000000 ) ) ;
#30020 = CIRCLE ( 'NONE', #60507, 4.000000000000000888 ) ;
#30021 = MECHANICAL_DESIGN_GEOMETRIC_PRESENTATION_REPRESENTATION (  '', ( #69562 ), #26663 ) ;
#30022 = LINE ( 'NONE', #20468, #47678 ) ;
#30023 = DIRECTION ( 'NONE',  ( -1.000000000000000000, 0.000000000000000000, 0.000000000000000000 ) ) ;
#30024 = CARTESIAN_POINT ( 'NONE',  ( 0.000000000000000000, -8.249999999999998224, -20.00000000000000000 ) ) ;
#30025 = AXIS2_PLACEMENT_3D ( 'NONE', #11143, #59930, #32714 ) ;
#30026 = CARTESIAN_POINT ( 'NONE',  ( 11.00000000000000000, -11.70000000000000284, 12.50000000000000000 ) ) ;
#30027 = ORIENTED_EDGE ( 'NONE', *, *, #31093, .F. ) ;
#30028 = LINE ( 'NONE', #13417, #12028 ) ;
#30029 = EDGE_CURVE ( 'NONE', #31517, #50228, #63713, .T. ) ;
#30030 = DIRECTION ( 'NONE',  ( -1.000000000000000000, 0.000000000000000000, 0.000000000000000000 ) ) ;
#30031 = CARTESIAN_POINT ( 'NONE',  ( 19.90000000000000213, -0.000000000000000000, 20.80000000000000426 ) ) ;
#30033 = VERTEX_POINT ( 'NONE', #61677 ) ;
#30032 = DIRECTION ( 'NONE',  ( 1.000000000000000000, 0.000000000000000000, 0.000000000000000000 ) ) ;
#30034 = CIRCLE ( 'NONE', #16472, 1.000000000000000000 ) ;
#30035 = DIRECTION ( 'NONE',  ( -1.000000000000000000, 0.000000000000000000, -0.000000000000000000 ) ) ;
#30036 = ADVANCED_FACE ( 'NONE', ( #13241 ), #13904, .T. ) ;
#30037 = EDGE_CURVE ( 'NONE', #22259, #18238, #38953, .T. ) ;
#30038 = VECTOR ( 'NONE', #67867, 1000.000000000000000 ) ;
#30039 = CYLINDRICAL_SURFACE ( 'NONE', #13772, 0.2500000000000002220 ) ;
#30040 = ORIENTED_EDGE ( 'NONE', *, *, #22333, .T. ) ;
#30041 = ORIENTED_EDGE ( 'NONE', *, *, #54161, .T. ) ;
#30042 = FACE_OUTER_BOUND ( 'NONE', #46525, .T. ) ;
#30043 = DIRECTION ( 'NONE',  ( 0.000000000000000000, -0.7051282051282045105, 0.7090798363602486276 ) ) ;
#30044 = ORIENTED_EDGE ( 'NONE', *, *, #6622, .F. ) ;
#30045 = DIRECTION ( 'NONE',  ( 3.491481338843133355E-15, 1.000000000000000000, 1.836970198721029934E-16 ) ) ;
#30046 = PLANE ( 'NONE',  #61898 ) ;
#30047 = CARTESIAN_POINT ( 'NONE',  ( 11.32648345035333470, 4.393516549646570901, 195.0000000000000284 ) ) ;
#30048 = ADVANCED_FACE ( 'NONE', ( #1468 ), #28339, .F. ) ;
#30049 = DIRECTION ( 'NONE',  ( -0.000000000000000000, 1.000000000000000000, -0.000000000000000000 ) ) ;
#30050 = EDGE_LOOP ( 'NONE', ( #58705, #11197, #49815, #38875 ) ) ;
#30051 = DIRECTION ( 'NONE',  ( 0.000000000000000000, 1.000000000000000000, -0.000000000000000000 ) ) ;
#30052 = VERTEX_POINT ( 'NONE', #22701 ) ;
#30053 = ORIENTED_EDGE ( 'NONE', *, *, #65116, .F. ) ;
#30054 = VECTOR ( 'NONE', #53891, 1000.000000000000000 ) ;
#30055 = ORIENTED_EDGE ( 'NONE', *, *, #52157, .F. ) ;
#30056 = LINE ( 'NONE', #51635, #61909 ) ;
#30057 = AXIS2_PLACEMENT_3D ( 'NONE', #41627, #57886, #20757 ) ;
#30058 = LINE ( 'NONE', #1787, #26508 ) ;
#30059 = AXIS2_PLACEMENT_3D ( 'NONE', #31176, #10293, #15947 ) ;
#30060 = DIRECTION ( 'NONE',  ( -0.8660254037844322683, 0.5000000000000111022, 0.000000000000000000 ) ) ;
#30061 = ORIENTED_EDGE ( 'NONE', *, *, #54021, .F. ) ;
#30062 = ORIENTED_EDGE ( 'NONE', *, *, #11357, .T. ) ;
#30063 = DIRECTION ( 'NONE',  ( -1.000000000000000000, 0.000000000000000000, 0.000000000000000000 ) ) ;
#30064 = ORIENTED_EDGE ( 'NONE', *, *, #25391, .F. ) ;
#30065 = ORIENTED_EDGE ( 'NONE', *, *, #23000, .T. ) ;
#30066 = VECTOR ( 'NONE', #29332, 1000.000000000000000 ) ;
#30067 = CYLINDRICAL_SURFACE ( 'NONE', #6688, 0.1999999999999996503 ) ;
#30068 = DIRECTION ( 'NONE',  ( 0.000000000000000000, -0.7071067811865474617, 0.7071067811865474617 ) ) ;
#30069 = CARTESIAN_POINT ( 'NONE',  ( 15.89999999999999680, 20.60000000000000142, -13.86939075806900057 ) ) ;
#30070 = FACE_OUTER_BOUND ( 'NONE', #11991, .T. ) ;
#30071 = EDGE_LOOP ( 'NONE', ( #7259, #51848, #40675, #33262 ) ) ;
#30072 = CARTESIAN_POINT ( 'NONE',  ( 25.50000000000000355, 0.000000000000000000, -24.75000000000000000 ) ) ;
#30073 = VECTOR ( 'NONE', #42902, 1000.000000000000000 ) ;
#30074 = AXIS2_PLACEMENT_3D ( 'NONE', #32617, #54188, #27310 ) ;
#30075 = AXIS2_PLACEMENT_3D ( 'NONE', #39538, #18672, #8404 ) ;
#30077 = DIRECTION ( 'NONE',  ( 1.011922027653137735E-14, 1.000000000000000000, 0.000000000000000000 ) ) ;
#30076 = DIRECTION ( 'NONE',  ( 0.000000000000000000, -3.673940397442059868E-16, 1.000000000000000000 ) ) ;
#30078 = ORIENTED_EDGE ( 'NONE', *, *, #10475, .F. ) ;
#30080 = ORIENTED_EDGE ( 'NONE', *, *, #69942, .F. ) ;
#30079 = FACE_OUTER_BOUND ( 'NONE', #34581, .T. ) ;
#30081 = VERTEX_POINT ( 'NONE', #50256 ) ;
#30082 = EDGE_LOOP ( 'NONE', ( #31841, #41213, #28829, #62424 ) ) ;
#30083 = EDGE_CURVE ( 'NONE', #167, #37419, #18421, .T. ) ;
#30084 = CIRCLE ( 'NONE', #38030, 1.999999999999315436 ) ;
#30085 = DIRECTION ( 'NONE',  ( -1.000000000000000000, 0.000000000000000000, 0.000000000000000000 ) ) ;
#30086 = VECTOR ( 'NONE', #23134, 1000.000000000000000 ) ;
#30087 = CARTESIAN_POINT ( 'NONE',  ( -6.344366288193410419, 5.779227145995219139, 26.00000000000000711 ) ) ;
#30088 = ORIENTED_EDGE ( 'NONE', *, *, #43547, .F. ) ;
#30089 = ORIENTED_EDGE ( 'NONE', *, *, #59243, .F. ) ;
#30090 = EDGE_CURVE ( 'NONE', #31863, #67236, #65829, .T. ) ;
#30091 = LINE ( 'NONE', #68973, #27418 ) ;
#30092 = DIRECTION ( 'NONE',  ( 1.000000000000000000, 0.000000000000000000, 0.000000000000000000 ) ) ;
#30093 = ORIENTED_EDGE ( 'NONE', *, *, #45983, .T. ) ;
#30094 = ORIENTED_EDGE ( 'NONE', *, *, #39432, .F. ) ;
#30095 = DIRECTION ( 'NONE',  ( -0.000000000000000000, 0.000000000000000000, -1.000000000000000000 ) ) ;
#30096 = ADVANCED_FACE ( 'NONE', ( #33653 ), #60860, .F. ) ;
#30097 = CARTESIAN_POINT ( 'NONE',  ( 7.450000000000003730, -7.249999999999997335, -13.50000000000000178 ) ) ;
#30098 = ORIENTED_EDGE ( 'NONE', *, *, #17234, .T. ) ;
#30099 = DIRECTION ( 'NONE',  ( 0.000000000000000000, -1.000000000000000000, 0.000000000000000000 ) ) ;
#30100 = CARTESIAN_POINT ( 'NONE',  ( 275.0000000000000000, -39.79999999999905214, -12.19999999999906315 ) ) ;
#30101 = AXIS2_PLACEMENT_3D ( 'NONE', #48490, #54147, #21622 ) ;
#30103 = ORIENTED_EDGE ( 'NONE', *, *, #26617, .T. ) ;
#30102 = LINE ( 'NONE', #35751, #5801 ) ;
#30104 = ORIENTED_EDGE ( 'NONE', *, *, #29943, .F. ) ;
#30105 = DIRECTION ( 'NONE',  ( -1.000000000000000000, 0.000000000000000000, 0.000000000000000000 ) ) ;
#30106 = AXIS2_PLACEMENT_3D ( 'NONE', #26687, #48601, #37302 ) ;
#30107 = CARTESIAN_POINT ( 'NONE',  ( 8.406483450353405829, 7.603567055985406498, 455.0000000000000568 ) ) ;
#30108 = DIRECTION ( 'NONE',  ( 0.000000000000000000, 0.000000000000000000, 1.000000000000000000 ) ) ;
#30109 = CARTESIAN_POINT ( 'NONE',  ( -9.722976262117239088, 7.290476262117218553, 26.00000000000000711 ) ) ;
#30110 = CARTESIAN_POINT ( 'NONE',  ( -7.250000000000000000, -7.449999999999998401, -13.00000000000000178 ) ) ;
#30111 = VECTOR ( 'NONE', #69330, 1000.000000000000000 ) ;
#30112 = DIRECTION ( 'NONE',  ( -1.349135440953254490E-14, -1.000000000000000000, 0.000000000000000000 ) ) ;
#30113 = ORIENTED_EDGE ( 'NONE', *, *, #68823, .T. ) ;
#30114 = LINE ( 'NONE', #51330, #12274 ) ;
#30115 = EDGE_CURVE ( 'NONE', #62940, #45716, #35638, .T. ) ;
#30117 = ORIENTED_EDGE ( 'NONE', *, *, #69497, .T. ) ;
#30116 = DIRECTION ( 'NONE',  ( -1.000000000000000000, 0.000000000000000000, 0.000000000000000000 ) ) ;
#30119 = CARTESIAN_POINT ( 'NONE',  ( -1.077516549646778010, -10.74648345035343056, 195.0000000000000284 ) ) ;
#30118 = AXIS2_PLACEMENT_3D ( 'NONE', #37422, #58979, #10193 ) ;
#30120 = DIRECTION ( 'NONE',  ( 0.000000000000000000, 1.000000000000000000, 0.000000000000000000 ) ) ;
#30121 = EDGE_CURVE ( 'NONE', #26906, #47459, #6769, .T. ) ;
#30122 = EDGE_CURVE ( 'NONE', #20149, #54700, #16182, .T. ) ;
#30123 = CARTESIAN_POINT ( 'NONE',  ( 14.50000000000000000, 0.000000000000000000, -26.50000000000000000 ) ) ;
#30124 = LINE ( 'NONE', #51705, #62324 ) ;
#30125 = VECTOR ( 'NONE', #60114, 1000.000000000000000 ) ;
#30126 = AXIS2_PLACEMENT_3D ( 'NONE', #24954, #30959, #8691 ) ;
#30127 = DIRECTION ( 'NONE',  ( -0.000000000000000000, -0.000000000000000000, -1.000000000000000000 ) ) ;
#30128 = EDGE_CURVE ( 'NONE', #2608, #43786, #390, .T. ) ;
#30129 = ORIENTED_EDGE ( 'NONE', *, *, #69006, .F. ) ;
#30130 = FACE_OUTER_BOUND ( 'NONE', #61812, .T. ) ;
#30131 = FACE_OUTER_BOUND ( 'NONE', #23781, .T. ) ;
#30132 = ORIENTED_EDGE ( 'NONE', *, *, #4303, .T. ) ;
#30133 = EDGE_CURVE ( 'NONE', #36865, #7150, #5987, .T. ) ;
#30134 = VECTOR ( 'NONE', #47674, 1000.000000000000000 ) ;
#30135 = DIRECTION ( 'NONE',  ( -0.000000000000000000, -0.000000000000000000, -1.000000000000000000 ) ) ;
#30136 = EDGE_CURVE ( 'NONE', #23076, #8233, #28685, .T. ) ;
#30137 = EDGE_CURVE ( 'NONE', #51421, #31198, #15025, .T. ) ;
#30138 = CIRCLE ( 'NONE', #52729, 3.999999999999993339 ) ;
#30139 = DIRECTION ( 'NONE',  ( 0.000000000000000000, 0.000000000000000000, 1.000000000000000000 ) ) ;
#30140 = ORIENTED_EDGE ( 'NONE', *, *, #51678, .T. ) ;
#30141 = DIRECTION ( 'NONE',  ( 0.000000000000000000, -0.7046037717859411353, -0.7096009616573427659 ) ) ;
#30142 = ORIENTED_EDGE ( 'NONE', *, *, #55349, .F. ) ;
#30143 = ORIENTED_EDGE ( 'NONE', *, *, #57080, .F. ) ;
#30144 = DIRECTION ( 'NONE',  ( 0.000000000000000000, 0.7071067811865450192, 0.7071067811865500152 ) ) ;
#30145 = DIRECTION ( 'NONE',  ( -1.000000000000000000, 0.000000000000000000, 0.000000000000000000 ) ) ;
#30146 = CARTESIAN_POINT ( 'NONE',  ( -15.50000000000129852, -15.50000000000000000, 22.50000000000000000 ) ) ;
#30147 = LINE ( 'NONE', #19528, #37713 ) ;
#30148 = PLANE ( 'NONE',  #66747 ) ;
#30149 = ORIENTED_EDGE ( 'NONE', *, *, #58315, .F. ) ;
#30150 = ORIENTED_EDGE ( 'NONE', *, *, #55581, .F. ) ;
#30152 = VERTEX_POINT ( 'NONE', #18072 ) ;
#30151 = DIRECTION ( 'NONE',  ( -1.000000000000000000, 0.000000000000000000, 0.000000000000000000 ) ) ;
#30153 = EDGE_LOOP ( 'NONE', ( #8134, #52366, #15306, #47192 ) ) ;
#30154 = DIRECTION ( 'NONE',  ( 0.000000000000000000, 1.000000000000000000, 0.000000000000000000 ) ) ;
#30155 = CARTESIAN_POINT ( 'NONE',  ( 283.0000000000000568, -23.29603921945599865, 12.50000000000000000 ) ) ;
#30156 = CARTESIAN_POINT ( 'NONE',  ( 28.90000000000000213, -21.00000000000000000, 13.86939075806900057 ) ) ;
#30157 = EDGE_CURVE ( 'NONE', #22414, #16920, #46257, .T. ) ;
#30158 = PLANE ( 'NONE',  #4901 ) ;
#30159 = VECTOR ( 'NONE', #66988, 1000.000000000000000 ) ;
#30160 = CARTESIAN_POINT ( 'NONE',  ( 6.006483450353401921, 7.393516549646579783, 455.0000000000000568 ) ) ;
#30161 = DIRECTION ( 'NONE',  ( -0.6414496315691484707, 0.7671651518153074223, 2.309356642088893343E-17 ) ) ;
#30162 = ORIENTED_EDGE ( 'NONE', *, *, #23879, .F. ) ;
#30163 = ORIENTED_EDGE ( 'NONE', *, *, #5385, .T. ) ;
#30164 = ORIENTED_EDGE ( 'NONE', *, *, #20688, .F. ) ;
#30165 = ADVANCED_FACE ( 'NONE', ( #61196 ), #64740, .F. ) ;
#30166 = CIRCLE ( 'NONE', #50496, 0.1749999999999998224 ) ;
#30167 = AXIS2_PLACEMENT_3D ( 'NONE', #46898, #51517, #35951 ) ;
#30168 = CIRCLE ( 'NONE', #66302, 3.299999999999473577 ) ;
#30169 = ORIENTED_EDGE ( 'NONE', *, *, #41936, .F. ) ;
#30170 = CARTESIAN_POINT ( 'NONE',  ( -10.08346604330787777, 2.893516549646604208, 455.0000000000000568 ) ) ;
#30171 = LINE ( 'NONE', #67651, #56909 ) ;
#30172 = EDGE_CURVE ( 'NONE', #49071, #55278, #22367, .T. ) ;
#30173 = AXIS2_PLACEMENT_3D ( 'NONE', #497, #60573, #44642 ) ;
#30174 = AXIS2_PLACEMENT_3D ( 'NONE', #57055, #61659, #40078 ) ;
#30175 = CARTESIAN_POINT ( 'NONE',  ( 8.250000000000005329, 8.250000000000001776, -26.00000000000001066 ) ) ;
#30176 = ORIENTED_EDGE ( 'NONE', *, *, #48478, .T. ) ;
#30177 = ORIENTED_EDGE ( 'NONE', *, *, #53413, .F. ) ;
#30178 = VERTEX_POINT ( 'NONE', #51573 ) ;
#30179 = CARTESIAN_POINT ( 'NONE',  ( -1.466476262117323737, -9.404523737882843903, 54.00000000000000711 ) ) ;
#30180 = VECTOR ( 'NONE', #36639, 1000.000000000000000 ) ;
#30181 = EDGE_LOOP ( 'NONE', ( #52626, #16019, #67916, #23206 ) ) ;
#30182 = EDGE_LOOP ( 'NONE', ( #15967, #28726, #56323, #59215 ) ) ;
#30183 = CARTESIAN_POINT ( 'NONE',  ( 29.89999999999999858, 20.60000000000000142, 13.86939075806899702 ) ) ;
#30184 = VERTEX_POINT ( 'NONE', #3141 ) ;
#30185 = ORIENTED_EDGE ( 'NONE', *, *, #67951, .F. ) ;
#30186 = DIRECTION ( 'NONE',  ( 0.000000000000000000, 1.000000000000000000, 3.673940397442059868E-16 ) ) ;
#30187 = EDGE_CURVE ( 'NONE', #31998, #21817, #43914, .T. ) ;
#30189 = EDGE_LOOP ( 'NONE', ( #42771, #8988, #50645, #63099 ) ) ;
#30188 = DIRECTION ( 'NONE',  ( 1.000000000000000000, -1.952517519553884087E-14, 1.836970198720994435E-16 ) ) ;
#30190 = EDGE_LOOP ( 'NONE', ( #32275, #8397, #31523, #37997 ) ) ;
#30191 = CARTESIAN_POINT ( 'NONE',  ( -4.383466043307922000, -8.606483450353396236, 195.0000000000000284 ) ) ;
#30192 = VECTOR ( 'NONE', #68207, 1000.000000000000000 ) ;
#30193 = PLANE ( 'NONE',  #30712 ) ;
#30194 = PLANE ( 'NONE',  #7643 ) ;
#30195 = EDGE_CURVE ( 'NONE', #2261, #24784, #11724, .T. ) ;
#30197 = ORIENTED_EDGE ( 'NONE', *, *, #28837, .F. ) ;
#30196 = LINE ( 'NONE', #51766, #12057 ) ;
#30198 = EDGE_CURVE ( 'NONE', #61047, #58319, #14796, .T. ) ;
#30199 = ORIENTED_EDGE ( 'NONE', *, *, #6130, .F. ) ;
#30200 = CARTESIAN_POINT ( 'NONE',  ( -7.342976262117269393, -4.961189459949999936, 26.00000000000000711 ) ) ;
#30201 = EDGE_CURVE ( 'NONE', #13751, #64704, #20785, .T. ) ;
#30202 = CARTESIAN_POINT ( 'NONE',  ( 7.450000000000004619, -1.336933437520057563E-15, -17.50000000000000000 ) ) ;
#30203 = EDGE_CURVE ( 'NONE', #54664, #10280, #68543, .T. ) ;
#30204 = EDGE_CURVE ( 'NONE', #4613, #18545, #4539, .T. ) ;
#30205 = CARTESIAN_POINT ( 'NONE',  ( -29.25000000000000000, -5.200000000000001066, 60.00000000000000000 ) ) ;
#30206 = FACE_OUTER_BOUND ( 'NONE', #16067, .T. ) ;
#30207 = ORIENTED_EDGE ( 'NONE', *, *, #2942, .F. ) ;
#30208 = CARTESIAN_POINT ( 'NONE',  ( 4.201500623656039934, 7.259684009079806266, 455.0000000000000568 ) ) ;
#30209 = EDGE_CURVE ( 'NONE', #27966, #43050, #61324, .T. ) ;
#30210 = DIRECTION ( 'NONE',  ( 0.000000000000000000, 0.000000000000000000, -1.000000000000000000 ) ) ;
#30211 = DIRECTION ( 'NONE',  ( 1.000000000000000000, 0.000000000000000000, 0.000000000000000000 ) ) ;
#30212 = EDGE_CURVE ( 'NONE', #32551, #14268, #20096, .T. ) ;
#30213 = CIRCLE ( 'NONE', #1984, 1.620999999999997332 ) ;
#30214 = ORIENTED_EDGE ( 'NONE', *, *, #39908, .F. ) ;
#30215 = CARTESIAN_POINT ( 'NONE',  ( 29.50000000000000355, -11.50000000000100009, -15.00000000000084910 ) ) ;
#30216 = EDGE_CURVE ( 'NONE', #65652, #36958, #5388, .T. ) ;
#30217 = DIRECTION ( 'NONE',  ( -1.000000000000000000, 8.728482790395504563E-15, 0.000000000000000000 ) ) ;
#30218 = CARTESIAN_POINT ( 'NONE',  ( -6.835476262117334834, -10.50702373788278798, 54.00000000000000711 ) ) ;
#30219 = ORIENTED_EDGE ( 'NONE', *, *, #60896, .T. ) ;
#30220 = VECTOR ( 'NONE', #20797, 1000.000000000000000 ) ;
#30221 = CIRCLE ( 'NONE', #34691, 0.8099999999999999423 ) ;
#30222 = VECTOR ( 'NONE', #34867, 1000.000000000000000 ) ;
#30223 =( NAMED_UNIT ( * ) SI_UNIT ( $, .STERADIAN. ) SOLID_ANGLE_UNIT ( ) );
#30224 = EDGE_CURVE ( 'NONE', #4508, #22980, #25219, .T. ) ;
#30225 = LINE ( 'NONE', #8647, #20958 ) ;
#30226 = EDGE_CURVE ( 'NONE', #21406, #46314, #68888, .T. ) ;
#30227 = AXIS2_PLACEMENT_3D ( 'NONE', #3977, #31558, #25902 ) ;
#30228 = AXIS2_PLACEMENT_3D ( 'NONE', #23749, #24451, #8522 ) ;
#30229 = PLANE ( 'NONE',  #46267 ) ;
#30230 = ORIENTED_EDGE ( 'NONE', *, *, #10610, .T. ) ;
#30231 = DIRECTION ( 'NONE',  ( -1.000000000000000000, 0.000000000000000000, 0.000000000000000000 ) ) ;
#30232 = DIRECTION ( 'NONE',  ( -0.7071067811865401342, 0.7071067811865550112, 1.365336182113289717E-30 ) ) ;
#30233 = DIRECTION ( 'NONE',  ( 3.491481338843133355E-15, 1.000000000000000000, 1.836970198721029934E-16 ) ) ;
#30234 = VECTOR ( 'NONE', #60206, 1000.000000000000000 ) ;
#30235 = CARTESIAN_POINT ( 'NONE',  ( 10.14575131106465378, -25.50000000000000355, -17.00000000000000000 ) ) ;
#30236 = VECTOR ( 'NONE', #58959, 1000.000000000000000 ) ;
#30237 = DIRECTION ( 'NONE',  ( 0.000000000000000000, 0.000000000000000000, -1.000000000000000000 ) ) ;
#30238 = VERTEX_POINT ( 'NONE', #51925 ) ;
#30239 = CARTESIAN_POINT ( 'NONE',  ( 11.00000000000000000, -5.599999999999999645, -27.00000000000000000 ) ) ;
#30240 = CARTESIAN_POINT ( 'NONE',  ( 38.90000000000000568, 20.60000000000000142, 13.86939075806900057 ) ) ;
#30241 = FACE_OUTER_BOUND ( 'NONE', #50196, .T. ) ;
#30242 = SURFACE_STYLE_USAGE ( .BOTH. , #13960 ) ;
#30243 = FACE_OUTER_BOUND ( 'NONE', #8305, .T. ) ;
#30244 = VERTEX_POINT ( 'NONE', #31420 ) ;
#30246 = EDGE_LOOP ( 'NONE', ( #34844, #10011, #35483, #14772 ) ) ;
#30245 = CARTESIAN_POINT ( 'NONE',  ( -7.450000000000001954, -7.249999999999998224, -16.50000000000000000 ) ) ;
#30247 = AXIS2_PLACEMENT_3D ( 'NONE', #66380, #50463, #33838 ) ;
#30248 = FACE_OUTER_BOUND ( 'NONE', #62175, .T. ) ;
#30249 = CARTESIAN_POINT ( 'NONE',  ( 12.00648345035336284, 7.813516549646607245, 195.0000000000000284 ) ) ;
#30250 = DIRECTION ( 'NONE',  ( 0.000000000000000000, 0.000000000000000000, 1.000000000000000000 ) ) ;
#30251 = ORIENTED_EDGE ( 'NONE', *, *, #52118, .F. ) ;
#30252 = PLANE ( 'NONE',  #64599 ) ;
#30253 = ORIENTED_EDGE ( 'NONE', *, *, #49121, .T. ) ;
#30254 = EDGE_CURVE ( 'NONE', #3304, #50773, #57572, .T. ) ;
#30255 = ORIENTED_EDGE ( 'NONE', *, *, #61191, .F. ) ;
#30256 = ORIENTED_EDGE ( 'NONE', *, *, #40676, .T. ) ;
#30257 = PLANE ( 'NONE',  #18281 ) ;
#30258 = CARTESIAN_POINT ( 'NONE',  ( -16.89194109070750116, -5.000000000000000000, -26.25000000000000000 ) ) ;
#30259 = ADVANCED_FACE ( 'NONE', ( #9138 ), #4883, .F. ) ;
#30260 = CARTESIAN_POINT ( 'NONE',  ( -28.00000000000000000, -16.28999999999710369, 15.00000000000794920 ) ) ;
#30261 = DIRECTION ( 'NONE',  ( 0.000000000000000000, 0.000000000000000000, 1.000000000000000000 ) ) ;
#30262 = MECHANICAL_DESIGN_GEOMETRIC_PRESENTATION_REPRESENTATION (  '', ( #48337 ), #4341 ) ;
#30263 = VERTEX_POINT ( 'NONE', #57920 ) ;
#30264 = ORIENTED_EDGE ( 'NONE', *, *, #54809, .T. ) ;
#30265 = EDGE_CURVE ( 'NONE', #39386, #50504, #41657, .T. ) ;
#30266 = FACE_OUTER_BOUND ( 'NONE', #23218, .T. ) ;
#30267 = DIRECTION ( 'NONE',  ( 0.000000000000000000, 0.000000000000000000, 1.000000000000000000 ) ) ;
#30268 = VERTEX_POINT ( 'NONE', #26451 ) ;
#30269 = EDGE_CURVE ( 'NONE', #63123, #49409, #9848, .T. ) ;
#30270 = ORIENTED_EDGE ( 'NONE', *, *, #55188, .F. ) ;
#30271 = VERTEX_POINT ( 'NONE', #3487 ) ;
#30272 = ORIENTED_EDGE ( 'NONE', *, *, #4980, .T. ) ;
#30273 = CARTESIAN_POINT ( 'NONE',  ( 8.406483450353334774, 4.383466043307768345, 195.0000000000000284 ) ) ;
#30274 = UNCERTAINTY_MEASURE_WITH_UNIT (LENGTH_MEASURE( 1.000000000000000082E-05 ), #5183, 'distance_accuracy_value', 'NONE');
#30275 = EDGE_CURVE ( 'NONE', #31134, #8535, #53335, .T. ) ;
#30277 = ORIENTED_EDGE ( 'NONE', *, *, #30964, .T. ) ;
#30276 = CARTESIAN_POINT ( 'NONE',  ( 29.50000000000000355, -11.50000000000000000, 11.00000000000000000 ) ) ;
#30278 = VECTOR ( 'NONE', #64341, 1000.000000000000000 ) ;
#30279 = DIRECTION ( 'NONE',  ( 0.000000000000000000, 0.000000000000000000, 1.000000000000000000 ) ) ;
#30280 = CARTESIAN_POINT ( 'NONE',  ( 10.31452373788281562, -3.857023737882814718, 26.00000000000000711 ) ) ;
#30281 = ORIENTED_EDGE ( 'NONE', *, *, #15619, .F. ) ;
#30282 = ORIENTED_EDGE ( 'NONE', *, *, #32431, .F. ) ;
#30283 = VECTOR ( 'NONE', #1390, 1000.000000000000000 ) ;
#30284 = AXIS2_PLACEMENT_3D ( 'NONE', #66681, #39793, #62066 ) ;
#30285 = EDGE_CURVE ( 'NONE', #15679, #3626, #63225, .T. ) ;
#30286 = DIRECTION ( 'NONE',  ( 0.000000000000000000, 1.000000000000000000, 0.000000000000000000 ) ) ;
#30287 = DIRECTION ( 'NONE',  ( 0.000000000000000000, -3.673940397442059868E-16, 1.000000000000000000 ) ) ;
#30288 = DIRECTION ( 'NONE',  ( 0.000000000000000000, -1.000000000000000000, 0.000000000000000000 ) ) ;
#30289 = AXIS2_PLACEMENT_3D ( 'NONE', #851, #11090, #53894 ) ;
#30290 = PLANE ( 'NONE',  #4032 ) ;
#30291 = PLANE ( 'NONE',  #10997 ) ;
#30293 = ORIENTED_EDGE ( 'NONE', *, *, #24672, .F. ) ;
#30292 = FACE_OUTER_BOUND ( 'NONE', #19608, .T. ) ;
#30294 = ORIENTED_EDGE ( 'NONE', *, *, #11518, .T. ) ;
#30295 = DIRECTION ( 'NONE',  ( -1.000000000000000000, 1.794541526872559352E-16, 0.000000000000000000 ) ) ;
#30296 = CYLINDRICAL_SURFACE ( 'NONE', #34658, 1.000000000000000000 ) ;
#30297 = CARTESIAN_POINT ( 'NONE',  ( 0.9555237378828180805, 9.915476262117216777, 54.00000000000000711 ) ) ;
#30298 = DIRECTION ( 'NONE',  ( 9.050731179009442381E-15, 1.000000000000000000, 0.000000000000000000 ) ) ;
#30299 = LINE ( 'NONE', #13676, #59067 ) ;
#30300 = VERTEX_POINT ( 'NONE', #63936 ) ;
#30301 = FACE_OUTER_BOUND ( 'NONE', #41410, .T. ) ;
#30302 = CARTESIAN_POINT ( 'NONE',  ( 4.396432944014576627, 8.393516549646587777, 455.0000000000000568 ) ) ;
#30303 = EDGE_CURVE ( 'NONE', #21925, #24235, #37413, .T. ) ;
#30304 = DIRECTION ( 'NONE',  ( -0.7071067811865485719, -0.7071067811865465735, 0.000000000000000000 ) ) ;
#30305 = CYLINDRICAL_SURFACE ( 'NONE', #13037, 2.215251240775983899 ) ;
#30306 = EDGE_CURVE ( 'NONE', #35699, #45713, #31764, .T. ) ;
#30307 = DIRECTION ( 'NONE',  ( 0.000000000000000000, 0.000000000000000000, -1.000000000000000000 ) ) ;
#30308 = CYLINDRICAL_SURFACE ( 'NONE', #18346, 0.5999999999999994227 ) ;
#30309 = CARTESIAN_POINT ( 'NONE',  ( -7.394232575409651176, -6.789561617636906909, 54.00000000000000711 ) ) ;
#30310 = VERTEX_POINT ( 'NONE', #46601 ) ;
#30311 = CARTESIAN_POINT ( 'NONE',  ( -11.00000000000000000, -14.04000000000000092, -14.80000000000000071 ) ) ;
#30312 = CARTESIAN_POINT ( 'NONE',  ( -2.893516549646771630, -10.09643294401457680, 195.0000000000000284 ) ) ;
#30313 = VERTEX_POINT ( 'NONE', #19723 ) ;
#30314 = DIRECTION ( 'NONE',  ( 0.000000000000000000, -1.000000000000000000, 0.000000000000000000 ) ) ;
#30315 = DIRECTION ( 'NONE',  ( -0.000000000000000000, 1.000000000000000000, -0.000000000000000000 ) ) ;
#30316 = DIRECTION ( 'NONE',  ( -1.000000000000000000, 0.000000000000000000, 0.000000000000000000 ) ) ;
#30317 = DIRECTION ( 'NONE',  ( 1.836970198721029934E-16, 1.836970198721010706E-16, -1.000000000000000000 ) ) ;
#30318 = CARTESIAN_POINT ( 'NONE',  ( 7.250000000000005329, -7.249999999999998224, -22.00000000000000000 ) ) ;
#30319 = VERTEX_POINT ( 'NONE', #16881 ) ;
#30320 = VECTOR ( 'NONE', #36151, 1000.000000000000000 ) ;
#30321 = LINE ( 'NONE', #9100, #43203 ) ;
#30322 = ORIENTED_EDGE ( 'NONE', *, *, #18362, .F. ) ;
#30323 = CARTESIAN_POINT ( 'NONE',  ( 23.48000000000000043, -17.50000000000000000, -26.00000000000000355 ) ) ;
#30324 = CARTESIAN_POINT ( 'NONE',  ( 30.00000000000000000, -12.00000000000000000, -11.00000000000000000 ) ) ;
#30325 = ORIENTED_EDGE ( 'NONE', *, *, #5685, .T. ) ;
#30326 = FACE_OUTER_BOUND ( 'NONE', #61033, .T. ) ;
#30327 = VECTOR ( 'NONE', #6198, 1000.000000000000000 ) ;
#30328 = VERTEX_POINT ( 'NONE', #11219 ) ;
#30329 = DIRECTION ( 'NONE',  ( -1.000000000000000000, 0.000000000000000000, 0.000000000000000000 ) ) ;
#30330 = ORIENTED_EDGE ( 'NONE', *, *, #35433, .T. ) ;
#30331 = ORIENTED_EDGE ( 'NONE', *, *, #7850, .T. ) ;
#30332 = FACE_BOUND ( 'NONE', #2557, .T. ) ;
#30333 = ORIENTED_EDGE ( 'NONE', *, *, #24853, .T. ) ;
#30334 = ORIENTED_EDGE ( 'NONE', *, *, #53970, .T. ) ;
#30335 = CIRCLE ( 'NONE', #68717, 0.2000000000000005107 ) ;
#30336 = EDGE_CURVE ( 'NONE', #42085, #16791, #65664, .T. ) ;
#30337 = DIRECTION ( 'NONE',  ( 1.000000000000000000, 0.000000000000000000, 0.000000000000000000 ) ) ;
#30338 = CARTESIAN_POINT ( 'NONE',  ( 39.90000000000000568, -16.96999999999999886, 21.00000000000000000 ) ) ;
#30339 = CARTESIAN_POINT ( 'NONE',  ( 8.250000000000005329, -7.249999999999998224, -22.00000000000000000 ) ) ;
#30340 = ORIENTED_EDGE ( 'NONE', *, *, #30643, .F. ) ;
#30341 = EDGE_CURVE ( 'NONE', #39384, #4186, #46655, .T. ) ;
#30342 = DIRECTION ( 'NONE',  ( 7.751221965937476285E-17, -1.000000000000000000, 0.000000000000000000 ) ) ;
#30344 = CYLINDRICAL_SURFACE ( 'NONE', #26558, 24.99999999998794920 ) ;
#30343 = PLANE ( 'NONE',  #27067 ) ;
#30345 = ORIENTED_EDGE ( 'NONE', *, *, #66979, .T. ) ;
#30347 = EDGE_LOOP ( 'NONE', ( #43584, #30197 ) ) ;
#30346 = DIRECTION ( 'NONE',  ( 0.000000000000000000, 0.000000000000000000, -1.000000000000000000 ) ) ;
#30348 = EDGE_CURVE ( 'NONE', #32705, #60377, #6266, .T. ) ;
#30349 = ORIENTED_EDGE ( 'NONE', *, *, #17680, .T. ) ;
#30350 = ADVANCED_FACE ( 'NONE', ( #44417 ), #5923, .F. ) ;
#30351 = SHAPE_DEFINITION_REPRESENTATION ( #18277, #49776 ) ;
#30352 = EDGE_CURVE ( 'NONE', #5855, #7022, #17213, .T. ) ;
#30353 = EDGE_CURVE ( 'NONE', #5423, #60569, #27435, .T. ) ;
#30354 = CARTESIAN_POINT ( 'NONE',  ( 11.78648345035333200, 4.173516549646566709, 195.0000000000000284 ) ) ;
#30356 = ORIENTED_EDGE ( 'NONE', *, *, #14742, .F. ) ;
#30355 = DIRECTION ( 'NONE',  ( 0.8660254037844322683, -0.5000000000000111022, 6.723777587268230953E-17 ) ) ;
#30357 = DIRECTION ( 'NONE',  ( 0.000000000000000000, 1.000000000000000000, 0.000000000000000000 ) ) ;
#30358 = EDGE_CURVE ( 'NONE', #46340, #47169, #49414, .T. ) ;
#30359 = CARTESIAN_POINT ( 'NONE',  ( -3.710438382363119736, 7.394232575409525943, 54.00000000000000711 ) ) ;
#30360 = VERTEX_POINT ( 'NONE', #64623 ) ;
#30361 = VERTEX_POINT ( 'NONE', #17560 ) ;
#30362 = PLANE ( 'NONE',  #49271 ) ;
#30363 = ORIENTED_EDGE ( 'NONE', *, *, #34277, .F. ) ;
#30364 = AXIS2_PLACEMENT_3D ( 'NONE', #5495, #27048, #6174 ) ;
#30365 = DIRECTION ( 'NONE',  ( 8.673617379884068604E-15, 1.000000000000000000, 0.000000000000000000 ) ) ;
#30366 = CARTESIAN_POINT ( 'NONE',  ( 5.257023737882801306, 5.242976262117200470, 54.00000000000000711 ) ) ;
#30367 = CARTESIAN_POINT ( 'NONE',  ( 7.250000000000005329, 7.250000000000000888, -16.50000000000000000 ) ) ;
#30368 = ORIENTED_EDGE ( 'NONE', *, *, #8965, .F. ) ;
#30369 = AXIS2_PLACEMENT_3D ( 'NONE', #40330, #18054, #45617 ) ;
#30370 = DIRECTION ( 'NONE',  ( 0.000000000000000000, -0.7071067811865474617, 0.7071067811865474617 ) ) ;
#30371 = FACE_OUTER_BOUND ( 'NONE', #29157, .T. ) ;
#30373 = ORIENTED_EDGE ( 'NONE', *, *, #9017, .F. ) ;
#30372 = SURFACE_SIDE_STYLE ('',( #46276 ) ) ;
#30375 = ORIENTED_EDGE ( 'NONE', *, *, #21200, .F. ) ;
#30374 = DIRECTION ( 'NONE',  ( -0.000000000000000000, -0.000000000000000000, -1.000000000000000000 ) ) ;
#30376 = CARTESIAN_POINT ( 'NONE',  ( 7.265214908726092879, 5.380658396643145380, 195.0000000000000284 ) ) ;
#30377 = VECTOR ( 'NONE', #37615, 1000.000000000000000 ) ;
#30378 = CARTESIAN_POINT ( 'NONE',  ( 9.899999999999998579, -14.06939075806902117, -20.80000000000000426 ) ) ;
#30379 = CARTESIAN_POINT ( 'NONE',  ( 11.12648345035335851, 7.793516549646610336, 195.0000000000000284 ) ) ;
#30380 = PLANE ( 'NONE',  #49765 ) ;
#30381 = VECTOR ( 'NONE', #57277, 1000.000000000000000 ) ;
#30382 = DIRECTION ( 'NONE',  ( -0.000000000000000000, 3.673940397442059868E-16, -1.000000000000000000 ) ) ;
#30383 = ORIENTED_EDGE ( 'NONE', *, *, #15984, .F. ) ;
#30384 = FACE_OUTER_BOUND ( 'NONE', #64595, .T. ) ;
#30385 = DIRECTION ( 'NONE',  ( 1.836970198721029934E-16, 1.836970198721010706E-16, -1.000000000000000000 ) ) ;
#30386 = CARTESIAN_POINT ( 'NONE',  ( 22.90000000000000213, 20.60000000000000142, -13.86939075806900057 ) ) ;
#30388 = VECTOR ( 'NONE', #21843, 1000.000000000000000 ) ;
#30387 = AXIS2_PLACEMENT_3D ( 'NONE', #24998, #9083, #25351 ) ;
#30390 = VERTEX_POINT ( 'NONE', #64978 ) ;
#30389 = CARTESIAN_POINT ( 'NONE',  ( -6.486996718459931088, 3.142976262117183062, 54.00000000000000711 ) ) ;
#30391 = EDGE_CURVE ( 'NONE', #2217, #8225, #27484, .T. ) ;
#30392 = DIRECTION ( 'NONE',  ( 0.000000000000000000, -0.7071067811865455743, -0.7071067811865495711 ) ) ;
#30393 = ADVANCED_FACE ( 'NONE', ( #22872 ), #27144, .T. ) ;
#30394 = CARTESIAN_POINT ( 'NONE',  ( 275.0000000000000000, -37.14999999999894698, -8.200000000002349410 ) ) ;
#30395 = ADVANCED_FACE ( 'NONE', ( #54709 ), #5240, .F. ) ;
#30396 = AXIS2_PLACEMENT_3D ( 'NONE', #47423, #46720, #14199 ) ;
#30397 = ORIENTED_EDGE ( 'NONE', *, *, #18313, .T. ) ;
#30398 = DIRECTION ( 'NONE',  ( 0.7071067811865550112, 0.7071067811865401342, 2.597868168706467285E-16 ) ) ;
#30399 = DIRECTION ( 'NONE',  ( 0.000000000000000000, 0.000000000000000000, 1.000000000000000000 ) ) ;
#30401 = ORIENTED_EDGE ( 'NONE', *, *, #3047, .F. ) ;
#30400 = ADVANCED_FACE ( 'NONE', ( #69924 ), #22190, .F. ) ;
#30402 = CARTESIAN_POINT ( 'NONE',  ( 9.562023737882814345, -7.969523737882825642, 54.00000000000000711 ) ) ;
#30403 = LINE ( 'NONE', #51969, #23041 ) ;
#30404 = LINE ( 'NONE', #41351, #58716 ) ;
#30405 = CARTESIAN_POINT ( 'NONE',  ( 4.186483450353335023, -12.00648345035338238, 195.0000000000000284 ) ) ;
#30406 = ORIENTED_EDGE ( 'NONE', *, *, #39275, .T. ) ;
#30407 = LINE ( 'NONE', #19441, #3272 ) ;
#30408 = ORIENTED_EDGE ( 'NONE', *, *, #36587, .T. ) ;
#30409 = ORIENTED_EDGE ( 'NONE', *, *, #41560, .T. ) ;
#30410 = ORIENTED_EDGE ( 'NONE', *, *, #56597, .F. ) ;
#30411 = DIRECTION ( 'NONE',  ( -0.000000000000000000, 3.673940397442059868E-16, -1.000000000000000000 ) ) ;
#30412 = AXIS2_PLACEMENT_3D ( 'NONE', #37542, #17011, #11351 ) ;
#30413 = DIRECTION ( 'NONE',  ( -1.000000000000000000, 2.602085213965213008E-15, 0.000000000000000000 ) ) ;
#30414 = CARTESIAN_POINT ( 'NONE',  ( 9.703773737882814387, 8.566576262117184370, 54.00000000000000711 ) ) ;
#30415 = EDGE_LOOP ( 'NONE', ( #15830, #46890, #5918, #53248 ) ) ;
#30416 = ORIENTED_EDGE ( 'NONE', *, *, #51801, .T. ) ;
#30417 = CARTESIAN_POINT ( 'NONE',  ( 283.0000000000000568, -25.50000000000000355, -14.74860679774999994 ) ) ;
#30418 = VECTOR ( 'NONE', #26772, 1000.000000000000000 ) ;
#30419 = ORIENTED_EDGE ( 'NONE', *, *, #27499, .F. ) ;
#30420 = VECTOR ( 'NONE', #19454, 1000.000000000000000 ) ;
#30421 = EDGE_LOOP ( 'NONE', ( #28310, #46331, #13475, #55720 ) ) ;
#30422 = ADVANCED_FACE ( 'NONE', ( #60338 ), #43750, .T. ) ;
#30423 = LINE ( 'NONE', #2839, #58647 ) ;
#30424 = CARTESIAN_POINT ( 'NONE',  ( 275.0000000000000000, -25.60000000000000142, -15.10000000000000142 ) ) ;
#30425 = DIRECTION ( 'NONE',  ( -1.000000000000000000, 0.000000000000000000, 0.000000000000000000 ) ) ;
#30426 = DIRECTION ( 'NONE',  ( 1.000000000000000000, -0.000000000000000000, 0.000000000000000000 ) ) ;
#30427 = ORIENTED_EDGE ( 'NONE', *, *, #7271, .T. ) ;
#30428 = CIRCLE ( 'NONE', #66557, 3.499999999999849454 ) ;
#30429 = DIRECTION ( 'NONE',  ( 0.000000000000000000, 0.000000000000000000, 1.000000000000000000 ) ) ;
#30431 = DIRECTION ( 'NONE',  ( 0.000000000000000000, -0.000000000000000000, 1.000000000000000000 ) ) ;
#30430 = CARTESIAN_POINT ( 'NONE',  ( 7.450000000000006395, 7.250000000000000888, -11.00000000000000000 ) ) ;
#30432 = ORIENTED_EDGE ( 'NONE', *, *, #48075, .F. ) ;
#30434 = ORIENTED_EDGE ( 'NONE', *, *, #11903, .T. ) ;
#30433 = CARTESIAN_POINT ( 'NONE',  ( -6.651770455163739548, 7.342976262117183239, 26.00000000000000711 ) ) ;
#30435 = EDGE_LOOP ( 'NONE', ( #23991, #55441, #18052, #8109 ) ) ;
#30436 = ORIENTED_EDGE ( 'NONE', *, *, #62437, .F. ) ;
#30437 = AXIS2_PLACEMENT_3D ( 'NONE', #8715, #4473, #29921 ) ;
#30438 = ADVANCED_FACE ( 'NONE', ( #270 ), #59315, .F. ) ;
#30439 = EDGE_CURVE ( 'NONE', #35258, #27638, #28470, .T. ) ;
#30440 = CARTESIAN_POINT ( 'NONE',  ( 7.250000000000005329, -7.449999999999998401, -9.000000000000001776 ) ) ;
#30441 = CIRCLE ( 'NONE', #69962, 0.2000000000000005107 ) ;
#30442 = DIRECTION ( 'NONE',  ( -0.000000000000000000, 0.000000000000000000, 1.000000000000000000 ) ) ;
#30443 = EDGE_CURVE ( 'NONE', #19389, #11295, #4782, .T. ) ;
#30444 = EDGE_LOOP ( 'NONE', ( #53914, #4027, #54289, #55655 ) ) ;
#30445 = ORIENTED_EDGE ( 'NONE', *, *, #24363, .T. ) ;
#30446 = AXIS2_PLACEMENT_3D ( 'NONE', #8056, #45898, #67487 ) ;
#30447 = CARTESIAN_POINT ( 'NONE',  ( -5.242976262117259978, 5.242976262117182706, 54.00000000000000711 ) ) ;
#30448 = CYLINDRICAL_SURFACE ( 'NONE', #66155, 0.1999999999999996503 ) ;
#30449 = VERTEX_POINT ( 'NONE', #44088 ) ;
#30450 = ORIENTED_EDGE ( 'NONE', *, *, #49994, .F. ) ;
#30451 = DIRECTION ( 'NONE',  ( 0.000000000000000000, 1.000000000000000000, 0.000000000000000000 ) ) ;
#30452 = DIRECTION ( 'NONE',  ( 0.000000000000000000, 0.000000000000000000, 1.000000000000000000 ) ) ;
#30453 = ORIENTED_EDGE ( 'NONE', *, *, #13336, .F. ) ;
#30454 = DIRECTION ( 'NONE',  ( 0.000000000000000000, 0.000000000000000000, 1.000000000000000000 ) ) ;
#30455 = CARTESIAN_POINT ( 'NONE',  ( 4.961189459950046121, 7.342976262117201003, 54.00000000000000711 ) ) ;
#30457 = VERTEX_POINT ( 'NONE', #55068 ) ;
#30456 = LINE ( 'NONE', #52028, #62254 ) ;
#30458 = ORIENTED_EDGE ( 'NONE', *, *, #6126, .T. ) ;
#30459 = CARTESIAN_POINT ( 'NONE',  ( 0.000000000000000000, -7.449999999999998401, -21.50000000000000000 ) ) ;
#30460 = PLANE ( 'NONE',  #8081 ) ;
#30461 = DIRECTION ( 'NONE',  ( 1.000000000000000000, 0.000000000000000000, 0.000000000000000000 ) ) ;
#30462 = DIRECTION ( 'NONE',  ( -1.000000000000000000, 1.047444401652939849E-14, -1.836970198721010706E-16 ) ) ;
#30463 = LINE ( 'NONE', #3598, #18109 ) ;
#30464 = LINE ( 'NONE', #69710, #61978 ) ;
#30465 = ORIENTED_EDGE ( 'NONE', *, *, #5588, .T. ) ;
#30466 = CARTESIAN_POINT ( 'NONE',  ( 176.4833316329832940, 0.000000000000000000, 280.6301873289890523 ) ) ;
#30467 = VECTOR ( 'NONE', #29176, 1000.000000000000000 ) ;
#30468 = CIRCLE ( 'NONE', #14378, 0.2000000000000005107 ) ;
#30469 = ORIENTED_EDGE ( 'NONE', *, *, #63697, .F. ) ;
#30470 = DIRECTION ( 'NONE',  ( 1.000000000000000000, 0.000000000000000000, 0.000000000000000000 ) ) ;
#30471 = VECTOR ( 'NONE', #45157, 1000.000000000000000 ) ;
#30472 = DIRECTION ( 'NONE',  ( 0.000000000000000000, 0.000000000000000000, -1.000000000000000000 ) ) ;
#30473 = ADVANCED_FACE ( 'NONE', ( #38819 ), #38155, .T. ) ;
#30474 = CARTESIAN_POINT ( 'NONE',  ( -7.415254214038345282, -3.006483450353401032, 455.0000000000000568 ) ) ;
#30475 = AXIS2_PLACEMENT_3D ( 'NONE', #3427, #31711, #53623 ) ;
#30476 = VERTEX_POINT ( 'NONE', #59705 ) ;
#30477 = CARTESIAN_POINT ( 'NONE',  ( -8.130476262117259267, 9.547976262117177981, 54.00000000000000711 ) ) ;
#30478 = FACE_OUTER_BOUND ( 'NONE', #38333, .T. ) ;
#30480 = ORIENTED_EDGE ( 'NONE', *, *, #36542, .T. ) ;
#30479 = EDGE_CURVE ( 'NONE', #44054, #7139, #17600, .T. ) ;
#30481 = CIRCLE ( 'NONE', #54173, 4.500000000000191847 ) ;
#30482 = FACE_OUTER_BOUND ( 'NONE', #51667, .T. ) ;
#30483 = AXIS2_PLACEMENT_3D ( 'NONE', #36134, #9984, #3624 ) ;
#30484 = CARTESIAN_POINT ( 'NONE',  ( 13.00000000000000178, -17.35230188589299871, -15.35019951917099945 ) ) ;
#30485 = EDGE_LOOP ( 'NONE', ( #30093, #28170, #39814, #48251 ) ) ;
#30486 = CARTESIAN_POINT ( 'NONE',  ( -16.89194109070750471, -5.000000000000000000, 26.25000000000000000 ) ) ;
#30487 = ORIENTED_EDGE ( 'NONE', *, *, #58938, .F. ) ;
#30488 = ORIENTED_EDGE ( 'NONE', *, *, #25989, .T. ) ;
#30489 = CARTESIAN_POINT ( 'NONE',  ( 7.250000000000005329, -7.249999999999998224, -12.50000000000000000 ) ) ;
#30490 = CIRCLE ( 'NONE', #21460, 25.39999999999999858 ) ;
#30491 = CARTESIAN_POINT ( 'NONE',  ( 11.50000000000000000, -11.50000000000100009, 15.00000000000084910 ) ) ;
#30492 = VECTOR ( 'NONE', #4455, 1000.000000000000000 ) ;
#30493 = CARTESIAN_POINT ( 'NONE',  ( -11.00000000000000000, -5.599999999999999645, 9.000000000000001776 ) ) ;
#30494 = DIRECTION ( 'NONE',  ( -0.000000000000000000, 0.000000000000000000, -1.000000000000000000 ) ) ;
#30495 = EDGE_CURVE ( 'NONE', #7103, #37166, #54410, .T. ) ;
#30496 = DIRECTION ( 'NONE',  ( 1.836970198721029934E-16, 1.836970198721010706E-16, -1.000000000000000000 ) ) ;
#30497 = ORIENTED_EDGE ( 'NONE', *, *, #11006, .T. ) ;
#30498 = ORIENTED_EDGE ( 'NONE', *, *, #14383, .F. ) ;
#30500 = ORIENTED_EDGE ( 'NONE', *, *, #66902, .T. ) ;
#30499 = DIRECTION ( 'NONE',  ( 0.000000000000000000, 0.000000000000000000, -1.000000000000000000 ) ) ;
#30501 = ORIENTED_EDGE ( 'NONE', *, *, #67057, .T. ) ;
#30502 = DIRECTION ( 'NONE',  ( 0.000000000000000000, 0.000000000000000000, -1.000000000000000000 ) ) ;
#30503 = LINE ( 'NONE', #52075, #422 ) ;
#30504 = CARTESIAN_POINT ( 'NONE',  ( 0.000000000000000000, -7.449999999999998401, -13.00000000000000178 ) ) ;
#30505 = AXIS2_PLACEMENT_3D ( 'NONE', #39804, #61372, #16268 ) ;
#30506 = CARTESIAN_POINT ( 'NONE',  ( -7.250000000000000888, -8.249999999999998224, -22.50000000000000000 ) ) ;
#30507 = CARTESIAN_POINT ( 'NONE',  ( 11.00000000000000000, -13.54524521594299991, -17.53999999999999915 ) ) ;
#30508 = DIRECTION ( 'NONE',  ( 0.000000000000000000, 0.000000000000000000, -1.000000000000000000 ) ) ;
#30509 = VERTEX_POINT ( 'NONE', #38490 ) ;
#30510 = EDGE_LOOP ( 'NONE', ( #2914, #48824, #46521, #64089 ) ) ;
#30511 = VERTEX_POINT ( 'NONE', #11590 ) ;
#30512 = ORIENTED_EDGE ( 'NONE', *, *, #33384, .F. ) ;
#30513 = AXIS2_PLACEMENT_3D ( 'NONE', #46022, #19844, #18795 ) ;
#30514 = CARTESIAN_POINT ( 'NONE',  ( -15.50000000000000000, -1.037157890325000054, 22.50000000000000000 ) ) ;
#30515 = CARTESIAN_POINT ( 'NONE',  ( -8.250000000000001776, -7.249999999999998224, -10.50000000000000000 ) ) ;
#30516 = VECTOR ( 'NONE', #31169, 1000.000000000000000 ) ;
#30517 = EDGE_CURVE ( 'NONE', #36887, #60315, #29580, .T. ) ;
#30518 = CARTESIAN_POINT ( 'NONE',  ( 85.07737089618308346, 47.95351654964650834, 318.7837994620735458 ) ) ;
#30519 = DIRECTION ( 'NONE',  ( -1.836970198721029934E-16, 1.836970198721036590E-16, -1.000000000000000000 ) ) ;
#30520 = AXIS2_PLACEMENT_3D ( 'NONE', #37372, #5193, #37716 ) ;
#30521 = ADVANCED_FACE ( 'NONE', ( #43430 ), #17251, .F. ) ;
#30522 = VERTEX_POINT ( 'NONE', #33173 ) ;
#30523 = VERTEX_POINT ( 'NONE', #65700 ) ;
#30524 = EDGE_CURVE ( 'NONE', #31048, #20952, #44459, .T. ) ;
#30525 = VERTEX_POINT ( 'NONE', #6308 ) ;
#30526 = VECTOR ( 'NONE', #20388, 1000.000000000000000 ) ;
#30527 = LINE ( 'NONE', #24873, #23773 ) ;
#30528 = ORIENTED_EDGE ( 'NONE', *, *, #28973, .T. ) ;
#30529 = EDGE_CURVE ( 'NONE', #61999, #61464, #32497, .T. ) ;
#30530 = VERTEX_POINT ( 'NONE', #27876 ) ;
#30531 = DIRECTION ( 'NONE',  ( -5.981805089575196197E-17, -1.000000000000000000, 0.000000000000000000 ) ) ;
#30532 = EDGE_LOOP ( 'NONE', ( #1146, #17042, #22934, #14889 ) ) ;
#30533 = ORIENTED_EDGE ( 'NONE', *, *, #56801, .F. ) ;
#30535 = EDGE_CURVE ( 'NONE', #55686, #8868, #9268, .T. ) ;
#30534 = PLANE ( 'NONE',  #32755 ) ;
#30536 = EDGE_CURVE ( 'NONE', #9391, #29478, #13789, .T. ) ;
#30537 = CIRCLE ( 'NONE', #51992, 0.2999999999998732569 ) ;
#30539 = VERTEX_POINT ( 'NONE', #49091 ) ;
#30538 = PLANE ( 'NONE',  #1796 ) ;
#30541 = ORIENTED_EDGE ( 'NONE', *, *, #22177, .T. ) ;
#30540 = EDGE_CURVE ( 'NONE', #45920, #57327, #22233, .T. ) ;
#30542 = CARTESIAN_POINT ( 'NONE',  ( -30.00000000000000000, -5.599999999999999645, -9.000000000000001776 ) ) ;
#30543 = DIRECTION ( 'NONE',  ( 0.000000000000000000, 0.000000000000000000, -1.000000000000000000 ) ) ;
#30544 = CARTESIAN_POINT ( 'NONE',  ( 7.250000000000004441, 7.450000000000001954, -24.50000000000000000 ) ) ;
#30546 = ORIENTED_EDGE ( 'NONE', *, *, #31604, .T. ) ;
#30545 = CARTESIAN_POINT ( 'NONE',  ( -13.00000000000000178, -15.50000000000000000, 20.05051025721700242 ) ) ;
#30547 = ORIENTED_EDGE ( 'NONE', *, *, #64485, .F. ) ;
#30548 = VECTOR ( 'NONE', #25165, 1000.000000000000000 ) ;
#30549 = CARTESIAN_POINT ( 'NONE',  ( 151.5599459900709860, 9.000000000000001776, 324.6739988703752715 ) ) ;
#30550 = VECTOR ( 'NONE', #52452, 1000.000000000000000 ) ;
#30551 = CYLINDRICAL_SURFACE ( 'NONE', #19347, 4.500000000000189182 ) ;
#30552 = CARTESIAN_POINT ( 'NONE',  ( 39.00000000000000000, 0.000000000000000000, 0.000000000000000000 ) ) ;
#30553 = PLANE ( 'NONE',  #67736 ) ;
#30554 = ORIENTED_EDGE ( 'NONE', *, *, #30254, .T. ) ;
#30555 = DIRECTION ( 'NONE',  ( -0.000000000000000000, -0.000000000000000000, 1.000000000000000000 ) ) ;
#30556 = LINE ( 'NONE', #58126, #49063 ) ;
#30557 = DIRECTION ( 'NONE',  ( 0.000000000000000000, 0.000000000000000000, -1.000000000000000000 ) ) ;
#30558 = AXIS2_PLACEMENT_3D ( 'NONE', #32629, #54204, #5761 ) ;
#30559 = VERTEX_POINT ( 'NONE', #6980 ) ;
#30560 = FACE_OUTER_BOUND ( 'NONE', #51445, .T. ) ;
#30561 = DIRECTION ( 'NONE',  ( 0.000000000000000000, 1.000000000000000000, 0.000000000000000000 ) ) ;
#30562 = DIRECTION ( 'NONE',  ( -1.000000000000000000, 8.728482790395504563E-15, 0.000000000000000000 ) ) ;
#30563 = ORIENTED_EDGE ( 'NONE', *, *, #47321, .T. ) ;
#30564 = CARTESIAN_POINT ( 'NONE',  ( 49.00000000000000000, 13.66939075806899950, 20.80000000000000426 ) ) ;
#30565 = AXIS2_PLACEMENT_3D ( 'NONE', #20457, #10541, #64297 ) ;
#30566 = DIRECTION ( 'NONE',  ( 0.7671651518153105309, -0.6414496315691445849, -0.000000000000000000 ) ) ;
#30567 = AXIS2_PLACEMENT_3D ( 'NONE', #4641, #25863, #26204 ) ;
#30568 = PLANE ( 'NONE',  #48509 ) ;
#30569 = ORIENTED_EDGE ( 'NONE', *, *, #37412, .T. ) ;
#30570 = CARTESIAN_POINT ( 'NONE',  ( -25.50000000000000355, -15.50000000000000000, 24.50000000000000000 ) ) ;
#30571 = CARTESIAN_POINT ( 'NONE',  ( 0.5000000000000000000, -42.50000000000000000, 26.50000000000000000 ) ) ;
#30572 = LINE ( 'NONE', #53213, #34190 ) ;
#30573 = AXIS2_PLACEMENT_3D ( 'NONE', #10925, #53722, #42751 ) ;
#30574 = CARTESIAN_POINT ( 'NONE',  ( -14.24999999999999822, -0.2715193793361453389, 22.98718409945082541 ) ) ;
#30575 = CARTESIAN_POINT ( 'NONE',  ( -7.250000000000000888, 8.250000000000001776, -26.00000000000001066 ) ) ;
#30577 = VERTEX_POINT ( 'NONE', #22907 ) ;
#30576 = EDGE_CURVE ( 'NONE', #26897, #61486, #50122, .T. ) ;
#30578 = CARTESIAN_POINT ( 'NONE',  ( 4.740315990920191958, 4.188533722949208560, 455.0000000000000568 ) ) ;
#30579 = FACE_OUTER_BOUND ( 'NONE', #33358, .T. ) ;
#30580 = DIRECTION ( 'NONE',  ( 0.000000000000000000, 0.000000000000000000, 1.000000000000000000 ) ) ;
#30581 = AXIS2_PLACEMENT_3D ( 'NONE', #60668, #585, #22503 ) ;
#30582 = AXIS2_PLACEMENT_3D ( 'NONE', #21896, #69295, #26173 ) ;
#30583 = DIRECTION ( 'NONE',  ( -1.000000000000000000, 0.000000000000000000, 0.000000000000000000 ) ) ;
#30584 = EDGE_CURVE ( 'NONE', #52916, #42765, #48752, .T. ) ;
#30585 = DIRECTION ( 'NONE',  ( 1.000000000000000000, 0.000000000000000000, 0.000000000000000000 ) ) ;
#30586 = VERTEX_POINT ( 'NONE', #43791 ) ;
#30588 = ORIENTED_EDGE ( 'NONE', *, *, #55458, .F. ) ;
#30587 = CARTESIAN_POINT ( 'NONE',  ( -7.813516549646711162, 11.99351654964660341, 195.0000000000000284 ) ) ;
#30589 = CIRCLE ( 'NONE', #29468, 24.99999999998784972 ) ;
#30590 = DIRECTION ( 'NONE',  ( 1.000000000000000000, 0.000000000000000000, 0.000000000000000000 ) ) ;
#30591 = DIRECTION ( 'NONE',  ( 0.000000000000000000, -0.000000000000000000, 1.000000000000000000 ) ) ;
#30592 = LINE ( 'NONE', #8675, #21759 ) ;
#30594 = EDGE_LOOP ( 'NONE', ( #23789, #38622, #5330, #48003 ) ) ;
#30593 = EDGE_CURVE ( 'NONE', #58343, #64845, #1676, .T. ) ;
#30595 = DIRECTION ( 'NONE',  ( 1.000000000000000000, -0.000000000000000000, -0.000000000000000000 ) ) ;
#30596 = EDGE_LOOP ( 'NONE', ( #42762, #50145, #22955, #68893 ) ) ;
#30597 = ORIENTED_EDGE ( 'NONE', *, *, #21496, .F. ) ;
#30598 = EDGE_CURVE ( 'NONE', #381, #52765, #23253, .T. ) ;
#30599 = ORIENTED_EDGE ( 'NONE', *, *, #8918, .T. ) ;
#30600 = ORIENTED_EDGE ( 'NONE', *, *, #5982, .T. ) ;
#30601 = FACE_OUTER_BOUND ( 'NONE', #66392, .T. ) ;
#30602 = DIRECTION ( 'NONE',  ( 0.000000000000000000, 0.000000000000000000, -1.000000000000000000 ) ) ;
#30603 = DIRECTION ( 'NONE',  ( -0.000000000000000000, -0.000000000000000000, -1.000000000000000000 ) ) ;
#30604 = CARTESIAN_POINT ( 'NONE',  ( 7.616533956692213003, -8.606483450353492159, 455.0000000000000568 ) ) ;
#30605 = AXIS2_PLACEMENT_3D ( 'NONE', #16539, #33819, #6271 ) ;
#30606 = EDGE_CURVE ( 'NONE', #1029, #16636, #27348, .T. ) ;
#30607 = ORIENTED_EDGE ( 'NONE', *, *, #18627, .T. ) ;
#30608 = EDGE_LOOP ( 'NONE', ( #53032, #14850, #32886, #54356 ) ) ;
#30609 = CARTESIAN_POINT ( 'NONE',  ( 3.677663764522614454, -4.149127210878770455, 54.00000000000000711 ) ) ;
#30610 = LINE ( 'NONE', #47572, #15865 ) ;
#30611 = ORIENTED_EDGE ( 'NONE', *, *, #40456, .F. ) ;
#30612 = ORIENTED_EDGE ( 'NONE', *, *, #54475, .F. ) ;
#30613 = ORIENTED_EDGE ( 'NONE', *, *, #45062, .F. ) ;
#30614 = ORIENTED_EDGE ( 'NONE', *, *, #18267, .T. ) ;
#30615 = CARTESIAN_POINT ( 'NONE',  ( -9.897976262117248680, -3.682023737882723857, 54.00000000000000711 ) ) ;
#30616 = EDGE_CURVE ( 'NONE', #67044, #56517, #37797, .T. ) ;
#30617 = VECTOR ( 'NONE', #39658, 1000.000000000000000 ) ;
#30619 = ORIENTED_EDGE ( 'NONE', *, *, #55873, .T. ) ;
#30618 = CARTESIAN_POINT ( 'NONE',  ( 9.804883450353454322, 10.19191654964656912, 455.0000000000000568 ) ) ;
#30620 = EDGE_CURVE ( 'NONE', #3378, #67312, #62343, .T. ) ;
#30621 = DIRECTION ( 'NONE',  ( 1.000000000000000000, -0.000000000000000000, 0.000000000000000000 ) ) ;
#30622 = AXIS2_PLACEMENT_3D ( 'NONE', #37951, #5438, #43242 ) ;
#30623 = PLANE ( 'NONE',  #32881 ) ;
#30624 = ORIENTED_EDGE ( 'NONE', *, *, #29118, .T. ) ;
#30625 = CIRCLE ( 'NONE', #2253, 0.1999999999999987899 ) ;
#30626 = VERTEX_POINT ( 'NONE', #28897 ) ;
#30627 = EDGE_CURVE ( 'NONE', #35155, #56406, #30716, .T. ) ;
#30628 = CIRCLE ( 'NONE', #44142, 0.1999999999999996503 ) ;
#30629 = AXIS2_PLACEMENT_3D ( 'NONE', #38095, #47644, #43027 ) ;
#30630 = DIRECTION ( 'NONE',  ( -0.000000000000000000, 3.673940397442059868E-16, -1.000000000000000000 ) ) ;
#30631 = DIRECTION ( 'NONE',  ( 0.000000000000000000, -1.000000000000000000, -0.000000000000000000 ) ) ;
#30632 = ORIENTED_EDGE ( 'NONE', *, *, #47918, .F. ) ;
#30633 = AXIS2_PLACEMENT_3D ( 'NONE', #63383, #19891, #41098 ) ;
#30634 = CIRCLE ( 'NONE', #9191, 1.000000000000000000 ) ;
#30635 = CARTESIAN_POINT ( 'NONE',  ( 41.09999999999999432, 21.00000000000000000, -13.98999642601811999 ) ) ;
#30636 = CARTESIAN_POINT ( 'NONE',  ( 152.0064834503532722, 2.160375375128253950, 5.000000000000000000 ) ) ;
#30637 = CARTESIAN_POINT ( 'NONE',  ( 29.50000000000000355, -11.50000000000100009, 15.00000000000084910 ) ) ;
#30638 = ORIENTED_EDGE ( 'NONE', *, *, #44602, .F. ) ;
#30639 = CARTESIAN_POINT ( 'NONE',  ( 151.5599459900709860, 9.000000000000001776, 324.6739988703752715 ) ) ;
#30640 = DIRECTION ( 'NONE',  ( 1.000000000000000000, 0.000000000000000000, 0.000000000000000000 ) ) ;
#30641 = CARTESIAN_POINT ( 'NONE',  ( 6.364920264886889001, 6.822336235477383326, 54.00000000000000711 ) ) ;
#30642 = CARTESIAN_POINT ( 'NONE',  ( 111.9257688011041836, 0.000000000000000000, 281.4830310981151911 ) ) ;
#30643 = EDGE_CURVE ( 'NONE', #14855, #42529, #18282, .T. ) ;
#30644 = DIRECTION ( 'NONE',  ( 0.000000000000000000, 0.000000000000000000, -1.000000000000000000 ) ) ;
#30645 = ORIENTED_EDGE ( 'NONE', *, *, #61879, .T. ) ;
#30646 = DIRECTION ( 'NONE',  ( -0.7071067811865549002, -0.7071067811865401342, -2.597868168706466792E-16 ) ) ;
#30647 = DIRECTION ( 'NONE',  ( -0.000000000000000000, 1.000000000000000000, -0.000000000000000000 ) ) ;
#30648 = DIRECTION ( 'NONE',  ( -1.000000000000000000, 3.491481338843133355E-15, 1.836970198721036344E-16 ) ) ;
#30649 = EDGE_CURVE ( 'NONE', #48624, #33817, #18633, .T. ) ;
#30650 = DIRECTION ( 'NONE',  ( 0.000000000000000000, -1.000000000000000000, 0.000000000000000000 ) ) ;
#30651 = VECTOR ( 'NONE', #66695, 1000.000000000000000 ) ;
#30652 = CARTESIAN_POINT ( 'NONE',  ( -1.466476262117310414, -8.612468434717262866, 26.00000000000000711 ) ) ;
#30653 = CARTESIAN_POINT ( 'NONE',  ( -9.897976262117285984, -6.657023737882751924, 26.00000000000000000 ) ) ;
#30654 = EDGE_CURVE ( 'NONE', #35302, #48024, #24088, .T. ) ;
#30655 = CARTESIAN_POINT ( 'NONE',  ( 7.250000000000005329, 7.250000000000000888, -21.00000000000000000 ) ) ;
#30656 = CARTESIAN_POINT ( 'NONE',  ( 38.90000000000000568, -21.00000000000000000, 13.86939075806900057 ) ) ;
#30657 = ORIENTED_EDGE ( 'NONE', *, *, #45707, .F. ) ;
#30658 = CARTESIAN_POINT ( 'NONE',  ( 7.000000000000000000, -23.65000000000000568, -12.40000000000000213 ) ) ;
#30659 = EDGE_CURVE ( 'NONE', #64180, #22939, #36518, .T. ) ;
#30660 = FACE_OUTER_BOUND ( 'NONE', #44450, .T. ) ;
#30661 = VERTEX_POINT ( 'NONE', #2037 ) ;
#30662 = CARTESIAN_POINT ( 'NONE',  ( 4.456444791733522252E-16, 7.450000000000002842, -20.50000000000000000 ) ) ;
#30663 = FACE_OUTER_BOUND ( 'NONE', #37767, .T. ) ;
#30664 = CARTESIAN_POINT ( 'NONE',  ( 7.357023737882817827, -3.848229544836346605, 54.00000000000000711 ) ) ;
#30665 = DIRECTION ( 'NONE',  ( -0.5000000000000004441, 0.8660254037844383745, 3.181725716174720005E-16 ) ) ;
#30666 = EDGE_CURVE ( 'NONE', #32098, #868, #39505, .T. ) ;
#30667 = PLANE ( 'NONE',  #15848 ) ;
#30668 = VECTOR ( 'NONE', #47079, 1000.000000000000000 ) ;
#30669 = VERTEX_POINT ( 'NONE', #40204 ) ;
#30670 = DIRECTION ( 'NONE',  ( 0.000000000000000000, -0.6787500000000000755, 0.7343694148723789450 ) ) ;
#30671 = CIRCLE ( 'NONE', #201, 0.2000000000000005107 ) ;
#30672 = ORIENTED_EDGE ( 'NONE', *, *, #20156, .T. ) ;
#30673 = DIRECTION ( 'NONE',  ( 0.000000000000000000, 0.000000000000000000, 1.000000000000000000 ) ) ;
#30674 = CARTESIAN_POINT ( 'NONE',  ( 14.99999999999999822, -42.00000000000000000, -15.10000000000000142 ) ) ;
#30676 = ORIENTED_EDGE ( 'NONE', *, *, #39294, .T. ) ;
#30675 = EDGE_CURVE ( 'NONE', #35475, #32206, #17176, .T. ) ;
#30677 = CARTESIAN_POINT ( 'NONE',  ( 29.50000000000000355, -12.00000000000000000, -11.00000000000000000 ) ) ;
#30678 = ADVANCED_FACE ( 'NONE', ( #7321 ), #46207, .F. ) ;
#30679 = CARTESIAN_POINT ( 'NONE',  ( 4.456444791733522252E-16, 7.450000000000002842, -14.50000000000000000 ) ) ;
#30680 = ORIENTED_EDGE ( 'NONE', *, *, #45695, .T. ) ;
#30682 = EDGE_CURVE ( 'NONE', #37044, #11521, #13686, .T. ) ;
#30681 = AXIS2_PLACEMENT_3D ( 'NONE', #36683, #48340, #47987 ) ;
#30683 = ADVANCED_FACE ( 'NONE', ( #45154 ), #67782, .T. ) ;
#30684 = AXIS2_PLACEMENT_3D ( 'NONE', #30763, #62225, #13786 ) ;
#30685 = CARTESIAN_POINT ( 'NONE',  ( 7.532023737882778569, 3.834182069070700916, 26.00000000000000711 ) ) ;
#30686 = VERTEX_POINT ( 'NONE', #66726 ) ;
#30687 = ORIENTED_EDGE ( 'NONE', *, *, #25215, .F. ) ;
#30688 = DIRECTION ( 'NONE',  ( 0.000000000000000000, 0.000000000000000000, 1.000000000000000000 ) ) ;
#30689 = EDGE_LOOP ( 'NONE', ( #22735, #39607, #16096, #43390 ) ) ;
#30690 = VERTEX_POINT ( 'NONE', #67078 ) ;
#30691 = ADVANCED_FACE ( 'NONE', ( #8371 ), #13337, .T. ) ;
#30692 = CARTESIAN_POINT ( 'NONE',  ( 2.906483450353420039, 10.91351654964658913, 455.0000000000000568 ) ) ;
#30693 = FACE_OUTER_BOUND ( 'NONE', #8704, .T. ) ;
#30694 = DIRECTION ( 'NONE',  ( 1.836970198721029934E-16, 1.836970198721010706E-16, -1.000000000000000000 ) ) ;
#30695 = ORIENTED_EDGE ( 'NONE', *, *, #59422, .F. ) ;
#30696 = CARTESIAN_POINT ( 'NONE',  ( 39.00000000000000000, 0.000000000000000000, 5.000000000000000000 ) ) ;
#30697 = AXIS2_PLACEMENT_3D ( 'NONE', #66471, #54836, #49865 ) ;
#30699 = CARTESIAN_POINT ( 'NONE',  ( 283.0000000000000568, -32.44999999999905071, 12.69999999999999929 ) ) ;
#30698 = FACE_OUTER_BOUND ( 'NONE', #21350, .T. ) ;
#30700 = ORIENTED_EDGE ( 'NONE', *, *, #47931, .T. ) ;
#30702 = ORIENTED_EDGE ( 'NONE', *, *, #2025, .F. ) ;
#30701 = DIRECTION ( 'NONE',  ( 0.000000000000000000, 0.000000000000000000, -1.000000000000000000 ) ) ;
#30703 = ORIENTED_EDGE ( 'NONE', *, *, #2086, .F. ) ;
#30704 = SHAPE_DEFINITION_REPRESENTATION ( #28433, #15926 ) ;
#30705 = DIRECTION ( 'NONE',  ( -1.836970198721029934E-16, 1.836970198721036344E-16, -1.000000000000000000 ) ) ;
#30706 = EDGE_CURVE ( 'NONE', #97, #37440, #11669, .T. ) ;
#30708 = ORIENTED_EDGE ( 'NONE', *, *, #15275, .F. ) ;
#30707 = CARTESIAN_POINT ( 'NONE',  ( 16.75000000000000000, -0.2038245569916320166, -21.77831216351300014 ) ) ;
#30709 = EDGE_CURVE ( 'NONE', #15085, #59830, #2724, .T. ) ;
#30710 = LINE ( 'NONE', #19044, #39308 ) ;
#30711 = CARTESIAN_POINT ( 'NONE',  ( -6.642976262117334940, -10.31452373788278898, 54.00000000000000711 ) ) ;
#30712 = AXIS2_PLACEMENT_3D ( 'NONE', #46447, #68022, #35130 ) ;
#30713 = EDGE_LOOP ( 'NONE', ( #10340, #57073, #41244, #36903 ) ) ;
#30714 = VERTEX_POINT ( 'NONE', #35233 ) ;
#30715 = CARTESIAN_POINT ( 'NONE',  ( 41.09999999999999432, 20.60000000000000142, -13.86939075806900057 ) ) ;
#30716 = CIRCLE ( 'NONE', #54605, 1.000000000000000000 ) ;
#30717 = ORIENTED_EDGE ( 'NONE', *, *, #20368, .T. ) ;
#30718 = DIRECTION ( 'NONE',  ( 1.000000000000000000, 0.000000000000000000, 0.000000000000000000 ) ) ;
#30719 = DIRECTION ( 'NONE',  ( -0.000000000000000000, -0.000000000000000000, -1.000000000000000000 ) ) ;
#30720 = AXIS2_PLACEMENT_3D ( 'NONE', #55166, #44888, #67151 ) ;
#30721 = ORIENTED_EDGE ( 'NONE', *, *, #7562, .F. ) ;
#30722 = DIRECTION ( 'NONE',  ( 1.000000000000000000, -1.047444401652939849E-14, 1.836970198721010706E-16 ) ) ;
#30723 = CARTESIAN_POINT ( 'NONE',  ( 4.396432944014527777, -8.406483450353478659, 455.0000000000000568 ) ) ;
#30725 = ORIENTED_EDGE ( 'NONE', *, *, #13497, .T. ) ;
#30724 = CARTESIAN_POINT ( 'NONE',  ( 7.900000000000000355, -18.00000000000000355, -21.00000000000000000 ) ) ;
#30727 = ORIENTED_EDGE ( 'NONE', *, *, #51408, .F. ) ;
#30726 = LINE ( 'NONE', #62534, #27564 ) ;
#30728 = CYLINDRICAL_SURFACE ( 'NONE', #40782, 0.1749999999999998224 ) ;
#30729 = CARTESIAN_POINT ( 'NONE',  ( -7.259684009079916400, -4.201500623655988420, 195.0000000000000284 ) ) ;
#30730 = CARTESIAN_POINT ( 'NONE',  ( -11.75000000000000000, -5.000000000000000000, -11.75000000000000000 ) ) ;
#30731 = CIRCLE ( 'NONE', #46513, 0.2000000000000005107 ) ;
#30732 = LINE ( 'NONE', #52300, #43003 ) ;
#30733 = DIRECTION ( 'NONE',  ( 0.000000000000000000, 1.000000000000000000, 0.000000000000000000 ) ) ;
#30734 = VERTEX_POINT ( 'NONE', #45865 ) ;
#30735 = PLANE ( 'NONE',  #50400 ) ;
#30736 = CARTESIAN_POINT ( 'NONE',  ( -4.383466043307858939, 8.593516549646588842, 455.0000000000000568 ) ) ;
#30737 = DIRECTION ( 'NONE',  ( 1.000000000000000000, -5.163402228214835223E-15, -1.836970198721039302E-16 ) ) ;
#30738 = EDGE_CURVE ( 'NONE', #12110, #58380, #14032, .T. ) ;
#30740 = ORIENTED_EDGE ( 'NONE', *, *, #16015, .F. ) ;
#30739 = DIRECTION ( 'NONE',  ( -0.7671651518153006499, 0.6414496315691565753, -0.000000000000000000 ) ) ;
#30741 = CARTESIAN_POINT ( 'NONE',  ( 283.0000000000000568, -25.00000000000000000, 17.50000000000000000 ) ) ;
#30742 = AXIS2_PLACEMENT_3D ( 'NONE', #15564, #15891, #42760 ) ;
#30743 = DIRECTION ( 'NONE',  ( -0.000000000000000000, 1.000000000000000000, -0.000000000000000000 ) ) ;
#30744 = EDGE_CURVE ( 'NONE', #64822, #22435, #18994, .T. ) ;
#30745 = AXIS2_PLACEMENT_3D ( 'NONE', #44809, #39503, #34189 ) ;
#30746 = CARTESIAN_POINT ( 'NONE',  ( -10.30047626211724499, -3.857023737882708581, 26.00000000000000000 ) ) ;
#30747 = ORIENTED_EDGE ( 'NONE', *, *, #43218, .T. ) ;
#30748 = DIRECTION ( 'NONE',  ( 1.836970198721029934E-16, 1.836970198721010706E-16, -1.000000000000000000 ) ) ;
#30749 = EDGE_CURVE ( 'NONE', #43736, #33316, #25002, .T. ) ;
#30750 = CARTESIAN_POINT ( 'NONE',  ( 39.90000000000000568, 20.60000000000000142, -13.86939075806900057 ) ) ;
#30751 = EDGE_CURVE ( 'NONE', #14970, #47719, #51528, .T. ) ;
#30752 = ORIENTED_EDGE ( 'NONE', *, *, #6506, .T. ) ;
#30753 = LINE ( 'NONE', #36764, #51490 ) ;
#30754 = DIRECTION ( 'NONE',  ( 9.912705577010386883E-15, 1.000000000000000000, 0.000000000000000000 ) ) ;
#30755 = FACE_OUTER_BOUND ( 'NONE', #7434, .T. ) ;
#30756 = EDGE_CURVE ( 'NONE', #14841, #28718, #21690, .T. ) ;
#30757 = EDGE_CURVE ( 'NONE', #55302, #63213, #66877, .T. ) ;
#30758 = CARTESIAN_POINT ( 'NONE',  ( 30.00000000000000000, -11.70000000000000284, 12.50000000000000000 ) ) ;
#30759 = LINE ( 'NONE', #30405, #53472 ) ;
#30760 = VERTEX_POINT ( 'NONE', #58229 ) ;
#30761 = CARTESIAN_POINT ( 'NONE',  ( 11.00000000000000000, -11.50000000000000000, -15.00000000000000000 ) ) ;
#30762 = ORIENTED_EDGE ( 'NONE', *, *, #19041, .T. ) ;
#30763 = CARTESIAN_POINT ( 'NONE',  ( 25.50000000000000355, -5.200000000000001066, 22.50000000000000000 ) ) ;
#30764 = ORIENTED_EDGE ( 'NONE', *, *, #65775, .T. ) ;
#30765 = DIRECTION ( 'NONE',  ( 0.000000000000000000, 0.000000000000000000, 1.000000000000000000 ) ) ;
#30766 = VECTOR ( 'NONE', #10485, 1000.000000000000000 ) ;
#30767 = CARTESIAN_POINT ( 'NONE',  ( -7.450000000000001954, -7.249999999999998224, -24.50000000000000000 ) ) ;
#30768 = DIRECTION ( 'NONE',  ( 0.000000000000000000, 0.000000000000000000, -1.000000000000000000 ) ) ;
#30769 = EDGE_LOOP ( 'NONE', ( #51841, #45992, #64361, #66176 ) ) ;
#30770 = ORIENTED_EDGE ( 'NONE', *, *, #1366, .T. ) ;
#30771 = VECTOR ( 'NONE', #66016, 1000.000000000000000 ) ;
#30772 = PLANE ( 'NONE',  #41990 ) ;
#30773 = ORIENTED_EDGE ( 'NONE', *, *, #64991, .T. ) ;
#30774 = ORIENTED_EDGE ( 'NONE', *, *, #18587, .F. ) ;
#30775 = CARTESIAN_POINT ( 'NONE',  ( 11.34648345035338046, -1.090483450353491035, 455.0000000000000568 ) ) ;
#30776 = DIRECTION ( 'NONE',  ( 0.000000000000000000, 0.000000000000000000, -1.000000000000000000 ) ) ;
#30777 = CARTESIAN_POINT ( 'NONE',  ( -16.33757311576526305, -0.3152598339554808504, -21.54019739087904384 ) ) ;
#30778 = FACE_OUTER_BOUND ( 'NONE', #52272, .T. ) ;
#30779 = ORIENTED_EDGE ( 'NONE', *, *, #39865, .T. ) ;
#30780 = DIRECTION ( 'NONE',  ( -1.084202172485504434E-16, 1.000000000000000000, 0.000000000000000000 ) ) ;
#30782 = DIRECTION ( 'NONE',  ( 0.000000000000000000, 1.000000000000000000, 3.673940397442059868E-16 ) ) ;
#30781 = DIRECTION ( 'NONE',  ( -1.000000000000000000, 0.000000000000000000, 0.000000000000000000 ) ) ;
#30783 = ORIENTED_EDGE ( 'NONE', *, *, #67403, .F. ) ;
#30785 = ORIENTED_EDGE ( 'NONE', *, *, #1284, .F. ) ;
#30784 = DIRECTION ( 'NONE',  ( 0.000000000000000000, 0.000000000000000000, -1.000000000000000000 ) ) ;
#30786 = VERTEX_POINT ( 'NONE', #5190 ) ;
#30787 = VECTOR ( 'NONE', #8586, 1000.000000000000114 ) ;
#30788 = LINE ( 'NONE', #56603, #44542 ) ;
#30789 = ADVANCED_FACE ( 'NONE', ( #68133 ), #47272, .T. ) ;
#30790 = LINE ( 'NONE', #69319, #63160 ) ;
#30791 = ORIENTED_EDGE ( 'NONE', *, *, #20370, .F. ) ;
#30792 = VERTEX_POINT ( 'NONE', #26404 ) ;
#30793 = EDGE_CURVE ( 'NONE', #17426, #48590, #64244, .T. ) ;
#30794 = VECTOR ( 'NONE', #58585, 1000.000000000000000 ) ;
#30796 = DIRECTION ( 'NONE',  ( 0.000000000000000000, 0.000000000000000000, -1.000000000000000000 ) ) ;
#30795 = VECTOR ( 'NONE', #3621, 1000.000000000000000 ) ;
#30797 = FACE_OUTER_BOUND ( 'NONE', #4906, .T. ) ;
#30798 = VERTEX_POINT ( 'NONE', #35958 ) ;
#30799 = VERTEX_POINT ( 'NONE', #46905 ) ;
#30800 = CARTESIAN_POINT ( 'NONE',  ( -7.798499376344067535, 4.727349090213367688, 195.0000000000000284 ) ) ;
#30801 = VECTOR ( 'NONE', #29668, 1000.000000000000000 ) ;
#30802 = CARTESIAN_POINT ( 'NONE',  ( 10.00000000000000000, -18.00000000000000355, 21.00000000000000000 ) ) ;
#30803 = ORIENTED_EDGE ( 'NONE', *, *, #37308, .F. ) ;
#30804 = LINE ( 'NONE', #36099, #52700 ) ;
#30805 = CARTESIAN_POINT ( 'NONE',  ( 7.250000000000004441, 7.450000000000001954, -9.500000000000001776 ) ) ;
#30807 = ORIENTED_EDGE ( 'NONE', *, *, #13798, .T. ) ;
#30806 = DIRECTION ( 'NONE',  ( 0.000000000000000000, 0.000000000000000000, -1.000000000000000000 ) ) ;
#30808 = ORIENTED_EDGE ( 'NONE', *, *, #1680, .T. ) ;
#30809 = LINE ( 'NONE', #14193, #16323 ) ;
#30810 = DIRECTION ( 'NONE',  ( -1.000000000000000000, 1.671920889371702854E-15, 6.142537696789956391E-31 ) ) ;
#30811 = AXIS2_PLACEMENT_3D ( 'NONE', #69815, #59548, #64509 ) ;
#30812 = DIRECTION ( 'NONE',  ( 0.000000000000000000, 0.000000000000000000, 1.000000000000000000 ) ) ;
#30813 = DIRECTION ( 'NONE',  ( 0.000000000000000000, 3.673940397442059868E-16, -1.000000000000000000 ) ) ;
#30814 = DIRECTION ( 'NONE',  ( 0.000000000000000000, 0.000000000000000000, 1.000000000000000000 ) ) ;
#30815 = DIRECTION ( 'NONE',  ( 0.000000000000000000, 0.7071067811865474617, 0.7071067811865474617 ) ) ;
#30816 = AXIS2_PLACEMENT_3D ( 'NONE', #47261, #55012, #45064 ) ;
#30817 = ORIENTED_EDGE ( 'NONE', *, *, #14393, .T. ) ;
#30818 = CARTESIAN_POINT ( 'NONE',  ( 39.00000000000000000, -14.48845687959340012, -21.00000000000000000 ) ) ;
#30820 = ORIENTED_EDGE ( 'NONE', *, *, #32340, .F. ) ;
#30819 = PLANE ( 'NONE',  #27730 ) ;
#30821 = EDGE_CURVE ( 'NONE', #59076, #28788, #14748, .T. ) ;
#30822 = DIRECTION ( 'NONE',  ( -1.048062100069321163E-14, -1.000000000000000000, 0.000000000000000000 ) ) ;
#30823 = B_SPLINE_CURVE_WITH_KNOTS ( 'NONE', 3,
 ( #62744, #30574, #31985, #9358, #25635, #21011 ),
 .UNSPECIFIED., .F., .F.,
 ( 4, 2, 4 ),
 ( 1.820537833122031213, 2.555393473688635453, 3.290249114255239693 ),
 .UNSPECIFIED. ) ;
#30824 = CARTESIAN_POINT ( 'NONE',  ( -7.250000000000000888, 8.750000000000001776, -26.00000000000001066 ) ) ;
#30825 = VECTOR ( 'NONE', #59051, 1000.000000000000000 ) ;
#30826 = CARTESIAN_POINT ( 'NONE',  ( -18.85410196625000268, -15.50000000000000000, 21.50000000000000000 ) ) ;
#30827 = VERTEX_POINT ( 'NONE', #52585 ) ;
#30828 = CARTESIAN_POINT ( 'NONE',  ( -16.75000000000000355, -0.2715193793361416197, 22.01281590054916748 ) ) ;
#30829 = EDGE_CURVE ( 'NONE', #35354, #45642, #9088, .T. ) ;
#30830 = CARTESIAN_POINT ( 'NONE',  ( -11.00000000000000000, -5.200000000000001066, 26.59999999999999787 ) ) ;
#30831 = EDGE_CURVE ( 'NONE', #21095, #59900, #26758, .T. ) ;
#30832 = ORIENTED_EDGE ( 'NONE', *, *, #11395, .F. ) ;
#30833 = CARTESIAN_POINT ( 'NONE',  ( 49.00000000000000000, -14.06939075806900163, -20.80000000000000426 ) ) ;
#30834 = DIRECTION ( 'NONE',  ( 0.000000000000000000, 0.000000000000000000, 1.000000000000000000 ) ) ;
#30835 = ADVANCED_FACE ( 'NONE', ( #37369 ), #57871, .F. ) ;
#30836 = ADVANCED_FACE ( 'NONE', ( #19678 ), #9438, .F. ) ;
#30837 = DIRECTION ( 'NONE',  ( 1.000000000000000000, -5.981805089575196197E-17, 0.000000000000000000 ) ) ;
#30838 = EDGE_CURVE ( 'NONE', #16525, #8213, #12662, .T. ) ;
#30839 = ORIENTED_EDGE ( 'NONE', *, *, #1483, .F. ) ;
#30840 = CARTESIAN_POINT ( 'NONE',  ( -1.677516549646825839, -10.74648345035347141, 455.0000000000000568 ) ) ;
#30841 = VERTEX_POINT ( 'NONE', #4150 ) ;
#30842 = ORIENTED_EDGE ( 'NONE', *, *, #65408, .T. ) ;
#30843 = CIRCLE ( 'NONE', #69254, 0.2000000000000005107 ) ;
#30844 = DIRECTION ( 'NONE',  ( -0.6414496315691592399, -0.7671651518152985405, 0.000000000000000000 ) ) ;
#30845 = DIRECTION ( 'NONE',  ( 0.000000000000000000, 0.000000000000000000, 1.000000000000000000 ) ) ;
#30846 = DIRECTION ( 'NONE',  ( 1.000000000000000000, -0.000000000000000000, -0.000000000000000000 ) ) ;
#30847 = VECTOR ( 'NONE', #60386, 1000.000000000000000 ) ;
#30848 = CARTESIAN_POINT ( 'NONE',  ( 6.364920264886885448, -3.677663764522628664, 54.00000000000000711 ) ) ;
#30849 = AXIS2_PLACEMENT_3D ( 'NONE', #24366, #63607, #24717 ) ;
#30850 = AXIS2_PLACEMENT_3D ( 'NONE', #63167, #20729, #62447 ) ;
#30851 = DIRECTION ( 'NONE',  ( -1.836970198721029934E-16, 1.836970198721036344E-16, -1.000000000000000000 ) ) ;
#30852 = ORIENTED_EDGE ( 'NONE', *, *, #1802, .F. ) ;
#30853 = ORIENTED_EDGE ( 'NONE', *, *, #62466, .T. ) ;
#30854 = ORIENTED_EDGE ( 'NONE', *, *, #63904, .F. ) ;
#30855 = EDGE_LOOP ( 'NONE', ( #19135, #17814, #49750, #65865 ) ) ;
#30856 = CARTESIAN_POINT ( 'NONE',  ( 7.616533956692213003, -8.606483450353396236, 195.0000000000000284 ) ) ;
#30857 = VECTOR ( 'NONE', #21590, 1000.000000000000000 ) ;
#30858 = CARTESIAN_POINT ( 'NONE',  ( -29.50000000000000355, -12.00000000000000000, 11.00000000000000000 ) ) ;
#30859 = DIRECTION ( 'NONE',  ( -0.000000000000000000, -0.000000000000000000, 1.000000000000000000 ) ) ;
#30860 = FACE_BOUND ( 'NONE', #59431, .T. ) ;
#30861 = DIRECTION ( 'NONE',  ( 0.000000000000000000, 0.000000000000000000, 1.000000000000000000 ) ) ;
#30863 = LINE ( 'NONE', #13628, #37973 ) ;
#30862 = CARTESIAN_POINT ( 'NONE',  ( 283.0000000000000568, -42.00000000000000000, 7.000000000000000000 ) ) ;
#30864 = AXIS2_PLACEMENT_3D ( 'NONE', #40749, #42145, #41798 ) ;
#30865 = ORIENTED_EDGE ( 'NONE', *, *, #21935, .F. ) ;
#30866 = ORIENTED_EDGE ( 'NONE', *, *, #5944, .T. ) ;
#30867 = VERTEX_POINT ( 'NONE', #69537 ) ;
#30868 = ORIENTED_EDGE ( 'NONE', *, *, #27202, .F. ) ;
#30869 = DIRECTION ( 'NONE',  ( 0.000000000000000000, 0.5000000000000189848, 0.8660254037844277164 ) ) ;
#30870 = VECTOR ( 'NONE', #26807, 1000.000000000000000 ) ;
#30871 = DIRECTION ( 'NONE',  ( -1.836970198721029934E-16, 1.836970198721036344E-16, -1.000000000000000000 ) ) ;
#30872 = DIRECTION ( 'NONE',  ( 0.000000000000000000, 0.000000000000000000, 1.000000000000000000 ) ) ;
#30873 = CARTESIAN_POINT ( 'NONE',  ( -7.259684009079983902, -7.811466277050722162, 195.0000000000000284 ) ) ;
#30874 = ORIENTED_EDGE ( 'NONE', *, *, #31873, .F. ) ;
#30875 = ORIENTED_EDGE ( 'NONE', *, *, #7672, .T. ) ;
#30876 = ORIENTED_EDGE ( 'NONE', *, *, #19809, .F. ) ;
#30877 = VECTOR ( 'NONE', #1722, 1000.000000000000114 ) ;
#30878 = EDGE_CURVE ( 'NONE', #2772, #15483, #22880, .T. ) ;
#30879 = EDGE_CURVE ( 'NONE', #38207, #20840, #68843, .T. ) ;
#30880 = FACE_OUTER_BOUND ( 'NONE', #11209, .T. ) ;
#30881 = EDGE_LOOP ( 'NONE', ( #14138, #26447, #16664, #37141, #53964, #10677, #32371, #52453 ) ) ;
#30882 = ORIENTED_EDGE ( 'NONE', *, *, #58403, .F. ) ;
#30883 = DIRECTION ( 'NONE',  ( 0.000000000000000000, 0.000000000000000000, 1.000000000000000000 ) ) ;
#30884 = EDGE_CURVE ( 'NONE', #2028, #50683, #49976, .T. ) ;
#30885 = ORIENTED_EDGE ( 'NONE', *, *, #62173, .T. ) ;
#30886 = ORIENTED_EDGE ( 'NONE', *, *, #56149, .F. ) ;
#30887 = CARTESIAN_POINT ( 'NONE',  ( -17.00000000000000000, -17.50000000000000000, -19.33772233983200195 ) ) ;
#30889 = VERTEX_POINT ( 'NONE', #30656 ) ;
#30888 = CARTESIAN_POINT ( 'NONE',  ( 49.00000000000000000, -0.7500000000000000000, -3.929058411375429216 ) ) ;
#30890 = ORIENTED_EDGE ( 'NONE', *, *, #20555, .F. ) ;
#30891 = VECTOR ( 'NONE', #31888, 1000.000000000000000 ) ;
#30893 = LINE ( 'NONE', #36913, #61166 ) ;
#30892 = VECTOR ( 'NONE', #10859, 1000.000000000000000 ) ;
#30894 = DIRECTION ( 'NONE',  ( -1.836970198721029934E-16, 1.836970198721036344E-16, -1.000000000000000000 ) ) ;
#30896 = EDGE_LOOP ( 'NONE', ( #193, #30703, #22458, #63580 ) ) ;
#30895 = LINE ( 'NONE', #25604, #53836 ) ;
#30898 = EDGE_LOOP ( 'NONE', ( #61348, #67285, #599, #47377 ) ) ;
#30897 = VECTOR ( 'NONE', #2735, 1000.000000000000000 ) ;
#30899 = CARTESIAN_POINT ( 'NONE',  ( -28.00000000000000000, -16.64230188589299786, 14.64519951917100116 ) ) ;
#30900 = VECTOR ( 'NONE', #44048, 1000.000000000000000 ) ;
#30901 = VECTOR ( 'NONE', #12076, 1000.000000000000000 ) ;
#30902 = CARTESIAN_POINT ( 'NONE',  ( -17.00000000000000000, -15.50000000000000000, -14.50000000000000000 ) ) ;
#30903 = CARTESIAN_POINT ( 'NONE',  ( -7.249999999999995559, -7.848062532927998269, -5.000000000000000000 ) ) ;
#30904 = LINE ( 'NONE', #53530, #60959 ) ;
#30905 = PRESENTATION_LAYER_ASSIGNMENT (  '', '', ( #54585 ) ) ;
#30906 = VECTOR ( 'NONE', #58811, 1000.000000000000000 ) ;
#30907 = VERTEX_POINT ( 'NONE', #37031 ) ;
#30908 = LINE ( 'NONE', #30208, #34847 ) ;
#30909 = CARTESIAN_POINT ( 'NONE',  ( 7.450000000000003730, -7.249999999999997335, -13.00000000000000178 ) ) ;
#30910 = DIRECTION ( 'NONE',  ( -1.000000000000000000, 0.000000000000000000, 0.000000000000000000 ) ) ;
#30911 = ORIENTED_EDGE ( 'NONE', *, *, #62299, .F. ) ;
#30912 = DIRECTION ( 'NONE',  ( 0.7071067811865474617, 0.7071067811865474617, 0.000000000000000000 ) ) ;
#30913 = CYLINDRICAL_SURFACE ( 'NONE', #26117, 4.500000000000188294 ) ;
#30914 = DIRECTION ( 'NONE',  ( 0.000000000000000000, 0.000000000000000000, -1.000000000000000000 ) ) ;
#30915 = VERTEX_POINT ( 'NONE', #68496 ) ;
#30916 = LINE ( 'NONE', #15359, #62971 ) ;
#30917 = DIRECTION ( 'NONE',  ( 0.000000000000000000, 0.000000000000000000, 1.000000000000000000 ) ) ;
#30918 = EDGE_CURVE ( 'NONE', #68236, #14490, #53634, .T. ) ;
#30919 = EDGE_CURVE ( 'NONE', #59636, #37440, #10141, .T. ) ;
#30920 = DIRECTION ( 'NONE',  ( 0.000000000000000000, -0.7075259945834421194, -0.7066873191084661610 ) ) ;
#30921 = ORIENTED_EDGE ( 'NONE', *, *, #22855, .T. ) ;
#30922 = CARTESIAN_POINT ( 'NONE',  ( 7.000000000000000000, -25.93000000000544958, 9.412893218815410634 ) ) ;
#30923 = CARTESIAN_POINT ( 'NONE',  ( 151.5599459900709860, 9.000000000000001776, 326.8892501111512843 ) ) ;
#30924 = EDGE_CURVE ( 'NONE', #41126, #14914, #49017, .T. ) ;
#30925 = CYLINDRICAL_SURFACE ( 'NONE', #45503, 5.000000000000004441 ) ;
#30926 = FACE_BOUND ( 'NONE', #22418, .T. ) ;
#30927 = CARTESIAN_POINT ( 'NONE',  ( -8.250000000000001776, -7.249999999999998224, -13.50000000000000178 ) ) ;
#30928 = ORIENTED_EDGE ( 'NONE', *, *, #56521, .T. ) ;
#30929 = DIRECTION ( 'NONE',  ( 1.000000000000000000, 0.000000000000000000, 0.000000000000000000 ) ) ;
#30930 = LINE ( 'NONE', #52503, #67757 ) ;
#30931 = EDGE_CURVE ( 'NONE', #11798, #31047, #10829, .T. ) ;
#30932 = CARTESIAN_POINT ( 'NONE',  ( 7.250000000000004441, 7.450000000000001954, -17.50000000000000000 ) ) ;
#30933 = PRODUCT_DEFINITION ( 'UNKNOWN', '', #26814, #55130 ) ;
#30934 = CARTESIAN_POINT ( 'NONE',  ( 15.50000000000000000, -5.000000000000000000, -26.50000000000000000 ) ) ;
#30935 = APPLICATION_CONTEXT ( 'automotive_design' ) ;
#30936 = EDGE_CURVE ( 'NONE', #26720, #13935, #54326, .T. ) ;
#30937 = CARTESIAN_POINT ( 'NONE',  ( -7.250000000000001776, -7.249999999999998224, -23.00000000000000000 ) ) ;
#30938 = ORIENTED_EDGE ( 'NONE', *, *, #8159, .F. ) ;
#30940 = VERTEX_POINT ( 'NONE', #21793 ) ;
#30939 = DIRECTION ( 'NONE',  ( 1.836970198721029934E-16, 1.836970198721010706E-16, -1.000000000000000000 ) ) ;
#30941 = EDGE_CURVE ( 'NONE', #46298, #15622, #18321, .T. ) ;
#30942 = VECTOR ( 'NONE', #9386, 1000.000000000000000 ) ;
#30943 = CARTESIAN_POINT ( 'NONE',  ( 13.00000000000000178, -15.50000000000000000, -14.50000000000000000 ) ) ;
#30944 = CARTESIAN_POINT ( 'NONE',  ( 13.00000000000000178, -15.50000000000000000, -14.50000000000000000 ) ) ;
#30945 = CARTESIAN_POINT ( 'NONE',  ( 283.0000000000000568, -38.09999999999885034, -8.400000000000000355 ) ) ;
#30946 = EDGE_LOOP ( 'NONE', ( #56695, #26043, #4190, #12021 ) ) ;
#30947 = AXIS2_PLACEMENT_3D ( 'NONE', #53558, #32335, #5115 ) ;
#30948 = CARTESIAN_POINT ( 'NONE',  ( 9.306483450353418618, 10.91351654964656426, 455.0000000000000568 ) ) ;
#30949 = ORIENTED_EDGE ( 'NONE', *, *, #28802, .T. ) ;
#30950 = ORIENTED_EDGE ( 'NONE', *, *, #9775, .T. ) ;
#30952 = ORIENTED_EDGE ( 'NONE', *, *, #6953, .F. ) ;
#30951 = AXIS2_PLACEMENT_3D ( 'NONE', #24852, #46758, #68337 ) ;
#30953 = DIRECTION ( 'NONE',  ( 0.000000000000000000, 0.000000000000000000, 1.000000000000000000 ) ) ;
#30954 = DIRECTION ( 'NONE',  ( -3.903627567395476653E-15, -1.000000000000000000, -1.836970198721029194E-16 ) ) ;
#30955 = CARTESIAN_POINT ( 'NONE',  ( 49.00000000000000000, -21.00000000000000000, 13.86939075806900057 ) ) ;
#30956 = DIRECTION ( 'NONE',  ( 0.000000000000000000, 0.000000000000000000, 1.000000000000000000 ) ) ;
#30957 = ORIENTED_EDGE ( 'NONE', *, *, #23570, .F. ) ;
#30958 = ORIENTED_EDGE ( 'NONE', *, *, #57209, .F. ) ;
#30959 = DIRECTION ( 'NONE',  ( 0.000000000000000000, 0.000000000000000000, -1.000000000000000000 ) ) ;
#30960 = VECTOR ( 'NONE', #38941, 1000.000000000000000 ) ;
#30961 = DIRECTION ( 'NONE',  ( 1.000000000000000000, -0.000000000000000000, -0.000000000000000000 ) ) ;
#30962 = VERTEX_POINT ( 'NONE', #43712 ) ;
#30963 = ORIENTED_EDGE ( 'NONE', *, *, #16806, .T. ) ;
#30964 = EDGE_CURVE ( 'NONE', #47223, #11065, #55590, .T. ) ;
#30965 = EDGE_LOOP ( 'NONE', ( #27962, #10645, #64264, #15474 ) ) ;
#30966 = ORIENTED_EDGE ( 'NONE', *, *, #7685, .F. ) ;
#30967 = DIRECTION ( 'NONE',  ( -1.000000000000000000, 0.000000000000000000, 0.000000000000000000 ) ) ;
#30968 = UNCERTAINTY_MEASURE_WITH_UNIT (LENGTH_MEASURE( 1.000000000000000082E-05 ), #9341, 'distance_accuracy_value', 'NONE');
#30970 = ORIENTED_EDGE ( 'NONE', *, *, #57002, .F. ) ;
#30969 = LINE ( 'NONE', #47239, #52545 ) ;
#30971 = DIRECTION ( 'NONE',  ( 1.836970198721029934E-16, 1.836970198721010706E-16, -1.000000000000000000 ) ) ;
#30972 = DIRECTION ( 'NONE',  ( -1.000000000000000000, 0.000000000000000000, 0.000000000000000000 ) ) ;
#30973 = DIRECTION ( 'NONE',  ( 1.000000000000000000, 0.000000000000000000, 0.000000000000000000 ) ) ;
#30974 = ORIENTED_EDGE ( 'NONE', *, *, #38021, .T. ) ;
#30975 = AXIS2_PLACEMENT_3D ( 'NONE', #36220, #63453, #57788 ) ;
#30976 = VERTEX_POINT ( 'NONE', #5535 ) ;
#30977 = EDGE_CURVE ( 'NONE', #34023, #40740, #22496, .T. ) ;
#30978 = AXIS2_PLACEMENT_3D ( 'NONE', #49458, #11943, #69978 ) ;
#30979 = DIRECTION ( 'NONE',  ( 0.000000000000000000, 1.000000000000000000, -0.000000000000000000 ) ) ;
#30980 = EDGE_CURVE ( 'NONE', #13668, #53236, #57856, .T. ) ;
#30981 = LINE ( 'NONE', #4124, #63138 ) ;
#30982 = ORIENTED_EDGE ( 'NONE', *, *, #26617, .F. ) ;
#30983 = VECTOR ( 'NONE', #2164, 1000.000000000000000 ) ;
#30984 = CARTESIAN_POINT ( 'NONE',  ( 41.09999999999999432, 13.66939075806899950, 20.80000000000000426 ) ) ;
#30985 = DIRECTION ( 'NONE',  ( 0.000000000000000000, 0.000000000000000000, 1.000000000000000000 ) ) ;
#30986 = ORIENTED_EDGE ( 'NONE', *, *, #63649, .F. ) ;
#30987 = CARTESIAN_POINT ( 'NONE',  ( 10.09643294401453240, 9.093516549646613711, 195.0000000000000284 ) ) ;
#30988 = LINE ( 'NONE', #20725, #26817 ) ;
#30989 = CIRCLE ( 'NONE', #33267, 1.000000000000000000 ) ;
#30991 = AXIS2_PLACEMENT_3D ( 'NONE', #28040, #7140, #49601 ) ;
#30990 = FACE_OUTER_BOUND ( 'NONE', #337, .T. ) ;
#30992 = CARTESIAN_POINT ( 'NONE',  ( -22.14589803375000088, -15.50000000000000000, -21.50000000000000000 ) ) ;
#30993 = ADVANCED_FACE ( 'NONE', ( #575 ), #22145, .F. ) ;
#30994 = VECTOR ( 'NONE', #49813, 1000.000000000000000 ) ;
#30995 = CYLINDRICAL_SURFACE ( 'NONE', #50066, 3.500000000000003109 ) ;
#30996 = ORIENTED_EDGE ( 'NONE', *, *, #51267, .T. ) ;
#30997 = CARTESIAN_POINT ( 'NONE',  ( 16.75000000000000000, -2.500000000000000000, -21.77831216351300014 ) ) ;
#30998 = LINE ( 'NONE', #21433, #66649 ) ;
#30999 = DIRECTION ( 'NONE',  ( 0.000000000000000000, 0.000000000000000000, -1.000000000000000000 ) ) ;
#31000 = CARTESIAN_POINT ( 'NONE',  ( 5.793274621760841292, 6.344366288193348247, 54.00000000000000711 ) ) ;
#31001 = ADVANCED_FACE ( 'NONE', ( #16835 ), #64934, .F. ) ;
#31002 = CARTESIAN_POINT ( 'NONE',  ( 8.250000000000005329, 7.250000000000000888, -22.50000000000000000 ) ) ;
#31003 = CARTESIAN_POINT ( 'NONE',  ( 28.90000000000000213, 0.000000000000000000, 2.154935995002245293E-15 ) ) ;
#31004 = AXIS2_PLACEMENT_3D ( 'NONE', #59395, #49484, #43471 ) ;
#31005 = DIRECTION ( 'NONE',  ( -1.000000000000000000, 1.047444401652939849E-14, 0.000000000000000000 ) ) ;
#31006 = DIRECTION ( 'NONE',  ( 0.000000000000000000, 0.000000000000000000, 1.000000000000000000 ) ) ;
#31007 = VERTEX_POINT ( 'NONE', #38740 ) ;
#31008 = LINE ( 'NONE', #14750, #54713 ) ;
#31009 = DIRECTION ( 'NONE',  ( -3.614007241618349165E-15, -1.000000000000000000, 0.000000000000000000 ) ) ;
#31010 = EDGE_CURVE ( 'NONE', #27141, #40597, #23984, .T. ) ;
#31011 = CARTESIAN_POINT ( 'NONE',  ( 7.000000000000000000, -42.50000000000000000, -15.10000000000000142 ) ) ;
#31012 = DIRECTION ( 'NONE',  ( 0.000000000000000000, 0.000000000000000000, 1.000000000000000000 ) ) ;
#31013 = CARTESIAN_POINT ( 'NONE',  ( 14.75000000000000533, -42.25000000000000000, -26.74999999999999645 ) ) ;
#31014 = CARTESIAN_POINT ( 'NONE',  ( -3.650476262117221093, 10.49297626211717116, 26.00000000000000711 ) ) ;
#31015 = ADVANCED_FACE ( 'NONE', ( #38075 ), #27097, .F. ) ;
#31016 = DIRECTION ( 'NONE',  ( -1.000000000000000000, 0.000000000000000000, 0.000000000000000000 ) ) ;
#31017 = VERTEX_POINT ( 'NONE', #33444 ) ;
#31018 = ADVANCED_FACE ( 'NONE', ( #39089 ), #7021, .T. ) ;
#31019 = VERTEX_POINT ( 'NONE', #49702 ) ;
#31020 = CARTESIAN_POINT ( 'NONE',  ( 8.000000000000001776, -6.879816696376140683, 5.000000000000000000 ) ) ;
#31021 = CARTESIAN_POINT ( 'NONE',  ( -24.00000000000000000, -15.50000000000000000, 14.50000000000000000 ) ) ;
#31022 = VERTEX_POINT ( 'NONE', #231 ) ;
#31023 = VECTOR ( 'NONE', #53394, 1000.000000000000000 ) ;
#31024 = DIRECTION ( 'NONE',  ( 0.000000000000000000, 1.000000000000000000, 0.000000000000000000 ) ) ;
#31025 = CARTESIAN_POINT ( 'NONE',  ( 14.89999999999999680, -0.2000000000089119934, -8.913009219568841313E-12 ) ) ;
#31026 = ADVANCED_FACE ( 'NONE', ( #60299 ), #43005, .F. ) ;
#31027 = VECTOR ( 'NONE', #37374, 1000.000000000000000 ) ;
#31028 = ORIENTED_EDGE ( 'NONE', *, *, #20237, .F. ) ;
#31029 = DIRECTION ( 'NONE',  ( -1.000000000000000000, 0.000000000000000000, 0.000000000000000000 ) ) ;
#31030 = ORIENTED_EDGE ( 'NONE', *, *, #66840, .F. ) ;
#31031 = ORIENTED_EDGE ( 'NONE', *, *, #67640, .F. ) ;
#31032 = DIRECTION ( 'NONE',  ( -1.000000000000000000, 0.000000000000000000, 0.000000000000000000 ) ) ;
#31033 = ORIENTED_EDGE ( 'NONE', *, *, #8756, .F. ) ;
#31034 = ORIENTED_EDGE ( 'NONE', *, *, #48808, .T. ) ;
#31035 = DIRECTION ( 'NONE',  ( 1.836970198721029934E-16, 1.836970198721010706E-16, -1.000000000000000000 ) ) ;
#31036 = LINE ( 'NONE', #5227, #66365 ) ;
#31037 = VECTOR ( 'NONE', #55520, 1000.000000000000000 ) ;
#31038 = AXIS2_PLACEMENT_3D ( 'NONE', #16967, #22616, #6687 ) ;
#31039 = FACE_OUTER_BOUND ( 'NONE', #25234, .T. ) ;
#31040 = EDGE_CURVE ( 'NONE', #65081, #2958, #27389, .T. ) ;
#31041 = EDGE_LOOP ( 'NONE', ( #25414, #7687, #18474, #15047, #57394, #37066 ) ) ;
#31042 = CARTESIAN_POINT ( 'NONE',  ( -11.00000000000000000, -12.00000000000000000, 12.20000000000000107 ) ) ;
#31044 = CARTESIAN_POINT ( 'NONE',  ( 18.89999999999999858, 20.60000000000000142, -13.86939075806900057 ) ) ;
#31043 = LINE ( 'NONE', #15135, #53079 ) ;
#31045 = CIRCLE ( 'NONE', #27664, 0.2000000000000005107 ) ;
#31046 = ORIENTED_EDGE ( 'NONE', *, *, #63085, .F. ) ;
#31047 = VERTEX_POINT ( 'NONE', #16138 ) ;
#31048 = VERTEX_POINT ( 'NONE', #60662 ) ;
#31049 = EDGE_CURVE ( 'NONE', #28114, #67635, #12206, .T. ) ;
#31050 = CONTEXT_DEPENDENT_SHAPE_REPRESENTATION ( #47659, #39168 ) ;
#31051 = VECTOR ( 'NONE', #40427, 1000.000000000000000 ) ;
#31052 = DIRECTION ( 'NONE',  ( 0.000000000000000000, 0.000000000000000000, 1.000000000000000000 ) ) ;
#31054 = EDGE_LOOP ( 'NONE', ( #64314, #8977, #23576, #9485 ) ) ;
#31053 = CARTESIAN_POINT ( 'NONE',  ( 10.00000000000000000, 21.00000000000000000, -18.00000000000000355 ) ) ;
#31055 = ADVANCED_FACE ( 'NONE', ( #23170 ), #13259, .F. ) ;
#31056 = CYLINDRICAL_SURFACE ( 'NONE', #46933, 1.000000000000000000 ) ;
#31057 = CIRCLE ( 'NONE', #49124, 5.000000000000004441 ) ;
#31058 = CARTESIAN_POINT ( 'NONE',  ( -11.18071654964669825, 11.99351654964660341, 455.0000000000000568 ) ) ;
#31059 = ORIENTED_EDGE ( 'NONE', *, *, #24624, .F. ) ;
#31060 = ORIENTED_EDGE ( 'NONE', *, *, #34493, .F. ) ;
#31061 = ADVANCED_FACE ( 'NONE', ( #34458 ), #29167, .F. ) ;
#31062 = CIRCLE ( 'NONE', #573, 0.1999999999999987899 ) ;
#31063 = EDGE_CURVE ( 'NONE', #28581, #53820, #61690, .T. ) ;
#31064 = CARTESIAN_POINT ( 'NONE',  ( -8.250000000000001776, 7.250000000000000888, -26.00000000000001066 ) ) ;
#31065 = ORIENTED_EDGE ( 'NONE', *, *, #21595, .T. ) ;
#31066 = DIRECTION ( 'NONE',  ( 0.000000000000000000, 0.000000000000000000, -1.000000000000000000 ) ) ;
#31067 = FACE_OUTER_BOUND ( 'NONE', #865, .T. ) ;
#31068 = EDGE_CURVE ( 'NONE', #2050, #26250, #20612, .T. ) ;
#31069 = DIRECTION ( 'NONE',  ( 0.000000000000000000, 0.000000000000000000, -1.000000000000000000 ) ) ;
#31070 = VERTEX_POINT ( 'NONE', #51086 ) ;
#31071 = CIRCLE ( 'NONE', #588, 0.1999999999999987899 ) ;
#31072 = FACE_OUTER_BOUND ( 'NONE', #26769, .T. ) ;
#31073 = CARTESIAN_POINT ( 'NONE',  ( 30.00000000000000000, -17.50000000000000000, -26.64999999999999858 ) ) ;
#31074 = EDGE_CURVE ( 'NONE', #6107, #2927, #43176, .T. ) ;
#31076 = ORIENTED_EDGE ( 'NONE', *, *, #69219, .T. ) ;
#31075 = FACE_OUTER_BOUND ( 'NONE', #16116, .T. ) ;
#31078 = VERTEX_POINT ( 'NONE', #1960 ) ;
#31077 = DIRECTION ( 'NONE',  ( -0.000000000000000000, -0.000000000000000000, -1.000000000000000000 ) ) ;
#31079 = EDGE_CURVE ( 'NONE', #36053, #24957, #44321, .T. ) ;
#31080 = CARTESIAN_POINT ( 'NONE',  ( -5.242976262117275077, -5.257023737882800418, 26.00000000000000711 ) ) ;
#31081 = LINE ( 'NONE', #42033, #27351 ) ;
#31082 = EDGE_CURVE ( 'NONE', #67161, #27668, #67360, .T. ) ;
#31083 = AXIS2_PLACEMENT_3D ( 'NONE', #2567, #1196, #33702 ) ;
#31084 = LINE ( 'NONE', #36378, #31331 ) ;
#31085 = EDGE_CURVE ( 'NONE', #34215, #43571, #56047, .T. ) ;
#31086 = ADVANCED_FACE ( 'NONE', ( #40477 ), #56740, .T. ) ;
#31087 = CARTESIAN_POINT ( 'NONE',  ( -7.250000000000001776, -7.249999999999998224, -26.00000000000001066 ) ) ;
#31088 = CIRCLE ( 'NONE', #5147, 0.1749999999999989342 ) ;
#31089 = CARTESIAN_POINT ( 'NONE',  ( -7.813516549646711162, 11.99351654964660341, 195.0000000000000284 ) ) ;
#31090 = ORIENTED_EDGE ( 'NONE', *, *, #50026, .T. ) ;
#31091 = CYLINDRICAL_SURFACE ( 'NONE', #49360, 0.1999999999999996503 ) ;
#31092 = DIRECTION ( 'NONE',  ( 1.000000000000000000, 0.000000000000000000, 0.000000000000000000 ) ) ;
#31093 = EDGE_CURVE ( 'NONE', #10643, #34099, #23523, .T. ) ;
#31094 = SURFACE_SIDE_STYLE ('',( #57952 ) ) ;
#31096 = ORIENTED_EDGE ( 'NONE', *, *, #30757, .F. ) ;
#31095 = CARTESIAN_POINT ( 'NONE',  ( 7.272650909786598561, -7.811466277050860718, 455.0000000000000568 ) ) ;
#31097 = CIRCLE ( 'NONE', #38998, 0.1999999999999992339 ) ;
#31098 = AXIS2_PLACEMENT_3D ( 'NONE', #5954, #27521, #6640 ) ;
#31099 = VECTOR ( 'NONE', #4714, 1000.000000000000000 ) ;
#31100 = CARTESIAN_POINT ( 'NONE',  ( 25.90000000000000213, -0.000000000000000000, 20.80000000000000426 ) ) ;
#31101 = AXIS2_PLACEMENT_3D ( 'NONE', #26886, #69675, #42781 ) ;
#31102 = EDGE_CURVE ( 'NONE', #60595, #49899, #8292, .T. ) ;
#31103 = FACE_OUTER_BOUND ( 'NONE', #57257, .T. ) ;
#31104 = EDGE_CURVE ( 'NONE', #20722, #60486, #21734, .T. ) ;
#31105 = AXIS2_PLACEMENT_3D ( 'NONE', #15136, #53668, #25757 ) ;
#31106 = VECTOR ( 'NONE', #25923, 1000.000000000000000 ) ;
#31107 = DIRECTION ( 'NONE',  ( -1.000000000000000000, 1.671920889371702854E-15, 0.000000000000000000 ) ) ;
#31108 = ORIENTED_EDGE ( 'NONE', *, *, #10641, .F. ) ;
#31109 = FACE_OUTER_BOUND ( 'NONE', #2085, .T. ) ;
#31110 = LINE ( 'NONE', #42052, #45289 ) ;
#31111 = ORIENTED_EDGE ( 'NONE', *, *, #47362, .F. ) ;
#31112 =( LENGTH_UNIT ( ) NAMED_UNIT ( * ) SI_UNIT ( .MILLI., .METRE. ) );
#31113 = CARTESIAN_POINT ( 'NONE',  ( 11.78648345035340839, 7.813516549646560172, 455.0000000000000568 ) ) ;
#31114 = AXIS2_PLACEMENT_3D ( 'NONE', #42167, #36890, #57387 ) ;
#31115 = CARTESIAN_POINT ( 'NONE',  ( -8.250000000000001776, -7.249999999999998224, -9.500000000000001776 ) ) ;
#31116 = ADVANCED_FACE ( 'NONE', ( #45077 ), #34116, .F. ) ;
#31117 = CARTESIAN_POINT ( 'NONE',  ( 30.00000000000000000, -13.79999999999979998, 17.30000000000000071 ) ) ;
#31118 = ADVANCED_FACE ( 'NONE', ( #35510 ), #28466, .F. ) ;
#31119 = CARTESIAN_POINT ( 'NONE',  ( -5.993516549646711766, 5.993516549646603409, 455.0000000000000568 ) ) ;
#31120 = ORIENTED_EDGE ( 'NONE', *, *, #52166, .T. ) ;
#31121 = VERTEX_POINT ( 'NONE', #66652 ) ;
#31122 = ORIENTED_EDGE ( 'NONE', *, *, #21588, .T. ) ;
#31123 = ORIENTED_EDGE ( 'NONE', *, *, #28478, .T. ) ;
#31124 = ORIENTED_EDGE ( 'NONE', *, *, #39473, .F. ) ;
#31125 = AXIS2_PLACEMENT_3D ( 'NONE', #31536, #24818, #41771 ) ;
#31126 = DIRECTION ( 'NONE',  ( -1.000000000000000000, 0.000000000000000000, 0.000000000000000000 ) ) ;
#31127 = EDGE_CURVE ( 'NONE', #46765, #55302, #18211, .T. ) ;
#31128 = CARTESIAN_POINT ( 'NONE',  ( 7.000000000000000000, -38.65000000000095781, 13.20000000000094253 ) ) ;
#31129 = DIRECTION ( 'NONE',  ( 0.000000000000000000, -0.9938079899998859545, 0.1111111111112941946 ) ) ;
#31130 = ORIENTED_EDGE ( 'NONE', *, *, #49001, .F. ) ;
#31131 = ORIENTED_EDGE ( 'NONE', *, *, #49526, .T. ) ;
#31132 = CARTESIAN_POINT ( 'NONE',  ( -30.00000000000000000, -17.50000000000000000, -26.64999999999999858 ) ) ;
#31133 = ORIENTED_EDGE ( 'NONE', *, *, #27890, .T. ) ;
#31134 = VERTEX_POINT ( 'NONE', #12890 ) ;
#31135 = DIRECTION ( 'NONE',  ( -0.8660254037844383745, -0.5000000000000004441, -1.836970198721031660E-16 ) ) ;
#31136 = CARTESIAN_POINT ( 'NONE',  ( -7.394232575409605879, -3.724485858128642413, 54.00000000000000711 ) ) ;
#31137 = CYLINDRICAL_SURFACE ( 'NONE', #58055, 0.7499999999999997780 ) ;
#31138 = VECTOR ( 'NONE', #58988, 1000.000000000000114 ) ;
#31139 = ORIENTED_EDGE ( 'NONE', *, *, #52564, .T. ) ;
#31140 = CARTESIAN_POINT ( 'NONE',  ( 283.0000000000000568, -32.46196062927499781, -8.091291340630698770 ) ) ;
#31142 = DIRECTION ( 'NONE',  ( 0.000000000000000000, 0.000000000000000000, -1.000000000000000000 ) ) ;
#31141 = DIRECTION ( 'NONE',  ( 0.000000000000000000, 1.000000000000000000, 0.000000000000000000 ) ) ;
#31143 = VERTEX_POINT ( 'NONE', #50734 ) ;
#31145 = ORIENTED_EDGE ( 'NONE', *, *, #1949, .F. ) ;
#31144 = DIRECTION ( 'NONE',  ( 0.000000000000000000, 1.000000000000000000, -0.000000000000000000 ) ) ;
#31146 = AXIS2_PLACEMENT_3D ( 'NONE', #55456, #33187, #47456 ) ;
#31147 = VERTEX_POINT ( 'NONE', #2305 ) ;
#31148 = CIRCLE ( 'NONE', #646, 1.000000000000000000 ) ;
#31149 = CARTESIAN_POINT ( 'NONE',  ( 7.272650909786602114, 4.188533722949199678, 455.0000000000000568 ) ) ;
#31150 = EDGE_CURVE ( 'NONE', #59678, #54089, #23869, .T. ) ;
#31151 = VECTOR ( 'NONE', #51049, 1000.000000000000000 ) ;
#31152 = VECTOR ( 'NONE', #12966, 1000.000000000000000 ) ;
#31154 = LINE ( 'NONE', #9576, #53042 ) ;
#31153 = AXIS2_PLACEMENT_3D ( 'NONE', #21325, #64466, #60865 ) ;
#31155 = ORIENTED_EDGE ( 'NONE', *, *, #15319, .F. ) ;
#31156 = ORIENTED_EDGE ( 'NONE', *, *, #10361, .T. ) ;
#31157 = EDGE_CURVE ( 'NONE', #56057, #46124, #69454, .T. ) ;
#31158 = VECTOR ( 'NONE', #32719, 1000.000000000000114 ) ;
#31159 = CIRCLE ( 'NONE', #67277, 1.000000000000000000 ) ;
#31160 = CIRCLE ( 'NONE', #19826, 0.3499999999999996447 ) ;
#31161 = DIRECTION ( 'NONE',  ( 0.000000000000000000, -1.000000000000000000, 0.000000000000000000 ) ) ;
#31162 = ADVANCED_FACE ( 'NONE', ( #52144 ), #41538, .T. ) ;
#31163 = LINE ( 'NONE', #52736, #52652 ) ;
#31164 = ORIENTED_EDGE ( 'NONE', *, *, #31182, .T. ) ;
#31165 = VERTEX_POINT ( 'NONE', #30927 ) ;
#31166 = CARTESIAN_POINT ( 'NONE',  ( -7.250000000000000888, 7.250000000000001776, -24.00000000000000000 ) ) ;
#31167 = AXIS2_PLACEMENT_3D ( 'NONE', #60340, #39470, #5925 ) ;
#31168 = EDGE_CURVE ( 'NONE', #4444, #57821, #52499, .T. ) ;
#31169 = DIRECTION ( 'NONE',  ( 0.000000000000000000, 0.000000000000000000, 1.000000000000000000 ) ) ;
#31170 = ORIENTED_EDGE ( 'NONE', *, *, #8079, .T. ) ;
#31171 = DIRECTION ( 'NONE',  ( 1.836970198721029934E-16, 1.836970198721010706E-16, -1.000000000000000000 ) ) ;
#31172 = CARTESIAN_POINT ( 'NONE',  ( 5.257023737882819070, -5.257023737882825287, 54.00000000000000711 ) ) ;
#31174 = ORIENTED_EDGE ( 'NONE', *, *, #33839, .T. ) ;
#31173 = CYLINDRICAL_SURFACE ( 'NONE', #23847, 0.7112000000000124889 ) ;
#31175 = VECTOR ( 'NONE', #7670, 1000.000000000000000 ) ;
#31177 = ORIENTED_EDGE ( 'NONE', *, *, #18873, .T. ) ;
#31176 = CARTESIAN_POINT ( 'NONE',  ( -19.00000000000000000, -5.000000000000000000, 22.50000000000000000 ) ) ;
#31178 = CARTESIAN_POINT ( 'NONE',  ( 32.89999999999999858, 13.66939075806899950, 20.80000000000000426 ) ) ;
#31179 = DIRECTION ( 'NONE',  ( 1.000000000000000000, 0.000000000000000000, 0.000000000000000000 ) ) ;
#31180 = CARTESIAN_POINT ( 'NONE',  ( 8.249999999999996447, -7.848062532927998269, -1.000000000000000000 ) ) ;
#31181 = DIRECTION ( 'NONE',  ( 0.000000000000000000, 0.000000000000000000, -1.000000000000000000 ) ) ;
#31182 = EDGE_CURVE ( 'NONE', #12532, #45380, #42582, .T. ) ;
#31183 = PLANE ( 'NONE',  #4620 ) ;
#31184 = PLANE ( 'NONE',  #64276 ) ;
#31185 = ORIENTED_EDGE ( 'NONE', *, *, #45027, .F. ) ;
#31186 = DIRECTION ( 'NONE',  ( -1.000000000000000000, 0.000000000000000000, 0.000000000000000000 ) ) ;
#31188 = ORIENTED_EDGE ( 'NONE', *, *, #29939, .T. ) ;
#31187 = DIRECTION ( 'NONE',  ( 1.000000000000000000, -8.728482790395504563E-15, -3.206792553201184024E-30 ) ) ;
#31189 = FACE_OUTER_BOUND ( 'NONE', #48147, .T. ) ;
#31190 = FACE_OUTER_BOUND ( 'NONE', #15591, .T. ) ;
#31191 = CARTESIAN_POINT ( 'NONE',  ( 8.900000000000005684, -21.00000000000000000, 13.86939075806900057 ) ) ;
#31192 = VECTOR ( 'NONE', #45761, 1000.000000000000000 ) ;
#31193 = CARTESIAN_POINT ( 'NONE',  ( 10.31452373788281562, -3.857023737882824932, 54.00000000000000711 ) ) ;
#31194 = AXIS2_PLACEMENT_3D ( 'NONE', #30324, #19693, #68857 ) ;
#31195 = ORIENTED_EDGE ( 'NONE', *, *, #41199, .F. ) ;
#31196 = CARTESIAN_POINT ( 'NONE',  ( -9.942044687070568543, 2.752095193409294982, 455.0000000000000568 ) ) ;
#31197 = LINE ( 'NONE', #4331, #33887 ) ;
#31198 = VERTEX_POINT ( 'NONE', #15721 ) ;
#31199 = CARTESIAN_POINT ( 'NONE',  ( 105.8309041053263257, 3.657408540445008960, 0.000000000000000000 ) ) ;
#31200 = AXIS2_PLACEMENT_3D ( 'NONE', #23091, #27717, #48943 ) ;
#31201 = DIRECTION ( 'NONE',  ( -1.836970198721029934E-16, 1.836970198721036344E-16, -1.000000000000000000 ) ) ;
#31202 = ADVANCED_FACE ( 'NONE', ( #52869 ), #19607, .T. ) ;
#31203 = ADVANCED_FACE ( 'NONE', ( #63104 ), #63808, .F. ) ;
#31204 = VECTOR ( 'NONE', #54914, 1000.000000000000000 ) ;
#31205 = AXIS2_PLACEMENT_3D ( 'NONE', #761, #69364, #37201 ) ;
#31206 = VECTOR ( 'NONE', #39899, 1000.000000000000114 ) ;
#31207 = CARTESIAN_POINT ( 'NONE',  ( 3.606483450353369147, -7.428221114745098497, 455.0000000000000568 ) ) ;
#31208 = VERTEX_POINT ( 'NONE', #25636 ) ;
#31209 = DIRECTION ( 'NONE',  ( -1.053224967557348291E-14, -1.000000000000000000, 0.000000000000000000 ) ) ;
#31210 = ORIENTED_EDGE ( 'NONE', *, *, #49726, .T. ) ;
#31211 = EDGE_CURVE ( 'NONE', #57411, #33481, #53439, .T. ) ;
#31212 = VERTEX_POINT ( 'NONE', #36573 ) ;
#31213 = CARTESIAN_POINT ( 'NONE',  ( 7.826483450353374671, 11.99351654964662295, 195.0000000000000284 ) ) ;
#31215 = CARTESIAN_POINT ( 'NONE',  ( -5.380658396643234198, 4.734785091273867152, 195.0000000000000284 ) ) ;
#31214 = AXIS2_PLACEMENT_3D ( 'NONE', #69432, #20984, #10384 ) ;
#31216 = VECTOR ( 'NONE', #63394, 1000.000000000000000 ) ;
#31217 = VECTOR ( 'NONE', #16621, 1000.000000000000000 ) ;
#31218 = FACE_OUTER_BOUND ( 'NONE', #10149, .T. ) ;
#31219 = AXIS2_PLACEMENT_3D ( 'NONE', #38707, #50004, #16455 ) ;
#31220 = DIRECTION ( 'NONE',  ( 0.000000000000000000, 1.000000000000000000, 0.000000000000000000 ) ) ;
#31221 = DIRECTION ( 'NONE',  ( 1.000000000000000000, 0.000000000000000000, 0.000000000000000000 ) ) ;
#31222 = EDGE_LOOP ( 'NONE', ( #17167, #25036, #50226, #47017, #24335, #45784, #12084, #5341 ) ) ;
#31223 = VERTEX_POINT ( 'NONE', #47200 ) ;
#31225 = ORIENTED_EDGE ( 'NONE', *, *, #63293, .T. ) ;
#31224 = DIRECTION ( 'NONE',  ( -1.836970198721029934E-16, 1.836970198721036590E-16, -1.000000000000000000 ) ) ;
#31226 = EDGE_LOOP ( 'NONE', ( #5725, #58276, #44679, #60256 ) ) ;
#31227 = CIRCLE ( 'NONE', #35737, 0.2000000000000005107 ) ;
#31228 = CARTESIAN_POINT ( 'NONE',  ( 5.257023737882819070, -5.257023737882825287, 54.00000000000000711 ) ) ;
#31229 = LINE ( 'NONE', #37222, #24126 ) ;
#31230 = DIRECTION ( 'NONE',  ( -1.000000000000000000, 0.000000000000000000, 0.000000000000000000 ) ) ;
#31231 = LINE ( 'NONE', #52803, #31106 ) ;
#31233 = PLANE ( 'NONE',  #21052 ) ;
#31232 = CARTESIAN_POINT ( 'NONE',  ( 0.000000000000000000, -8.249999999999998224, -14.00000000000000000 ) ) ;
#31234 = ORIENTED_EDGE ( 'NONE', *, *, #56035, .F. ) ;
#31235 = ORIENTED_EDGE ( 'NONE', *, *, #12463, .F. ) ;
#31236 = VERTEX_POINT ( 'NONE', #3706 ) ;
#31237 = DIRECTION ( 'NONE',  ( 0.000000000000000000, -0.9921567416492215186, 0.1249999999999996531 ) ) ;
#31238 = CARTESIAN_POINT ( 'NONE',  ( -7.342976262117259623, 5.538810540049946773, 26.00000000000000711 ) ) ;
#31239 = EDGE_CURVE ( 'NONE', #15146, #30523, #47542, .T. ) ;
#31240 = DIRECTION ( 'NONE',  ( 1.000000000000000000, -0.000000000000000000, 0.000000000000000000 ) ) ;
#31241 = VERTEX_POINT ( 'NONE', #24921 ) ;
#31242 = ORIENTED_EDGE ( 'NONE', *, *, #37969, .F. ) ;
#31243 = AXIS2_PLACEMENT_3D ( 'NONE', #18811, #40384, #61941 ) ;
#31244 = VERTEX_POINT ( 'NONE', #20316 ) ;
#31245 = EDGE_CURVE ( 'NONE', #25606, #7476, #69108, .T. ) ;
#31246 = CARTESIAN_POINT ( 'NONE',  ( -2.355476262117229158, 9.547976262117156665, 54.00000000000000711 ) ) ;
#31247 = ORIENTED_EDGE ( 'NONE', *, *, #26871, .T. ) ;
#31248 = AXIS2_PLACEMENT_3D ( 'NONE', #65555, #17110, #53921 ) ;
#31249 = VERTEX_POINT ( 'NONE', #46481 ) ;
#31250 = EDGE_CURVE ( 'NONE', #45686, #27049, #68056, .T. ) ;
#31251 = CARTESIAN_POINT ( 'NONE',  ( -1.853252480934758584, 9.404046420173985510, 195.0000000000000284 ) ) ;
#31252 = EDGE_CURVE ( 'NONE', #55063, #7002, #61267, .T. ) ;
#31253 = VERTEX_POINT ( 'NONE', #14662 ) ;
#31254 = ORIENTED_EDGE ( 'NONE', *, *, #38043, .T. ) ;
#31255 = CIRCLE ( 'NONE', #53866, 1.620999999999997332 ) ;
#31257 = DIRECTION ( 'NONE',  ( -1.000000000000000000, 0.000000000000000000, 0.000000000000000000 ) ) ;
#31256 = AXIS2_PLACEMENT_3D ( 'NONE', #58021, #47410, #35748 ) ;
#31258 = ADVANCED_FACE ( 'NONE', ( #63457 ), #36948, .F. ) ;
#31259 = EDGE_CURVE ( 'NONE', #68411, #38943, #58148, .T. ) ;
#31261 = ORIENTED_EDGE ( 'NONE', *, *, #34535, .F. ) ;
#31260 = DIRECTION ( 'NONE',  ( 1.000000000000000000, -1.920292680692490463E-14, 1.836970198720994682E-16 ) ) ;
#31262 = ORIENTED_EDGE ( 'NONE', *, *, #45417, .T. ) ;
#31263 = CIRCLE ( 'NONE', #65172, 0.1749999999999980738 ) ;
#31264 = AXIS2_PLACEMENT_3D ( 'NONE', #17945, #12976, #60737 ) ;
#31265 = AXIS2_PLACEMENT_3D ( 'NONE', #5247, #27152, #42713 ) ;
#31266 = CARTESIAN_POINT ( 'NONE',  ( 7.000000000000000000, -53.81370849898476649, 16.03137303340311348 ) ) ;
#31267 = EDGE_CURVE ( 'NONE', #26713, #53236, #25272, .T. ) ;
#31268 = DIRECTION ( 'NONE',  ( -1.000000000000000000, 0.000000000000000000, 0.000000000000000000 ) ) ;
#31270 = VERTEX_POINT ( 'NONE', #31299 ) ;
#31269 = DIRECTION ( 'NONE',  ( 0.5773502691896230665, -0.5773502691896230665, 0.5773502691896311712 ) ) ;
#31271 = ORIENTED_EDGE ( 'NONE', *, *, #2333, .T. ) ;
#31272 = AXIS2_PLACEMENT_3D ( 'NONE', #49171, #59435, #5360 ) ;
#31273 = CARTESIAN_POINT ( 'NONE',  ( 3.430747519065294071, -7.852485183457023510, 455.0000000000000568 ) ) ;
#31274 = VECTOR ( 'NONE', #68166, 1000.000000000000000 ) ;
#31275 = CARTESIAN_POINT ( 'NONE',  ( 7.000000000000000000, -27.13000000000000611, 13.50000000000000000 ) ) ;
#31276 = FACE_OUTER_BOUND ( 'NONE', #12441, .T. ) ;
#31277 = DIRECTION ( 'NONE',  ( 0.000000000000000000, -1.000000000000000000, -3.673940397442060361E-16 ) ) ;
#31278 = VECTOR ( 'NONE', #57236, 1000.000000000000000 ) ;
#31279 = ORIENTED_EDGE ( 'NONE', *, *, #16106, .T. ) ;
#31280 = CARTESIAN_POINT ( 'NONE',  ( 9.955011587777235604, -2.765062094116182312, 455.0000000000000568 ) ) ;
#31281 = VECTOR ( 'NONE', #14195, 1000.000000000000000 ) ;
#31282 = DIRECTION ( 'NONE',  ( 1.000000000000000000, -0.000000000000000000, 0.000000000000000000 ) ) ;
#31283 = CARTESIAN_POINT ( 'NONE',  ( 18.89999999999999858, 20.60000000000000142, 13.86939075806900057 ) ) ;
#31284 = LINE ( 'NONE', #25622, #41535 ) ;
#31285 = DIRECTION ( 'NONE',  ( -1.356437060717832013E-15, -1.000000000000000000, -1.836970198721033878E-16 ) ) ;
#31286 = CARTESIAN_POINT ( 'NONE',  ( -7.394232575409614761, 3.710438382363058896, 54.00000000000000711 ) ) ;
#31287 = ORIENTED_EDGE ( 'NONE', *, *, #51801, .F. ) ;
#31288 = CARTESIAN_POINT ( 'NONE',  ( 11.08848345035334404, -11.48848345035349183, 455.0000000000000568 ) ) ;
#31289 = CARTESIAN_POINT ( 'NONE',  ( 7.249999999999995559, 8.250000000000001776, 5.000000000000000000 ) ) ;
#31290 = EDGE_CURVE ( 'NONE', #48836, #36185, #4877, .T. ) ;
#31291 = CARTESIAN_POINT ( 'NONE',  ( -11.00000000000000000, -8.959999999999999076, -17.04524521594300523 ) ) ;
#31292 = ORIENTED_EDGE ( 'NONE', *, *, #55251, .T. ) ;
#31293 = CARTESIAN_POINT ( 'NONE',  ( -7.813516549646836395, -11.78648345035340661, 455.0000000000000568 ) ) ;
#31294 = CARTESIAN_POINT ( 'NONE',  ( -6.642976262117328723, -9.912023737882789121, 54.00000000000000711 ) ) ;
#31295 = DIRECTION ( 'NONE',  ( 0.000000000000000000, -0.9938079899998859545, 0.1111111111112941946 ) ) ;
#31296 = EDGE_CURVE ( 'NONE', #30686, #373, #5107, .T. ) ;
#31297 = EDGE_CURVE ( 'NONE', #46798, #31830, #37988, .T. ) ;
#31298 = LINE ( 'NONE', #52867, #48255 ) ;
#31299 = CARTESIAN_POINT ( 'NONE',  ( 0.5000000000000000000, 18.00000000000000355, -21.00000000000000000 ) ) ;
#31300 = EDGE_LOOP ( 'NONE', ( #58483, #47810, #53708, #9269 ) ) ;
#31301 = DIRECTION ( 'NONE',  ( 0.8660254037844311581, -0.5000000000000129896, 6.723777587268175486E-17 ) ) ;
#31302 = CARTESIAN_POINT ( 'NONE',  ( 5.257023737882819070, -5.257023737882825287, 54.00000000000000711 ) ) ;
#31303 = AXIS2_PLACEMENT_3D ( 'NONE', #59684, #22548, #44103 ) ;
#31304 = DIRECTION ( 'NONE',  ( 1.000000000000000000, -0.000000000000000000, -0.000000000000000000 ) ) ;
#31305 = EDGE_CURVE ( 'NONE', #9808, #4698, #42929, .T. ) ;
#31306 = AXIS2_PLACEMENT_3D ( 'NONE', #4917, #53704, #16213 ) ;
#31307 = AXIS2_PLACEMENT_3D ( 'NONE', #8433, #46980, #25781 ) ;
#31308 = DIRECTION ( 'NONE',  ( 0.000000000000000000, -0.6801302850037772574, -0.7330912599538208507 ) ) ;
#31309 = LINE ( 'NONE', #58157, #14791 ) ;
#31310 = ORIENTED_EDGE ( 'NONE', *, *, #26777, .T. ) ;
#31312 = ORIENTED_EDGE ( 'NONE', *, *, #42486, .T. ) ;
#31311 = CARTESIAN_POINT ( 'NONE',  ( 30.00000000000000000, -14.04000000000000092, -14.80000000000000071 ) ) ;
#31313 = AXIS2_PLACEMENT_3D ( 'NONE', #37637, #37287, #47880 ) ;
#31314 = VECTOR ( 'NONE', #43322, 1000.000000000000000 ) ;
#31315 = LINE ( 'NONE', #69119, #23410 ) ;
#31316 = AXIS2_PLACEMENT_3D ( 'NONE', #66075, #13383, #8063 ) ;
#31317 = CARTESIAN_POINT ( 'NONE',  ( -8.916576262117361651, -10.05377373788273587, 54.00000000000000711 ) ) ;
#31318 = CARTESIAN_POINT ( 'NONE',  ( -9.404046420174124066, 1.853252480934674873, 455.0000000000000568 ) ) ;
#31319 = ORIENTED_EDGE ( 'NONE', *, *, #12644, .F. ) ;
#31320 = CIRCLE ( 'NONE', #49375, 0.4000000000000010214 ) ;
#31322 =( LENGTH_UNIT ( ) NAMED_UNIT ( * ) SI_UNIT ( .MILLI., .METRE. ) );
#31321 = AXIS2_PLACEMENT_3D ( 'NONE', #24771, #3557, #25120 ) ;
#31323 = CARTESIAN_POINT ( 'NONE',  ( 3.664523737882781518, -10.31452373788281029, 54.00000000000000711 ) ) ;
#31324 = ORIENTED_EDGE ( 'NONE', *, *, #13542, .F. ) ;
#31325 = ORIENTED_EDGE ( 'NONE', *, *, #51264, .T. ) ;
#31326 = AXIS2_PLACEMENT_3D ( 'NONE', #50784, #3753, #67418 ) ;
#31327 = ORIENTED_EDGE ( 'NONE', *, *, #28860, .F. ) ;
#31328 = LINE ( 'NONE', #10092, #23049 ) ;
#31329 = DIRECTION ( 'NONE',  ( 0.000000000000000000, 0.000000000000000000, -1.000000000000000000 ) ) ;
#31330 = FACE_OUTER_BOUND ( 'NONE', #22504, .T. ) ;
#31331 = VECTOR ( 'NONE', #26134, 1000.000000000000000 ) ;
#31332 = ADVANCED_FACE ( 'NONE', ( #32670 ), #49295, .F. ) ;
#31333 = ORIENTED_EDGE ( 'NONE', *, *, #12303, .F. ) ;
#31334 = ORIENTED_EDGE ( 'NONE', *, *, #14962, .F. ) ;
#31335 = DIRECTION ( 'NONE',  ( 1.000000000000000000, 0.000000000000000000, 0.000000000000000000 ) ) ;
#31336 = LINE ( 'NONE', #43666, #13582 ) ;
#31337 = ORIENTED_EDGE ( 'NONE', *, *, #13035, .F. ) ;
#31338 = ORIENTED_EDGE ( 'NONE', *, *, #41917, .F. ) ;
#31339 = ORIENTED_EDGE ( 'NONE', *, *, #46818, .F. ) ;
#31340 = VERTEX_POINT ( 'NONE', #22747 ) ;
#31341 = CARTESIAN_POINT ( 'NONE',  ( -8.393516549646712122, 6.331612867284047041, 455.0000000000000568 ) ) ;
#31342 = ADVANCED_FACE ( 'NONE', ( #59198 ), #21368, .F. ) ;
#31344 = VERTEX_POINT ( 'NONE', #17434 ) ;
#31343 = LINE ( 'NONE', #57137, #57068 ) ;
#31345 = DIRECTION ( 'NONE',  ( 0.000000000000000000, -0.7071067811865474617, -0.7071067811865474617 ) ) ;
#31346 = DIRECTION ( 'NONE',  ( 0.000000000000000000, -1.000000000000000000, 0.000000000000000000 ) ) ;
#31347 = EDGE_CURVE ( 'NONE', #43188, #61781, #6501, .T. ) ;
#31348 = CARTESIAN_POINT ( 'NONE',  ( -2.530476262117228092, 9.722976262117159152, 54.00000000000000711 ) ) ;
#31349 = VECTOR ( 'NONE', #8989, 1000.000000000000114 ) ;
#31350 = ORIENTED_EDGE ( 'NONE', *, *, #33638, .F. ) ;
#31351 = ORIENTED_EDGE ( 'NONE', *, *, #17978, .F. ) ;
#31352 = CARTESIAN_POINT ( 'NONE',  ( 12.00648345035338060, -4.186483450353492231, 455.0000000000000568 ) ) ;
#31353 = AXIS2_PLACEMENT_3D ( 'NONE', #12678, #46268, #7732 ) ;
#31354 = CIRCLE ( 'NONE', #7589, 0.1749999999999989342 ) ;
#31355 = LINE ( 'NONE', #20717, #7802 ) ;
#31356 = EDGE_LOOP ( 'NONE', ( #2006, #6075, #30638, #66825 ) ) ;
#31357 = AXIS2_PLACEMENT_3D ( 'NONE', #76, #21636, #16326 ) ;
#31359 = ADVANCED_FACE ( 'NONE', ( #11102 ), #48897, .T. ) ;
#31358 = AXIS2_PLACEMENT_3D ( 'NONE', #42550, #11743, #33666 ) ;
#31360 = ORIENTED_EDGE ( 'NONE', *, *, #3002, .F. ) ;
#31361 = DIRECTION ( 'NONE',  ( -0.000000000000000000, 1.000000000000000000, -0.000000000000000000 ) ) ;
#31362 = CARTESIAN_POINT ( 'NONE',  ( -18.85410196625000268, -15.50000000000000000, -21.50000000000000000 ) ) ;
#31363 = ORIENTED_EDGE ( 'NONE', *, *, #61152, .T. ) ;
#31364 = CARTESIAN_POINT ( 'NONE',  ( -8.821682069070824639, -8.144523737882760628, 26.00000000000000000 ) ) ;
#31365 = LINE ( 'NONE', #48305, #41491 ) ;
#31366 = CIRCLE ( 'NONE', #12100, 1.224999999999999423 ) ;
#31367 = CIRCLE ( 'NONE', #61823, 2.458500000000000796 ) ;
#31368 = CARTESIAN_POINT ( 'NONE',  ( 2.906483450353420928, 11.11351654964658842, 455.0000000000000568 ) ) ;
#31369 = FACE_OUTER_BOUND ( 'NONE', #56350, .T. ) ;
#31370 = PLANE ( 'NONE',  #11649 ) ;
#31371 = ORIENTED_EDGE ( 'NONE', *, *, #22449, .F. ) ;
#31372 = FACE_OUTER_BOUND ( 'NONE', #51030, .T. ) ;
#31373 = CARTESIAN_POINT ( 'NONE',  ( -25.50000000000000355, -15.12100000000000044, 22.50000000000000000 ) ) ;
#31374 = CARTESIAN_POINT ( 'NONE',  ( 12.00000000000000000, 11.18999999999999950, -5.000000000000000000 ) ) ;
#31375 = CARTESIAN_POINT ( 'NONE',  ( 6.006483450353377940, 7.393516549646627745, 195.0000000000000284 ) ) ;
#31376 = ORIENTED_EDGE ( 'NONE', *, *, #46039, .T. ) ;
#31377 = CARTESIAN_POINT ( 'NONE',  ( 283.0000000000000568, -32.45000000000000995, 12.69999999999999929 ) ) ;
#31378 = LINE ( 'NONE', #47616, #30794 ) ;
#31379 = EDGE_CURVE ( 'NONE', #47728, #28426, #48939, .T. ) ;
#31380 = PLANE ( 'NONE',  #61703 ) ;
#31381 = DIRECTION ( 'NONE',  ( 0.000000000000000000, 0.000000000000000000, -1.000000000000000000 ) ) ;
#31382 = VERTEX_POINT ( 'NONE', #65541 ) ;
#31383 = CARTESIAN_POINT ( 'NONE',  ( -7.250000000000001776, -7.249999999999998224, -8.500000000000000000 ) ) ;
#31384 = CARTESIAN_POINT ( 'NONE',  ( -17.51999999999999957, -17.50000000000000000, 26.00000000000000355 ) ) ;
#31385 = LINE ( 'NONE', #31724, #10785 ) ;
#31386 = EDGE_CURVE ( 'NONE', #28477, #64355, #27711, .T. ) ;
#31387 = DIRECTION ( 'NONE',  ( 0.000000000000000000, 0.000000000000000000, 1.000000000000000000 ) ) ;
#31388 = PRESENTATION_STYLE_ASSIGNMENT (( #37037 ) ) ;
#31389 = CARTESIAN_POINT ( 'NONE',  ( -25.50000000000000355, 0.000000000000000000, -22.50000000000000000 ) ) ;
#31390 = ORIENTED_EDGE ( 'NONE', *, *, #57347, .F. ) ;
#31391 = VERTEX_POINT ( 'NONE', #32330 ) ;
#31392 = CYLINDRICAL_SURFACE ( 'NONE', #28190, 24.99999999998784972 ) ;
#31393 = DIRECTION ( 'NONE',  ( 0.000000000000000000, 0.000000000000000000, -1.000000000000000000 ) ) ;
#31394 = ORIENTED_EDGE ( 'NONE', *, *, #31971, .T. ) ;
#31395 = DIRECTION ( 'NONE',  ( -1.836970198721029934E-16, 1.836970198721036344E-16, -1.000000000000000000 ) ) ;
#31396 = FACE_OUTER_BOUND ( 'NONE', #35994, .T. ) ;
#31397 = ORIENTED_EDGE ( 'NONE', *, *, #42251, .T. ) ;
#31398 = EDGE_CURVE ( 'NONE', #50489, #51462, #11439, .T. ) ;
#31399 = CARTESIAN_POINT ( 'NONE',  ( 5.257023737882801306, 5.242976262117200470, 54.00000000000000711 ) ) ;
#31400 = ORIENTED_EDGE ( 'NONE', *, *, #51300, .T. ) ;
#31401 = ORIENTED_EDGE ( 'NONE', *, *, #28645, .T. ) ;
#31402 = DIRECTION ( 'NONE',  ( -0.000000000000000000, 3.673940397442059868E-16, -1.000000000000000000 ) ) ;
#31403 = ORIENTED_EDGE ( 'NONE', *, *, #34026, .F. ) ;
#31404 = AXIS2_PLACEMENT_3D ( 'NONE', #3898, #3547, #9910 ) ;
#31405 = DIRECTION ( 'NONE',  ( 1.000000000000000000, 0.000000000000000000, 0.000000000000000000 ) ) ;
#31406 = DIRECTION ( 'NONE',  ( -1.000000000000000000, 0.000000000000000000, 0.000000000000000000 ) ) ;
#31407 = DIRECTION ( 'NONE',  ( 0.000000000000000000, 0.7071067811865875408, -0.7071067811865076047 ) ) ;
#31408 = VERTEX_POINT ( 'NONE', #5468 ) ;
#31409 = CARTESIAN_POINT ( 'NONE',  ( 4.186483450353423841, 11.99351654964658742, 455.0000000000000568 ) ) ;
#31410 = VECTOR ( 'NONE', #23071, 1000.000000000000000 ) ;
#31411 = CONICAL_SURFACE ( 'NONE', #55120, 1732.050807568785558, 1.047197551196574761 ) ;
#31413 = DIRECTION ( 'NONE',  ( -1.000000000000000000, 0.000000000000000000, 0.000000000000000000 ) ) ;
#31412 = CARTESIAN_POINT ( 'NONE',  ( -9.880476262117236175, 7.447976262117216528, 54.00000000000000711 ) ) ;
#31414 = EDGE_LOOP ( 'NONE', ( #5076, #41713, #16630, #15170 ) ) ;
#31415 = VERTEX_POINT ( 'NONE', #44302 ) ;
#31416 = ORIENTED_EDGE ( 'NONE', *, *, #32382, .F. ) ;
#31418 = ORIENTED_EDGE ( 'NONE', *, *, #60866, .F. ) ;
#31417 = ITEM_DEFINED_TRANSFORMATION ( 'NONE', 'NONE', #64077,  #45918 ) ;
#31419 = DIRECTION ( 'NONE',  ( 9.799566706031580591E-15, 1.000000000000000000, 1.836970198721018348E-16 ) ) ;
#31421 = ORIENTED_EDGE ( 'NONE', *, *, #54841, .F. ) ;
#31420 = CARTESIAN_POINT ( 'NONE',  ( 8.930623737882843471, 8.566576262117187923, 54.00000000000000711 ) ) ;
#31422 = EDGE_CURVE ( 'NONE', #43603, #46652, #498, .T. ) ;
#31423 = AXIS2_PLACEMENT_3D ( 'NONE', #3342, #9347, #52487 ) ;
#31424 = CARTESIAN_POINT ( 'NONE',  ( 11.90000000000000036, 13.66939075806899240, 20.79999999999999361 ) ) ;
#31425 = DIRECTION ( 'NONE',  ( 0.000000000000000000, 0.000000000000000000, -1.000000000000000000 ) ) ;
#31426 = EDGE_CURVE ( 'NONE', #7623, #31930, #48243, .T. ) ;
#31427 = ORIENTED_EDGE ( 'NONE', *, *, #22280, .F. ) ;
#31428 = EDGE_CURVE ( 'NONE', #6920, #29479, #43966, .T. ) ;
#31429 = ORIENTED_EDGE ( 'NONE', *, *, #43630, .F. ) ;
#31430 = CARTESIAN_POINT ( 'NONE',  ( -7.250000000000001776, -7.249999999999998224, -26.00000000000001066 ) ) ;
#31431 = EDGE_CURVE ( 'NONE', #27077, #14139, #7117, .T. ) ;
#31432 = EDGE_LOOP ( 'NONE', ( #40951, #69458, #27699, #51051 ) ) ;
#31433 = PRODUCT_RELATED_PRODUCT_CATEGORY ( 'part', '', ( #56556 ) ) ;
#31434 = CARTESIAN_POINT ( 'NONE',  ( -15.29633693294650421, -0.2717122460102769921, -23.82579074638668715 ) ) ;
#31435 = CARTESIAN_POINT ( 'NONE',  ( 283.0000000000000568, -26.79000000000000625, 0.000000000000000000 ) ) ;
#31436 = EDGE_CURVE ( 'NONE', #24121, #13405, #38671, .T. ) ;
#31437 = DIRECTION ( 'NONE',  ( 0.000000000000000000, 1.000000000000000000, 0.000000000000000000 ) ) ;
#31438 = ORIENTED_EDGE ( 'NONE', *, *, #67789, .F. ) ;
#31439 = EDGE_CURVE ( 'NONE', #58411, #51947, #2586, .T. ) ;
#31440 = CARTESIAN_POINT ( 'NONE',  ( 14.25000000000000000, -0.2038245569916330158, 21.77831216351300014 ) ) ;
#31441 = LINE ( 'NONE', #14097, #52758 ) ;
#31442 = VECTOR ( 'NONE', #6731, 1000.000000000000000 ) ;
#31444 = ORIENTED_EDGE ( 'NONE', *, *, #18587, .T. ) ;
#31443 = FACE_OUTER_BOUND ( 'NONE', #44338, .T. ) ;
#31446 = EDGE_LOOP ( 'NONE', ( #40783, #34333, #59100, #9301, #50971, #36104, #48446, #58974 ) ) ;
#31445 = CARTESIAN_POINT ( 'NONE',  ( -8.250000000000001776, -8.249999999999998224, -26.00000000000001066 ) ) ;
#31447 = CARTESIAN_POINT ( 'NONE',  ( 13.00000000000000178, -15.50000000000000000, 20.05051025721700242 ) ) ;
#31448 = FACE_OUTER_BOUND ( 'NONE', #38592, .T. ) ;
#31449 = DIRECTION ( 'NONE',  ( 0.000000000000000000, 0.000000000000000000, -1.000000000000000000 ) ) ;
#31450 = CARTESIAN_POINT ( 'NONE',  ( -25.50000000000000355, -5.200000000000001066, 24.75000000000000000 ) ) ;
#31451 = CARTESIAN_POINT ( 'NONE',  ( 6.006483450353379716, -6.006483450353490738, 455.0000000000000568 ) ) ;
#31452 = ORIENTED_EDGE ( 'NONE', *, *, #39135, .F. ) ;
#31453 = DIRECTION ( 'NONE',  ( 1.000000000000000000, -1.671920889371702854E-15, 0.000000000000000000 ) ) ;
#31454 = CARTESIAN_POINT ( 'NONE',  ( 4.456444791733522252E-16, 7.450000000000002842, -15.50000000000000000 ) ) ;
#31455 = FACE_OUTER_BOUND ( 'NONE', #30182, .T. ) ;
#31456 = CIRCLE ( 'NONE', #11095, 0.2000000000000005107 ) ;
#31458 = EDGE_LOOP ( 'NONE', ( #25927, #40148, #8969, #15816 ) ) ;
#31457 = DIRECTION ( 'NONE',  ( 0.000000000000000000, 0.000000000000000000, 1.000000000000000000 ) ) ;
#31459 = FACE_OUTER_BOUND ( 'NONE', #54404, .T. ) ;
#31460 = ADVANCED_FACE ( 'NONE', ( #10412 ), #53552, .F. ) ;
#31461 = CARTESIAN_POINT ( 'NONE',  ( -10.91351654964680584, -9.306483450353375986, 455.0000000000000568 ) ) ;
#31462 = DIRECTION ( 'NONE',  ( 0.000000000000000000, 0.000000000000000000, 1.000000000000000000 ) ) ;
#31463 = CIRCLE ( 'NONE', #54022, 1.000000000000000000 ) ;
#31464 = FACE_OUTER_BOUND ( 'NONE', #24623, .T. ) ;
#31465 = ORIENTED_EDGE ( 'NONE', *, *, #65837, .F. ) ;
#31466 = CARTESIAN_POINT ( 'NONE',  ( 7.450000000000006395, 7.250000000000000888, -9.000000000000001776 ) ) ;
#31467 = DIRECTION ( 'NONE',  ( 0.000000000000000000, 0.000000000000000000, 1.000000000000000000 ) ) ;
#31468 = VERTEX_POINT ( 'NONE', #2920 ) ;
#31469 = CARTESIAN_POINT ( 'NONE',  ( -17.00000000000000000, -16.64230188589299786, 14.64519951917100116 ) ) ;
#31470 = PLANE ( 'NONE',  #61427 ) ;
#31471 = DIRECTION ( 'NONE',  ( 1.000000000000000000, -0.000000000000000000, 0.000000000000000000 ) ) ;
#31472 = AXIS2_PLACEMENT_3D ( 'NONE', #51706, #59008, #58328 ) ;
#31473 = DIRECTION ( 'NONE',  ( 0.000000000000000000, -0.000000000000000000, 1.000000000000000000 ) ) ;
#31474 = VERTEX_POINT ( 'NONE', #29784 ) ;
#31475 = VERTEX_POINT ( 'NONE', #12811 ) ;
#31476 = CYLINDRICAL_SURFACE ( 'NONE', #51011, 0.2000000000000005107 ) ;
#31477 = ORIENTED_EDGE ( 'NONE', *, *, #33147, .T. ) ;
#31478 = VERTEX_POINT ( 'NONE', #29433 ) ;
#31479 = LINE ( 'NONE', #15207, #68699 ) ;
#31480 = FACE_OUTER_BOUND ( 'NONE', #53146, .T. ) ;
#31481 = ADVANCED_FACE ( 'NONE', ( #34036 ), #67626, .T. ) ;
#31482 = CARTESIAN_POINT ( 'NONE',  ( -11.00000000000000000, -17.00000000000000000, 15.70499999999969809 ) ) ;
#31483 = ORIENTED_EDGE ( 'NONE', *, *, #56984, .F. ) ;
#31484 = ORIENTED_EDGE ( 'NONE', *, *, #49490, .F. ) ;
#31485 = DIRECTION ( 'NONE',  ( 0.000000000000000000, 0.000000000000000000, -1.000000000000000000 ) ) ;
#31486 = VERTEX_POINT ( 'NONE', #18127 ) ;
#31487 = EDGE_LOOP ( 'NONE', ( #12878, #24244, #54424, #58004, #64030, #65787, #55506, #42282 ) ) ;
#31488 = CARTESIAN_POINT ( 'NONE',  ( 49.00000000000000000, -0.2000000000089119934, -8.913009219568841313E-12 ) ) ;
#31489 = CARTESIAN_POINT ( 'NONE',  ( 30.00000000000000000, -9.199999999999999289, -12.34999999999989839 ) ) ;
#31490 = CARTESIAN_POINT ( 'NONE',  ( 10.05377373788278739, -9.703773737882823269, 54.00000000000000711 ) ) ;
#31491 = EDGE_CURVE ( 'NONE', #22868, #66424, #24496, .T. ) ;
#31492 = ORIENTED_EDGE ( 'NONE', *, *, #62654, .T. ) ;
#31493 = CARTESIAN_POINT ( 'NONE',  ( 8.000000000000001776, -8.000000000000000000, 0.000000000000000000 ) ) ;
#31495 = LINE ( 'NONE', #58371, #62674 ) ;
#31494 = LINE ( 'NONE', #19461, #34357 ) ;
#31496 = EDGE_LOOP ( 'NONE', ( #58629, #34981, #45212, #27551, #53343, #57030, #24224, #180 ) ) ;
#31499 = EDGE_CURVE ( 'NONE', #48338, #53184, #55619, .T. ) ;
#31498 = ORIENTED_EDGE ( 'NONE', *, *, #26181, .T. ) ;
#31497 = CARTESIAN_POINT ( 'NONE',  ( 30.00000000000000000, -5.599999999999999645, -9.400000000000000355 ) ) ;
#31500 = ORIENTED_EDGE ( 'NONE', *, *, #50125, .T. ) ;
#31501 = ADVANCED_FACE ( 'NONE', ( #61248 ), #46055, .T. ) ;
#31502 = CYLINDRICAL_SURFACE ( 'NONE', #36696, 0.1749999999999989342 ) ;
#31503 = AXIS2_PLACEMENT_3D ( 'NONE', #15475, #58604, #63198 ) ;
#31504 = FACE_OUTER_BOUND ( 'NONE', #39980, .T. ) ;
#31505 = ADVANCED_FACE ( 'NONE', ( #7163 ), #23788, .T. ) ;
#31506 = VERTEX_POINT ( 'NONE', #39694 ) ;
#31507 = EDGE_CURVE ( 'NONE', #45115, #9110, #13173, .T. ) ;
#31508 = AXIS2_PLACEMENT_3D ( 'NONE', #16117, #54649, #62900 ) ;
#31509 = DIRECTION ( 'NONE',  ( -1.000000000000000000, 0.000000000000000000, 0.000000000000000000 ) ) ;
#31510 = DIRECTION ( 'NONE',  ( -1.000000000000000000, 0.000000000000000000, 0.000000000000000000 ) ) ;
#31511 = EDGE_LOOP ( 'NONE', ( #65520, #66138, #15295, #41501, #68986, #33333, #67648, #65482 ) ) ;
#31512 = ORIENTED_EDGE ( 'NONE', *, *, #7262, .F. ) ;
#31513 = AXIS2_PLACEMENT_3D ( 'NONE', #1436, #24041, #34654 ) ;
#31514 = DIRECTION ( 'NONE',  ( 9.912705577010319041E-15, 1.000000000000000000, 0.000000000000000000 ) ) ;
#31515 = EDGE_CURVE ( 'NONE', #29091, #23661, #39353, .T. ) ;
#31516 = CARTESIAN_POINT ( 'NONE',  ( 4.740315990920172418, 7.798499376343941414, 455.0000000000000568 ) ) ;
#31517 = VERTEX_POINT ( 'NONE', #40400 ) ;
#31518 = EDGE_CURVE ( 'NONE', #45363, #51724, #24139, .T. ) ;
#31519 = VECTOR ( 'NONE', #12967, 1000.000000000000000 ) ;
#31520 = CARTESIAN_POINT ( 'NONE',  ( 9.737023737882781305, 3.667976262117152775, 54.00000000000000711 ) ) ;
#31521 = CARTESIAN_POINT ( 'NONE',  ( 283.0000000000000568, -25.50000000000000355, 14.74860679774999994 ) ) ;
#31523 = ORIENTED_EDGE ( 'NONE', *, *, #42129, .F. ) ;
#31522 = CARTESIAN_POINT ( 'NONE',  ( -7.250000000000000888, 8.250000000000001776, -15.50000000000000000 ) ) ;
#31525 = VERTEX_POINT ( 'NONE', #44643 ) ;
#31524 = FACE_OUTER_BOUND ( 'NONE', #40037, .T. ) ;
#31526 = LINE ( 'NONE', #59077, #12473 ) ;
#31527 = VECTOR ( 'NONE', #55171, 1000.000000000000000 ) ;
#31528 = LINE ( 'NONE', #56968, #47626 ) ;
#31529 = EDGE_CURVE ( 'NONE', #2927, #62127, #60574, .T. ) ;
#31530 = CARTESIAN_POINT ( 'NONE',  ( 6.364920264886846368, 3.663616288756996298, 26.00000000000000711 ) ) ;
#31531 = CARTESIAN_POINT ( 'NONE',  ( 4.046023737882819660, -3.157023737882826087, 54.00000000000000711 ) ) ;
#31532 = DIRECTION ( 'NONE',  ( 0.000000000000000000, 0.000000000000000000, -1.000000000000000000 ) ) ;
#31533 = DIRECTION ( 'NONE',  ( -0.7071067811865361374, 0.7071067811865588970, 2.810316974849854557E-30 ) ) ;
#31534 = ORIENTED_EDGE ( 'NONE', *, *, #55417, .F. ) ;
#31535 = PLANE ( 'NONE',  #47388 ) ;
#31537 = EDGE_LOOP ( 'NONE', ( #45712, #24573, #62234, #47667 ) ) ;
#31536 = CARTESIAN_POINT ( 'NONE',  ( 30.00000000000000000, -5.000000000000000000, 27.00000000000000000 ) ) ;
#31538 = DIRECTION ( 'NONE',  ( 0.000000000000000000, 0.000000000000000000, 1.000000000000000000 ) ) ;
#31539 = DIRECTION ( 'NONE',  ( 0.000000000000000000, -0.000000000000000000, 1.000000000000000000 ) ) ;
#31540 = FACE_OUTER_BOUND ( 'NONE', #66905, .T. ) ;
#31541 = ORIENTED_EDGE ( 'NONE', *, *, #36742, .T. ) ;
#31542 = PLANE ( 'NONE',  #17346 ) ;
#31543 = PLANE ( 'NONE',  #58808 ) ;
#31544 = ORIENTED_EDGE ( 'NONE', *, *, #35517, .F. ) ;
#31545 = VECTOR ( 'NONE', #28765, 1000.000000000000000 ) ;
#31546 = ADVANCED_FACE ( 'NONE', ( #13525, #33700, #7522, #67276, #12469, #17789, #66574, #56661, #50311 ), #35081, .T. ) ;
#31547 = DIRECTION ( 'NONE',  ( 0.000000000000000000, 0.000000000000000000, -1.000000000000000000 ) ) ;
#31548 = DIRECTION ( 'NONE',  ( 1.000000000000000000, -1.047444401652940007E-14, 0.000000000000000000 ) ) ;
#31549 = AXIS2_PLACEMENT_3D ( 'NONE', #47126, #43202, #20245 ) ;
#31550 = ADVANCED_FACE ( 'NONE', ( #29093 ), #50657, .T. ) ;
#31551 = LINE ( 'NONE', #26239, #68194 ) ;
#31552 = ORIENTED_EDGE ( 'NONE', *, *, #38511, .F. ) ;
#31553 = CARTESIAN_POINT ( 'NONE',  ( -8.393516549646712122, 5.655420232009161552, 195.0000000000000284 ) ) ;
#31554 = ORIENTED_EDGE ( 'NONE', *, *, #51989, .F. ) ;
#31555 = EDGE_CURVE ( 'NONE', #51662, #16082, #40993, .T. ) ;
#31556 = ORIENTED_EDGE ( 'NONE', *, *, #34937, .F. ) ;
#31557 = CIRCLE ( 'NONE', #24723, 0.3999999999993835154 ) ;
#31558 = DIRECTION ( 'NONE',  ( -1.000000000000000000, 0.000000000000000000, 0.000000000000000000 ) ) ;
#31559 = CARTESIAN_POINT ( 'NONE',  ( -28.00000000000000000, -16.28999999999710369, 14.50000000000000000 ) ) ;
#31560 = EDGE_CURVE ( 'NONE', #40309, #47485, #2220, .T. ) ;
#31561 = DIRECTION ( 'NONE',  ( -0.000000000000000000, -0.000000000000000000, -1.000000000000000000 ) ) ;
#31562 = EDGE_CURVE ( 'NONE', #58992, #61956, #9278, .T. ) ;
#31563 = CARTESIAN_POINT ( 'NONE',  ( -6.749999999999998224, 7.750000000000001776, 5.000000000000000000 ) ) ;
#31564 = VERTEX_POINT ( 'NONE', #31215 ) ;
#31565 = ORIENTED_EDGE ( 'NONE', *, *, #60854, .T. ) ;
#31567 = ORIENTED_EDGE ( 'NONE', *, *, #30831, .F. ) ;
#31566 = PLANE ( 'NONE',  #170 ) ;
#31568 = ORIENTED_EDGE ( 'NONE', *, *, #34026, .T. ) ;
#31569 = CARTESIAN_POINT ( 'NONE',  ( 8.249999999999996447, 8.250000000000001776, -5.000000000000000000 ) ) ;
#31570 = CARTESIAN_POINT ( 'NONE',  ( 7.250000000000005329, -7.249999999999998224, -14.00000000000000000 ) ) ;
#31571 = DIRECTION ( 'NONE',  ( 1.000000000000000000, -0.000000000000000000, 0.000000000000000000 ) ) ;
#31572 = EDGE_CURVE ( 'NONE', #24795, #50489, #26246, .T. ) ;
#31573 = ADVANCED_FACE ( 'NONE', ( #3270 ), #57363, .T. ) ;
#31574 = CARTESIAN_POINT ( 'NONE',  ( 4.456444791733522252E-16, 7.450000000000002842, -21.00000000000000000 ) ) ;
#31575 = VECTOR ( 'NONE', #9127, 1000.000000000000000 ) ;
#31577 = CARTESIAN_POINT ( 'NONE',  ( 6.344579767990805585, 8.393516549646626856, 195.0000000000000284 ) ) ;
#31576 = DIRECTION ( 'NONE',  ( 1.000000000000000000, -0.000000000000000000, 0.000000000000000000 ) ) ;
#31578 = VERTEX_POINT ( 'NONE', #3978 ) ;
#31579 = ORIENTED_EDGE ( 'NONE', *, *, #13491, .T. ) ;
#31580 = ORIENTED_EDGE ( 'NONE', *, *, #16075, .F. ) ;
#31581 = EDGE_CURVE ( 'NONE', #20102, #20187, #19183, .T. ) ;
#31582 = ADVANCED_FACE ( 'NONE', ( #36868 ), #62308, .F. ) ;
#31583 = CARTESIAN_POINT ( 'NONE',  ( -25.50000000000000355, 0.000000000000000000, -22.50000000000000000 ) ) ;
#31584 = FACE_OUTER_BOUND ( 'NONE', #61108, .T. ) ;
#31585 = ADVANCED_FACE ( 'NONE', ( #47115 ), #68686, .T. ) ;
#31586 = SHAPE_REPRESENTATION_RELATIONSHIP ( 'NONE' , 'NONE' ,  #64796, #34287 ) ;
#31587 = LINE ( 'NONE', #21668, #32019 ) ;
#31588 = CIRCLE ( 'NONE', #18021, 0.3499999999999996447 ) ;
#31589 = ORIENTED_EDGE ( 'NONE', *, *, #10170, .F. ) ;
#31590 = ORIENTED_EDGE ( 'NONE', *, *, #62041, .F. ) ;
#31591 = ORIENTED_EDGE ( 'NONE', *, *, #2909, .T. ) ;
#31592 = CARTESIAN_POINT ( 'NONE',  ( 3.682023737882818448, 9.722976262117203561, 54.00000000000000711 ) ) ;
#31593 = ORIENTED_EDGE ( 'NONE', *, *, #17318, .T. ) ;
#31594 = DIRECTION ( 'NONE',  ( 0.000000000000000000, 0.000000000000000000, -1.000000000000000000 ) ) ;
#31595 = ORIENTED_EDGE ( 'NONE', *, *, #38828, .F. ) ;
#31596 = VERTEX_POINT ( 'NONE', #35792 ) ;
#31597 = DIRECTION ( 'NONE',  ( -1.920885163218982051E-15, -1.000000000000000000, 0.000000000000000000 ) ) ;
#31598 = ADVANCED_FACE ( 'NONE', ( #51719 ), #63731, .T. ) ;
#31600 = VERTEX_POINT ( 'NONE', #46748 ) ;
#31599 = LINE ( 'NONE', #58818, #67268 ) ;
#31601 = AXIS2_PLACEMENT_3D ( 'NONE', #53644, #59285, #26076 ) ;
#31602 = ORIENTED_EDGE ( 'NONE', *, *, #10473, .T. ) ;
#31603 = AXIS2_PLACEMENT_3D ( 'NONE', #48436, #11962, #39201 ) ;
#31604 = EDGE_CURVE ( 'NONE', #68514, #16845, #52062, .T. ) ;
#31605 = CARTESIAN_POINT ( 'NONE',  ( 5.257023737882801306, 5.242976262117200470, 54.00000000000000711 ) ) ;
#31606 = CARTESIAN_POINT ( 'NONE',  ( 15.50000000000000000, -5.000000000000000000, -22.50000000000000000 ) ) ;
#31608 = ORIENTED_EDGE ( 'NONE', *, *, #56139, .F. ) ;
#31607 = LINE ( 'NONE', #69425, #62796 ) ;
#31609 = ORIENTED_EDGE ( 'NONE', *, *, #5385, .F. ) ;
#31610 = VECTOR ( 'NONE', #27953, 1000.000000000000114 ) ;
#31611 = CARTESIAN_POINT ( 'NONE',  ( 11.90000000000000036, 13.66939075806899240, -20.79999999999999361 ) ) ;
#31612 = CARTESIAN_POINT ( 'NONE',  ( 7.000000000000000000, -26.42999999999999972, -5.874955318979029784 ) ) ;
#31613 = DIRECTION ( 'NONE',  ( 0.000000000000000000, 1.000000000000000000, 0.000000000000000000 ) ) ;
#31614 = CYLINDRICAL_SURFACE ( 'NONE', #31214, 0.1749999999999989342 ) ;
#31615 = CIRCLE ( 'NONE', #14638, 5.250000000000000000 ) ;
#31616 = CARTESIAN_POINT ( 'NONE',  ( 7.450000000000003730, -7.249999999999997335, -22.50000000000000000 ) ) ;
#31617 = ORIENTED_EDGE ( 'NONE', *, *, #57568, .T. ) ;
#31618 = CARTESIAN_POINT ( 'NONE',  ( 275.0000000000000000, -26.42999999999999972, -9.412893218813501051 ) ) ;
#31619 = VECTOR ( 'NONE', #492, 1000.000000000000000 ) ;
#31620 = ORIENTED_EDGE ( 'NONE', *, *, #38452, .T. ) ;
#31621 = DIRECTION ( 'NONE',  ( 1.000000000000000000, -0.000000000000000000, 0.000000000000000000 ) ) ;
#31622 = SURFACE_STYLE_USAGE ( .BOTH. , #20295 ) ;
#31623 = DIRECTION ( 'NONE',  ( 0.000000000000000000, 0.000000000000000000, 1.000000000000000000 ) ) ;
#31624 = FACE_OUTER_BOUND ( 'NONE', #65839, .T. ) ;
#31625 = AXIS2_PLACEMENT_3D ( 'NONE', #14994, #3332, #68740 ) ;
#31626 = CARTESIAN_POINT ( 'NONE',  ( -16.75000000000000000, -2.500000000000000000, 23.22168783648699986 ) ) ;
#31627 = EDGE_LOOP ( 'NONE', ( #19224, #450, #46936, #1828 ) ) ;
#31628 = LINE ( 'NONE', #68754, #33640 ) ;
#31629 = PRESENTATION_STYLE_ASSIGNMENT (( #69804 ) ) ;
#31630 = EDGE_CURVE ( 'NONE', #31998, #11694, #13945, .T. ) ;
#31631 = DIRECTION ( 'NONE',  ( 0.000000000000000000, -0.000000000000000000, 1.000000000000000000 ) ) ;
#31632 = ORIENTED_EDGE ( 'NONE', *, *, #6499, .F. ) ;
#31633 = CIRCLE ( 'NONE', #67746, 1.000000000000000888 ) ;
#31634 = DIRECTION ( 'NONE',  ( 3.304235192336778667E-15, 1.000000000000000000, 0.000000000000000000 ) ) ;
#31635 = CARTESIAN_POINT ( 'NONE',  ( 0.9555237378827876604, -9.404523737882779955, 26.00000000000000000 ) ) ;
#31636 = CARTESIAN_POINT ( 'NONE',  ( 29.50000000000000355, -11.50000000000100009, -15.00000000000084910 ) ) ;
#31637 = EDGE_CURVE ( 'NONE', #49163, #62636, #17322, .T. ) ;
#31638 = CARTESIAN_POINT ( 'NONE',  ( -7.250000000000000888, 7.250000000000001776, -26.00000000000001066 ) ) ;
#31639 = DIRECTION ( 'NONE',  ( -0.000000000000000000, 0.000000000000000000, -1.000000000000000000 ) ) ;
#31640 = EDGE_LOOP ( 'NONE', ( #20262, #5519, #61643, #64894 ) ) ;
#31641 = LINE ( 'NONE', #64511, #62660 ) ;
#31642 = DIRECTION ( 'NONE',  ( 0.000000000000000000, -3.673940397442059868E-16, 1.000000000000000000 ) ) ;
#31643 = EDGE_CURVE ( 'NONE', #43706, #42184, #47799, .T. ) ;
#31644 = ADVANCED_FACE ( 'NONE', ( #36493 ), #3628, .F. ) ;
#31645 = CYLINDRICAL_SURFACE ( 'NONE', #5252, 0.3499999999998886224 ) ;
#31646 = ADVANCED_FACE ( 'NONE', ( #69023 ), #20231, .T. ) ;
#31647 = CARTESIAN_POINT ( 'NONE',  ( 7.250000000000005329, -7.249999999999998224, -25.00000000000000000 ) ) ;
#31648 = EDGE_CURVE ( 'NONE', #37548, #62567, #15288, .T. ) ;
#31649 = ORIENTED_EDGE ( 'NONE', *, *, #37894, .F. ) ;
#31650 = VECTOR ( 'NONE', #54609, 1000.000000000000000 ) ;
#31652 = ORIENTED_EDGE ( 'NONE', *, *, #60779, .T. ) ;
#31651 = CARTESIAN_POINT ( 'NONE',  ( 39.90000000000000568, -21.00000000000000000, 13.86939075806900057 ) ) ;
#31653 = VECTOR ( 'NONE', #36693, 1000.000000000000000 ) ;
#31654 = CIRCLE ( 'NONE', #1153, 3.500000000000003109 ) ;
#31655 = DIRECTION ( 'NONE',  ( -0.000000000000000000, -0.000000000000000000, -1.000000000000000000 ) ) ;
#31656 = DIRECTION ( 'NONE',  ( 0.000000000000000000, -1.000000000000000000, 0.000000000000000000 ) ) ;
#31657 = CARTESIAN_POINT ( 'NONE',  ( 2.369523737882786918, -9.562023737882798358, 54.00000000000000711 ) ) ;
#31658 = ORIENTED_EDGE ( 'NONE', *, *, #48565, .F. ) ;
#31659 = CIRCLE ( 'NONE', #2258, 0.2000000000000000944 ) ;
#31660 = LINE ( 'NONE', #64872, #37816 ) ;
#31661 = DIRECTION ( 'NONE',  ( -1.000000000000000000, 0.000000000000000000, 0.000000000000000000 ) ) ;
#31662 = ORIENTED_EDGE ( 'NONE', *, *, #32290, .F. ) ;
#31663 = ORIENTED_EDGE ( 'NONE', *, *, #13662, .T. ) ;
#31664 = VECTOR ( 'NONE', #39514, 1000.000000000000000 ) ;
#31665 = EDGE_LOOP ( 'NONE', ( #41278, #9210, #3810, #62263 ) ) ;
#31666 = VECTOR ( 'NONE', #66953, 1000.000000000000000 ) ;
#31667 = DIRECTION ( 'NONE',  ( -0.7071067811865446862, 0.7071067811865503483, 0.000000000000000000 ) ) ;
#31668 = AXIS2_PLACEMENT_3D ( 'NONE', #56573, #40660, #62936 ) ;
#31669 = CARTESIAN_POINT ( 'NONE',  ( 9.306483450353418618, 10.91351654964656426, 455.0000000000000568 ) ) ;
#31670 = DIRECTION ( 'NONE',  ( 0.000000000000000000, 0.000000000000000000, 1.000000000000000000 ) ) ;
#31671 = VERTEX_POINT ( 'NONE', #9632 ) ;
#31672 = ORIENTED_EDGE ( 'NONE', *, *, #33890, .F. ) ;
#31674 = CARTESIAN_POINT ( 'NONE',  ( 15.50000000000000000, -2.500000000000000000, -21.05662432702600029 ) ) ;
#31673 = VECTOR ( 'NONE', #52756, 1000.000000000000000 ) ;
#31675 = VECTOR ( 'NONE', #49407, 1000.000000000000000 ) ;
#31676 = ORIENTED_EDGE ( 'NONE', *, *, #25495, .F. ) ;
#31677 = ORIENTED_EDGE ( 'NONE', *, *, #63584, .T. ) ;
#31678 = ORIENTED_EDGE ( 'NONE', *, *, #29531, .T. ) ;
#31679 = ORIENTED_EDGE ( 'NONE', *, *, #36583, .F. ) ;
#31680 = DIRECTION ( 'NONE',  ( 0.000000000000000000, 0.000000000000000000, 1.000000000000000000 ) ) ;
#31681 = UNCERTAINTY_MEASURE_WITH_UNIT (LENGTH_MEASURE( 1.000000000000000082E-05 ), #38648, 'distance_accuracy_value', 'NONE');
#31683 = ORIENTED_EDGE ( 'NONE', *, *, #29933, .T. ) ;
#31682 = DIRECTION ( 'NONE',  ( 1.000000000000000000, -0.000000000000000000, -0.000000000000000000 ) ) ;
#31684 = DIRECTION ( 'NONE',  ( 0.000000000000000000, 0.000000000000000000, 1.000000000000000000 ) ) ;
#31685 = EDGE_CURVE ( 'NONE', #41344, #17425, #48942, .T. ) ;
#31686 = CARTESIAN_POINT ( 'NONE',  ( -7.250000000000000888, 7.450000000000003730, -17.50000000000000000 ) ) ;
#31687 = VECTOR ( 'NONE', #20100, 1000.000000000000000 ) ;
#31688 = DIRECTION ( 'NONE',  ( 1.000000000000000000, -0.000000000000000000, -0.000000000000000000 ) ) ;
#31689 = VERTEX_POINT ( 'NONE', #15983 ) ;
#31690 = EDGE_CURVE ( 'NONE', #60747, #16870, #16688, .T. ) ;
#31691 = EDGE_LOOP ( 'NONE', ( #35128, #36760, #3782, #21963 ) ) ;
#31692 = CARTESIAN_POINT ( 'NONE',  ( -7.955476262117324282, -9.562023737882771712, 54.00000000000000711 ) ) ;
#31693 = AXIS2_PLACEMENT_3D ( 'NONE', #36461, #53789, #47768 ) ;
#31694 = DIRECTION ( 'NONE',  ( -1.000000000000000000, 0.000000000000000000, 0.000000000000000000 ) ) ;
#31695 = AXIS2_PLACEMENT_3D ( 'NONE', #64385, #15938, #37510 ) ;
#31696 = ORIENTED_EDGE ( 'NONE', *, *, #34633, .T. ) ;
#31697 = AXIS2_PLACEMENT_3D ( 'NONE', #30100, #51680, #57325 ) ;
#31698 = CARTESIAN_POINT ( 'NONE',  ( 7.450000000000004619, -1.336933437520057563E-15, -16.50000000000000000 ) ) ;
#31699 = LINE ( 'NONE', #38384, #44892 ) ;
#31700 = SURFACE_STYLE_FILL_AREA ( #37010 ) ;
#31701 = ORIENTED_EDGE ( 'NONE', *, *, #4546, .T. ) ;
#31702 = CARTESIAN_POINT ( 'NONE',  ( 11.32648345035337734, -4.206483450353492692, 455.0000000000000568 ) ) ;
#31704 = CARTESIAN_POINT ( 'NONE',  ( -4.947141984184534991, -7.357023737882802727, 26.00000000000000711 ) ) ;
#31703 = VECTOR ( 'NONE', #3613, 1000.000000000000000 ) ;
#31705 = CARTESIAN_POINT ( 'NONE',  ( 7.000000000000000000, -26.50000000000000000, -5.809475019311129529 ) ) ;
#31706 = DIRECTION ( 'NONE',  ( -2.135044278125301343E-15, 1.000000000000000000, 0.000000000000000000 ) ) ;
#31707 = VECTOR ( 'NONE', #57881, 1000.000000000000000 ) ;
#31708 = FACE_OUTER_BOUND ( 'NONE', #66245, .T. ) ;
#31709 = ORIENTED_EDGE ( 'NONE', *, *, #6208, .F. ) ;
#31710 = CARTESIAN_POINT ( 'NONE',  ( 3.606483450353406450, 7.415254214038213831, 455.0000000000000568 ) ) ;
#31711 = DIRECTION ( 'NONE',  ( -1.000000000000000000, 0.000000000000000000, 0.000000000000000000 ) ) ;
#31712 = CARTESIAN_POINT ( 'NONE',  ( -2.406732575409589625, 8.697938382363036069, 26.00000000000000711 ) ) ;
#31713 = CARTESIAN_POINT ( 'NONE',  ( 39.90000000000000568, 4.286263797015736595E-16, -3.500000000000000000 ) ) ;
#31714 = EDGE_CURVE ( 'NONE', #37597, #17477, #22975, .T. ) ;
#31715 = ORIENTED_EDGE ( 'NONE', *, *, #40326, .T. ) ;
#31716 = DIRECTION ( 'NONE',  ( 1.000000000000000000, 0.000000000000000000, 0.000000000000000000 ) ) ;
#31717 = LINE ( 'NONE', #68492, #59058 ) ;
#31718 = AXIS2_PLACEMENT_3D ( 'NONE', #22978, #44532, #34265 ) ;
#31719 = DIRECTION ( 'NONE',  ( -1.000000000000000000, 0.000000000000000000, 0.000000000000000000 ) ) ;
#31720 = CARTESIAN_POINT ( 'NONE',  ( -9.722976262117256852, 2.530476262117183683, 54.00000000000000711 ) ) ;
#31721 = ORIENTED_EDGE ( 'NONE', *, *, #66181, .F. ) ;
#31722 = CARTESIAN_POINT ( 'NONE',  ( -8.250000000000001776, -7.249999999999998224, -13.00000000000000178 ) ) ;
#31723 = CARTESIAN_POINT ( 'NONE',  ( 39.00000000000000000, 6.123233995736766282E-16, -5.000000000000000000 ) ) ;
#31724 = CARTESIAN_POINT ( 'NONE',  ( -4.188533722949421723, -7.272650909786664286, 455.0000000000000568 ) ) ;
#31725 = CARTESIAN_POINT ( 'NONE',  ( 8.250000000000005329, 7.250000000000000888, -26.00000000000001066 ) ) ;
#31726 = CARTESIAN_POINT ( 'NONE',  ( 8.241237374594303944, -1.634292677759887846, 54.00000000000000711 ) ) ;
#31727 = EDGE_CURVE ( 'NONE', #55220, #59753, #52318, .T. ) ;
#31728 = DIRECTION ( 'NONE',  ( 1.000000000000000000, 0.000000000000000000, 0.000000000000000000 ) ) ;
#31729 = EDGE_CURVE ( 'NONE', #50148, #27481, #62479, .T. ) ;
#31730 = ORIENTED_EDGE ( 'NONE', *, *, #58713, .F. ) ;
#31731 = VERTEX_POINT ( 'NONE', #31904 ) ;
#31732 = ADVANCED_FACE ( 'NONE', ( #54855 ), #65129, .T. ) ;
#31733 = FACE_OUTER_BOUND ( 'NONE', #38463, .T. ) ;
#31734 = VECTOR ( 'NONE', #4200, 1000.000000000000000 ) ;
#31735 = CARTESIAN_POINT ( 'NONE',  ( -7.793516549646827940, -11.12648345035340647, 455.0000000000000568 ) ) ;
#31736 = ORIENTED_EDGE ( 'NONE', *, *, #14348, .F. ) ;
#31737 = DIRECTION ( 'NONE',  ( 0.000000000000000000, 1.000000000000000000, 0.000000000000000000 ) ) ;
#31738 = CARTESIAN_POINT ( 'NONE',  ( 4.396432944014529554, 8.393516549646633962, 195.0000000000000284 ) ) ;
#31739 = ORIENTED_EDGE ( 'NONE', *, *, #26347, .F. ) ;
#31740 = CARTESIAN_POINT ( 'NONE',  ( -5.993516549646711766, 5.993516549646603409, 195.0000000000000284 ) ) ;
#31741 = VERTEX_POINT ( 'NONE', #17022 ) ;
#31742 = ORIENTED_EDGE ( 'NONE', *, *, #68292, .F. ) ;
#31743 = CARTESIAN_POINT ( 'NONE',  ( 7.826483450353380000, -11.78648345035349010, 455.0000000000000568 ) ) ;
#31744 = AXIS2_PLACEMENT_3D ( 'NONE', #23653, #18338, #39905 ) ;
#31745 = ORIENTED_EDGE ( 'NONE', *, *, #36428, .T. ) ;
#31746 = CARTESIAN_POINT ( 'NONE',  ( -30.00000000000000000, -9.454754784057099570, -17.53999999999999915 ) ) ;
#31747 = CARTESIAN_POINT ( 'NONE',  ( -29.25000000000000000, -5.000000000000000000, 11.75000000000000000 ) ) ;
#31748 = VECTOR ( 'NONE', #33834, 1000.000000000000000 ) ;
#31750 = LINE ( 'NONE', #4870, #23108 ) ;
#31749 = VECTOR ( 'NONE', #14665, 1000.000000000000000 ) ;
#31751 = VERTEX_POINT ( 'NONE', #6416 ) ;
#31752 = ORIENTED_EDGE ( 'NONE', *, *, #62051, .T. ) ;
#31753 = AXIS2_PLACEMENT_3D ( 'NONE', #61155, #12711, #50571 ) ;
#31754 = LINE ( 'NONE', #40937, #8678 ) ;
#31756 = LINE ( 'NONE', #5234, #41224 ) ;
#31755 = LINE ( 'NONE', #37403, #3341 ) ;
#31757 = ORIENTED_EDGE ( 'NONE', *, *, #8892, .F. ) ;
#31758 = ORIENTED_EDGE ( 'NONE', *, *, #22005, .T. ) ;
#31759 = AXIS2_PLACEMENT_3D ( 'NONE', #18133, #61609, #8220 ) ;
#31760 = AXIS2_PLACEMENT_3D ( 'NONE', #19364, #14770, #8395 ) ;
#31762 = ORIENTED_EDGE ( 'NONE', *, *, #37220, .F. ) ;
#31761 = APPLICATION_PROTOCOL_DEFINITION ( 'draft international standard', 'automotive_design', 1998, #66133 ) ;
#31763 = CARTESIAN_POINT ( 'NONE',  ( -7.250000000000000000, -7.449999999999998401, -20.50000000000000000 ) ) ;
#31765 = EDGE_LOOP ( 'NONE', ( #4130, #58721, #9673, #3610 ) ) ;
#31764 = LINE ( 'NONE', #58970, #59086 ) ;
#31766 = VECTOR ( 'NONE', #41547, 1000.000000000000000 ) ;
#31767 = PLANE ( 'NONE',  #29971 ) ;
#31768 = DIRECTION ( 'NONE',  ( 1.836970198721029934E-16, 1.836970198721010706E-16, -1.000000000000000000 ) ) ;
#31769 = VERTEX_POINT ( 'NONE', #27981 ) ;
#31770 = VERTEX_POINT ( 'NONE', #417 ) ;
#31771 = EDGE_CURVE ( 'NONE', #10965, #15214, #53826, .T. ) ;
#31772 = EDGE_CURVE ( 'NONE', #45585, #62156, #11026, .T. ) ;
#31773 = EDGE_CURVE ( 'NONE', #4905, #48072, #69374, .T. ) ;
#31774 = VECTOR ( 'NONE', #26477, 1000.000000000000000 ) ;
#31775 = DIRECTION ( 'NONE',  ( -0.000000000000000000, 0.000000000000000000, 1.000000000000000000 ) ) ;
#31776 = ORIENTED_EDGE ( 'NONE', *, *, #16592, .F. ) ;
#31777 = EDGE_CURVE ( 'NONE', #45123, #30361, #36512, .T. ) ;
#31778 = CARTESIAN_POINT ( 'NONE',  ( 10.92648345035337343, -9.306483450353493225, 455.0000000000000568 ) ) ;
#31779 = CARTESIAN_POINT ( 'NONE',  ( -5.538810540050023157, 7.342976262117183239, 26.00000000000000711 ) ) ;
#31780 = LINE ( 'NONE', #26122, #20421 ) ;
#31781 = ORIENTED_EDGE ( 'NONE', *, *, #42488, .F. ) ;
#31782 = DIRECTION ( 'NONE',  ( 0.000000000000000000, 1.000000000000000000, 0.000000000000000000 ) ) ;
#31783 = AXIS2_PLACEMENT_3D ( 'NONE', #29913, #19649, #67043 ) ;
#31785 = ORIENTED_EDGE ( 'NONE', *, *, #50874, .F. ) ;
#31784 =( LENGTH_UNIT ( ) NAMED_UNIT ( * ) SI_UNIT ( .MILLI., .METRE. ) );
#31787 = ORIENTED_EDGE ( 'NONE', *, *, #46377, .F. ) ;
#31786 = LINE ( 'NONE', #54650, #56870 ) ;
#31788 = CARTESIAN_POINT ( 'NONE',  ( -7.250000000000000888, 7.250000000000001776, -19.50000000000000000 ) ) ;
#31789 = DIRECTION ( 'NONE',  ( -1.000000000000000000, 3.016910393003147986E-15, 1.108394896831706469E-30 ) ) ;
#31790 = CYLINDRICAL_SURFACE ( 'NONE', #69731, 1.000000000000001776 ) ;
#31791 = CARTESIAN_POINT ( 'NONE',  ( 0.000000000000000000, 0.000000000000000000, -5.000000000000000000 ) ) ;
#31792 = FACE_OUTER_BOUND ( 'NONE', #62528, .T. ) ;
#31793 = ORIENTED_EDGE ( 'NONE', *, *, #30606, .T. ) ;
#31794 = CARTESIAN_POINT ( 'NONE',  ( 8.606483450353406894, 7.603567055985405609, 455.0000000000000568 ) ) ;
#31795 = CARTESIAN_POINT ( 'NONE',  ( 7.000000000000000000, -39.79999999999905214, -12.19999999999906315 ) ) ;
#31796 = AXIS2_PLACEMENT_3D ( 'NONE', #42901, #16040, #37610 ) ;
#31797 = PLANE ( 'NONE',  #51493 ) ;
#31799 = ORIENTED_EDGE ( 'NONE', *, *, #69015, .F. ) ;
#31798 = CARTESIAN_POINT ( 'NONE',  ( 2.906483450353349429, -10.09643294401453950, 195.0000000000000284 ) ) ;
#31800 = PRODUCT_DEFINITION_SHAPE ( 'NONE', 'NONE',  #69990 ) ;
#31801 = CIRCLE ( 'NONE', #1295, 24.99999999998794920 ) ;
#31802 = DIRECTION ( 'NONE',  ( 0.000000000000000000, 1.000000000000000000, 0.000000000000000000 ) ) ;
#31803 = CARTESIAN_POINT ( 'NONE',  ( 7.357023737882817827, -6.665817930929295088, 26.00000000000000000 ) ) ;
#31804 = CARTESIAN_POINT ( 'NONE',  ( -11.00000000000000000, -10.85999999999999943, -9.350000000000269651 ) ) ;
#31805 = DIRECTION ( 'NONE',  ( 0.000000000000000000, 1.000000000000000000, 0.000000000000000000 ) ) ;
#31806 = ORIENTED_EDGE ( 'NONE', *, *, #10433, .T. ) ;
#31807 = CARTESIAN_POINT ( 'NONE',  ( 40.90000000000000568, 0.000000000000000000, 0.000000000000000000 ) ) ;
#31808 = CARTESIAN_POINT ( 'NONE',  ( 50.83090410532631864, 3.657408540445007628, 10.00000000000000000 ) ) ;
#31809 = ORIENTED_EDGE ( 'NONE', *, *, #34549, .F. ) ;
#31810 = CYLINDRICAL_SURFACE ( 'NONE', #39068, 0.1999999999999987899 ) ;
#31811 = AXIS2_PLACEMENT_3D ( 'NONE', #60145, #65804, #49208 ) ;
#31812 = AXIS2_PLACEMENT_3D ( 'NONE', #38169, #20496, #42063 ) ;
#31813 = LINE ( 'NONE', #59366, #54977 ) ;
#31814 = LINE ( 'NONE', #47360, #3882 ) ;
#31815 = DIRECTION ( 'NONE',  ( -0.7142857142857395036, 0.000000000000000000, -0.6998542122237394469 ) ) ;
#31816 = EDGE_CURVE ( 'NONE', #6182, #48126, #15643, .T. ) ;
#31817 = CARTESIAN_POINT ( 'NONE',  ( 275.2500000000001137, -0.2499999999999431288, -26.74999999999993250 ) ) ;
#31818 = ORIENTED_EDGE ( 'NONE', *, *, #11856, .F. ) ;
#31819 = EDGE_CURVE ( 'NONE', #7937, #51374, #34207, .T. ) ;
#31820 = ORIENTED_EDGE ( 'NONE', *, *, #29577, .T. ) ;
#31821 = DIRECTION ( 'NONE',  ( -0.000000000000000000, -0.000000000000000000, -1.000000000000000000 ) ) ;
#31822 = ORIENTED_EDGE ( 'NONE', *, *, #32287, .T. ) ;
#31823 = ADVANCED_FACE ( 'NONE', ( #32934 ), #43885, .F. ) ;
#31824 = EDGE_LOOP ( 'NONE', ( #34923, #17692, #55305, #61259 ) ) ;
#31825 = DIRECTION ( 'NONE',  ( -0.000000000000000000, 1.000000000000000000, -0.000000000000000000 ) ) ;
#31826 = AXIS2_PLACEMENT_3D ( 'NONE', #10396, #66215, #39337 ) ;
#31827 = EDGE_CURVE ( 'NONE', #23661, #32632, #54172, .T. ) ;
#31828 = DIRECTION ( 'NONE',  ( 0.000000000000000000, 0.000000000000000000, 1.000000000000000000 ) ) ;
#31829 = DIRECTION ( 'NONE',  ( 0.000000000000000000, -0.7071067811865077157, 0.7071067811865873187 ) ) ;
#31830 = VERTEX_POINT ( 'NONE', #22343 ) ;
#31831 = EDGE_CURVE ( 'NONE', #56310, #69782, #24083, .T. ) ;
#31832 = VERTEX_POINT ( 'NONE', #53474 ) ;
#31833 = DIRECTION ( 'NONE',  ( 0.7071067811865451302, -0.7071067811865500152, -2.597868168706484048E-16 ) ) ;
#31835 = ORIENTED_EDGE ( 'NONE', *, *, #66271, .T. ) ;
#31834 = EDGE_CURVE ( 'NONE', #32632, #12243, #65465, .T. ) ;
#31836 = EDGE_LOOP ( 'NONE', ( #48704, #55069, #68630, #43687 ) ) ;
#31837 = CARTESIAN_POINT ( 'NONE',  ( 15.29686605390242526, -0.2715358723600077018, -23.82609623451301317 ) ) ;
#31838 = DIRECTION ( 'NONE',  ( 1.000000000000000000, 0.000000000000000000, 0.000000000000000000 ) ) ;
#31839 = CARTESIAN_POINT ( 'NONE',  ( -3.667976262117330410, -9.912023737882817542, 54.00000000000000711 ) ) ;
#31840 = VECTOR ( 'NONE', #10031, 1000.000000000000000 ) ;
#31841 = ORIENTED_EDGE ( 'NONE', *, *, #1580, .F. ) ;
#31842 = DIRECTION ( 'NONE',  ( -1.000000000000000000, 0.000000000000000000, 0.000000000000000000 ) ) ;
#31844 = CYLINDRICAL_SURFACE ( 'NONE', #17654, 1.000000000000000888 ) ;
#31843 = DIRECTION ( 'NONE',  ( 0.000000000000000000, 0.000000000000000000, 1.000000000000000000 ) ) ;
#31845 = VERTEX_POINT ( 'NONE', #78 ) ;
#31847 = VERTEX_POINT ( 'NONE', #32239 ) ;
#31846 = DIRECTION ( 'NONE',  ( 2.478176394252584099E-15, 1.000000000000000000, 0.000000000000000000 ) ) ;
#31848 = ORIENTED_EDGE ( 'NONE', *, *, #11906, .T. ) ;
#31849 = CARTESIAN_POINT ( 'NONE',  ( 40.90000000000000568, -14.48845687959340012, 21.00000000000000000 ) ) ;
#31850 = VECTOR ( 'NONE', #41060, 1000.000000000000114 ) ;
#31851 = DIRECTION ( 'NONE',  ( 0.000000000000000000, 0.000000000000000000, -1.000000000000000000 ) ) ;
#31852 = MECHANICAL_DESIGN_GEOMETRIC_PRESENTATION_REPRESENTATION (  '', ( #28384 ), #14883 ) ;
#31853 = ORIENTED_EDGE ( 'NONE', *, *, #27644, .T. ) ;
#31854 = CARTESIAN_POINT ( 'NONE',  ( -8.250000000000001776, 0.000000000000000000, -19.50000000000000000 ) ) ;
#31855 = CARTESIAN_POINT ( 'NONE',  ( -30.00000000000000000, -14.04000000000000092, -17.04524521594300523 ) ) ;
#31856 = ORIENTED_EDGE ( 'NONE', *, *, #38043, .F. ) ;
#31857 = AXIS2_PLACEMENT_3D ( 'NONE', #23888, #18575, #40493 ) ;
#31858 = VECTOR ( 'NONE', #27538, 1000.000000000000000 ) ;
#31859 = VERTEX_POINT ( 'NONE', #5392 ) ;
#31860 = DIRECTION ( 'NONE',  ( 0.000000000000000000, 1.000000000000000000, 0.000000000000000000 ) ) ;
#31861 = LINE ( 'NONE', #37169, #25613 ) ;
#31862 = LINE ( 'NONE', #32196, #52 ) ;
#31863 = VERTEX_POINT ( 'NONE', #26948 ) ;
#31864 = AXIS2_PLACEMENT_3D ( 'NONE', #57288, #47378, #31485 ) ;
#31865 = LINE ( 'NONE', #65083, #27850 ) ;
#31866 = CARTESIAN_POINT ( 'NONE',  ( -11.00000000000000000, -5.599999999999999645, -9.000000000000001776 ) ) ;
#31868 = ORIENTED_EDGE ( 'NONE', *, *, #12781, .T. ) ;
#31867 = FACE_OUTER_BOUND ( 'NONE', #28398, .T. ) ;
#31870 = ORIENTED_EDGE ( 'NONE', *, *, #6716, .F. ) ;
#31869 = CARTESIAN_POINT ( 'NONE',  ( -2.406732575409590069, 8.697938382363036069, 54.00000000000000711 ) ) ;
#31872 = FACE_OUTER_BOUND ( 'NONE', #63659, .T. ) ;
#31871 = VECTOR ( 'NONE', #754, 1000.000000000000000 ) ;
#31873 = EDGE_CURVE ( 'NONE', #42019, #42376, #51185, .T. ) ;
#31874 = LINE ( 'NONE', #5358, #21693 ) ;
#31875 = DIRECTION ( 'NONE',  ( 1.000000000000000000, 3.016910393003147986E-15, 1.108394896831706469E-30 ) ) ;
#31876 = DIRECTION ( 'NONE',  ( 0.000000000000000000, 0.000000000000000000, 1.000000000000000000 ) ) ;
#31877 = DIRECTION ( 'NONE',  ( -1.000000000000000000, -1.570596175624152290E-15, 0.000000000000000000 ) ) ;
#31878 = EDGE_CURVE ( 'NONE', #8233, #5332, #33959, .T. ) ;
#31879 = DIRECTION ( 'NONE',  ( -1.000000000000000000, 0.000000000000000000, 0.000000000000000000 ) ) ;
#31880 = ORIENTED_EDGE ( 'NONE', *, *, #13183, .F. ) ;
#31881 = CARTESIAN_POINT ( 'NONE',  ( -11.50000000000000000, -11.50000000000100009, 15.00000000000084910 ) ) ;
#31883 = ORIENTED_EDGE ( 'NONE', *, *, #47027, .T. ) ;
#31882 = DIRECTION ( 'NONE',  ( -1.000000000000000000, 0.000000000000000000, 0.000000000000000000 ) ) ;
#31884 = CARTESIAN_POINT ( 'NONE',  ( -3.667976262117323305, -9.737023737882815055, 26.00000000000000000 ) ) ;
#31885 = FILL_AREA_STYLE_COLOUR ( '', #12018 ) ;
#31886 = PLANE ( 'NONE',  #28404 ) ;
#31887 = ORIENTED_EDGE ( 'NONE', *, *, #38883, .F. ) ;
#31888 = DIRECTION ( 'NONE',  ( -1.000000000000000000, 0.000000000000000000, 0.000000000000000000 ) ) ;
#31889 = FACE_OUTER_BOUND ( 'NONE', #27050, .T. ) ;
#31890 = AXIS2_PLACEMENT_3D ( 'NONE', #51877, #61066, #50475 ) ;
#31891 = ADVANCED_FACE ( 'NONE', ( #40573 ), #41270, .T. ) ;
#31892 = ORIENTED_EDGE ( 'NONE', *, *, #48082, .F. ) ;
#31893 = LINE ( 'NONE', #404, #40197 ) ;
#31894 = LINE ( 'NONE', #5015, #38206 ) ;
#31895 = VECTOR ( 'NONE', #26832, 1000.000000000000000 ) ;
#31896 = CYLINDRICAL_SURFACE ( 'NONE', #11591, 0.1749999999999998224 ) ;
#31897 = EDGE_LOOP ( 'NONE', ( #5390, #5591, #22944, #44675 ) ) ;
#31898 = EDGE_CURVE ( 'NONE', #54850, #43836, #67460, .T. ) ;
#31899 = DIRECTION ( 'NONE',  ( 0.000000000000000000, 0.000000000000000000, 1.000000000000000000 ) ) ;
#31900 = VERTEX_POINT ( 'NONE', #55197 ) ;
#31901 = ORIENTED_EDGE ( 'NONE', *, *, #1989, .F. ) ;
#31902 = CIRCLE ( 'NONE', #37551, 3.500000000000000444 ) ;
#31903 = CARTESIAN_POINT ( 'NONE',  ( -9.390476262117209316, -1.480523737882732060, 54.00000000000000711 ) ) ;
#31904 = CARTESIAN_POINT ( 'NONE',  ( 7.757955312929553315, 8.452095193409265406, 455.0000000000000568 ) ) ;
#31905 = VECTOR ( 'NONE', #28080, 1000.000000000000000 ) ;
#31906 = DIRECTION ( 'NONE',  ( 0.000000000000000000, 0.000000000000000000, 1.000000000000000000 ) ) ;
#31907 = DIRECTION ( 'NONE',  ( 0.000000000000000000, -1.000000000000000000, 0.000000000000000000 ) ) ;
#31908 = ORIENTED_EDGE ( 'NONE', *, *, #66355, .F. ) ;
#31909 = ADVANCED_FACE ( 'NONE', ( #29964 ), #51893, .F. ) ;
#31910 = ORIENTED_EDGE ( 'NONE', *, *, #8799, .F. ) ;
#31912 = ORIENTED_EDGE ( 'NONE', *, *, #28929, .F. ) ;
#31911 = CARTESIAN_POINT ( 'NONE',  ( 3.157023737882792780, 4.031976262117212606, 26.00000000000000711 ) ) ;
#31914 = ORIENTED_EDGE ( 'NONE', *, *, #19497, .T. ) ;
#31913 = EDGE_CURVE ( 'NONE', #47996, #34611, #33626, .T. ) ;
#31915 = DIRECTION ( 'NONE',  ( -0.000000000000000000, 3.673940397442059868E-16, -1.000000000000000000 ) ) ;
#31916 = FACE_OUTER_BOUND ( 'NONE', #12385, .T. ) ;
#31917 = DIRECTION ( 'NONE',  ( 0.000000000000000000, 0.000000000000000000, -1.000000000000000000 ) ) ;
#31918 = VECTOR ( 'NONE', #57175, 1000.000000000000000 ) ;
#31919 = CARTESIAN_POINT ( 'NONE',  ( 30.90000000000000213, 20.60000000000000142, -13.86939075806900057 ) ) ;
#31921 = CARTESIAN_POINT ( 'NONE',  ( 24.90000000000000213, 13.66939075806899950, 20.80000000000000426 ) ) ;
#31920 = DIRECTION ( 'NONE',  ( 0.000000000000000000, 0.000000000000000000, 1.000000000000000000 ) ) ;
#31922 = VERTEX_POINT ( 'NONE', #57537 ) ;
#31923 = VERTEX_POINT ( 'NONE', #62131 ) ;
#31924 = ORIENTED_EDGE ( 'NONE', *, *, #586, .T. ) ;
#31925 = ORIENTED_EDGE ( 'NONE', *, *, #39425, .T. ) ;
#31926 = DIRECTION ( 'NONE',  ( -1.000000000000000000, -0.000000000000000000, -0.000000000000000000 ) ) ;
#31927 = DIRECTION ( 'NONE',  ( 0.000000000000000000, 0.000000000000000000, -1.000000000000000000 ) ) ;
#31928 = CARTESIAN_POINT ( 'NONE',  ( 7.450000000000003730, -7.249999999999997335, -8.500000000000000000 ) ) ;
#31929 = EDGE_LOOP ( 'NONE', ( #49053, #42564, #18930, #56948 ) ) ;
#31930 = VERTEX_POINT ( 'NONE', #45879 ) ;
#31931 = ORIENTED_EDGE ( 'NONE', *, *, #63074, .T. ) ;
#31932 = LINE ( 'NONE', #59145, #65536 ) ;
#31933 = ORIENTED_EDGE ( 'NONE', *, *, #53670, .T. ) ;
#31934 = DIRECTION ( 'NONE',  ( 0.000000000000000000, 0.000000000000000000, -1.000000000000000000 ) ) ;
#31935 = CARTESIAN_POINT ( 'NONE',  ( 33.89999999999999858, 20.60000000000000142, 2.801416793502919355E-15 ) ) ;
#31936 = AXIS2_PLACEMENT_3D ( 'NONE', #42309, #63886, #63543 ) ;
#31937 = ORIENTED_EDGE ( 'NONE', *, *, #61496, .T. ) ;
#31938 = EDGE_CURVE ( 'NONE', #66510, #4435, #9102, .T. ) ;
#31939 = VERTEX_POINT ( 'NONE', #65802 ) ;
#31940 = CARTESIAN_POINT ( 'NONE',  ( 12.00648345035336284, 7.813516549646607245, 195.0000000000000284 ) ) ;
#31941 = AXIS2_PLACEMENT_3D ( 'NONE', #38055, #20382, #16123 ) ;
#31943 = ORIENTED_EDGE ( 'NONE', *, *, #46598, .F. ) ;
#31942 = DIRECTION ( 'NONE',  ( 0.000000000000000000, 0.000000000000000000, 1.000000000000000000 ) ) ;
#31944 = ORIENTED_EDGE ( 'NONE', *, *, #50070, .T. ) ;
#31945 = EDGE_CURVE ( 'NONE', #61504, #53333, #14414, .T. ) ;
#31946 = DIRECTION ( 'NONE',  ( 0.000000000000000000, 0.000000000000000000, 1.000000000000000000 ) ) ;
#31947 = ADVANCED_FACE ( 'NONE', ( #13701 ), #49544, .F. ) ;
#31949 = ORIENTED_EDGE ( 'NONE', *, *, #40526, .F. ) ;
#31948 = DIRECTION ( 'NONE',  ( -0.000000000000000000, -0.000000000000000000, 1.000000000000000000 ) ) ;
#31950 = ORIENTED_EDGE ( 'NONE', *, *, #30341, .F. ) ;
#31951 = CARTESIAN_POINT ( 'NONE',  ( 3.606483450353350051, 4.609516549646638595, 195.0000000000000284 ) ) ;
#31952 = LINE ( 'NONE', #6115, #48153 ) ;
#31953 = EDGE_CURVE ( 'NONE', #21660, #11628, #38929, .T. ) ;
#31954 = DIRECTION ( 'NONE',  ( -1.836970198721029934E-16, 1.836970198721036344E-16, -1.000000000000000000 ) ) ;
#31955 = LINE ( 'NONE', #48221, #2977 ) ;
#31956 = LINE ( 'NONE', #69792, #58722 ) ;
#31957 = ADVANCED_FACE ( 'NONE', ( #12379 ), #6744, .T. ) ;
#31958 = ORIENTED_EDGE ( 'NONE', *, *, #21816, .F. ) ;
#31959 = CARTESIAN_POINT ( 'NONE',  ( -7.450000000000001954, -7.249999999999998224, -11.50000000000000000 ) ) ;
#31960 = VERTEX_POINT ( 'NONE', #17712 ) ;
#31961 = CARTESIAN_POINT ( 'NONE',  ( -3.593516549646712299, 4.609516549646604844, 455.0000000000000568 ) ) ;
#31962 = CIRCLE ( 'NONE', #38753, 1.620999999999997332 ) ;
#31963 = CARTESIAN_POINT ( 'NONE',  ( 16.75000000000000000, -0.2714405302574886547, 22.01253933645462624 ) ) ;
#31964 = EDGE_CURVE ( 'NONE', #14096, #18237, #40918, .T. ) ;
#31965 = CARTESIAN_POINT ( 'NONE',  ( 40.90000000000000568, -14.06939075806900874, 20.80000000000001137 ) ) ;
#31966 = EDGE_CURVE ( 'NONE', #35449, #62948, #24766, .T. ) ;
#31968 = DIRECTION ( 'NONE',  ( 0.000000000000000000, -1.000000000000000000, 0.000000000000000000 ) ) ;
#31967 = VECTOR ( 'NONE', #40828, 1000.000000000000114 ) ;
#31969 = CIRCLE ( 'NONE', #61300, 1.000000000000000000 ) ;
#31970 = CARTESIAN_POINT ( 'NONE',  ( -2.693516549646675529, 10.91351654964657314, 455.0000000000000568 ) ) ;
#31971 = EDGE_CURVE ( 'NONE', #26273, #49178, #62474, .T. ) ;
#31972 = EDGE_CURVE ( 'NONE', #58217, #35004, #3105, .T. ) ;
#31973 = EDGE_CURVE ( 'NONE', #2132, #32328, #28653, .T. ) ;
#31974 = ORIENTED_EDGE ( 'NONE', *, *, #56460, .T. ) ;
#31975 = DIRECTION ( 'NONE',  ( 0.000000000000000000, 1.000000000000000000, 0.000000000000000000 ) ) ;
#31976 = VECTOR ( 'NONE', #33924, 1000.000000000000114 ) ;
#31977 = EDGE_CURVE ( 'NONE', #46313, #38349, #50232, .T. ) ;
#31978 = VECTOR ( 'NONE', #21248, 1000.000000000000000 ) ;
#31979 = EDGE_LOOP ( 'NONE', ( #52906, #52103, #47437, #7809 ) ) ;
#31980 = EDGE_CURVE ( 'NONE', #24537, #27925, #37253, .T. ) ;
#31981 = CARTESIAN_POINT ( 'NONE',  ( 11.78648345035337819, -4.186483450353492231, 455.0000000000000568 ) ) ;
#31982 = LINE ( 'NONE', #863, #20774 ) ;
#31983 = DIRECTION ( 'NONE',  ( 0.000000000000000000, 0.000000000000000000, 1.000000000000000000 ) ) ;
#31984 = ORIENTED_EDGE ( 'NONE', *, *, #22319, .F. ) ;
#31985 = CARTESIAN_POINT ( 'NONE',  ( -14.25000000000000000, -0.3156864504677174277, 22.74361999681791247 ) ) ;
#31986 = CARTESIAN_POINT ( 'NONE',  ( 8.406483450353398723, 5.655420232009111814, 455.0000000000000568 ) ) ;
#31987 = EDGE_LOOP ( 'NONE', ( #34901, #50080, #1526, #40405 ) ) ;
#31988 = LINE ( 'NONE', #43276, #44583 ) ;
#31989 = DIRECTION ( 'NONE',  ( 0.000000000000000000, -0.000000000000000000, -1.000000000000000000 ) ) ;
#31990 = VECTOR ( 'NONE', #33018, 1000.000000000000000 ) ;
#31991 = CARTESIAN_POINT ( 'NONE',  ( 8.580623737882843827, 9.689726262117162037, 26.00000000000000711 ) ) ;
#31992 = DIRECTION ( 'NONE',  ( 1.000000000000000000, 0.000000000000000000, 0.000000000000000000 ) ) ;
#31993 = DIRECTION ( 'NONE',  ( 0.000000000000000000, 0.000000000000000000, 1.000000000000000000 ) ) ;
#31994 = AXIS2_PLACEMENT_3D ( 'NONE', #1818, #44951, #66521 ) ;
#31995 = EDGE_CURVE ( 'NONE', #57625, #6981, #36676, .T. ) ;
#31996 = ORIENTED_EDGE ( 'NONE', *, *, #22054, .T. ) ;
#31998 = VERTEX_POINT ( 'NONE', #69199 ) ;
#31997 = LINE ( 'NONE', #6152, #28305 ) ;
#31999 = EDGE_CURVE ( 'NONE', #16443, #24527, #68856, .T. ) ;
#32000 = CARTESIAN_POINT ( 'NONE',  ( 105.8309041053263257, 63.65740854044500452, 2.000000000000000000 ) ) ;
#32001 = FACE_OUTER_BOUND ( 'NONE', #57243, .T. ) ;
#32002 = DIRECTION ( 'NONE',  ( -1.000000000000000000, 1.115702204244423151E-14, 0.000000000000000000 ) ) ;
#32003 = EDGE_LOOP ( 'NONE', ( #9915, #13531, #68092, #36261 ) ) ;
#32004 = VECTOR ( 'NONE', #50162, 1000.000000000000000 ) ;
#32005 = FACE_OUTER_BOUND ( 'NONE', #49188, .T. ) ;
#32006 = LINE ( 'NONE', #48267, #3630 ) ;
#32007 = ORIENTED_EDGE ( 'NONE', *, *, #63917, .T. ) ;
#32008 = ORIENTED_EDGE ( 'NONE', *, *, #30682, .T. ) ;
#32009 = EDGE_LOOP ( 'NONE', ( #39472, #54788, #9494, #32694 ) ) ;
#32010 = CARTESIAN_POINT ( 'NONE',  ( -5.242976262117280406, -5.257023737882805747, 54.00000000000000711 ) ) ;
#32011 = CARTESIAN_POINT ( 'NONE',  ( 7.250000000000005329, 7.250000000000000888, -26.00000000000001066 ) ) ;
#32012 = DIRECTION ( 'NONE',  ( -1.000000000000000000, 0.000000000000000000, 0.000000000000000000 ) ) ;
#32013 = AXIS2_PLACEMENT_3D ( 'NONE', #67198, #2842, #25122 ) ;
#32014 = ORIENTED_EDGE ( 'NONE', *, *, #53981, .F. ) ;
#32015 = ORIENTED_EDGE ( 'NONE', *, *, #49359, .T. ) ;
#32016 = CIRCLE ( 'NONE', #3735, 0.3999999999999993006 ) ;
#32017 = PLANE ( 'NONE',  #2276 ) ;
#32018 = EDGE_LOOP ( 'NONE', ( #34918, #64000, #366, #27527 ) ) ;
#32019 = VECTOR ( 'NONE', #9309, 1000.000000000000000 ) ;
#32020 = ORIENTED_EDGE ( 'NONE', *, *, #1685, .F. ) ;
#32021 = VERTEX_POINT ( 'NONE', #52954 ) ;
#32022 = ORIENTED_EDGE ( 'NONE', *, *, #53461, .T. ) ;
#32023 = DIRECTION ( 'NONE',  ( 0.5000000000000004441, -0.8660254037844383745, 0.000000000000000000 ) ) ;
#32024 = CIRCLE ( 'NONE', #34252, 0.5000000000000000000 ) ;
#32025 = VECTOR ( 'NONE', #37019, 1000.000000000000000 ) ;
#32027 = ORIENTED_EDGE ( 'NONE', *, *, #33651, .T. ) ;
#32026 = CARTESIAN_POINT ( 'NONE',  ( 8.144523737882817471, -8.835729544836345539, 54.00000000000000711 ) ) ;
#32028 = ADVANCED_FACE ( 'NONE', ( #25730, #4164 ), #52238, .T. ) ;
#32029 = DIRECTION ( 'NONE',  ( -1.000000000000000000, 0.000000000000000000, 0.000000000000000000 ) ) ;
#32030 = CARTESIAN_POINT ( 'NONE',  ( -14.25000000000000000, -0.2038245569916330158, 21.77831216351300014 ) ) ;
#32031 = DIRECTION ( 'NONE',  ( 0.000000000000000000, -0.9921567416492215186, 0.1249999999999996531 ) ) ;
#32032 = ADVANCED_FACE ( 'NONE', ( #58246 ), #36319, .T. ) ;
#32033 = ORIENTED_EDGE ( 'NONE', *, *, #35561, .F. ) ;
#32034 = ADVANCED_FACE ( 'NONE', ( #21456 ), #10496, .T. ) ;
#32035 = AXIS2_PLACEMENT_3D ( 'NONE', #64428, #26589, #10330 ) ;
#32036 = CARTESIAN_POINT ( 'NONE',  ( 30.00000000000000000, -17.35230188589299871, 15.35019951917099945 ) ) ;
#32037 = EDGE_CURVE ( 'NONE', #6255, #32021, #63171, .T. ) ;
#32038 = CARTESIAN_POINT ( 'NONE',  ( -7.250000000000000888, 8.250000000000001776, -22.50000000000000000 ) ) ;
#32039 = ORIENTED_EDGE ( 'NONE', *, *, #26741, .F. ) ;
#32040 = DIRECTION ( 'NONE',  ( 0.000000000000000000, 0.000000000000000000, 1.000000000000000000 ) ) ;
#32041 = PLANE ( 'NONE',  #47139 ) ;
#32042 = ORIENTED_EDGE ( 'NONE', *, *, #30083, .T. ) ;
#32043 = DIRECTION ( 'NONE',  ( 0.000000000000000000, -1.000000000000000000, 0.000000000000000000 ) ) ;
#32044 = DIRECTION ( 'NONE',  ( 0.000000000000000000, 1.000000000000000000, 0.000000000000000000 ) ) ;
#32045 = CARTESIAN_POINT ( 'NONE',  ( 283.0000000000000568, -42.00000000000000000, 7.000000000000000000 ) ) ;
#32046 = EDGE_CURVE ( 'NONE', #52724, #18593, #9819, .T. ) ;
#32047 = CARTESIAN_POINT ( 'NONE',  ( -10.73351654964669599, -1.690483450353341910, 455.0000000000000568 ) ) ;
#32048 = DIRECTION ( 'NONE',  ( 1.000000000000000000, -0.000000000000000000, 0.000000000000000000 ) ) ;
#32049 = DIRECTION ( 'NONE',  ( -0.000000000000000000, -0.000000000000000000, -1.000000000000000000 ) ) ;
#32050 = DIRECTION ( 'NONE',  ( -1.836970198721029934E-16, 1.836970198721036590E-16, -1.000000000000000000 ) ) ;
#32051 = CARTESIAN_POINT ( 'NONE',  ( -9.690000000000001279, 10.50000000000000000, -5.000000000000000000 ) ) ;
#32052 = ORIENTED_EDGE ( 'NONE', *, *, #6499, .T. ) ;
#32053 = CARTESIAN_POINT ( 'NONE',  ( -8.250000000000000000, 7.250000000000001776, -23.00000000000000000 ) ) ;
#32054 = CARTESIAN_POINT ( 'NONE',  ( 8.250000000000005329, 7.250000000000000888, -26.00000000000001066 ) ) ;
#32055 = DIRECTION ( 'NONE',  ( 0.000000000000000000, -1.000000000000000000, 0.000000000000000000 ) ) ;
#32056 = DIRECTION ( 'NONE',  ( 0.000000000000000000, -0.1111111111108836896, -0.9938079899999319178 ) ) ;
#32057 = AXIS2_PLACEMENT_3D ( 'NONE', #12814, #66917, #67282 ) ;
#32058 = ORIENTED_EDGE ( 'NONE', *, *, #34931, .T. ) ;
#32059 = VECTOR ( 'NONE', #40460, 1000.000000000000000 ) ;
#32060 = CARTESIAN_POINT ( 'NONE',  ( 49.00000000000000000, 20.60000000000000142, -13.86939075806900057 ) ) ;
#32061 = CARTESIAN_POINT ( 'NONE',  ( 8.249999999999996447, -7.848062532927998269, -5.000000000000000000 ) ) ;
#32062 = CARTESIAN_POINT ( 'NONE',  ( 49.00000000000000000, 20.60000000000000142, -13.86939075806900057 ) ) ;
#32063 = CARTESIAN_POINT ( 'NONE',  ( 0.000000000000000000, -42.00000000000000000, 26.50000000000000000 ) ) ;
#32064 = CIRCLE ( 'NONE', #61396, 0.1749999999999998224 ) ;
#32066 = VECTOR ( 'NONE', #44028, 1000.000000000000000 ) ;
#32065 = CARTESIAN_POINT ( 'NONE',  ( 7.500000000000000000, -53.81370849898476649, -20.00000000000000000 ) ) ;
#32067 = DIRECTION ( 'NONE',  ( -0.6414496315691592399, 0.7671651518152985405, 2.587583378555132735E-16 ) ) ;
#32068 = EDGE_CURVE ( 'NONE', #25480, #27416, #37379, .T. ) ;
#32069 = EDGE_LOOP ( 'NONE', ( #44558, #830, #49561, #14451 ) ) ;
#32070 = ADVANCED_FACE ( 'NONE', ( #41977 ), #47982, .T. ) ;
#32071 = ORIENTED_EDGE ( 'NONE', *, *, #40717, .T. ) ;
#32072 = CARTESIAN_POINT ( 'NONE',  ( 7.000000000000000000, -32.94999999999885176, -8.199999999997979572 ) ) ;
#32073 = CARTESIAN_POINT ( 'NONE',  ( -6.467976262117279163, -5.257023737882805747, 54.00000000000000711 ) ) ;
#32074 = ORIENTED_EDGE ( 'NONE', *, *, #56535, .T. ) ;
#32075 = ADVANCED_FACE ( 'NONE', ( #64593 ), #31392, .T. ) ;
#32076 = DIRECTION ( 'NONE',  ( -1.000000000000000000, 9.050731179009442381E-15, 3.325184690495119758E-30 ) ) ;
#32077 = CARTESIAN_POINT ( 'NONE',  ( -1.677516549646826061, -10.74648345035347141, 455.0000000000000568 ) ) ;
#32078 = ORIENTED_EDGE ( 'NONE', *, *, #69566, .F. ) ;
#32079 = CARTESIAN_POINT ( 'NONE',  ( 0.000000000000000000, -8.249999999999998224, -20.50000000000000000 ) ) ;
#32080 = ORIENTED_EDGE ( 'NONE', *, *, #58013, .F. ) ;
#32081 = VERTEX_POINT ( 'NONE', #37041 ) ;
#32082 = CARTESIAN_POINT ( 'NONE',  ( 4.149127210878720717, 6.822336235477395761, 26.00000000000000711 ) ) ;
#32083 = ORIENTED_EDGE ( 'NONE', *, *, #38066, .F. ) ;
#32084 = LINE ( 'NONE', #46679, #3775 ) ;
#32085 = LINE ( 'NONE', #26790, #68887 ) ;
#32086 = LINE ( 'NONE', #53660, #55079 ) ;
#32087 = VERTEX_POINT ( 'NONE', #58601 ) ;
#32088 = VECTOR ( 'NONE', #57442, 1000.000000000000000 ) ;
#32089 = ORIENTED_EDGE ( 'NONE', *, *, #56640, .T. ) ;
#32090 = PLANE ( 'NONE',  #39157 ) ;
#32092 = CARTESIAN_POINT ( 'NONE',  ( 275.2500000000001137, -42.24999999999992184, 26.75000000000003197 ) ) ;
#32091 = DIRECTION ( 'NONE',  ( 1.067128122525083795E-14, 1.000000000000000000, 0.000000000000000000 ) ) ;
#32093 = VERTEX_POINT ( 'NONE', #64255 ) ;
#32094 = ORIENTED_EDGE ( 'NONE', *, *, #22062, .T. ) ;
#32095 = ORIENTED_EDGE ( 'NONE', *, *, #12897, .T. ) ;
#32096 = CARTESIAN_POINT ( 'NONE',  ( 23.90000000000000213, 20.60000000000000142, -13.86939075806900057 ) ) ;
#32098 = VERTEX_POINT ( 'NONE', #3799 ) ;
#32097 = DIRECTION ( 'NONE',  ( 0.000000000000000000, 3.673940397442059868E-16, -1.000000000000000000 ) ) ;
#32099 = EDGE_CURVE ( 'NONE', #46021, #14139, #43016, .T. ) ;
#32100 = FACE_OUTER_BOUND ( 'NONE', #33272, .T. ) ;
#32101 = VECTOR ( 'NONE', #8373, 1000.000000000000000 ) ;
#32102 = VECTOR ( 'NONE', #43657, 1000.000000000000000 ) ;
#32103 = CARTESIAN_POINT ( 'NONE',  ( 7.250000000000004441, 7.450000000000001954, -7.500000000000000000 ) ) ;
#32104 = VERTEX_POINT ( 'NONE', #16154 ) ;
#32105 = ORIENTED_EDGE ( 'NONE', *, *, #69540, .F. ) ;
#32106 = ADVANCED_FACE ( 'NONE', ( #31733 ), #37726, .F. ) ;
#32107 = AXIS2_PLACEMENT_3D ( 'NONE', #47725, #47373, #35703 ) ;
#32108 = AXIS2_PLACEMENT_3D ( 'NONE', #58836, #27691, #48229 ) ;
#32109 = LINE ( 'NONE', #15514, #33497 ) ;
#32110 = EDGE_CURVE ( 'NONE', #42141, #56362, #46923, .T. ) ;
#32111 = EDGE_CURVE ( 'NONE', #13215, #41070, #68509, .T. ) ;
#32112 = VERTEX_POINT ( 'NONE', #42675 ) ;
#32113 = DIRECTION ( 'NONE',  ( -4.956352788505168198E-15, -1.000000000000000000, 0.000000000000000000 ) ) ;
#32114 = CARTESIAN_POINT ( 'NONE',  ( -8.452095193409402185, 7.744988412222746810, 455.0000000000000568 ) ) ;
#32115 = ADVANCED_FACE ( 'NONE', ( #59972 ), #54340, .F. ) ;
#32116 = CARTESIAN_POINT ( 'NONE',  ( -3.650476262117221093, 10.49297626211717116, 54.00000000000000711 ) ) ;
#32117 = EDGE_CURVE ( 'NONE', #28065, #25655, #43365, .T. ) ;
#32118 = ORIENTED_EDGE ( 'NONE', *, *, #39134, .T. ) ;
#32119 = ADVANCED_FACE ( 'NONE', ( #27458 ), #53995, .F. ) ;
#32120 = DIRECTION ( 'NONE',  ( -1.000000000000000000, 0.000000000000000000, 0.000000000000000000 ) ) ;
#32122 = VERTEX_POINT ( 'NONE', #6589 ) ;
#32121 = FACE_OUTER_BOUND ( 'NONE', #27399, .T. ) ;
#32123 = VERTEX_POINT ( 'NONE', #11185 ) ;
#32124 = CIRCLE ( 'NONE', #24191, 4.000000000000000888 ) ;
#32125 = CARTESIAN_POINT ( 'NONE',  ( 25.50000000000000355, -15.50000000000000000, -24.50000000000000000 ) ) ;
#32126 = CARTESIAN_POINT ( 'NONE',  ( -14.25000000000000000, -2.500000000000000000, 23.22168783648699986 ) ) ;
#32127 = FACE_OUTER_BOUND ( 'NONE', #5346, .T. ) ;
#32128 = CARTESIAN_POINT ( 'NONE',  ( 275.5000000000000000, -0.5000000000000000000, -27.00000000000000000 ) ) ;
#32129 = LINE ( 'NONE', #69621, #3695 ) ;
#32130 = ORIENTED_EDGE ( 'NONE', *, *, #43753, .F. ) ;
#32131 = CARTESIAN_POINT ( 'NONE',  ( 11.32648345035335780, 7.593516549646611047, 195.0000000000000284 ) ) ;
#32132 = PLANE ( 'NONE',  #14679 ) ;
#32133 = FACE_OUTER_BOUND ( 'NONE', #51630, .T. ) ;
#32135 = VERTEX_POINT ( 'NONE', #33103 ) ;
#32134 = LINE ( 'NONE', #20820, #66094 ) ;
#32136 = SURFACE_STYLE_FILL_AREA ( #10565 ) ;
#32137 = DIRECTION ( 'NONE',  ( 1.000000000000000000, 1.301042606982605321E-16, -0.000000000000000000 ) ) ;
#32138 = VECTOR ( 'NONE', #29700, 1000.000000000000000 ) ;
#32139 = PLANE ( 'NONE',  #54481 ) ;
#32140 = CARTESIAN_POINT ( 'NONE',  ( -7.250000000000001776, -7.249999999999998224, -19.50000000000000000 ) ) ;
#32141 = ORIENTED_EDGE ( 'NONE', *, *, #39388, .F. ) ;
#32142 = DIRECTION ( 'NONE',  ( 1.000000000000000000, -0.000000000000000000, -0.000000000000000000 ) ) ;
#32143 = CARTESIAN_POINT ( 'NONE',  ( 18.85410196625000268, -15.50000000000000000, -21.50000000000000000 ) ) ;
#32144 = VECTOR ( 'NONE', #20402, 1000.000000000000000 ) ;
#32145 = VERTEX_POINT ( 'NONE', #39444 ) ;
#32146 = CARTESIAN_POINT ( 'NONE',  ( 24.00000000000000000, -17.35230188589299516, -15.35019951917100478 ) ) ;
#32147 = CARTESIAN_POINT ( 'NONE',  ( 30.00000000000000000, -12.00000000000000000, 10.69999999999999929 ) ) ;
#32148 = FACE_OUTER_BOUND ( 'NONE', #27733, .T. ) ;
#32149 = DIRECTION ( 'NONE',  ( 1.000000000000000000, -0.000000000000000000, 0.000000000000000000 ) ) ;
#32150 = FACE_OUTER_BOUND ( 'NONE', #18455, .T. ) ;
#32151 = VECTOR ( 'NONE', #1270, 1000.000000000000000 ) ;
#32152 = ORIENTED_EDGE ( 'NONE', *, *, #32689, .F. ) ;
#32153 = ORIENTED_EDGE ( 'NONE', *, *, #18040, .F. ) ;
#32154 = DIRECTION ( 'NONE',  ( -1.000000000000000000, 0.000000000000000000, -0.000000000000000000 ) ) ;
#32155 = VERTEX_POINT ( 'NONE', #28479 ) ;
#32156 = ORIENTED_EDGE ( 'NONE', *, *, #42870, .T. ) ;
#32157 = EDGE_CURVE ( 'NONE', #7905, #2702, #15783, .T. ) ;
#32158 = DIRECTION ( 'NONE',  ( 0.000000000000000000, -1.000000000000000000, 3.819861094142539476E-12 ) ) ;
#32159 = EDGE_CURVE ( 'NONE', #66978, #61720, #27046, .T. ) ;
#32160 = CIRCLE ( 'NONE', #44594, 0.3999999999999993006 ) ;
#32161 = EDGE_CURVE ( 'NONE', #17317, #48505, #11524, .T. ) ;
#32162 = DIRECTION ( 'NONE',  ( -0.000000000000000000, 3.673940397442059868E-16, -1.000000000000000000 ) ) ;
#32163 = VECTOR ( 'NONE', #65896, 1000.000000000000000 ) ;
#32164 = CARTESIAN_POINT ( 'NONE',  ( 152.5922698879801942, -30.42541106249863603, 0.000000000000000000 ) ) ;
#32165 = ORIENTED_EDGE ( 'NONE', *, *, #68472, .F. ) ;
#32166 = ORIENTED_EDGE ( 'NONE', *, *, #21260, .F. ) ;
#32167 = FACE_OUTER_BOUND ( 'NONE', #67471, .T. ) ;
#32168 = ORIENTED_EDGE ( 'NONE', *, *, #49203, .F. ) ;
#32169 = ORIENTED_EDGE ( 'NONE', *, *, #58976, .T. ) ;
#32170 = DIRECTION ( 'NONE',  ( -1.794541526872559352E-16, -1.000000000000000000, 0.000000000000000000 ) ) ;
#32171 = LINE ( 'NONE', #31136, #834 ) ;
#32172 = CIRCLE ( 'NONE', #29923, 24.99999999998784972 ) ;
#32173 = DIRECTION ( 'NONE',  ( 0.000000000000000000, 0.000000000000000000, -1.000000000000000000 ) ) ;
#32174 = AXIS2_PLACEMENT_3D ( 'NONE', #39324, #66196, #1836 ) ;
#32175 = VERTEX_POINT ( 'NONE', #6235 ) ;
#32176 = AXIS2_PLACEMENT_3D ( 'NONE', #22942, #51201, #39539 ) ;
#32177 = LINE ( 'NONE', #54785, #7453 ) ;
#32179 = CYLINDRICAL_SURFACE ( 'NONE', #61546, 1.399999999999999245 ) ;
#32178 = DIRECTION ( 'NONE',  ( 0.000000000000000000, 0.000000000000000000, 1.000000000000000000 ) ) ;
#32180 = EDGE_LOOP ( 'NONE', ( #52328, #38447, #37090, #44474 ) ) ;
#32181 = VERTEX_POINT ( 'NONE', #64945 ) ;
#32183 = ORIENTED_EDGE ( 'NONE', *, *, #13898, .F. ) ;
#32182 = DIRECTION ( 'NONE',  ( -1.000000000000000000, 0.000000000000000000, 0.000000000000000000 ) ) ;
#32184 = VERTEX_POINT ( 'NONE', #55376 ) ;
#32185 = LINE ( 'NONE', #36804, #67163 ) ;
#32186 = CARTESIAN_POINT ( 'NONE',  ( 39.00000000000000000, 16.96999999999999886, 21.00000000000000000 ) ) ;
#32187 = ORIENTED_EDGE ( 'NONE', *, *, #55583, .T. ) ;
#32188 = AXIS2_PLACEMENT_3D ( 'NONE', #65386, #59383, #65041 ) ;
#32189 = DIRECTION ( 'NONE',  ( -1.000000000000000000, 0.000000000000000000, -0.000000000000000000 ) ) ;
#32190 = CARTESIAN_POINT ( 'NONE',  ( 6.006483450353401921, 5.993516549646582092, 455.0000000000000568 ) ) ;
#32191 = VECTOR ( 'NONE', #21719, 1000.000000000000000 ) ;
#32192 = ORIENTED_EDGE ( 'NONE', *, *, #28188, .T. ) ;
#32193 = VERTEX_POINT ( 'NONE', #33790 ) ;
#32194 = DIRECTION ( 'NONE',  ( 0.000000000000000000, -1.000000000000000000, 0.000000000000000000 ) ) ;
#32195 = LINE ( 'NONE', #53777, #53828 ) ;
#32196 = CARTESIAN_POINT ( 'NONE',  ( 9.247904806590689475, -9.955011587777349291, 455.0000000000000568 ) ) ;
#32197 = ADVANCED_FACE ( 'NONE', ( #6915 ), #44386, .F. ) ;
#32198 = EDGE_LOOP ( 'NONE', ( #1509, #49973, #44838, #68640 ) ) ;
#32199 = VECTOR ( 'NONE', #15963, 1000.000000000000000 ) ;
#32200 = CIRCLE ( 'NONE', #8453, 0.9999999999999991118 ) ;
#32201 = EDGE_CURVE ( 'NONE', #7017, #44833, #27809, .T. ) ;
#32202 = PLANE ( 'NONE',  #9790 ) ;
#32203 = LINE ( 'NONE', #31866, #10240 ) ;
#32204 = ADVANCED_FACE ( 'NONE', ( #243 ), #591, .F. ) ;
#32206 = VERTEX_POINT ( 'NONE', #60313 ) ;
#32205 = FACE_OUTER_BOUND ( 'NONE', #58966, .T. ) ;
#32208 = ORIENTED_EDGE ( 'NONE', *, *, #52625, .T. ) ;
#32207 = PLANE ( 'NONE',  #26696 ) ;
#32209 = DIRECTION ( 'NONE',  ( 1.000000000000000000, -0.000000000000000000, -0.000000000000000000 ) ) ;
#32210 = VECTOR ( 'NONE', #9128, 1000.000000000000000 ) ;
#32211 = VECTOR ( 'NONE', #35447, 1000.000000000000000 ) ;
#32212 = LINE ( 'NONE', #53790, #58939 ) ;
#32213 = DIRECTION ( 'NONE',  ( 0.000000000000000000, 0.000000000000000000, 1.000000000000000000 ) ) ;
#32214 = CARTESIAN_POINT ( 'NONE',  ( 13.90000000000000213, -0.2000000000089119934, 8.909539772616881237E-12 ) ) ;
#32215 = CARTESIAN_POINT ( 'NONE',  ( -2.693516549646682190, 10.08346604330774454, 455.0000000000000568 ) ) ;
#32216 = VECTOR ( 'NONE', #4004, 1000.000000000000000 ) ;
#32217 = PLANE ( 'NONE',  #42814 ) ;
#32218 = ORIENTED_EDGE ( 'NONE', *, *, #21646, .F. ) ;
#32219 = CARTESIAN_POINT ( 'NONE',  ( -11.31351654964674047, -7.606483450353325182, 195.0000000000000284 ) ) ;
#32220 = EDGE_CURVE ( 'NONE', #20561, #58160, #65629, .T. ) ;
#32222 = ORIENTED_EDGE ( 'NONE', *, *, #57467, .T. ) ;
#32221 = DIRECTION ( 'NONE',  ( 0.000000000000000000, -1.000000000000000000, 0.000000000000000000 ) ) ;
#32224 = ORIENTED_EDGE ( 'NONE', *, *, #24585, .T. ) ;
#32223 = CARTESIAN_POINT ( 'NONE',  ( -4.609516549646752281, -3.606483450353441533, 455.0000000000000568 ) ) ;
#32225 = AXIS2_PLACEMENT_3D ( 'NONE', #21708, #5097, #64848 ) ;
#32226 = LINE ( 'NONE', #58418, #63455 ) ;
#32227 = ORIENTED_EDGE ( 'NONE', *, *, #21859, .T. ) ;
#32228 = DIRECTION ( 'NONE',  ( -0.000000000000000000, 3.673940397442059868E-16, -1.000000000000000000 ) ) ;
#32229 = LINE ( 'NONE', #65110, #107 ) ;
#32230 = ORIENTED_EDGE ( 'NONE', *, *, #38429, .T. ) ;
#32231 = DIRECTION ( 'NONE',  ( -1.000000000000000000, 0.000000000000000000, 0.000000000000000000 ) ) ;
#32232 = LINE ( 'NONE', #11018, #6685 ) ;
#32233 = SURFACE_SIDE_STYLE ('',( #42836 ) ) ;
#32234 = EDGE_LOOP ( 'NONE', ( #32020, #38699, #16023, #14042 ) ) ;
#32235 = CYLINDRICAL_SURFACE ( 'NONE', #62109, 4.500000000000189182 ) ;
#32236 = ORIENTED_EDGE ( 'NONE', *, *, #40375, .T. ) ;
#32237 = ORIENTED_EDGE ( 'NONE', *, *, #61731, .F. ) ;
#32238 = DIRECTION ( 'NONE',  ( 1.836970198721029934E-16, -1.836970198721036344E-16, 1.000000000000000000 ) ) ;
#32239 = CARTESIAN_POINT ( 'NONE',  ( -17.00000000000000000, -15.50000000000000000, 19.33772233983200195 ) ) ;
#32240 = CONICAL_SURFACE ( 'NONE', #13027, 6.000000000000005329, 0.1292750040481423779 ) ;
#32241 = EDGE_CURVE ( 'NONE', #31340, #57095, #36066, .T. ) ;
#32242 = DIRECTION ( 'NONE',  ( 0.7671651518153065341, 0.6414496315691495809, -0.000000000000000000 ) ) ;
#32243 = VECTOR ( 'NONE', #48673, 1000.000000000000000 ) ;
#32244 = DIRECTION ( 'NONE',  ( 1.000000000000000000, 0.000000000000000000, 0.000000000000000000 ) ) ;
#32245 = ORIENTED_EDGE ( 'NONE', *, *, #424, .F. ) ;
#32246 = ORIENTED_EDGE ( 'NONE', *, *, #26238, .F. ) ;
#32248 = ORIENTED_EDGE ( 'NONE', *, *, #37008, .F. ) ;
#32247 = CARTESIAN_POINT ( 'NONE',  ( 283.0000000000000568, -53.81370849898476649, 17.35424868893542438 ) ) ;
#32249 = ORIENTED_EDGE ( 'NONE', *, *, #66981, .F. ) ;
#32250 = AXIS2_PLACEMENT_3D ( 'NONE', #25683, #31682, #53254 ) ;
#32251 = CIRCLE ( 'NONE', #16457, 4.500000000000191847 ) ;
#32252 = AXIS2_PLACEMENT_3D ( 'NONE', #40252, #57569, #51572 ) ;
#32253 = DIRECTION ( 'NONE',  ( -1.000000000000000000, 1.794541526872559352E-16, 0.000000000000000000 ) ) ;
#32254 = CYLINDRICAL_SURFACE ( 'NONE', #26412, 0.5000000000009441337 ) ;
#32255 = DIRECTION ( 'NONE',  ( -3.540573132209558464E-15, -1.000000000000000000, 0.000000000000000000 ) ) ;
#32256 = FACE_OUTER_BOUND ( 'NONE', #65061, .T. ) ;
#32257 = VECTOR ( 'NONE', #63565, 1000.000000000000000 ) ;
#32258 = PRESENTATION_LAYER_ASSIGNMENT (  '', '', ( #69562 ) ) ;
#32259 = EDGE_CURVE ( 'NONE', #41478, #59416, #44055, .T. ) ;
#32261 = LINE ( 'NONE', #37924, #51526 ) ;
#32260 = DIRECTION ( 'NONE',  ( -0.000000000000000000, 3.673940397442059868E-16, -1.000000000000000000 ) ) ;
#32262 = VERTEX_POINT ( 'NONE', #16507 ) ;
#32264 = EDGE_LOOP ( 'NONE', ( #7636, #11725, #19187, #47314 ) ) ;
#32263 = CARTESIAN_POINT ( 'NONE',  ( 283.0000000000000568, -38.15000000000000568, 13.19999999999999929 ) ) ;
#32265 = ORIENTED_EDGE ( 'NONE', *, *, #47778, .F. ) ;
#32266 = EDGE_LOOP ( 'NONE', ( #38832, #69676, #2976, #21940 ) ) ;
#32267 = AXIS2_PLACEMENT_3D ( 'NONE', #29205, #40167, #30279 ) ;
#32268 = EDGE_CURVE ( 'NONE', #49486, #47595, #38087, .T. ) ;
#32269 = PLANE ( 'NONE',  #34446 ) ;
#32270 = FACE_OUTER_BOUND ( 'NONE', #17717, .T. ) ;
#32271 = CARTESIAN_POINT ( 'NONE',  ( 0.000000000000000000, 0.000000000000000000, 0.000000000000000000 ) ) ;
#32272 = VECTOR ( 'NONE', #53724, 1000.000000000000000 ) ;
#32273 = DIRECTION ( 'NONE',  ( 0.7671651518152998728, -0.6414496315691575745, 2.309356642088859447E-17 ) ) ;
#32274 = ORIENTED_EDGE ( 'NONE', *, *, #21260, .T. ) ;
#32275 = ORIENTED_EDGE ( 'NONE', *, *, #4285, .T. ) ;
#32276 = VERTEX_POINT ( 'NONE', #22838 ) ;
#32277 = CIRCLE ( 'NONE', #1768, 0.5000000000009441337 ) ;
#32278 = CYLINDRICAL_SURFACE ( 'NONE', #18120, 4.500000000000188294 ) ;
#32279 = DIRECTION ( 'NONE',  ( -1.836970198721029934E-16, 1.836970198721036344E-16, -1.000000000000000000 ) ) ;
#32280 = LINE ( 'NONE', #59147, #16458 ) ;
#32281 = VERTEX_POINT ( 'NONE', #33456 ) ;
#32282 = EDGE_LOOP ( 'NONE', ( #60851, #2225, #35300, #45509 ) ) ;
#32283 = DIRECTION ( 'NONE',  ( -1.000000000000000000, 1.920885163218982051E-15, 1.836970198721033385E-16 ) ) ;
#32284 =( REPRESENTATION_RELATIONSHIP ('NONE','NONE', #4299, #15926 ) REPRESENTATION_RELATIONSHIP_WITH_TRANSFORMATION ( #1992 )SHAPE_REPRESENTATION_RELATIONSHIP( ) );
#32285 = CARTESIAN_POINT ( 'NONE',  ( -15.70313394609757296, -0.2715358723600092006, -23.82609623451302028 ) ) ;
#32286 = ORIENTED_EDGE ( 'NONE', *, *, #40047, .F. ) ;
#32287 = EDGE_CURVE ( 'NONE', #67312, #69051, #43726, .T. ) ;
#32288 = ADVANCED_FACE ( 'NONE', ( #66330 ), #56062, .F. ) ;
#32289 = CARTESIAN_POINT ( 'NONE',  ( 7.806483450353418618, 11.31351654964657172, 455.0000000000000568 ) ) ;
#32290 = EDGE_CURVE ( 'NONE', #43546, #42345, #61346, .T. ) ;
#32291 = CIRCLE ( 'NONE', #44674, 3.499999999999849454 ) ;
#32293 = EDGE_LOOP ( 'NONE', ( #43105, #56641, #59971, #44298 ) ) ;
#32292 = FACE_OUTER_BOUND ( 'NONE', #33904, .T. ) ;
#32294 = ORIENTED_EDGE ( 'NONE', *, *, #36682, .T. ) ;
#32295 = DIRECTION ( 'NONE',  ( -1.794541526872559352E-16, -1.000000000000000000, 0.000000000000000000 ) ) ;
#32296 = CARTESIAN_POINT ( 'NONE',  ( 10.50702373788278265, 3.650476262117142934, 54.00000000000000711 ) ) ;
#32297 = ADVANCED_FACE ( 'NONE', ( #51807 ), #23884, .F. ) ;
#32298 = AXIS2_PLACEMENT_3D ( 'NONE', #46146, #34470, #12906 ) ;
#32299 = CARTESIAN_POINT ( 'NONE',  ( 4.149127210878726935, -6.836383711243002814, 54.00000000000000711 ) ) ;
#32300 = DIRECTION ( 'NONE',  ( 1.836970198721029934E-16, -1.836970198721036344E-16, 1.000000000000000000 ) ) ;
#32301 = EDGE_CURVE ( 'NONE', #56758, #9312, #24932, .T. ) ;
#32302 = DIRECTION ( 'NONE',  ( -0.000000000000000000, -1.000000000000000000, -0.000000000000000000 ) ) ;
#32303 = VECTOR ( 'NONE', #10630, 1000.000000000000000 ) ;
#32304 = EDGE_CURVE ( 'NONE', #48411, #18604, #53052, .T. ) ;
#32305 = VERTEX_POINT ( 'NONE', #57105 ) ;
#32306 = FACE_BOUND ( 'NONE', #44162, .T. ) ;
#32307 = ADVANCED_FACE ( 'NONE', ( #30248 ), #7619, .T. ) ;
#32308 = EDGE_LOOP ( 'NONE', ( #58464, #29276, #18684, #20497 ) ) ;
#32310 = PLANE ( 'NONE',  #17403 ) ;
#32309 = CIRCLE ( 'NONE', #28889, 1.000000000000000000 ) ;
#32311 = DIRECTION ( 'NONE',  ( 0.000000000000000000, 0.000000000000000000, -1.000000000000000000 ) ) ;
#32312 = LINE ( 'NONE', #4406, #68651 ) ;
#32313 = DIRECTION ( 'NONE',  ( -1.000000000000000000, 0.000000000000000000, 0.000000000000000000 ) ) ;
#32314 = VECTOR ( 'NONE', #2984, 1000.000000000000000 ) ;
#32315 = VECTOR ( 'NONE', #55556, 1000.000000000000000 ) ;
#32316 = AXIS2_PLACEMENT_3D ( 'NONE', #44938, #29714, #41024 ) ;
#32317 = CARTESIAN_POINT ( 'NONE',  ( 49.00000000000000000, 13.66939075806899950, 20.80000000000000426 ) ) ;
#32318 = EDGE_LOOP ( 'NONE', ( #1710, #69208, #25386, #18366 ) ) ;
#32319 = AXIS2_PLACEMENT_3D ( 'NONE', #5152, #68460, #3747 ) ;
#32320 = LINE ( 'NONE', #54938, #25732 ) ;
#32321 = CARTESIAN_POINT ( 'NONE',  ( -8.250000000000001776, 7.250000000000000888, -14.50000000000000000 ) ) ;
#32322 = VECTOR ( 'NONE', #3443, 1000.000000000000000 ) ;
#32323 = ORIENTED_EDGE ( 'NONE', *, *, #41694, .F. ) ;
#32324 = LINE ( 'NONE', #16060, #65423 ) ;
#32325 = EDGE_CURVE ( 'NONE', #58158, #45382, #18570, .T. ) ;
#32326 = CARTESIAN_POINT ( 'NONE',  ( 283.0000000000000568, -41.99999999999906208, 14.49999999999903899 ) ) ;
#32327 = CIRCLE ( 'NONE', #40171, 0.2000000000000005107 ) ;
#32328 = VERTEX_POINT ( 'NONE', #1971 ) ;
#32329 = DIRECTION ( 'NONE',  ( 0.000000000000000000, 0.000000000000000000, 1.000000000000000000 ) ) ;
#32330 = CARTESIAN_POINT ( 'NONE',  ( 6.836383711243005479, -6.364920264886896994, 26.00000000000000711 ) ) ;
#32331 = ORIENTED_EDGE ( 'NONE', *, *, #32991, .F. ) ;
#32332 = CARTESIAN_POINT ( 'NONE',  ( 4.456444791733522252E-16, 7.450000000000002842, -15.50000000000000000 ) ) ;
#32333 = LINE ( 'NONE', #69113, #52647 ) ;
#32334 = EDGE_CURVE ( 'NONE', #26265, #57216, #50412, .T. ) ;
#32335 = DIRECTION ( 'NONE',  ( 0.000000000000000000, 3.673940397442059868E-16, -1.000000000000000000 ) ) ;
#32336 = FACE_OUTER_BOUND ( 'NONE', #37076, .T. ) ;
#32337 = EDGE_LOOP ( 'NONE', ( #26800, #29660, #28226, #6536 ) ) ;
#32339 = ORIENTED_EDGE ( 'NONE', *, *, #39635, .F. ) ;
#32338 = CARTESIAN_POINT ( 'NONE',  ( -10.19191654964671301, 11.47551654964660450, 455.0000000000000568 ) ) ;
#32340 = EDGE_CURVE ( 'NONE', #19393, #48826, #29883, .T. ) ;
#32341 = DIRECTION ( 'NONE',  ( -1.836970198721029934E-16, 1.836970198721036590E-16, -1.000000000000000000 ) ) ;
#32342 = CARTESIAN_POINT ( 'NONE',  ( 8.711985858128686644, 8.079219948824833963, 54.00000000000000711 ) ) ;
#32343 = DIRECTION ( 'NONE',  ( 0.000000000000000000, -3.673940397442059868E-16, 1.000000000000000000 ) ) ;
#32344 = ORIENTED_EDGE ( 'NONE', *, *, #22, .T. ) ;
#32345 = VECTOR ( 'NONE', #37968, 1000.000000000000000 ) ;
#32346 = CARTESIAN_POINT ( 'NONE',  ( 7.826483450353380000, -12.00648345035349251, 455.0000000000000568 ) ) ;
#32347 = LINE ( 'NONE', #49975, #1395 ) ;
#32348 = VECTOR ( 'NONE', #39022, 1000.000000000000000 ) ;
#32349 = ORIENTED_EDGE ( 'NONE', *, *, #64801, .T. ) ;
#32350 = ORIENTED_EDGE ( 'NONE', *, *, #25632, .T. ) ;
#32351 = EDGE_LOOP ( 'NONE', ( #54884, #61189, #13619, #58624 ) ) ;
#32352 = EDGE_CURVE ( 'NONE', #5599, #40609, #58697, .T. ) ;
#32353 = CARTESIAN_POINT ( 'NONE',  ( -2.893516549646782732, -11.12648345035340647, 195.0000000000000284 ) ) ;
#32354 = CARTESIAN_POINT ( 'NONE',  ( 7.250000000000005329, -7.249999999999998224, -21.00000000000000000 ) ) ;
#32355 = DIRECTION ( 'NONE',  ( 1.000000000000000000, 0.000000000000000000, 0.000000000000000000 ) ) ;
#32356 = AXIS2_PLACEMENT_3D ( 'NONE', #22034, #64824, #27346 ) ;
#32357 = VECTOR ( 'NONE', #69323, 1000.000000000000000 ) ;
#32358 = ORIENTED_EDGE ( 'NONE', *, *, #31831, .T. ) ;
#32359 = EDGE_CURVE ( 'NONE', #62514, #55737, #56753, .T. ) ;
#32360 = ORIENTED_EDGE ( 'NONE', *, *, #14975, .F. ) ;
#32361 = EDGE_CURVE ( 'NONE', #47818, #57661, #13620, .T. ) ;
#32362 = PLANE ( 'NONE',  #39555 ) ;
#32363 = VECTOR ( 'NONE', #63076, 1000.000000000000000 ) ;
#32364 = VECTOR ( 'NONE', #19117, 1000.000000000000000 ) ;
#32365 = ORIENTED_EDGE ( 'NONE', *, *, #59580, .T. ) ;
#32366 = EDGE_CURVE ( 'NONE', #19510, #14855, #24237, .T. ) ;
#32367 = ORIENTED_EDGE ( 'NONE', *, *, #59901, .F. ) ;
#32368 = ADVANCED_FACE ( 'NONE', ( #28823 ), #45438, .T. ) ;
#32369 = EDGE_CURVE ( 'NONE', #22889, #19590, #34127, .T. ) ;
#32370 = VERTEX_POINT ( 'NONE', #23534 ) ;
#32371 = ORIENTED_EDGE ( 'NONE', *, *, #64056, .T. ) ;
#32372 = VECTOR ( 'NONE', #46104, 1000.000000000000000 ) ;
#32373 = DIRECTION ( 'NONE',  ( -1.000000000000000000, 0.000000000000000000, 0.000000000000000000 ) ) ;
#32374 = UNCERTAINTY_MEASURE_WITH_UNIT (LENGTH_MEASURE( 1.000000000000000082E-05 ), #37190, 'distance_accuracy_value', 'NONE');
#32376 = ORIENTED_EDGE ( 'NONE', *, *, #53200, .F. ) ;
#32375 = DIRECTION ( 'NONE',  ( -0.7071067811865475727, 0.7071067811865475727, 0.000000000000000000 ) ) ;
#32377 = EDGE_CURVE ( 'NONE', #62134, #29982, #58749, .T. ) ;
#32378 = LINE ( 'NONE', #39051, #16515 ) ;
#32379 = PRODUCT_DEFINITION_SHAPE ( 'NONE', 'NONE',  #69987 ) ;
#32380 = VECTOR ( 'NONE', #29403, 1000.000000000000000 ) ;
#32381 = LINE ( 'NONE', #53950, #44168 ) ;
#32382 = EDGE_CURVE ( 'NONE', #11693, #16217, #40488, .T. ) ;
#32383 = LINE ( 'NONE', #22112, #12093 ) ;
#32384 = ORIENTED_EDGE ( 'NONE', *, *, #41391, .T. ) ;
#32385 = EDGE_CURVE ( 'NONE', #60382, #17661, #47426, .T. ) ;
#32386 = DIRECTION ( 'NONE',  ( 0.000000000000000000, 0.7046037717862339012, 0.7096009616570518874 ) ) ;
#32387 = ADVANCED_FACE ( 'NONE', ( #9013 ), #36963, .F. ) ;
#32388 = CARTESIAN_POINT ( 'NONE',  ( 275.0000000000000000, -26.28355339059299922, 9.766446609406699508 ) ) ;
#32389 = ORIENTED_EDGE ( 'NONE', *, *, #51972, .T. ) ;
#32390 = LINE ( 'NONE', #57589, #28062 ) ;
#32391 = EDGE_CURVE ( 'NONE', #35825, #57481, #63116, .T. ) ;
#32392 = CARTESIAN_POINT ( 'NONE',  ( 7.250000000000005329, -7.249999999999998224, -12.00000000000000000 ) ) ;
#32393 = CARTESIAN_POINT ( 'NONE',  ( 9.306483450353379538, -10.09643294401465852, 455.0000000000000568 ) ) ;
#32394 = AXIS2_PLACEMENT_3D ( 'NONE', #62639, #53112, #63712 ) ;
#32395 = ORIENTED_EDGE ( 'NONE', *, *, #7113, .F. ) ;
#32396 = CARTESIAN_POINT ( 'NONE',  ( 275.5000000000000000, -0.5000000000000000000, 27.00000000000000000 ) ) ;
#32397 = LINE ( 'NONE', #31705, #25169 ) ;
#32398 = CARTESIAN_POINT ( 'NONE',  ( 11.00000000000000000, -12.00000000000000000, 10.20500000000000007 ) ) ;
#32399 = VECTOR ( 'NONE', #2114, 1000.000000000000000 ) ;
#32400 = VECTOR ( 'NONE', #53004, 1000.000000000000000 ) ;
#32401 = LINE ( 'NONE', #5525, #69262 ) ;
#32402 = DIRECTION ( 'NONE',  ( 0.000000000000000000, 0.000000000000000000, -1.000000000000000000 ) ) ;
#32403 = DIRECTION ( 'NONE',  ( 1.000000000000000000, 0.000000000000000000, 0.000000000000000000 ) ) ;
#32404 = PRESENTATION_STYLE_ASSIGNMENT (( #15443 ) ) ;
#32405 = CARTESIAN_POINT ( 'NONE',  ( 7.000000000000000000, -23.65000000000000568, 12.40000000000000213 ) ) ;
#32406 = VECTOR ( 'NONE', #64581, 1000.000000000000000 ) ;
#32407 = VECTOR ( 'NONE', #23308, 1000.000000000000000 ) ;
#32408 = AXIS2_PLACEMENT_3D ( 'NONE', #32271, #53851, #22948 ) ;
#32409 = ORIENTED_EDGE ( 'NONE', *, *, #52574, .T. ) ;
#32410 = CARTESIAN_POINT ( 'NONE',  ( 34.89999999999999858, 0.000000000000000000, 2.801416793502919355E-15 ) ) ;
#32411 = CARTESIAN_POINT ( 'NONE',  ( 10.90000000000000036, 13.66939075806899950, 20.80000000000000426 ) ) ;
#32412 = VECTOR ( 'NONE', #25164, 1000.000000000000000 ) ;
#32413 = LINE ( 'NONE', #37368, #40254 ) ;
#32414 = DIRECTION ( 'NONE',  ( 0.000000000000000000, 0.000000000000000000, 1.000000000000000000 ) ) ;
#32415 = ORIENTED_EDGE ( 'NONE', *, *, #26224, .F. ) ;
#32416 = LINE ( 'NONE', #26408, #63757 ) ;
#32417 = DIRECTION ( 'NONE',  ( -1.000000000000000000, 0.000000000000000000, 0.000000000000000000 ) ) ;
#32418 = FACE_OUTER_BOUND ( 'NONE', #16674, .T. ) ;
#32419 = EDGE_CURVE ( 'NONE', #31147, #47898, #15832, .T. ) ;
#32420 = CIRCLE ( 'NONE', #56119, 1.000000000000000000 ) ;
#32421 = CARTESIAN_POINT ( 'NONE',  ( -9.690000000000001279, 9.690000000000001279, -4.250000000000000000 ) ) ;
#32422 = FACE_OUTER_BOUND ( 'NONE', #68927, .T. ) ;
#32423 = LINE ( 'NONE', #33786, #64468 ) ;
#32424 = VERTEX_POINT ( 'NONE', #36237 ) ;
#32425 = EDGE_CURVE ( 'NONE', #51349, #14532, #40655, .T. ) ;
#32426 = AXIS2_PLACEMENT_3D ( 'NONE', #8812, #57248, #39917 ) ;
#32427 = ORIENTED_EDGE ( 'NONE', *, *, #50077, .T. ) ;
#32428 = DIRECTION ( 'NONE',  ( -0.000000000000000000, -1.000000000000000000, -0.000000000000000000 ) ) ;
#32429 = CYLINDRICAL_SURFACE ( 'NONE', #65062, 1.224999999999998757 ) ;
#32430 = ORIENTED_EDGE ( 'NONE', *, *, #42968, .F. ) ;
#32431 = EDGE_CURVE ( 'NONE', #49465, #15450, #26686, .T. ) ;
#32432 = FACE_OUTER_BOUND ( 'NONE', #9929, .T. ) ;
#32433 = CARTESIAN_POINT ( 'NONE',  ( 275.0000000000000000, -42.00000000000000000, -7.000000000000000000 ) ) ;
#32434 = EDGE_CURVE ( 'NONE', #48863, #54361, #31315, .T. ) ;
#32435 = ORIENTED_EDGE ( 'NONE', *, *, #45677, .T. ) ;
#32436 = CARTESIAN_POINT ( 'NONE',  ( 28.90000000000000213, 0.000000000000000000, 2.458500000000000796 ) ) ;
#32437 = ORIENTED_EDGE ( 'NONE', *, *, #24208, .F. ) ;
#32438 = EDGE_CURVE ( 'NONE', #53130, #19388, #52512, .T. ) ;
#32439 = ORIENTED_EDGE ( 'NONE', *, *, #19469, .T. ) ;
#32440 = PLANE ( 'NONE',  #8040 ) ;
#32441 = VERTEX_POINT ( 'NONE', #10423 ) ;
#32442 = CARTESIAN_POINT ( 'NONE',  ( 1.480523737882788238, -9.404523737882783507, 26.00000000000000000 ) ) ;
#32443 = CARTESIAN_POINT ( 'NONE',  ( -11.25000000000000000, 11.18999999999999950, -4.250000000000000000 ) ) ;
#32444 = DIRECTION ( 'NONE',  ( 0.000000000000000000, 0.000000000000000000, -1.000000000000000000 ) ) ;
#32445 = VECTOR ( 'NONE', #61681, 1000.000000000000000 ) ;
#32446 = ORIENTED_EDGE ( 'NONE', *, *, #21564, .F. ) ;
#32447 = ORIENTED_EDGE ( 'NONE', *, *, #41863, .T. ) ;
#32448 = DIRECTION ( 'NONE',  ( 1.000000000000000000, 0.000000000000000000, 0.000000000000000000 ) ) ;
#32449 = EDGE_CURVE ( 'NONE', #4444, #48626, #37296, .T. ) ;
#32451 = CARTESIAN_POINT ( 'NONE',  ( 2.906483450353342324, -11.12648345035346331, 455.0000000000000568 ) ) ;
#32450 = DIRECTION ( 'NONE',  ( -1.000000000000000000, -5.013651664672856055E-16, -1.841985738954423698E-31 ) ) ;
#32452 = ORIENTED_EDGE ( 'NONE', *, *, #25290, .F. ) ;
#32453 = EDGE_LOOP ( 'NONE', ( #69001, #41275, #63533, #24063 ) ) ;
#32454 = EDGE_CURVE ( 'NONE', #60315, #35394, #47216, .T. ) ;
#32456 = ORIENTED_EDGE ( 'NONE', *, *, #16335, .F. ) ;
#32455 = APPLICATION_PROTOCOL_DEFINITION ( 'draft international standard', 'automotive_design', 1998, #28643 ) ;
#32457 = AXIS2_PLACEMENT_3D ( 'NONE', #42384, #14112, #63975 ) ;
#32458 = AXIS2_PLACEMENT_3D ( 'NONE', #65272, #15771, #5861 ) ;
#32459 = DIRECTION ( 'NONE',  ( 0.000000000000000000, 0.000000000000000000, 1.000000000000000000 ) ) ;
#32461 = ORIENTED_EDGE ( 'NONE', *, *, #1675, .T. ) ;
#32460 = CARTESIAN_POINT ( 'NONE',  ( 2.906483450353343656, -10.92648345035346402, 455.0000000000000568 ) ) ;
#32462 = AXIS2_PLACEMENT_3D ( 'NONE', #49954, #7162, #1517 ) ;
#32463 = AXIS2_PLACEMENT_3D ( 'NONE', #34246, #45210, #8073 ) ;
#32464 = FACE_OUTER_BOUND ( 'NONE', #4884, .T. ) ;
#32465 = CARTESIAN_POINT ( 'NONE',  ( 47.00000000000000000, 0.7500000000000000000, -4.943429983321300014 ) ) ;
#32466 = ORIENTED_EDGE ( 'NONE', *, *, #28577, .F. ) ;
#32467 = VERTEX_POINT ( 'NONE', #25999 ) ;
#32468 = VECTOR ( 'NONE', #32043, 1000.000000000000000 ) ;
#32469 = VECTOR ( 'NONE', #44842, 1000.000000000000000 ) ;
#32470 = LINE ( 'NONE', #21160, #13152 ) ;
#32471 = ORIENTED_EDGE ( 'NONE', *, *, #65201, .T. ) ;
#32472 = DIRECTION ( 'NONE',  ( -1.000000000000000000, 0.000000000000000000, 0.000000000000000000 ) ) ;
#32473 = CARTESIAN_POINT ( 'NONE',  ( 151.5599459900709860, 0.000000000000000000, 324.6739988703752715 ) ) ;
#32474 = EDGE_CURVE ( 'NONE', #32678, #68170, #33826, .T. ) ;
#32475 = VERTEX_POINT ( 'NONE', #21023 ) ;
#32476 = EDGE_CURVE ( 'NONE', #33832, #53367, #57804, .T. ) ;
#32477 = VECTOR ( 'NONE', #26476, 1000.000000000000000 ) ;
#32478 = SURFACE_STYLE_USAGE ( .BOTH. , #20804 ) ;
#32479 = LINE ( 'NONE', #15859, #40303 ) ;
#32481 = VERTEX_POINT ( 'NONE', #63469 ) ;
#32480 = CARTESIAN_POINT ( 'NONE',  ( -8.250000000000001776, -7.249999999999998224, -20.50000000000000000 ) ) ;
#32482 = ORIENTED_EDGE ( 'NONE', *, *, #34647, .T. ) ;
#32483 = LINE ( 'NONE', #20121, #25298 ) ;
#32484 = CARTESIAN_POINT ( 'NONE',  ( 7.250000000000005329, -8.249999999999998224, -8.000000000000000000 ) ) ;
#32485 = CARTESIAN_POINT ( 'NONE',  ( 46.39999999999999858, 21.00000000000000000, 0.7500000000000000000 ) ) ;
#32486 = CYLINDRICAL_SURFACE ( 'NONE', #53233, 0.8100000000000017186 ) ;
#32487 = DIRECTION ( 'NONE',  ( 1.000000000000000000, 0.000000000000000000, 0.000000000000000000 ) ) ;
#32488 = VERTEX_POINT ( 'NONE', #42240 ) ;
#32489 = DIRECTION ( 'NONE',  ( 0.000000000000000000, 0.000000000000000000, 1.000000000000000000 ) ) ;
#32490 = CARTESIAN_POINT ( 'NONE',  ( 7.450000000000006395, 7.250000000000000888, -7.000000000000000000 ) ) ;
#32491 = DIRECTION ( 'NONE',  ( 0.000000000000000000, 1.000000000000000000, 0.000000000000000000 ) ) ;
#32493 = VERTEX_POINT ( 'NONE', #9371 ) ;
#32492 = DIRECTION ( 'NONE',  ( -1.047444401652940007E-14, -1.000000000000000000, -1.836970198721029934E-16 ) ) ;
#32494 = DIRECTION ( 'NONE',  ( -1.047444401652940007E-14, -1.000000000000000000, -1.836970198721029934E-16 ) ) ;
#32495 = DIRECTION ( 'NONE',  ( -0.000000000000000000, -0.000000000000000000, -1.000000000000000000 ) ) ;
#32496 = CARTESIAN_POINT ( 'NONE',  ( 8.250000000000005329, 7.250000000000000888, -22.00000000000000000 ) ) ;
#32497 = LINE ( 'NONE', #32830, #33131 ) ;
#32498 = VERTEX_POINT ( 'NONE', #25284 ) ;
#32499 = CARTESIAN_POINT ( 'NONE',  ( 7.357023737882797398, 4.947141984184415087, 54.00000000000000711 ) ) ;
#32500 = CARTESIAN_POINT ( 'NONE',  ( 15.50000000000000000, -5.000000000000000000, 22.50000000000000000 ) ) ;
#32501 = VERTEX_POINT ( 'NONE', #47895 ) ;
#32502 = DIRECTION ( 'NONE',  ( 0.000000000000000000, 0.000000000000000000, 1.000000000000000000 ) ) ;
#32503 = DIRECTION ( 'NONE',  ( 0.000000000000000000, 3.673940397442059868E-16, -1.000000000000000000 ) ) ;
#32504 = CIRCLE ( 'NONE', #53955, 4.000000000000000000 ) ;
#32505 = PLANE ( 'NONE',  #62553 ) ;
#32506 = DIRECTION ( 'NONE',  ( 0.000000000000000000, 1.000000000000000000, -0.000000000000000000 ) ) ;
#32507 = AXIS2_PLACEMENT_3D ( 'NONE', #12042, #11362, #54515 ) ;
#32508 = EDGE_CURVE ( 'NONE', #51395, #5174, #15029, .T. ) ;
#32510 = CARTESIAN_POINT ( 'NONE',  ( 41.09999999999999432, 20.60000000000000142, 13.86939075806900057 ) ) ;
#32509 = AXIS2_PLACEMENT_3D ( 'NONE', #57762, #4392, #68733 ) ;
#32511 = ORIENTED_EDGE ( 'NONE', *, *, #23176, .T. ) ;
#32512 = VERTEX_POINT ( 'NONE', #9729 ) ;
#32513 = DIRECTION ( 'NONE',  ( -1.000000000000000000, 0.000000000000000000, 0.000000000000000000 ) ) ;
#32514 = EDGE_LOOP ( 'NONE', ( #26569, #59805, #21166, #58551, #41133, #45229, #12637, #31931 ) ) ;
#32515 = DIRECTION ( 'NONE',  ( 1.000000000000000000, 0.000000000000000000, 0.000000000000000000 ) ) ;
#32516 = VECTOR ( 'NONE', #7395, 1000.000000000000000 ) ;
#32517 = ORIENTED_EDGE ( 'NONE', *, *, #49405, .F. ) ;
#32518 = EDGE_CURVE ( 'NONE', #24504, #18955, #52882, .T. ) ;
#32519 = CARTESIAN_POINT ( 'NONE',  ( -4.193516549646675529, 11.11351654964658842, 195.0000000000000284 ) ) ;
#32520 = AXIS2_PLACEMENT_3D ( 'NONE', #5092, #68747, #20298 ) ;
#32521 = VECTOR ( 'NONE', #56766, 1000.000000000000114 ) ;
#32522 = EDGE_CURVE ( 'NONE', #44169, #11224, #4438, .T. ) ;
#32523 = EDGE_CURVE ( 'NONE', #61811, #59233, #53565, .T. ) ;
#32524 = CARTESIAN_POINT ( 'NONE',  ( -1.991476262117235274, 8.598420958951582094, 26.00000000000000711 ) ) ;
#32525 = DIRECTION ( 'NONE',  ( -1.000000000000000000, 0.000000000000000000, 0.000000000000000000 ) ) ;
#32526 = EDGE_LOOP ( 'NONE', ( #32456, #46034, #6342, #37877 ) ) ;
#32527 = EDGE_CURVE ( 'NONE', #31007, #64218, #41188, .T. ) ;
#32528 = ORIENTED_EDGE ( 'NONE', *, *, #2571, .F. ) ;
#32529 = EDGE_CURVE ( 'NONE', #19212, #33635, #35899, .T. ) ;
#32530 = DIRECTION ( 'NONE',  ( 0.000000000000000000, 1.000000000000000000, 0.000000000000000000 ) ) ;
#32531 = ORIENTED_EDGE ( 'NONE', *, *, #45787, .T. ) ;
#32532 = ORIENTED_EDGE ( 'NONE', *, *, #4683, .F. ) ;
#32533 = AXIS2_PLACEMENT_3D ( 'NONE', #17581, #26833, #44111 ) ;
#32534 = DIRECTION ( 'NONE',  ( -1.000000000000000000, 0.000000000000000000, 0.000000000000000000 ) ) ;
#32535 = CARTESIAN_POINT ( 'NONE',  ( 8.406483450353379183, -5.668387132716048882, 455.0000000000000568 ) ) ;
#32536 = LINE ( 'NONE', #54781, #12898 ) ;
#32537 = ADVANCED_FACE ( 'NONE', ( #14675 ), #37998, .F. ) ;
#32538 = VERTEX_POINT ( 'NONE', #22080 ) ;
#32539 = DIRECTION ( 'NONE',  ( -1.000000000000000000, 0.000000000000000000, 0.000000000000000000 ) ) ;
#32541 = DIRECTION ( 'NONE',  ( 0.000000000000000000, 0.000000000000000000, -1.000000000000000000 ) ) ;
#32540 = CYLINDRICAL_SURFACE ( 'NONE', #31004, 2.215251240775983899 ) ;
#32542 = EDGE_LOOP ( 'NONE', ( #32608, #20765 ) ) ;
#32543 = EDGE_LOOP ( 'NONE', ( #32550, #26544, #47248, #2677, #2143, #60706 ) ) ;
#32545 = ORIENTED_EDGE ( 'NONE', *, *, #32860, .T. ) ;
#32544 = DIRECTION ( 'NONE',  ( 1.000000000000000000, -0.000000000000000000, -0.000000000000000000 ) ) ;
#32546 = ORIENTED_EDGE ( 'NONE', *, *, #50132, .F. ) ;
#32547 = LINE ( 'NONE', #27238, #22009 ) ;
#32548 = FACE_OUTER_BOUND ( 'NONE', #36024, .T. ) ;
#32549 = CIRCLE ( 'NONE', #51716, 24.99999999998794920 ) ;
#32550 = ORIENTED_EDGE ( 'NONE', *, *, #69725, .F. ) ;
#32551 = VERTEX_POINT ( 'NONE', #65887 ) ;
#32552 = LINE ( 'NONE', #54116, #10951 ) ;
#32553 = CARTESIAN_POINT ( 'NONE',  ( 41.09999999999999432, -21.00000000000000000, 13.86939075806900057 ) ) ;
#32554 = ORIENTED_EDGE ( 'NONE', *, *, #12025, .T. ) ;
#32555 = VERTEX_POINT ( 'NONE', #64868 ) ;
#32556 = CARTESIAN_POINT ( 'NONE',  ( 23.90000000000000213, 13.66939075806899240, -20.79999999999999361 ) ) ;
#32557 = DIRECTION ( 'NONE',  ( 0.000000000000000000, 1.000000000000000000, 0.000000000000000000 ) ) ;
#32558 = CARTESIAN_POINT ( 'NONE',  ( 7.250000000000005329, -7.249999999999998224, -19.00000000000000000 ) ) ;
#32559 = ORIENTED_EDGE ( 'NONE', *, *, #58060, .T. ) ;
#32560 = CIRCLE ( 'NONE', #3171, 4.000000000000001776 ) ;
#32561 = EDGE_CURVE ( 'NONE', #59963, #7366, #49970, .T. ) ;
#32562 = DIRECTION ( 'NONE',  ( 1.000000000000000000, -0.000000000000000000, 0.000000000000000000 ) ) ;
#32563 = CARTESIAN_POINT ( 'NONE',  ( 11.00000000000000000, -5.599999999999999645, 9.000000000000001776 ) ) ;
#32566 = EDGE_LOOP ( 'NONE', ( #2243, #6372, #47570, #11043 ) ) ;
#32565 = EDGE_CURVE ( 'NONE', #14694, #67830, #65224, .T. ) ;
#32564 = CARTESIAN_POINT ( 'NONE',  ( 7.000000000000000000, -21.00000000000000000, 12.50000000000000000 ) ) ;
#32568 = ORIENTED_EDGE ( 'NONE', *, *, #8638, .F. ) ;
#32567 = CARTESIAN_POINT ( 'NONE',  ( 2.632023737882809744, -6.501044194225475081, 54.00000000000000711 ) ) ;
#32569 = EDGE_CURVE ( 'NONE', #28387, #14058, #5479, .T. ) ;
#32570 = CARTESIAN_POINT ( 'NONE',  ( -30.00000000000000000, -5.200000000000001066, 9.400000000000000355 ) ) ;
#32571 = VECTOR ( 'NONE', #13020, 1000.000000000000000 ) ;
#32572 = CARTESIAN_POINT ( 'NONE',  ( -7.450000000000001954, 7.250000000000000000, -10.50000000000000000 ) ) ;
#32573 = CARTESIAN_POINT ( 'NONE',  ( -16.75000000000000000, -0.2714405302574915413, -22.01253933645463334 ) ) ;
#32574 = CARTESIAN_POINT ( 'NONE',  ( -6.749999999999998224, 7.750000000000001776, 0.000000000000000000 ) ) ;
#32575 = EDGE_CURVE ( 'NONE', #21671, #11939, #44312, .T. ) ;
#32576 = CARTESIAN_POINT ( 'NONE',  ( -7.250000000000000888, 7.250000000000001776, -26.00000000000001066 ) ) ;
#32577 = DIRECTION ( 'NONE',  ( 0.000000000000000000, -1.000000000000000000, 0.000000000000000000 ) ) ;
#32578 = ORIENTED_EDGE ( 'NONE', *, *, #67472, .T. ) ;
#32579 = CARTESIAN_POINT ( 'NONE',  ( 28.90000000000000213, 3.010794155703768650E-16, -2.458500000000000796 ) ) ;
#32581 = EDGE_LOOP ( 'NONE', ( #57132, #4608, #7895, #3670 ) ) ;
#32580 = CARTESIAN_POINT ( 'NONE',  ( 13.00000000000000178, -17.50000000000000000, -15.70500000000000007 ) ) ;
#32583 = EDGE_LOOP ( 'NONE', ( #56662, #52911, #22211, #49619 ) ) ;
#32582 = CARTESIAN_POINT ( 'NONE',  ( 7.000000000000000000, -32.46196062927499781, 8.091291340630698770 ) ) ;
#32584 = CARTESIAN_POINT ( 'NONE',  ( 41.09999999999999432, 20.60000000000000142, 13.86939075806900057 ) ) ;
#32585 = DIRECTION ( 'NONE',  ( -1.000000000000000000, 0.000000000000000000, 0.000000000000000000 ) ) ;
#32586 = VERTEX_POINT ( 'NONE', #11114 ) ;
#32587 = DIRECTION ( 'NONE',  ( -8.673617379884087537E-15, -1.000000000000000000, 0.000000000000000000 ) ) ;
#32588 = DIRECTION ( 'NONE',  ( 0.000000000000000000, -0.6857142857147903170, 0.7278708115913530285 ) ) ;
#32589 = ORIENTED_EDGE ( 'NONE', *, *, #1486, .T. ) ;
#32590 = CARTESIAN_POINT ( 'NONE',  ( 41.09999999999999432, 13.66939075806899950, -20.80000000000000426 ) ) ;
#32591 = DIRECTION ( 'NONE',  ( -0.7671651518153028704, -0.6414496315691537998, -2.587583378555113506E-16 ) ) ;
#32592 = DIRECTION ( 'NONE',  ( -1.000000000000000000, 0.000000000000000000, 0.000000000000000000 ) ) ;
#32593 = EDGE_CURVE ( 'NONE', #27615, #8637, #18033, .T. ) ;
#32594 = ORIENTED_EDGE ( 'NONE', *, *, #6732, .T. ) ;
#32595 = DIRECTION ( 'NONE',  ( -1.000000000000000000, 1.254221251785257731E-14, 1.836970198721053107E-16 ) ) ;
#32596 = ORIENTED_EDGE ( 'NONE', *, *, #490, .T. ) ;
#32597 = VERTEX_POINT ( 'NONE', #59896 ) ;
#32598 = CARTESIAN_POINT ( 'NONE',  ( 6.619341603356837744, -4.747751991980742936, 455.0000000000000568 ) ) ;
#32599 = CARTESIAN_POINT ( 'NONE',  ( 283.0000000000000568, -20.40000000000000213, 12.40000000000000213 ) ) ;
#32600 = DIRECTION ( 'NONE',  ( -1.000000000000000000, 0.000000000000000000, 0.000000000000000000 ) ) ;
#32601 = DIRECTION ( 'NONE',  ( 0.000000000000000000, 0.000000000000000000, 1.000000000000000000 ) ) ;
#32602 = ORIENTED_EDGE ( 'NONE', *, *, #64840, .F. ) ;
#32603 = EDGE_CURVE ( 'NONE', #44836, #46298, #42941, .T. ) ;
#32604 = VERTEX_POINT ( 'NONE', #64522 ) ;
#32605 = EDGE_CURVE ( 'NONE', #26123, #7845, #59212, .T. ) ;
#32607 = VERTEX_POINT ( 'NONE', #32680 ) ;
#32606 = CARTESIAN_POINT ( 'NONE',  ( 275.0000000000000000, -25.00000000000000000, -17.50000000000000000 ) ) ;
#32608 = ORIENTED_EDGE ( 'NONE', *, *, #41694, .T. ) ;
#32609 = VECTOR ( 'NONE', #40577, 1000.000000000000000 ) ;
#32610 = DIRECTION ( 'NONE',  ( -1.836970198721029934E-16, 1.836970198721036344E-16, -1.000000000000000000 ) ) ;
#32611 = DIRECTION ( 'NONE',  ( 1.000000000000000000, -0.000000000000000000, -0.000000000000000000 ) ) ;
#32612 = EDGE_CURVE ( 'NONE', #33806, #23316, #27034, .T. ) ;
#32613 = PLANE ( 'NONE',  #59056 ) ;
#32614 = VECTOR ( 'NONE', #52479, 1000.000000000000000 ) ;
#32615 = CARTESIAN_POINT ( 'NONE',  ( -11.00000000000000000, -8.959999999999999076, -12.95475478405700009 ) ) ;
#32617 = CARTESIAN_POINT ( 'NONE',  ( -7.250000000000000888, 7.250000000000001776, -11.00000000000000000 ) ) ;
#32616 = DIRECTION ( 'NONE',  ( 0.000000000000000000, -1.000000000000000000, 0.000000000000000000 ) ) ;
#32618 = ORIENTED_EDGE ( 'NONE', *, *, #9239, .F. ) ;
#32620 = ORIENTED_EDGE ( 'NONE', *, *, #53279, .F. ) ;
#32619 = CYLINDRICAL_SURFACE ( 'NONE', #57869, 0.1749999999999998224 ) ;
#32621 = ORIENTED_EDGE ( 'NONE', *, *, #50695, .F. ) ;
#32622 = ORIENTED_EDGE ( 'NONE', *, *, #68341, .F. ) ;
#32623 = LINE ( 'NONE', #59490, #28801 ) ;
#32624 = FACE_OUTER_BOUND ( 'NONE', #52705, .T. ) ;
#32625 = DIRECTION ( 'NONE',  ( -1.000000000000000000, 0.000000000000000000, 0.000000000000000000 ) ) ;
#32626 = ORIENTED_EDGE ( 'NONE', *, *, #14123, .F. ) ;
#32627 = EDGE_LOOP ( 'NONE', ( #41488, #26017 ) ) ;
#32628 = ORIENTED_EDGE ( 'NONE', *, *, #2822, .F. ) ;
#32629 = CARTESIAN_POINT ( 'NONE',  ( -11.11351654964671098, 7.793516549646603231, 455.0000000000000568 ) ) ;
#32630 = CARTESIAN_POINT ( 'NONE',  ( 25.50000000000000355, -5.200000000000001066, 22.50000000000000000 ) ) ;
#32631 = DIRECTION ( 'NONE',  ( -0.6414496315691484707, 0.7671651518153074223, 2.309356642088893343E-17 ) ) ;
#32632 = VERTEX_POINT ( 'NONE', #54261 ) ;
#32633 = ORIENTED_EDGE ( 'NONE', *, *, #31063, .F. ) ;
#32634 = DIRECTION ( 'NONE',  ( 0.000000000000000000, 0.000000000000000000, 1.000000000000000000 ) ) ;
#32635 = DIRECTION ( 'NONE',  ( 0.000000000000000000, -3.673940397442059868E-16, 1.000000000000000000 ) ) ;
#32636 = ORIENTED_EDGE ( 'NONE', *, *, #52764, .F. ) ;
#32637 = DIRECTION ( 'NONE',  ( -3.491481338843133355E-15, -1.000000000000000000, -1.836970198721029934E-16 ) ) ;
#32640 = ORIENTED_EDGE ( 'NONE', *, *, #41069, .F. ) ;
#32639 = ADVANCED_FACE ( 'NONE', ( #22428 ), #28400, .F. ) ;
#32638 = DIRECTION ( 'NONE',  ( 1.836970198721029934E-16, 1.836970198721010706E-16, -1.000000000000000000 ) ) ;
#32641 = ORIENTED_EDGE ( 'NONE', *, *, #49996, .F. ) ;
#32642 = EDGE_CURVE ( 'NONE', #62873, #167, #43289, .T. ) ;
#32643 = ADVANCED_FACE ( 'NONE', ( #33714 ), #53919, .F. ) ;
#32644 = CARTESIAN_POINT ( 'NONE',  ( -15.50000000000000000, -0.2000000000000000111, -19.20000000000052509 ) ) ;
#32645 = CARTESIAN_POINT ( 'NONE',  ( 8.711985858128693749, -2.420780051175180692, 54.00000000000000711 ) ) ;
#32646 = DIRECTION ( 'NONE',  ( 1.000000000000000000, 0.000000000000000000, 0.000000000000000000 ) ) ;
#32647 = LINE ( 'NONE', #1492, #13157 ) ;
#32648 = ADVANCED_FACE ( 'NONE', ( #17108 ), #54959, .F. ) ;
#32649 = AXIS2_PLACEMENT_3D ( 'NONE', #68080, #9746, #57468 ) ;
#32650 = LINE ( 'NONE', #65187, #55334 ) ;
#32651 = ORIENTED_EDGE ( 'NONE', *, *, #36284, .F. ) ;
#32652 = DIRECTION ( 'NONE',  ( -1.836970198721029934E-16, 1.836970198721036344E-16, -1.000000000000000000 ) ) ;
#32653 = VERTEX_POINT ( 'NONE', #6831 ) ;
#32654 = DIRECTION ( 'NONE',  ( 1.000000000000000000, 0.000000000000000000, 0.000000000000000000 ) ) ;
#32655 = DIRECTION ( 'NONE',  ( 0.000000000000000000, 0.000000000000000000, -1.000000000000000000 ) ) ;
#32656 = CARTESIAN_POINT ( 'NONE',  ( -7.249999999999995559, -7.848062532927998269, 5.000000000000000000 ) ) ;
#32657 = DIRECTION ( 'NONE',  ( 0.000000000000000000, 0.000000000000000000, -1.000000000000000000 ) ) ;
#32658 = AXIS2_PLACEMENT_3D ( 'NONE', #1496, #23765, #33341 ) ;
#32659 = DIRECTION ( 'NONE',  ( 0.7071067811865550112, 0.7071067811865401342, 2.597868168706466299E-16 ) ) ;
#32660 = EDGE_LOOP ( 'NONE', ( #64661, #60933, #21814, #21312 ) ) ;
#32661 = CIRCLE ( 'NONE', #19123, 3.999999999999993339 ) ;
#32662 = PLANE ( 'NONE',  #42677 ) ;
#32663 = FACE_OUTER_BOUND ( 'NONE', #65831, .T. ) ;
#32664 = VECTOR ( 'NONE', #35567, 1000.000000000000000 ) ;
#32665 = ORIENTED_EDGE ( 'NONE', *, *, #31239, .F. ) ;
#32666 = LINE ( 'NONE', #54943, #39500 ) ;
#32667 = CARTESIAN_POINT ( 'NONE',  ( -11.31351654964671027, 7.593516549646603941, 455.0000000000000568 ) ) ;
#32668 = VERTEX_POINT ( 'NONE', #38680 ) ;
#32669 = DIRECTION ( 'NONE',  ( -1.836970198721029934E-16, 1.836970198721036590E-16, -1.000000000000000000 ) ) ;
#32670 = FACE_OUTER_BOUND ( 'NONE', #22445, .T. ) ;
#32671 = VERTEX_POINT ( 'NONE', #43975 ) ;
#32672 = DIRECTION ( 'NONE',  ( 0.4998444328988824181, 0.000000000000000000, -0.8661152018640445593 ) ) ;
#32673 = CARTESIAN_POINT ( 'NONE',  ( 41.09999999999999432, 13.66939075806899950, 20.80000000000000426 ) ) ;
#32674 = CARTESIAN_POINT ( 'NONE',  ( -10.49297626211729551, -6.849523737882748264, 54.00000000000000711 ) ) ;
#32675 = CARTESIAN_POINT ( 'NONE',  ( -4.383466043307859827, 8.393516549646591329, 195.0000000000000284 ) ) ;
#32676 = ORIENTED_EDGE ( 'NONE', *, *, #30203, .F. ) ;
#32678 = VERTEX_POINT ( 'NONE', #65554 ) ;
#32677 = DIRECTION ( 'NONE',  ( 8.951101527228104953E-17, 1.000000000000000000, 0.000000000000000000 ) ) ;
#32679 = EDGE_CURVE ( 'NONE', #36149, #44524, #60234, .T. ) ;
#32680 = CARTESIAN_POINT ( 'NONE',  ( 40.90000000000000568, 13.66939075806899240, 20.79999999999999361 ) ) ;
#32681 = EDGE_CURVE ( 'NONE', #43112, #15685, #68886, .T. ) ;
#32682 = CARTESIAN_POINT ( 'NONE',  ( 41.09999999999999432, -21.00000000000000000, 13.86939075806900057 ) ) ;
#32683 = VECTOR ( 'NONE', #25492, 1000.000000000000114 ) ;
#32684 = CYLINDRICAL_SURFACE ( 'NONE', #20640, 0.3499999999999996447 ) ;
#32685 = VERTEX_POINT ( 'NONE', #39706 ) ;
#32686 = EDGE_CURVE ( 'NONE', #53157, #11546, #50669, .T. ) ;
#32687 = CARTESIAN_POINT ( 'NONE',  ( -30.00000000000000000, -15.97213595500069871, -14.50000000000000000 ) ) ;
#32688 = LINE ( 'NONE', #518, #68029 ) ;
#32689 = EDGE_CURVE ( 'NONE', #38911, #1574, #39480, .T. ) ;
#32690 = ORIENTED_EDGE ( 'NONE', *, *, #3138, .F. ) ;
#32691 = ORIENTED_EDGE ( 'NONE', *, *, #15311, .T. ) ;
#32692 = ADVANCED_FACE ( 'NONE', ( #67639 ), #55631, .T. ) ;
#32693 = EDGE_CURVE ( 'NONE', #4940, #20447, #7174, .T. ) ;
#32694 = ORIENTED_EDGE ( 'NONE', *, *, #61020, .F. ) ;
#32695 = EDGE_CURVE ( 'NONE', #63351, #61661, #44655, .T. ) ;
#32696 = DIRECTION ( 'NONE',  ( -0.000000000000000000, -0.000000000000000000, -1.000000000000000000 ) ) ;
#32697 = EDGE_CURVE ( 'NONE', #48298, #33481, #66585, .T. ) ;
#32698 = AXIS2_PLACEMENT_3D ( 'NONE', #50150, #51196, #17967 ) ;
#32699 = DIRECTION ( 'NONE',  ( 0.000000000000000000, 0.000000000000000000, -1.000000000000000000 ) ) ;
#32700 = ORIENTED_EDGE ( 'NONE', *, *, #25340, .F. ) ;
#32701 = VERTEX_POINT ( 'NONE', #28748 ) ;
#32702 = EDGE_LOOP ( 'NONE', ( #60621, #28715, #58443, #32511 ) ) ;
#32703 = AXIS2_PLACEMENT_3D ( 'NONE', #23335, #27601, #55173 ) ;
#32704 = CARTESIAN_POINT ( 'NONE',  ( 283.0000000000000568, -20.50000000000000000, 17.00000000000000000 ) ) ;
#32705 = VERTEX_POINT ( 'NONE', #7533 ) ;
#32706 = EDGE_LOOP ( 'NONE', ( #30963, #2860, #51831, #46809 ) ) ;
#32707 = VERTEX_POINT ( 'NONE', #40763 ) ;
#32708 = VECTOR ( 'NONE', #48417, 1000.000000000000000 ) ;
#32709 = ORIENTED_EDGE ( 'NONE', *, *, #15986, .F. ) ;
#32710 = DIRECTION ( 'NONE',  ( 0.000000000000000000, 0.000000000000000000, 1.000000000000000000 ) ) ;
#32712 = EDGE_LOOP ( 'NONE', ( #64289, #15818, #45365, #53179, #54777, #65473, #49328 ) ) ;
#32711 = CARTESIAN_POINT ( 'NONE',  ( -5.779227145995285753, 4.141586236041028712, 54.00000000000000711 ) ) ;
#32713 = VECTOR ( 'NONE', #39082, 1000.000000000000000 ) ;
#32714 = DIRECTION ( 'NONE',  ( -1.000000000000000000, 2.602085213965213008E-15, 0.000000000000000000 ) ) ;
#32715 = CARTESIAN_POINT ( 'NONE',  ( 11.32648345035337734, -4.406483450353491982, 455.0000000000000568 ) ) ;
#32716 = DIRECTION ( 'NONE',  ( 0.000000000000000000, -1.000000000000000000, 0.000000000000000000 ) ) ;
#32717 = ORIENTED_EDGE ( 'NONE', *, *, #10358, .F. ) ;
#32718 = VECTOR ( 'NONE', #45051, 1000.000000000000114 ) ;
#32719 = DIRECTION ( 'NONE',  ( 0.7671651518153105309, 0.6414496315691445849, 2.356647714346206145E-16 ) ) ;
#32720 = ORIENTED_EDGE ( 'NONE', *, *, #18867, .T. ) ;
#32721 = FACE_BOUND ( 'NONE', #150, .T. ) ;
#32722 = DIRECTION ( 'NONE',  ( 0.000000000000000000, 0.000000000000000000, -1.000000000000000000 ) ) ;
#32723 = CARTESIAN_POINT ( 'NONE',  ( -7.250000000000000888, 7.450000000000003730, -15.50000000000000000 ) ) ;
#32724 = CIRCLE ( 'NONE', #2234, 1.929199999999998028 ) ;
#32725 = VERTEX_POINT ( 'NONE', #29449 ) ;
#32726 = CYLINDRICAL_SURFACE ( 'NONE', #62942, 0.5000000000079367624 ) ;
#32727 = EDGE_CURVE ( 'NONE', #32123, #58343, #45010, .T. ) ;
#32728 = DIRECTION ( 'NONE',  ( 1.000000000000000000, 0.000000000000000000, 0.000000000000000000 ) ) ;
#32729 = CARTESIAN_POINT ( 'NONE',  ( 11.50000000000000000, -11.50000000000000000, -15.00000000000000000 ) ) ;
#32730 = EDGE_CURVE ( 'NONE', #5474, #33142, #7873, .T. ) ;
#32731 = FACE_OUTER_BOUND ( 'NONE', #23257, .T. ) ;
#32732 = LINE ( 'NONE', #43336, #24567 ) ;
#32733 = CARTESIAN_POINT ( 'NONE',  ( -2.693516549646675529, 10.91351654964657314, 455.0000000000000568 ) ) ;
#32734 = VECTOR ( 'NONE', #16427, 1000.000000000000000 ) ;
#32735 = CARTESIAN_POINT ( 'NONE',  ( 9.955011587777235604, -9.247904806590801385, 455.0000000000000568 ) ) ;
#32736 = VECTOR ( 'NONE', #5566, 1000.000000000000000 ) ;
#32737 = LINE ( 'NONE', #49368, #63900 ) ;
#32738 = VECTOR ( 'NONE', #45508, 1000.000000000000000 ) ;
#32739 = ORIENTED_EDGE ( 'NONE', *, *, #41037, .T. ) ;
#32740 = DIRECTION ( 'NONE',  ( -1.794541526872559352E-16, -1.000000000000000000, 0.000000000000000000 ) ) ;
#32741 = EDGE_CURVE ( 'NONE', #52360, #68006, #12366, .T. ) ;
#32742 = LINE ( 'NONE', #38737, #27417 ) ;
#32743 = VECTOR ( 'NONE', #20818, 1000.000000000000000 ) ;
#32744 = FACE_OUTER_BOUND ( 'NONE', #18976, .T. ) ;
#32745 = DIRECTION ( 'NONE',  ( 1.000000000000000000, 0.000000000000000000, 0.000000000000000000 ) ) ;
#32746 = ORIENTED_EDGE ( 'NONE', *, *, #52435, .T. ) ;
#32747 = LINE ( 'NONE', #21795, #59252 ) ;
#32748 = CARTESIAN_POINT ( 'NONE',  ( -30.00000000000000000, -5.000000000000000000, 27.00000000000000000 ) ) ;
#32749 = EDGE_CURVE ( 'NONE', #64704, #55424, #45705, .T. ) ;
#32750 = LINE ( 'NONE', #54331, #43540 ) ;
#32751 = VECTOR ( 'NONE', #19346, 1000.000000000000000 ) ;
#32752 = CARTESIAN_POINT ( 'NONE',  ( 40.90000000000000568, -0.2000000000089119934, 8.909539772616881237E-12 ) ) ;
#32753 = CARTESIAN_POINT ( 'NONE',  ( 7.806483450353379538, -11.32648345035348925, 455.0000000000000568 ) ) ;
#32754 = CARTESIAN_POINT ( 'NONE',  ( 7.250000000000004441, 7.450000000000001954, -25.00000000000000000 ) ) ;
#32755 = AXIS2_PLACEMENT_3D ( 'NONE', #52104, #68369, #63062 ) ;
#32756 = ORIENTED_EDGE ( 'NONE', *, *, #60462, .T. ) ;
#32757 = AXIS2_PLACEMENT_3D ( 'NONE', #67621, #19178, #65124 ) ;
#32758 = EDGE_LOOP ( 'NONE', ( #3093, #30251, #35985, #31608, #18856, #69505 ) ) ;
#32759 = CARTESIAN_POINT ( 'NONE',  ( 11.00000000000000000, -8.959999999999999076, 12.95475478405700009 ) ) ;
#32760 = EDGE_CURVE ( 'NONE', #37068, #355, #12822, .T. ) ;
#32761 = DIRECTION ( 'NONE',  ( -0.000000000000000000, -0.000000000000000000, -1.000000000000000000 ) ) ;
#32762 = ORIENTED_EDGE ( 'NONE', *, *, #6285, .T. ) ;
#32763 = AXIS2_PLACEMENT_3D ( 'NONE', #33675, #7488, #49262 ) ;
#32764 = VECTOR ( 'NONE', #38446, 1000.000000000000000 ) ;
#32765 = LINE ( 'NONE', #27462, #5900 ) ;
#32766 = EDGE_LOOP ( 'NONE', ( #32331, #58087, #23838, #60218 ) ) ;
#32767 = DIRECTION ( 'NONE',  ( 0.4999999999989361843, 0.000000000000000000, -0.8660254037850529940 ) ) ;
#32768 = ORIENTED_EDGE ( 'NONE', *, *, #8612, .T. ) ;
#32769 = ORIENTED_EDGE ( 'NONE', *, *, #854, .F. ) ;
#32771 = EDGE_CURVE ( 'NONE', #22764, #55087, #55980, .T. ) ;
#32770 = DIRECTION ( 'NONE',  ( -1.836970198721029934E-16, 1.836970198721036590E-16, -1.000000000000000000 ) ) ;
#32772 = ORIENTED_EDGE ( 'NONE', *, *, #53464, .F. ) ;
#32773 = CARTESIAN_POINT ( 'NONE',  ( 9.404523737882758638, 1.466476262117154983, 54.00000000000000711 ) ) ;
#32774 = ADVANCED_FACE ( 'NONE', ( #24506 ), #29107, .T. ) ;
#32775 = CARTESIAN_POINT ( 'NONE',  ( -5.242976262117275077, -5.257023737882800418, 26.00000000000000711 ) ) ;
#32776 = DIRECTION ( 'NONE',  ( 0.000000000000000000, 0.000000000000000000, -1.000000000000000000 ) ) ;
#32777 = VECTOR ( 'NONE', #61463, 1000.000000000000000 ) ;
#32778 = VERTEX_POINT ( 'NONE', #51368 ) ;
#32779 = VERTEX_POINT ( 'NONE', #18844 ) ;
#32780 = CARTESIAN_POINT ( 'NONE',  ( 7.000000000000000000, -20.50000000000000000, 13.00000000000000178 ) ) ;
#32781 = LINE ( 'NONE', #55061, #16413 ) ;
#32782 = ORIENTED_EDGE ( 'NONE', *, *, #53853, .F. ) ;
#32783 = ORIENTED_EDGE ( 'NONE', *, *, #49736, .T. ) ;
#32785 = ORIENTED_EDGE ( 'NONE', *, *, #28571, .F. ) ;
#32784 = CONTEXT_DEPENDENT_SHAPE_REPRESENTATION ( #65725, #65139 ) ;
#32786 = CYLINDRICAL_SURFACE ( 'NONE', #41268, 4.500000000000189182 ) ;
#32787 = VECTOR ( 'NONE', #48815, 1000.000000000000000 ) ;
#32789 = ORIENTED_EDGE ( 'NONE', *, *, #434, .T. ) ;
#32788 = CARTESIAN_POINT ( 'NONE',  ( 7.272650909786644746, 7.798499376343933420, 455.0000000000000568 ) ) ;
#32790 = DIRECTION ( 'NONE',  ( -1.000000000000000000, 1.334402673828312846E-16, 0.000000000000000000 ) ) ;
#32791 = VECTOR ( 'NONE', #55366, 1000.000000000000000 ) ;
#32792 = DIRECTION ( 'NONE',  ( -1.000000000000000000, 8.540177112501197482E-15, 3.137610169492823463E-30 ) ) ;
#32793 = VERTEX_POINT ( 'NONE', #61618 ) ;
#32794 = EDGE_LOOP ( 'NONE', ( #38955, #46292, #224, #20509 ) ) ;
#32795 = ORIENTED_EDGE ( 'NONE', *, *, #67714, .T. ) ;
#32796 = CIRCLE ( 'NONE', #23760, 0.2000000000000005107 ) ;
#32797 = EDGE_CURVE ( 'NONE', #7192, #54414, #56327, .T. ) ;
#32798 = DIRECTION ( 'NONE',  ( 0.000000000000000000, -0.000000000000000000, 1.000000000000000000 ) ) ;
#32799 = DIRECTION ( 'NONE',  ( -1.000000000000000000, 0.000000000000000000, 0.000000000000000000 ) ) ;
#32800 = VECTOR ( 'NONE', #118, 1000.000000000000000 ) ;
#32801 = ORIENTED_EDGE ( 'NONE', *, *, #35697, .T. ) ;
#32802 = EDGE_CURVE ( 'NONE', #16314, #60441, #24152, .T. ) ;
#32803 = CARTESIAN_POINT ( 'NONE',  ( -5.993516549646776603, -6.006483450353426790, 455.0000000000000568 ) ) ;
#32804 = LINE ( 'NONE', #21504, #818 ) ;
#32806 = ORIENTED_EDGE ( 'NONE', *, *, #46210, .F. ) ;
#32805 = CARTESIAN_POINT ( 'NONE',  ( -7.450000000000001954, -7.249999999999998224, -10.00000000000000000 ) ) ;
#32807 = ORIENTED_EDGE ( 'NONE', *, *, #3308, .F. ) ;
#32808 = ADVANCED_FACE ( 'NONE', ( #13537 ), #13888, .F. ) ;
#32809 = CARTESIAN_POINT ( 'NONE',  ( -6.835476262117327728, -10.31452373788278187, 26.00000000000000000 ) ) ;
#32810 = VECTOR ( 'NONE', #35669, 1000.000000000000000 ) ;
#32811 = AXIS2_PLACEMENT_3D ( 'NONE', #39381, #12504, #34066 ) ;
#32812 = LINE ( 'NONE', #4568, #20573 ) ;
#32813 = EDGE_CURVE ( 'NONE', #41344, #29414, #8227, .T. ) ;
#32814 = DIRECTION ( 'NONE',  ( 0.000000000000000000, 0.000000000000000000, 1.000000000000000000 ) ) ;
#32815 = CARTESIAN_POINT ( 'NONE',  ( 6.665817930929297752, -7.357023737882814274, 26.00000000000000000 ) ) ;
#32816 = EDGE_CURVE ( 'NONE', #27463, #34438, #20246, .T. ) ;
#32817 = DIRECTION ( 'NONE',  ( -1.000000000000000000, 0.000000000000000000, 0.000000000000000000 ) ) ;
#32818 = VERTEX_POINT ( 'NONE', #69383 ) ;
#32819 = CARTESIAN_POINT ( 'NONE',  ( 7.450000000000006395, 7.250000000000000888, -24.50000000000000000 ) ) ;
#32820 = DIRECTION ( 'NONE',  ( 0.000000000000000000, 0.000000000000000000, 1.000000000000000000 ) ) ;
#32821 = DIRECTION ( 'NONE',  ( -9.912705577010336396E-15, -1.000000000000000000, 0.000000000000000000 ) ) ;
#32823 = ORIENTED_EDGE ( 'NONE', *, *, #58008, .F. ) ;
#32822 = CARTESIAN_POINT ( 'NONE',  ( -4.193516549646831848, -11.12648345035344377, 455.0000000000000568 ) ) ;
#32824 = CARTESIAN_POINT ( 'NONE',  ( 21.90000000000000213, 13.66939075806899240, -20.79999999999999361 ) ) ;
#32825 = VECTOR ( 'NONE', #44420, 1000.000000000000000 ) ;
#32826 = DIRECTION ( 'NONE',  ( 1.000000000000000000, 0.000000000000000000, 0.000000000000000000 ) ) ;
#32827 = EDGE_CURVE ( 'NONE', #354, #8396, #20941, .T. ) ;
#32828 = CARTESIAN_POINT ( 'NONE',  ( -17.51999999999999957, -17.50000000000000000, 26.00000000000000355 ) ) ;
#32829 = ADVANCED_FACE ( 'NONE', ( #19538 ), #4357, .F. ) ;
#32830 = CARTESIAN_POINT ( 'NONE',  ( -8.250000000000001776, 7.250000000000000888, -26.00000000000001066 ) ) ;
#32831 = ORIENTED_EDGE ( 'NONE', *, *, #4465, .T. ) ;
#32832 = FACE_OUTER_BOUND ( 'NONE', #31640, .T. ) ;
#32833 = CARTESIAN_POINT ( 'NONE',  ( 7.428221114745003462, -3.606483450353489939, 455.0000000000000568 ) ) ;
#32834 = ORIENTED_EDGE ( 'NONE', *, *, #56098, .T. ) ;
#32835 = CARTESIAN_POINT ( 'NONE',  ( 3.677663764522615342, 4.135079735113118993, 26.00000000000000711 ) ) ;
#32836 = EDGE_CURVE ( 'NONE', #44658, #1276, #42516, .T. ) ;
#32837 = EDGE_CURVE ( 'NONE', #16044, #40989, #25919, .T. ) ;
#32838 = CARTESIAN_POINT ( 'NONE',  ( 5.257023737882801306, 5.242976262117200470, 54.00000000000000711 ) ) ;
#32839 = DIRECTION ( 'NONE',  ( 0.000000000000000000, 1.000000000000000000, 0.000000000000000000 ) ) ;
#32840 = CARTESIAN_POINT ( 'NONE',  ( 49.00000000000000000, -14.06939075806900163, -20.80000000000000426 ) ) ;
#32841 = VECTOR ( 'NONE', #55336, 1000.000000000000000 ) ;
#32842 = ADVANCED_FACE ( 'NONE', ( #19896 ), #3284, .F. ) ;
#32843 = CARTESIAN_POINT ( 'NONE',  ( -8.249999999999996447, -7.848062532927998269, -5.000000000000000000 ) ) ;
#32844 = AXIS2_PLACEMENT_3D ( 'NONE', #6376, #12338, #6702 ) ;
#32845 = ORIENTED_EDGE ( 'NONE', *, *, #55267, .T. ) ;
#32846 = EDGE_LOOP ( 'NONE', ( #58930, #16627 ) ) ;
#32847 = CARTESIAN_POINT ( 'NONE',  ( -8.250000000000001776, 7.250000000000000888, -21.50000000000000000 ) ) ;
#32848 = ORIENTED_EDGE ( 'NONE', *, *, #48918, .T. ) ;
#32849 = CARTESIAN_POINT ( 'NONE',  ( -11.77351654964670935, 4.393516549646602876, 455.0000000000000568 ) ) ;
#32850 = ORIENTED_EDGE ( 'NONE', *, *, #45492, .F. ) ;
#32851 = AXIS2_PLACEMENT_3D ( 'NONE', #38578, #39258, #49187 ) ;
#32852 = DIRECTION ( 'NONE',  ( 0.000000000000000000, 1.000000000000000000, 0.000000000000000000 ) ) ;
#32853 = VECTOR ( 'NONE', #47120, 1000.000000000000000 ) ;
#32854 = AXIS2_PLACEMENT_3D ( 'NONE', #64685, #59039, #27220 ) ;
#32855 = CARTESIAN_POINT ( 'NONE',  ( 6.849523737882817542, -10.50702373788281463, 26.00000000000000000 ) ) ;
#32856 = CARTESIAN_POINT ( 'NONE',  ( 73.77321854994620765, 47.95351654967443977, 0.000000000000000000 ) ) ;
#32857 = VERTEX_POINT ( 'NONE', #46412 ) ;
#32858 = VERTEX_POINT ( 'NONE', #63036 ) ;
#32860 = EDGE_CURVE ( 'NONE', #32488, #65011, #25566, .T. ) ;
#32859 = FACE_OUTER_BOUND ( 'NONE', #61082, .T. ) ;
#32861 = EDGE_LOOP ( 'NONE', ( #25458, #51465, #48288, #43974 ) ) ;
#32862 = VECTOR ( 'NONE', #50664, 1000.000000000000000 ) ;
#32863 = VERTEX_POINT ( 'NONE', #68701 ) ;
#32864 = EDGE_CURVE ( 'NONE', #42686, #55973, #41466, .T. ) ;
#32865 = DIRECTION ( 'NONE',  ( -0.7071067811865436870, 0.7071067811865514585, 0.000000000000000000 ) ) ;
#32866 = DIRECTION ( 'NONE',  ( 2.478176394252584099E-15, 1.000000000000000000, 0.000000000000000000 ) ) ;
#32867 = DIRECTION ( 'NONE',  ( 0.000000000000000000, 0.000000000000000000, 1.000000000000000000 ) ) ;
#32868 = ORIENTED_EDGE ( 'NONE', *, *, #49040, .F. ) ;
#32869 = DIRECTION ( 'NONE',  ( -1.000000000000000000, 0.000000000000000000, 0.000000000000000000 ) ) ;
#32870 = CIRCLE ( 'NONE', #12503, 0.2000000000000005107 ) ;
#32872 = LINE ( 'NONE', #13377, #614 ) ;
#32871 = CARTESIAN_POINT ( 'NONE',  ( 7.408280051175172076, -6.789561617636949542, 54.00000000000000711 ) ) ;
#32873 = ORIENTED_EDGE ( 'NONE', *, *, #31431, .T. ) ;
#32874 = EDGE_LOOP ( 'NONE', ( #9265, #34514, #27402, #61283 ) ) ;
#32876 = ORIENTED_EDGE ( 'NONE', *, *, #43622, .F. ) ;
#32875 = DIRECTION ( 'NONE',  ( 9.912705577010336396E-15, 1.000000000000000000, 0.000000000000000000 ) ) ;
#32877 = EDGE_LOOP ( 'NONE', ( #6361, #60927, #48184, #55102, #24444, #37628, #48093, #65203, #15392, #37666, #47098, #2169, #68026, #39859, #47475, #4964, #1449, #36800, #48677, #5085, #462, #21533, #55141, #51684, #46271, #68077, #18082, #33880, #6312, #600, #15948, #46135, #53687, #25769, #28179, #36543, #61276, #39268, #36050, #33116, #24140, #67516, #13839, #49841, #20961, #49135, #25485, #17521, #41321, #58359, #65058, #3654, #6614, #26231, #410, #69393, #63219, #19024, #10701, #55990, #60600, #33788, #68225, #58075, #67616, #12071, #59516, #799, #20894, #12438, #28331, #19724, #6815, #43305, #21369, #48916, #50822, #16046, #35796, #3986, #32389, #33398, #29635, #1935, #58751, #6817, #22861, #46994, #27478, #63645, #13992, #51241, #49542, #48138, #58178, #39350, #25645, #7527, #50881, #49434, #9760, #17902, #14172, #63157, #15038, #33679, #6544, #43186, #9152, #65552, #61887, #64639, #48355, #53550, #27299, #25699, #51543, #45542, #17554, #19791, #32022, #5499, #34418, #293, #56749, #35833, #49995, #54986, #66140, #60637, #33403, #14024, #29611, #23582, #58948, #13559, #20359, #7894, #11674, #1884, #60838, #40772, #1223, #39802, #37149, #39942, #15315, #38529, #26622, #32230, #32958, #45912, #22171, #44225, #5723, #29818, #31579, #241, #58335, #52031, #48375, #41846, #36433, #62016, #33694, #62667, #15659, #62621, #29899, #24838, #30497, #46085, #68172, #12259, #33343, #2306, #43924, #55808, #44560, #15575, #58975, #52976, #61268, #43544, #59220, #51044, #66762, #39925, #31937, #47233, #61938, #17649, #59393, #62055, #52927, #23706, #41572, #41489, #47576, #38677, #51780, #58688, #9726, #13912, #14213, #18412, #19355, #64305, #30842, #60012, #20522, #47943, #54370, #49242 ) ) ;
#32878 = DIRECTION ( 'NONE',  ( -0.000000000000000000, -0.000000000000000000, 1.000000000000000000 ) ) ;
#32879 = LINE ( 'NONE', #66078, #30283 ) ;
#32880 = EDGE_CURVE ( 'NONE', #42553, #56334, #12851, .T. ) ;
#32881 = AXIS2_PLACEMENT_3D ( 'NONE', #7645, #35203, #56784 ) ;
#32882 = ORIENTED_EDGE ( 'NONE', *, *, #16149, .F. ) ;
#32883 = EDGE_LOOP ( 'NONE', ( #65461, #45293, #12655, #58945 ) ) ;
#32884 = DIRECTION ( 'NONE',  ( -3.491481338843132961E-15, -1.000000000000000000, 0.000000000000000000 ) ) ;
#32885 = CARTESIAN_POINT ( 'NONE',  ( 10.09643294401454661, -2.906483450353395614, 195.0000000000000284 ) ) ;
#32886 = ORIENTED_EDGE ( 'NONE', *, *, #46551, .T. ) ;
#32887 = CARTESIAN_POINT ( 'NONE',  ( 11.19368345035335821, 11.18071654964659523, 195.0000000000000284 ) ) ;
#32888 = FACE_OUTER_BOUND ( 'NONE', #48781, .T. ) ;
#32889 = CARTESIAN_POINT ( 'NONE',  ( 106.4257688009193998, 0.000000000000000000, 289.4830310981789125 ) ) ;
#32890 = VECTOR ( 'NONE', #52116, 1000.000000000000000 ) ;
#32891 = ORIENTED_EDGE ( 'NONE', *, *, #3609, .T. ) ;
#32892 = EDGE_CURVE ( 'NONE', #47649, #14243, #15653, .T. ) ;
#32893 = VECTOR ( 'NONE', #58394, 1000.000000000000000 ) ;
#32894 = DIRECTION ( 'NONE',  ( 0.000000000000000000, -1.000000000000000000, 0.000000000000000000 ) ) ;
#32895 = DIRECTION ( 'NONE',  ( -0.000000000000000000, -0.000000000000000000, -1.000000000000000000 ) ) ;
#32897 = VERTEX_POINT ( 'NONE', #8930 ) ;
#32896 = DIRECTION ( 'NONE',  ( 8.994862468027880808E-15, 0.000000000000000000, 1.000000000000000000 ) ) ;
#32899 = ORIENTED_EDGE ( 'NONE', *, *, #68999, .F. ) ;
#32898 = CARTESIAN_POINT ( 'NONE',  ( 10.74648345035338082, -1.090483450353491035, 455.0000000000000568 ) ) ;
#32900 = EDGE_CURVE ( 'NONE', #6346, #46451, #31229, .T. ) ;
#32901 = DIRECTION ( 'NONE',  ( 0.000000000000000000, -1.000000000000000000, 0.000000000000000000 ) ) ;
#32902 = CARTESIAN_POINT ( 'NONE',  ( 3.682023737882818892, 9.897976262117202495, 54.00000000000000711 ) ) ;
#32903 = EDGE_CURVE ( 'NONE', #56261, #55138, #51730, .T. ) ;
#32904 = CARTESIAN_POINT ( 'NONE',  ( -9.722976262117288826, -6.832023737882753522, 26.00000000000000000 ) ) ;
#32905 = CARTESIAN_POINT ( 'NONE',  ( 30.00000000000000000, -17.50000000000000000, 26.64999999999999858 ) ) ;
#32906 = VECTOR ( 'NONE', #24844, 1000.000000000000000 ) ;
#32907 = DIRECTION ( 'NONE',  ( 0.7671651518153006499, 0.6414496315691565753, 0.000000000000000000 ) ) ;
#32908 = ADVANCED_FACE ( 'NONE', ( #52800 ), #69035, .F. ) ;
#32909 = EDGE_CURVE ( 'NONE', #41339, #2734, #30503, .T. ) ;
#32910 = DIRECTION ( 'NONE',  ( 1.000000000000000000, -1.260948829465469904E-14, 0.000000000000000000 ) ) ;
#32911 = ORIENTED_EDGE ( 'NONE', *, *, #43277, .T. ) ;
#32912 = DIRECTION ( 'NONE',  ( 0.000000000000000000, 0.000000000000000000, 1.000000000000000000 ) ) ;
#32913 = VECTOR ( 'NONE', #26953, 1000.000000000000000 ) ;
#32915 = EDGE_LOOP ( 'NONE', ( #13787, #61000, #9042, #37593 ) ) ;
#32914 = CARTESIAN_POINT ( 'NONE',  ( -9.293516549646817282, -10.09643294401455904, 455.0000000000000568 ) ) ;
#32917 = VERTEX_POINT ( 'NONE', #25205 ) ;
#32916 = DIRECTION ( 'NONE',  ( 0.000000000000000000, 0.000000000000000000, -1.000000000000000000 ) ) ;
#32918 = CARTESIAN_POINT ( 'NONE',  ( 8.250000000000005329, 0.000000000000000000, -8.000000000000000000 ) ) ;
#32919 = DIRECTION ( 'NONE',  ( 0.000000000000000000, -1.000000000000000000, -3.673940397442059868E-16 ) ) ;
#32920 = VERTEX_POINT ( 'NONE', #47812 ) ;
#32921 = LINE ( 'NONE', #33941, #15091 ) ;
#32922 = DIRECTION ( 'NONE',  ( -0.7071067811865470176, 0.7071067811865480168, 0.000000000000000000 ) ) ;
#32923 = ORIENTED_EDGE ( 'NONE', *, *, #63401, .F. ) ;
#32924 = CARTESIAN_POINT ( 'NONE',  ( 7.250000000000005329, -7.249999999999998224, -15.00000000000000000 ) ) ;
#32925 = CARTESIAN_POINT ( 'NONE',  ( 41.09999999999999432, 14.08845687959340331, -21.00000000000000000 ) ) ;
#32926 = PLANE ( 'NONE',  #9986 ) ;
#32927 = DIRECTION ( 'NONE',  ( 1.000000000000000000, -0.000000000000000000, 0.000000000000000000 ) ) ;
#32928 = EDGE_LOOP ( 'NONE', ( #32427, #63684, #64871, #68549 ) ) ;
#32929 = AXIS2_PLACEMENT_3D ( 'NONE', #34785, #24886, #2613 ) ;
#32930 = LINE ( 'NONE', #54167, #28257 ) ;
#32931 = VERTEX_POINT ( 'NONE', #14591 ) ;
#32932 = VERTEX_POINT ( 'NONE', #58446 ) ;
#32933 = CARTESIAN_POINT ( 'NONE',  ( 10.00000000000000000, 21.00000000000000000, -18.00000000000000355 ) ) ;
#32934 = FACE_OUTER_BOUND ( 'NONE', #39549, .T. ) ;
#32935 = DIRECTION ( 'NONE',  ( 0.000000000000000000, 0.000000000000000000, 1.000000000000000000 ) ) ;
#32936 = LINE ( 'NONE', #69740, #22752 ) ;
#32937 = ORIENTED_EDGE ( 'NONE', *, *, #11211, .F. ) ;
#32938 = VERTEX_POINT ( 'NONE', #36152 ) ;
#32939 = AXIS2_PLACEMENT_3D ( 'NONE', #65090, #69704, #48475 ) ;
#32942 = ORIENTED_EDGE ( 'NONE', *, *, #32259, .F. ) ;
#32941 = EDGE_CURVE ( 'NONE', #8558, #57661, #15300, .T. ) ;
#32940 = DIRECTION ( 'NONE',  ( 0.000000000000000000, -0.7071067811865475727, 0.7071067811865475727 ) ) ;
#32943 = ORIENTED_EDGE ( 'NONE', *, *, #60854, .F. ) ;
#32944 = PRODUCT_DEFINITION_SHAPE ( 'NONE', 'NONE',  #69986 ) ;
#32945 = EDGE_CURVE ( 'NONE', #36321, #15671, #4968, .T. ) ;
#32946 = CIRCLE ( 'NONE', #3574, 24.99999999998794920 ) ;
#32947 = LINE ( 'NONE', #44235, #41670 ) ;
#32948 = DIRECTION ( 'NONE',  ( 1.836970198721029934E-16, 1.836970198721010706E-16, -1.000000000000000000 ) ) ;
#32949 = CARTESIAN_POINT ( 'NONE',  ( 39.00000000000000000, 0.000000000000000000, 3.500000000000000000 ) ) ;
#32950 = EDGE_CURVE ( 'NONE', #14861, #29958, #65476, .T. ) ;
#32951 = SURFACE_SIDE_STYLE ('',( #17371 ) ) ;
#32953 = CARTESIAN_POINT ( 'NONE',  ( 0.000000000000000000, 8.250000000000001776, -18.50000000000000000 ) ) ;
#32952 = DIRECTION ( 'NONE',  ( -0.000000000000000000, 0.000000000000000000, 1.000000000000000000 ) ) ;
#32954 = VERTEX_POINT ( 'NONE', #10682 ) ;
#32956 = EDGE_LOOP ( 'NONE', ( #68600, #13445, #5840, #27427 ) ) ;
#32955 = LINE ( 'NONE', #59485, #65749 ) ;
#32957 = ORIENTED_EDGE ( 'NONE', *, *, #7726, .T. ) ;
#32958 = ORIENTED_EDGE ( 'NONE', *, *, #55674, .T. ) ;
#32959 = VECTOR ( 'NONE', #55200, 1000.000000000000000 ) ;
#32960 = AXIS2_PLACEMENT_3D ( 'NONE', #14500, #9195, #24400 ) ;
#32961 = CARTESIAN_POINT ( 'NONE',  ( 7.450000000000003730, -7.249999999999997335, -25.50000000000000355 ) ) ;
#32962 = CARTESIAN_POINT ( 'NONE',  ( 7.250000000000005329, 7.250000000000000888, -9.500000000000001776 ) ) ;
#32963 = AXIS2_PLACEMENT_3D ( 'NONE', #18390, #61892, #13093 ) ;
#32964 = DIRECTION ( 'NONE',  ( -1.000000000000000000, 0.000000000000000000, 0.000000000000000000 ) ) ;
#32966 = EDGE_CURVE ( 'NONE', #20506, #61285, #11710, .T. ) ;
#32965 = VERTEX_POINT ( 'NONE', #22352 ) ;
#32967 = ORIENTED_EDGE ( 'NONE', *, *, #45199, .T. ) ;
#32969 = DIRECTION ( 'NONE',  ( 1.836970198721029934E-16, 1.836970198721010706E-16, -1.000000000000000000 ) ) ;
#32968 = VECTOR ( 'NONE', #46380, 1000.000000000000000 ) ;
#32970 = DIRECTION ( 'NONE',  ( -1.836970198721029934E-16, 1.836970198721036590E-16, -1.000000000000000000 ) ) ;
#32971 = FACE_BOUND ( 'NONE', #42004, .T. ) ;
#32972 = ORIENTED_EDGE ( 'NONE', *, *, #60355, .F. ) ;
#32973 = VERTEX_POINT ( 'NONE', #17033 ) ;
#32974 = CARTESIAN_POINT ( 'NONE',  ( 2.369523737882793135, -8.835729544836320670, 54.00000000000000711 ) ) ;
#32975 = DIRECTION ( 'NONE',  ( -1.000000000000000000, 0.000000000000000000, 0.000000000000000000 ) ) ;
#32976 = ORIENTED_EDGE ( 'NONE', *, *, #56602, .T. ) ;
#32977 = ADVANCED_FACE ( 'NONE', ( #31916 ), #32254, .T. ) ;
#32978 = VECTOR ( 'NONE', #58113, 1000.000000000000000 ) ;
#32979 = CARTESIAN_POINT ( 'NONE',  ( -29.50000000000000355, -11.50000000000000000, -15.00000000000000000 ) ) ;
#32981 = ORIENTED_EDGE ( 'NONE', *, *, #2478, .F. ) ;
#32980 = CARTESIAN_POINT ( 'NONE',  ( 73.77321854994620765, 47.95351654967443977, 26.00000000000000355 ) ) ;
#32982 = EDGE_LOOP ( 'NONE', ( #11193, #54583, #62073, #59867 ) ) ;
#32983 = DIRECTION ( 'NONE',  ( -1.000000000000000000, 0.000000000000000000, 0.000000000000000000 ) ) ;
#32984 = DIRECTION ( 'NONE',  ( -1.836970198721029934E-16, 1.836970198721036344E-16, -1.000000000000000000 ) ) ;
#32985 = LINE ( 'NONE', #65184, #53253 ) ;
#32986 = EDGE_CURVE ( 'NONE', #20073, #144, #53486, .T. ) ;
#32987 = AXIS2_PLACEMENT_3D ( 'NONE', #26067, #20741, #41252 ) ;
#32988 = EDGE_CURVE ( 'NONE', #16520, #29410, #38605, .T. ) ;
#32989 = CARTESIAN_POINT ( 'NONE',  ( 15.70313394608857394, -0.2715358723588625622, 23.82609623451821079 ) ) ;
#32990 = CARTESIAN_POINT ( 'NONE',  ( 41.09999999999999432, -21.00000000000000000, 14.57806571531351914 ) ) ;
#32991 = EDGE_CURVE ( 'NONE', #25346, #57801, #54636, .T. ) ;
#32992 = ADVANCED_FACE ( 'NONE', ( #5740 ), #43204, .T. ) ;
#32993 = VECTOR ( 'NONE', #56543, 1000.000000000000000 ) ;
#32994 = ORIENTED_EDGE ( 'NONE', *, *, #29288, .F. ) ;
#32995 = CARTESIAN_POINT ( 'NONE',  ( 7.250000000000005329, -7.249999999999998224, -10.50000000000000000 ) ) ;
#32997 = ORIENTED_EDGE ( 'NONE', *, *, #57887, .F. ) ;
#32996 = DIRECTION ( 'NONE',  ( -1.000000000000000000, 0.000000000000000000, 0.000000000000000000 ) ) ;
#32998 = LINE ( 'NONE', #22397, #5008 ) ;
#32999 = DIRECTION ( 'NONE',  ( 0.000000000000000000, 0.000000000000000000, -1.000000000000000000 ) ) ;
#33000 = ADVANCED_FACE ( 'NONE', ( #16338 ), #88, .F. ) ;
#33001 = CYLINDRICAL_SURFACE ( 'NONE', #60707, 0.1749999999999998224 ) ;
#33002 = AXIS2_PLACEMENT_3D ( 'NONE', #8147, #18770, #12746 ) ;
#33003 = LINE ( 'NONE', #54580, #13721 ) ;
#33004 = DIRECTION ( 'NONE',  ( -1.000000000000000000, 1.047444401652939849E-14, 0.000000000000000000 ) ) ;
#33005 = ORIENTED_EDGE ( 'NONE', *, *, #32642, .F. ) ;
#33006 = AXIS2_PLACEMENT_3D ( 'NONE', #63910, #9462, #37046 ) ;
#33007 = ORIENTED_EDGE ( 'NONE', *, *, #37701, .T. ) ;
#33008 = CARTESIAN_POINT ( 'NONE',  ( 39.00000000000000000, -21.00000000000000000, 16.96999999999999886 ) ) ;
#33009 = LINE ( 'NONE', #12804, #53681 ) ;
#33010 = VECTOR ( 'NONE', #32530, 1000.000000000000000 ) ;
#33011 = AXIS2_PLACEMENT_3D ( 'NONE', #45165, #38831, #56147 ) ;
#33012 = ORIENTED_EDGE ( 'NONE', *, *, #65745, .T. ) ;
#33013 = DIRECTION ( 'NONE',  ( 1.000000000000000000, -1.920292680692490463E-14, 1.836970198720994435E-16 ) ) ;
#33014 = DIRECTION ( 'NONE',  ( 1.000000000000000000, -5.981805089575194965E-17, 0.000000000000000000 ) ) ;
#33015 = ORIENTED_EDGE ( 'NONE', *, *, #1675, .F. ) ;
#33016 = VECTOR ( 'NONE', #6643, 1000.000000000000000 ) ;
#33017 = CARTESIAN_POINT ( 'NONE',  ( 15.50000000000000000, -2.500000000000000000, 21.05662432702600029 ) ) ;
#33018 = DIRECTION ( 'NONE',  ( 0.000000000000000000, 1.000000000000000000, -0.000000000000000000 ) ) ;
#33019 = ORIENTED_EDGE ( 'NONE', *, *, #35866, .F. ) ;
#33020 = CARTESIAN_POINT ( 'NONE',  ( 11.32648345035337734, -4.206483450353396769, 195.0000000000000284 ) ) ;
#33021 = LINE ( 'NONE', #6148, #8607 ) ;
#33022 = CARTESIAN_POINT ( 'NONE',  ( 10.31452373788281562, -3.664523737882826815, 54.00000000000000711 ) ) ;
#33023 = CARTESIAN_POINT ( 'NONE',  ( -30.00000000000000000, -13.54524521594299991, 17.53999999999999915 ) ) ;
#33024 = ORIENTED_EDGE ( 'NONE', *, *, #10333, .F. ) ;
#33026 = ORIENTED_EDGE ( 'NONE', *, *, #47677, .F. ) ;
#33025 = CARTESIAN_POINT ( 'NONE',  ( 275.0000000000000000, -39.80000000000000426, -8.400000000000000355 ) ) ;
#33027 = CARTESIAN_POINT ( 'NONE',  ( -7.250000000000000000, -7.449999999999998401, -9.500000000000001776 ) ) ;
#33028 = FACE_OUTER_BOUND ( 'NONE', #46326, .T. ) ;
#33029 = DIRECTION ( 'NONE',  ( -1.000000000000000000, 0.000000000000000000, 0.000000000000000000 ) ) ;
#33030 = ORIENTED_EDGE ( 'NONE', *, *, #42189, .T. ) ;
#33031 = EDGE_CURVE ( 'NONE', #14864, #50893, #59478, .T. ) ;
#33032 = EDGE_CURVE ( 'NONE', #67047, #33736, #5034, .T. ) ;
#33033 = FACE_OUTER_BOUND ( 'NONE', #2537, .T. ) ;
#33034 = VECTOR ( 'NONE', #49378, 1000.000000000000000 ) ;
#33035 = ORIENTED_EDGE ( 'NONE', *, *, #45661, .T. ) ;
#33036 = ORIENTED_EDGE ( 'NONE', *, *, #37493, .F. ) ;
#33037 = EDGE_CURVE ( 'NONE', #47485, #31671, #20749, .T. ) ;
#33038 = EDGE_LOOP ( 'NONE', ( #34104, #43633, #4252, #61029 ) ) ;
#33039 = DIRECTION ( 'NONE',  ( 0.000000000000000000, -0.7084617869623469621, 0.7057491738671168857 ) ) ;
#33040 = CIRCLE ( 'NONE', #8186, 24.99999999998794920 ) ;
#33041 = DIRECTION ( 'NONE',  ( -1.000000000000000000, 0.000000000000000000, 0.000000000000000000 ) ) ;
#33042 = CARTESIAN_POINT ( 'NONE',  ( 29.89999999999999858, 0.000000000000000000, 2.458500000000000796 ) ) ;
#33043 = SHAPE_REPRESENTATION_RELATIONSHIP ( 'NONE' , 'NONE' ,  #53035, #44431 ) ;
#33044 = ORIENTED_EDGE ( 'NONE', *, *, #42272, .F. ) ;
#33045 = ORIENTED_EDGE ( 'NONE', *, *, #4491, .T. ) ;
#33046 = VERTEX_POINT ( 'NONE', #59128 ) ;
#33047 = CARTESIAN_POINT ( 'NONE',  ( 10.31452373788278187, 3.650476262117146042, 54.00000000000000711 ) ) ;
#33048 = EDGE_LOOP ( 'NONE', ( #53562, #48384, #29037, #44353, #11306, #7693, #3311, #63736 ) ) ;
#33049 = ORIENTED_EDGE ( 'NONE', *, *, #52684, .T. ) ;
#33050 = VERTEX_POINT ( 'NONE', #49219 ) ;
#33051 = VERTEX_POINT ( 'NONE', #21302 ) ;
#33052 = DIRECTION ( 'NONE',  ( -0.5773502691896257311, -0.5773502691896257311, -0.5773502691896257311 ) ) ;
#33053 = UNCERTAINTY_MEASURE_WITH_UNIT (LENGTH_MEASURE( 1.000000000000000082E-05 ), #41824, 'distance_accuracy_value', 'NONE');
#33055 = ORIENTED_EDGE ( 'NONE', *, *, #65699, .F. ) ;
#33054 = CARTESIAN_POINT ( 'NONE',  ( 50.00000000000000000, 0.000000000000000000, 0.000000000000000000 ) ) ;
#33056 = DIRECTION ( 'NONE',  ( 1.000000000000000000, -2.312964634635741083E-15, 5.349805401075652267E-30 ) ) ;
#33057 = SHAPE_REPRESENTATION ( 'BR-Y-111', ( #23359, #22265, #5322, #12094, #64077, #48258, #3072, #61756, #51628, #32408, #25652, #21155, #31316 ), #17754 ) ;
#33059 = CARTESIAN_POINT ( 'NONE',  ( 17.00000000000000000, -17.50000000000000000, -19.33772233983200195 ) ) ;
#33058 = AXIS2_PLACEMENT_3D ( 'NONE', #7176, #6519, #28751 ) ;
#33060 = CARTESIAN_POINT ( 'NONE',  ( 49.00000000000000000, -0.7500000000000000000, -4.943429983321300014 ) ) ;
#33061 = ORIENTED_EDGE ( 'NONE', *, *, #21613, .F. ) ;
#33062 = VECTOR ( 'NONE', #17869, 1000.000000000000000 ) ;
#33063 = AXIS2_PLACEMENT_3D ( 'NONE', #66734, #11599, #38827 ) ;
#33064 = DIRECTION ( 'NONE',  ( 0.000000000000000000, 0.000000000000000000, -1.000000000000000000 ) ) ;
#33065 = VECTOR ( 'NONE', #39577, 1000.000000000000000 ) ;
#33066 = EDGE_CURVE ( 'NONE', #59339, #52255, #44446, .T. ) ;
#33067 = ORIENTED_EDGE ( 'NONE', *, *, #8643, .T. ) ;
#33068 = DIRECTION ( 'NONE',  ( -0.000000000000000000, -0.000000000000000000, 1.000000000000000000 ) ) ;
#33069 = ADVANCED_FACE ( 'NONE', ( #64438 ), #49555, .T. ) ;
#33070 = FACE_OUTER_BOUND ( 'NONE', #3215, .T. ) ;
#33071 = CARTESIAN_POINT ( 'NONE',  ( -24.00000000000000000, -17.50000000000000000, 19.33772233983200195 ) ) ;
#33072 = DIRECTION ( 'NONE',  ( 1.836970198721029934E-16, -1.836970198721036344E-16, 1.000000000000000000 ) ) ;
#33073 = ADVANCED_FACE ( 'NONE', ( #15997 ), #43897, .F. ) ;
#33074 = EDGE_CURVE ( 'NONE', #50086, #27584, #45563, .T. ) ;
#33075 = ORIENTED_EDGE ( 'NONE', *, *, #3051, .T. ) ;
#33076 = DIRECTION ( 'NONE',  ( -1.000000000000000000, 0.000000000000000000, 0.000000000000000000 ) ) ;
#33077 = DIRECTION ( 'NONE',  ( -1.000000000000000000, 0.000000000000000000, 0.000000000000000000 ) ) ;
#33078 = CARTESIAN_POINT ( 'NONE',  ( -6.835476262117260227, 10.49297626211718359, 26.00000000000000711 ) ) ;
#33079 = PRODUCT_RELATED_PRODUCT_CATEGORY ( 'part', '', ( #6975 ) ) ;
#33080 = FACE_OUTER_BOUND ( 'NONE', #8796, .T. ) ;
#33081 = EDGE_CURVE ( 'NONE', #13295, #3338, #32064, .T. ) ;
#33082 = DIRECTION ( 'NONE',  ( 0.000000000000000000, 0.000000000000000000, -1.000000000000000000 ) ) ;
#33083 = CARTESIAN_POINT ( 'NONE',  ( 10.50702373788280219, 6.835476262117187396, 26.00000000000000711 ) ) ;
#33084 = VECTOR ( 'NONE', #45411, 1000.000000000000000 ) ;
#33086 = ADVANCED_FACE ( 'NONE', ( #35012 ), #39960, .F. ) ;
#33085 = LINE ( 'NONE', #54660, #61511 ) ;
#33087 = FACE_OUTER_BOUND ( 'NONE', #60724, .T. ) ;
#33088 = ORIENTED_EDGE ( 'NONE', *, *, #56094, .T. ) ;
#33089 = LINE ( 'NONE', #16832, #32713 ) ;
#33090 = CARTESIAN_POINT ( 'NONE',  ( 7.250000000000005329, -7.449999999999998401, -24.00000000000000000 ) ) ;
#33091 = VECTOR ( 'NONE', #55482, 1000.000000000000000 ) ;
#33092 = CARTESIAN_POINT ( 'NONE',  ( 282.8893988437589542, -20.72883876573683182, -17.22883876573683182 ) ) ;
#33093 = DIRECTION ( 'NONE',  ( 0.000000000000000000, -1.000000000000000000, 0.000000000000000000 ) ) ;
#33094 = EDGE_LOOP ( 'NONE', ( #62057, #37563, #52176, #46092 ) ) ;
#33095 = CARTESIAN_POINT ( 'NONE',  ( 9.795823737882804139, 9.781776262117173104, 54.00000000000000711 ) ) ;
#33096 = CARTESIAN_POINT ( 'NONE',  ( 11.00000000000000000, -5.599999999999379696, 26.60000000000059828 ) ) ;
#33097 = DIRECTION ( 'NONE',  ( 0.000000000000000000, 1.000000000000000000, 0.000000000000000000 ) ) ;
#33098 = DIRECTION ( 'NONE',  ( -0.7071067811865300312, 8.659560562355147330E-17, -0.7071067811865650032 ) ) ;
#33099 = CARTESIAN_POINT ( 'NONE',  ( 3.682023737882786918, -9.737023737882800845, 26.00000000000000000 ) ) ;
#33100 = ORIENTED_EDGE ( 'NONE', *, *, #41238, .F. ) ;
#33101 = AXIS2_PLACEMENT_3D ( 'NONE', #89, #49221, #32255 ) ;
#33102 = VERTEX_POINT ( 'NONE', #55210 ) ;
#33103 = CARTESIAN_POINT ( 'NONE',  ( -11.00000000000000000, -9.454754784057099570, -17.53999999999999915 ) ) ;
#33104 = LINE ( 'NONE', #69895, #9739 ) ;
#33105 = VERTEX_POINT ( 'NONE', #39284 ) ;
#33106 = VECTOR ( 'NONE', #3704, 1000.000000000000000 ) ;
#33107 = VECTOR ( 'NONE', #37721, 1000.000000000000000 ) ;
#33108 = FACE_OUTER_BOUND ( 'NONE', #13687, .T. ) ;
#33109 = ORIENTED_EDGE ( 'NONE', *, *, #53761, .F. ) ;
#33110 = EDGE_CURVE ( 'NONE', #43306, #15138, #61527, .T. ) ;
#33111 = CARTESIAN_POINT ( 'NONE',  ( -10.91351654964670637, 2.693516549646604030, 455.0000000000000568 ) ) ;
#33112 = ORIENTED_EDGE ( 'NONE', *, *, #8750, .T. ) ;
#33113 = CIRCLE ( 'NONE', #35371, 0.1999999999999987899 ) ;
#33114 = EDGE_LOOP ( 'NONE', ( #25116, #1612, #66952, #29563 ) ) ;
#33115 = CARTESIAN_POINT ( 'NONE',  ( 30.00000000000000000, -11.85423089348099879, -9.852125413066602277 ) ) ;
#33116 = ORIENTED_EDGE ( 'NONE', *, *, #60529, .T. ) ;
#33117 = CARTESIAN_POINT ( 'NONE',  ( 283.0000000000000568, -25.50000000000000355, -17.00000000000000000 ) ) ;
#33118 = DIRECTION ( 'NONE',  ( 0.000000000000000000, 1.000000000000000000, 0.000000000000000000 ) ) ;
#33119 = DIRECTION ( 'NONE',  ( -0.000000000000000000, 3.673940397442059868E-16, -1.000000000000000000 ) ) ;
#33120 = ORIENTED_EDGE ( 'NONE', *, *, #38584, .F. ) ;
#33121 = EDGE_LOOP ( 'NONE', ( #29583, #51039, #61203, #51105 ) ) ;
#33122 = FACE_OUTER_BOUND ( 'NONE', #56038, .T. ) ;
#33123 = DIRECTION ( 'NONE',  ( 0.000000000000000000, 0.000000000000000000, -1.000000000000000000 ) ) ;
#33124 = EDGE_CURVE ( 'NONE', #25912, #31241, #10611, .T. ) ;
#33125 = ORIENTED_EDGE ( 'NONE', *, *, #51835, .T. ) ;
#33126 = AXIS2_PLACEMENT_3D ( 'NONE', #16327, #37903, #59465 ) ;
#33127 = ORIENTED_EDGE ( 'NONE', *, *, #10257, .F. ) ;
#33128 = EDGE_LOOP ( 'NONE', ( #3727, #1584, #15698, #59423 ) ) ;
#33129 = EDGE_CURVE ( 'NONE', #60174, #13060, #13454, .T. ) ;
#33130 = DIRECTION ( 'NONE',  ( 0.000000000000000000, -0.7071067811865455743, -0.7071067811865495711 ) ) ;
#33131 = VECTOR ( 'NONE', #27526, 1000.000000000000000 ) ;
#33133 = VERTEX_POINT ( 'NONE', #66157 ) ;
#33132 = CARTESIAN_POINT ( 'NONE',  ( 106.4257688009193998, 0.000000000000000000, 285.9830310981789125 ) ) ;
#33134 = LINE ( 'NONE', #65993, #57082 ) ;
#33135 = FACE_OUTER_BOUND ( 'NONE', #28380, .T. ) ;
#33136 = ORIENTED_EDGE ( 'NONE', *, *, #44329, .F. ) ;
#33137 = ORIENTED_EDGE ( 'NONE', *, *, #17237, .F. ) ;
#33138 = EDGE_CURVE ( 'NONE', #30841, #3133, #45270, .T. ) ;
#33139 = ORIENTED_EDGE ( 'NONE', *, *, #38536, .F. ) ;
#33140 = FACE_BOUND ( 'NONE', #46910, .T. ) ;
#33141 = PLANE ( 'NONE',  #16631 ) ;
#33142 = VERTEX_POINT ( 'NONE', #66843 ) ;
#33143 = AXIS2_PLACEMENT_3D ( 'NONE', #43871, #33610, #17006 ) ;
#33144 = AXIS2_PLACEMENT_3D ( 'NONE', #43030, #33470, #28159 ) ;
#33145 = CARTESIAN_POINT ( 'NONE',  ( 7.250000000000005329, 7.250000000000000888, -26.00000000000001066 ) ) ;
#33146 = EDGE_CURVE ( 'NONE', #37986, #25888, #3844, .T. ) ;
#33147 = EDGE_CURVE ( 'NONE', #66290, #13668, #29024, .T. ) ;
#33149 = VERTEX_POINT ( 'NONE', #13099 ) ;
#33148 = LINE ( 'NONE', #17918, #42150 ) ;
#33150 = VERTEX_POINT ( 'NONE', #28671 ) ;
#33152 = CARTESIAN_POINT ( 'NONE',  ( 283.0000000000000568, -26.28355339059299922, -9.766446609406699508 ) ) ;
#33151 = AXIS2_PLACEMENT_3D ( 'NONE', #16591, #38166, #53383 ) ;
#33153 = AXIS2_PLACEMENT_3D ( 'NONE', #47549, #52874, #31308 ) ;
#33155 = AXIS2_PLACEMENT_3D ( 'NONE', #45373, #41124, #57037 ) ;
#33154 = FACE_OUTER_BOUND ( 'NONE', #26638, .T. ) ;
#33156 = EDGE_CURVE ( 'NONE', #6256, #13195, #50930, .T. ) ;
#33157 = CARTESIAN_POINT ( 'NONE',  ( 29.50000000000000355, -12.00000000000000000, 11.03137303340310282 ) ) ;
#33158 = DIRECTION ( 'NONE',  ( 0.000000000000000000, 0.000000000000000000, 1.000000000000000000 ) ) ;
#33159 = VECTOR ( 'NONE', #37434, 1000.000000000000114 ) ;
#33160 = AXIS2_PLACEMENT_3D ( 'NONE', #18480, #40042, #34751 ) ;
#33161 = CIRCLE ( 'NONE', #67024, 3.500000000000000444 ) ;
#33162 = CARTESIAN_POINT ( 'NONE',  ( 49.00000000000000000, -0.2000000000089119934, 8.909539772616881237E-12 ) ) ;
#33163 = EDGE_CURVE ( 'NONE', #17506, #2261, #17724, .T. ) ;
#33164 = ORIENTED_EDGE ( 'NONE', *, *, #2282, .F. ) ;
#33165 = CARTESIAN_POINT ( 'NONE',  ( 11.12648345035337982, -7.806483450353490561, 455.0000000000000568 ) ) ;
#33166 = FACE_OUTER_BOUND ( 'NONE', #12580, .T. ) ;
#33168 = EDGE_CURVE ( 'NONE', #191, #28622, #12394, .T. ) ;
#33167 = CARTESIAN_POINT ( 'NONE',  ( -3.667976262117228714, 9.722976262117169810, 54.00000000000000711 ) ) ;
#33169 = LINE ( 'NONE', #39167, #40092 ) ;
#33170 = CYLINDRICAL_SURFACE ( 'NONE', #8703, 2.204799999999997429 ) ;
#33171 = CYLINDRICAL_SURFACE ( 'NONE', #3281, 0.2000000000000005107 ) ;
#33172 = DIRECTION ( 'NONE',  ( -1.000000000000000000, 0.000000000000000000, 0.000000000000000000 ) ) ;
#33173 = CARTESIAN_POINT ( 'NONE',  ( 9.737023737882765317, 2.530476262117151709, 54.00000000000000711 ) ) ;
#33174 = ORIENTED_EDGE ( 'NONE', *, *, #4507, .T. ) ;
#33175 = FACE_OUTER_BOUND ( 'NONE', #46755, .T. ) ;
#33176 = CARTESIAN_POINT ( 'NONE',  ( 25.50000000000000355, -15.12100000000000044, 24.12099999999999511 ) ) ;
#33177 = EDGE_CURVE ( 'NONE', #23727, #24032, #67197, .T. ) ;
#33178 = ORIENTED_EDGE ( 'NONE', *, *, #48561, .T. ) ;
#33179 = CARTESIAN_POINT ( 'NONE',  ( 181.4833316329832940, 9.000000000000001776, 320.8239988703753056 ) ) ;
#33180 = DIRECTION ( 'NONE',  ( -2.135044278125299371E-15, 1.000000000000000000, -0.000000000000000000 ) ) ;
#33181 = CYLINDRICAL_SURFACE ( 'NONE', #33250, 0.5250000000000011324 ) ;
#33182 = CARTESIAN_POINT ( 'NONE',  ( -7.450000000000001954, -7.249999999999998224, -24.00000000000000000 ) ) ;
#33183 = DIRECTION ( 'NONE',  ( 1.000000000000000000, -0.000000000000000000, 0.000000000000000000 ) ) ;
#33184 = DIRECTION ( 'NONE',  ( -0.7071067811865446862, -0.7071067811865503483, -0.000000000000000000 ) ) ;
#33185 = VERTEX_POINT ( 'NONE', #2493 ) ;
#33186 = DIRECTION ( 'NONE',  ( 0.7071067811865435759, -0.7071067811865515695, -2.597868168706494402E-16 ) ) ;
#33187 = DIRECTION ( 'NONE',  ( 1.000000000000000000, -0.000000000000000000, -0.000000000000000000 ) ) ;
#33188 = ORIENTED_EDGE ( 'NONE', *, *, #31972, .T. ) ;
#33189 = CIRCLE ( 'NONE', #36625, 0.5250000000000003553 ) ;
#33190 = CARTESIAN_POINT ( 'NONE',  ( 17.51999999999999957, -15.50000000000000000, 26.00000000000000355 ) ) ;
#33191 = ADVANCED_FACE ( 'NONE', ( #23376 ), #28323, .F. ) ;
#33192 = CARTESIAN_POINT ( 'NONE',  ( -7.250000000000000000, -7.449999999999998401, -14.50000000000000000 ) ) ;
#33193 = LINE ( 'NONE', #33539, #42325 ) ;
#33194 = ORIENTED_EDGE ( 'NONE', *, *, #60892, .T. ) ;
#33195 =( REPRESENTATION_RELATIONSHIP ('NONE','NONE', #33057, #1995 ) REPRESENTATION_RELATIONSHIP_WITH_TRANSFORMATION ( #4879 )SHAPE_REPRESENTATION_RELATIONSHIP( ) );
#33196 = ORIENTED_EDGE ( 'NONE', *, *, #15197, .F. ) ;
#33197 = FACE_OUTER_BOUND ( 'NONE', #8285, .T. ) ;
#33198 = ORIENTED_EDGE ( 'NONE', *, *, #52974, .T. ) ;
#33199 = ADVANCED_FACE ( 'NONE', ( #12059 ), #66498, .F. ) ;
#33200 = ORIENTED_EDGE ( 'NONE', *, *, #20865, .T. ) ;
#33201 = PRODUCT_DEFINITION_CONTEXT ( 'detailed design', #49005, 'design' ) ;
#33202 = FACE_OUTER_BOUND ( 'NONE', #67415, .T. ) ;
#33203 = DIRECTION ( 'NONE',  ( 0.000000000000000000, 0.000000000000000000, -1.000000000000000000 ) ) ;
#33204 = AXIS2_PLACEMENT_3D ( 'NONE', #7323, #56818, #3094 ) ;
#33205 = VECTOR ( 'NONE', #2594, 1000.000000000000000 ) ;
#33206 = DIRECTION ( 'NONE',  ( -1.836970198721029934E-16, -1.836970198721010706E-16, 1.000000000000000000 ) ) ;
#33207 = ORIENTED_EDGE ( 'NONE', *, *, #52228, .T. ) ;
#33208 = EDGE_CURVE ( 'NONE', #10507, #44658, #37770, .T. ) ;
#33209 = CARTESIAN_POINT ( 'NONE',  ( -11.00000000000000000, -5.200000000000001066, -9.400000000000000355 ) ) ;
#33211 = DIRECTION ( 'NONE',  ( 1.836970198721029934E-16, 1.836970198721010706E-16, -1.000000000000000000 ) ) ;
#33210 = DIRECTION ( 'NONE',  ( 1.000000000000000000, 0.000000000000000000, 0.000000000000000000 ) ) ;
#33212 = ORIENTED_EDGE ( 'NONE', *, *, #67721, .T. ) ;
#33213 = CIRCLE ( 'NONE', #2705, 0.2000000000000005107 ) ;
#33215 = EDGE_LOOP ( 'NONE', ( #24889, #33903, #68071, #63206 ) ) ;
#33214 = VECTOR ( 'NONE', #27772, 1000.000000000000000 ) ;
#33217 = ORIENTED_EDGE ( 'NONE', *, *, #27090, .T. ) ;
#33216 = CARTESIAN_POINT ( 'NONE',  ( 8.580623737882818958, -8.930623737882845248, 26.00000000000000000 ) ) ;
#33218 = VERTEX_POINT ( 'NONE', #50594 ) ;
#33219 = AXIS2_PLACEMENT_3D ( 'NONE', #53403, #43119, #48090 ) ;
#33220 = EDGE_CURVE ( 'NONE', #42042, #22300, #35472, .T. ) ;
#33221 = CARTESIAN_POINT ( 'NONE',  ( 0.000000000000000000, 0.000000000000000000, -3.233000000000000096 ) ) ;
#33222 = DIRECTION ( 'NONE',  ( -0.000000000000000000, -0.000000000000000000, -1.000000000000000000 ) ) ;
#33223 = ORIENTED_EDGE ( 'NONE', *, *, #29943, .T. ) ;
#33224 = EDGE_CURVE ( 'NONE', #34394, #58172, #23713, .T. ) ;
#33225 = VERTEX_POINT ( 'NONE', #45619 ) ;
#33227 = ADVANCED_FACE ( 'NONE', ( #47039 ), #58365, .T. ) ;
#33226 = VECTOR ( 'NONE', #57381, 1000.000000000000000 ) ;
#33228 = LINE ( 'NONE', #56525, #35770 ) ;
#33229 = CARTESIAN_POINT ( 'NONE',  ( 41.09999999999999432, 13.66939075806899950, -20.80000000000000426 ) ) ;
#33230 = EDGE_CURVE ( 'NONE', #52237, #38194, #29828, .T. ) ;
#33231 = ADVANCED_FACE ( 'NONE', ( #57993 ), #19456, .F. ) ;
#33232 = ADVANCED_FACE ( 'NONE', ( #62238 ), #52713, .F. ) ;
#33233 = ORIENTED_EDGE ( 'NONE', *, *, #20366, .T. ) ;
#33234 = DIRECTION ( 'NONE',  ( -1.836970198721029934E-16, -1.836970198721010706E-16, 1.000000000000000000 ) ) ;
#33235 = DIRECTION ( 'NONE',  ( -1.000000000000000000, 0.000000000000000000, 0.000000000000000000 ) ) ;
#33236 = CARTESIAN_POINT ( 'NONE',  ( 15.50000000000000000, -1.037157890325000054, -26.00000000000000000 ) ) ;
#33237 = ORIENTED_EDGE ( 'NONE', *, *, #44466, .F. ) ;
#33238 = EDGE_CURVE ( 'NONE', #35699, #3732, #9923, .T. ) ;
#33239 = CARTESIAN_POINT ( 'NONE',  ( 25.90000000000000213, -0.1999999999911430404, -8.864436962241481021E-12 ) ) ;
#33240 = ADVANCED_FACE ( 'NONE', ( #24772 ), #10663, .F. ) ;
#33241 = DIRECTION ( 'NONE',  ( 0.000000000000000000, 3.673940397442059868E-16, -1.000000000000000000 ) ) ;
#33242 = CIRCLE ( 'NONE', #58128, 6.000000000000005329 ) ;
#33244 = ORIENTED_EDGE ( 'NONE', *, *, #47002, .F. ) ;
#33243 = DIRECTION ( 'NONE',  ( 1.000000000000000000, -0.000000000000000000, -0.000000000000000000 ) ) ;
#33246 = EDGE_LOOP ( 'NONE', ( #20907, #27252, #65299, #52030, #46251, #19719 ) ) ;
#33245 = DIRECTION ( 'NONE',  ( 1.000000000000000000, 0.000000000000000000, 0.000000000000000000 ) ) ;
#33247 = EDGE_CURVE ( 'NONE', #29049, #39153, #46273, .T. ) ;
#33248 = DIRECTION ( 'NONE',  ( -0.7671651518153065341, -0.6414496315691495809, -2.356647714346224881E-16 ) ) ;
#33249 = DIRECTION ( 'NONE',  ( -1.000000000000000000, 0.000000000000000000, 0.000000000000000000 ) ) ;
#33250 = AXIS2_PLACEMENT_3D ( 'NONE', #27883, #22579, #17261 ) ;
#33251 = CARTESIAN_POINT ( 'NONE',  ( -16.75000000000000355, -0.2715193793361450614, -22.98718409945082541 ) ) ;
#33252 = DIRECTION ( 'NONE',  ( -0.000000000000000000, -0.000000000000000000, -1.000000000000000000 ) ) ;
#33253 = DIRECTION ( 'NONE',  ( 1.000000000000000000, -0.000000000000000000, 0.000000000000000000 ) ) ;
#33254 = CARTESIAN_POINT ( 'NONE',  ( 181.4833316329832940, 9.000000000000001776, 276.7801873289890295 ) ) ;
#33255 = EDGE_CURVE ( 'NONE', #361, #53834, #25121, .T. ) ;
#33256 = EDGE_LOOP ( 'NONE', ( #4012, #20753 ) ) ;
#33257 = CYLINDRICAL_SURFACE ( 'NONE', #32703, 1.224999999999997868 ) ;
#33260 = ORIENTED_EDGE ( 'NONE', *, *, #48709, .F. ) ;
#33259 = EDGE_CURVE ( 'NONE', #53470, #18955, #52461, .T. ) ;
#33258 = LINE ( 'NONE', #49520, #2879 ) ;
#33262 = ORIENTED_EDGE ( 'NONE', *, *, #30201, .F. ) ;
#33261 = DIRECTION ( 'NONE',  ( 0.000000000000000000, 3.673940397442059868E-16, -1.000000000000000000 ) ) ;
#33263 = AXIS2_PLACEMENT_3D ( 'NONE', #31383, #35592, #8740 ) ;
#33264 = AXIS2_PLACEMENT_3D ( 'NONE', #29727, #3570, #68970 ) ;
#33265 = CYLINDRICAL_SURFACE ( 'NONE', #55009, 0.8128000000000145109 ) ;
#33266 = CARTESIAN_POINT ( 'NONE',  ( 11.75000000000000000, -5.200000000000001066, 60.00000000000000000 ) ) ;
#33267 = AXIS2_PLACEMENT_3D ( 'NONE', #33286, #11700, #26949 ) ;
#33268 = AXIS2_PLACEMENT_3D ( 'NONE', #47866, #5453, #54575 ) ;
#33269 = ORIENTED_EDGE ( 'NONE', *, *, #356, .F. ) ;
#33270 = LINE ( 'NONE', #54500, #19573 ) ;
#33271 = CARTESIAN_POINT ( 'NONE',  ( -8.250000000000001776, -7.249999999999998224, -26.00000000000001066 ) ) ;
#33272 = EDGE_LOOP ( 'NONE', ( #54553, #23189, #7032, #54433 ) ) ;
#33273 = CARTESIAN_POINT ( 'NONE',  ( -3.593516549646762481, -4.622483450353452206, 455.0000000000000568 ) ) ;
#33274 = CARTESIAN_POINT ( 'NONE',  ( 39.00000000000000000, -21.00000000000000000, -16.96999999999999886 ) ) ;
#33275 = AXIS2_PLACEMENT_3D ( 'NONE', #37056, #54619, #58617 ) ;
#33276 = FACE_OUTER_BOUND ( 'NONE', #5432, .T. ) ;
#33277 = FACE_OUTER_BOUND ( 'NONE', #15494, .T. ) ;
#33278 = PLANE ( 'NONE',  #52294 ) ;
#33279 = ORIENTED_EDGE ( 'NONE', *, *, #35976, .T. ) ;
#33280 = CARTESIAN_POINT ( 'NONE',  ( 11.50000000000000000, -11.50000000000100009, -15.00000000000084910 ) ) ;
#33281 = VERTEX_POINT ( 'NONE', #20168 ) ;
#33282 = ORIENTED_EDGE ( 'NONE', *, *, #28704, .T. ) ;
#33283 = AXIS2_PLACEMENT_3D ( 'NONE', #37835, #703, #43825 ) ;
#33284 = DIRECTION ( 'NONE',  ( -1.000000000000000000, 0.000000000000000000, 0.000000000000000000 ) ) ;
#33285 = DIRECTION ( 'NONE',  ( 0.000000000000000000, 0.000000000000000000, 1.000000000000000000 ) ) ;
#33286 = CARTESIAN_POINT ( 'NONE',  ( 7.250000000000005329, -7.249999999999998224, -24.50000000000000000 ) ) ;
#33287 = DIRECTION ( 'NONE',  ( -1.000000000000000000, 1.130039751537441866E-14, 0.000000000000000000 ) ) ;
#33288 = VERTEX_POINT ( 'NONE', #9564 ) ;
#33289 = ORIENTED_EDGE ( 'NONE', *, *, #51342, .T. ) ;
#33291 = ORIENTED_EDGE ( 'NONE', *, *, #32110, .T. ) ;
#33290 = CARTESIAN_POINT ( 'NONE',  ( 11.00000000000000000, -11.50000000000000000, 15.00000000000000000 ) ) ;
#33292 = ORIENTED_EDGE ( 'NONE', *, *, #45682, .F. ) ;
#33293 = EDGE_CURVE ( 'NONE', #5400, #52304, #68615, .T. ) ;
#33294 = FACE_OUTER_BOUND ( 'NONE', #53920, .T. ) ;
#33295 = CARTESIAN_POINT ( 'NONE',  ( 8.250000000000005329, -8.249999999999998224, -26.00000000000001066 ) ) ;
#33296 = PLANE ( 'NONE',  #27456 ) ;
#33297 = EDGE_CURVE ( 'NONE', #44963, #50749, #63664, .T. ) ;
#33298 = DIRECTION ( 'NONE',  ( 0.000000000000000000, 0.000000000000000000, 1.000000000000000000 ) ) ;
#33300 = LINE ( 'NONE', #49560, #10849 ) ;
#33299 = CARTESIAN_POINT ( 'NONE',  ( -7.813516549646711162, 11.77351654964660277, 455.0000000000000568 ) ) ;
#33301 = ORIENTED_EDGE ( 'NONE', *, *, #24406, .T. ) ;
#33302 = EDGE_CURVE ( 'NONE', #67901, #4292, #53059, .T. ) ;
#33304 = ORIENTED_EDGE ( 'NONE', *, *, #59592, .T. ) ;
#33303 = DIRECTION ( 'NONE',  ( 0.000000000000000000, 0.000000000000000000, 1.000000000000000000 ) ) ;
#33305 = AXIS2_PLACEMENT_3D ( 'NONE', #2044, #66733, #2731 ) ;
#33306 = VERTEX_POINT ( 'NONE', #41019 ) ;
#33307 = ORIENTED_EDGE ( 'NONE', *, *, #60427, .T. ) ;
#33308 = DIRECTION ( 'NONE',  ( -1.836970198721029934E-16, 1.836970198721036344E-16, -1.000000000000000000 ) ) ;
#33309 = EDGE_CURVE ( 'NONE', #2756, #21626, #68957, .T. ) ;
#33310 = DIRECTION ( 'NONE',  ( 0.000000000000000000, 0.000000000000000000, -1.000000000000000000 ) ) ;
#33311 = CIRCLE ( 'NONE', #1693, 2.500000000000000000 ) ;
#33313 = DIRECTION ( 'NONE',  ( 1.000000000000000000, -0.000000000000000000, 0.000000000000000000 ) ) ;
#33312 = VECTOR ( 'NONE', #8416, 1000.000000000000000 ) ;
#33314 = CARTESIAN_POINT ( 'NONE',  ( -7.250000000000001776, -7.249999999999998224, -18.00000000000000000 ) ) ;
#33315 = ORIENTED_EDGE ( 'NONE', *, *, #48728, .F. ) ;
#33316 = VERTEX_POINT ( 'NONE', #3207 ) ;
#33317 = CIRCLE ( 'NONE', #5109, 0.5000000000009406920 ) ;
#33318 = CARTESIAN_POINT ( 'NONE',  ( -9.093516549646711411, 10.91351654964659978, 455.0000000000000568 ) ) ;
#33319 = CARTESIAN_POINT ( 'NONE',  ( -9.547976262117256141, 2.530476262117183683, 54.00000000000000711 ) ) ;
#33320 = EDGE_LOOP ( 'NONE', ( #37943, #12901, #66921, #53062 ) ) ;
#33321 = ADVANCED_FACE ( 'NONE', ( #51649 ), #31137, .T. ) ;
#33322 = ORIENTED_EDGE ( 'NONE', *, *, #64318, .T. ) ;
#33323 = DIRECTION ( 'NONE',  ( 1.000000000000000000, -5.981805089575196197E-17, 0.000000000000000000 ) ) ;
#33324 = CIRCLE ( 'NONE', #52556, 2.000000000000001776 ) ;
#33325 = CARTESIAN_POINT ( 'NONE',  ( 49.00000000000000000, -0.7500000000000000000, -3.929058411375430104 ) ) ;
#33326 = VERTEX_POINT ( 'NONE', #19798 ) ;
#33327 = CIRCLE ( 'NONE', #51383, 0.7499999999999997780 ) ;
#33328 = LINE ( 'NONE', #49251, #49417 ) ;
#33329 = AXIS2_PLACEMENT_3D ( 'NONE', #12429, #55586, #27682 ) ;
#33331 = VERTEX_POINT ( 'NONE', #20513 ) ;
#33330 = DIRECTION ( 'NONE',  ( -1.000000000000000000, 0.000000000000000000, 0.000000000000000000 ) ) ;
#33332 = AXIS2_PLACEMENT_3D ( 'NONE', #40728, #18102, #8189 ) ;
#33333 = ORIENTED_EDGE ( 'NONE', *, *, #58509, .T. ) ;
#33334 = LINE ( 'NONE', #44271, #64885 ) ;
#33335 = CARTESIAN_POINT ( 'NONE',  ( -11.11351654964670743, 9.093516549646603053, 455.0000000000000568 ) ) ;
#33336 = LINE ( 'NONE', #58830, #3571 ) ;
#33337 = CARTESIAN_POINT ( 'NONE',  ( -7.798499376344067535, 4.727349090213368576, 455.0000000000000568 ) ) ;
#33338 = DIRECTION ( 'NONE',  ( -0.000000000000000000, -0.000000000000000000, -1.000000000000000000 ) ) ;
#33339 = EDGE_CURVE ( 'NONE', #60888, #15307, #47386, .T. ) ;
#33340 = ORIENTED_EDGE ( 'NONE', *, *, #25163, .T. ) ;
#33341 = DIRECTION ( 'NONE',  ( -0.5000000000000004441, 0.8660254037844382635, 0.000000000000000000 ) ) ;
#33343 = ORIENTED_EDGE ( 'NONE', *, *, #65103, .T. ) ;
#33342 = ADVANCED_FACE ( 'NONE', ( #69303 ), #42777, .F. ) ;
#33344 = DIRECTION ( 'NONE',  ( -0.7071067811865486830, -0.7071067811865464625, -2.597868168706476160E-16 ) ) ;
#33345 = LINE ( 'NONE', #54577, #753 ) ;
#33346 = CARTESIAN_POINT ( 'NONE',  ( -17.00000000000000000, -17.35230188589299871, 15.35019951917099945 ) ) ;
#33347 = DIRECTION ( 'NONE',  ( 0.000000000000000000, 0.7071067811865474617, -0.7071067811865474617 ) ) ;
#33348 = CARTESIAN_POINT ( 'NONE',  ( 12.90000000000000213, -0.1999999999911795112, 8.826273045769999343E-12 ) ) ;
#33349 = VECTOR ( 'NONE', #11780, 1000.000000000000114 ) ;
#33350 = ORIENTED_EDGE ( 'NONE', *, *, #47527, .F. ) ;
#33351 = ORIENTED_EDGE ( 'NONE', *, *, #57895, .T. ) ;
#33352 = VECTOR ( 'NONE', #63994, 1000.000000000000000 ) ;
#33353 = DIRECTION ( 'NONE',  ( 1.000000000000000000, 0.000000000000000000, 0.000000000000000000 ) ) ;
#33354 = CARTESIAN_POINT ( 'NONE',  ( -8.198316549646774476, -6.006483450353403697, 455.0000000000000568 ) ) ;
#33355 = CIRCLE ( 'NONE', #64961, 0.1999999999999987899 ) ;
#33356 = CIRCLE ( 'NONE', #42391, 0.1749999999999989342 ) ;
#33357 = CIRCLE ( 'NONE', #608, 0.1749999999999998224 ) ;
#33358 = EDGE_LOOP ( 'NONE', ( #16955, #61153, #39137, #38711, #45268, #2286, #35116, #23997 ) ) ;
#33359 = CARTESIAN_POINT ( 'NONE',  ( 17.00000000000000000, -17.00000000000000000, 15.70499999999969809 ) ) ;
#33360 = DIRECTION ( 'NONE',  ( 0.000000000000000000, -1.887379141859195671E-12, 1.000000000000000000 ) ) ;
#33361 = ORIENTED_EDGE ( 'NONE', *, *, #57009, .F. ) ;
#33362 = CARTESIAN_POINT ( 'NONE',  ( -11.31351654964670850, 7.793516549646603231, 195.0000000000000284 ) ) ;
#33363 = CARTESIAN_POINT ( 'NONE',  ( 8.250000000000005329, -8.249999999999998224, -26.00000000000001066 ) ) ;
#33364 = VECTOR ( 'NONE', #66427, 1000.000000000000000 ) ;
#33365 = AXIS2_PLACEMENT_3D ( 'NONE', #11118, #39369, #34051 ) ;
#33366 = ORIENTED_EDGE ( 'NONE', *, *, #39943, .T. ) ;
#33367 = CARTESIAN_POINT ( 'NONE',  ( -30.00000000000000000, -8.959999999999999076, -12.95475478405700009 ) ) ;
#33368 = CARTESIAN_POINT ( 'NONE',  ( -1.677516549646683730, 9.828310488885911411, 195.0000000000000284 ) ) ;
#33369 = AXIS2_PLACEMENT_3D ( 'NONE', #48017, #63591, #36713 ) ;
#33370 = CARTESIAN_POINT ( 'NONE',  ( 7.250000000000005329, -8.249999999999998224, -26.00000000000001066 ) ) ;
#33371 = CARTESIAN_POINT ( 'NONE',  ( 18.89999999999999858, -21.00000000000000000, 13.86939075806900057 ) ) ;
#33372 = ORIENTED_EDGE ( 'NONE', *, *, #20897, .F. ) ;
#33374 = ORIENTED_EDGE ( 'NONE', *, *, #66758, .T. ) ;
#33373 = DIRECTION ( 'NONE',  ( 1.000000000000000000, -0.000000000000000000, 0.000000000000000000 ) ) ;
#33375 = EDGE_CURVE ( 'NONE', #19854, #53029, #36600, .T. ) ;
#33376 = CARTESIAN_POINT ( 'NONE',  ( 9.562023737882805463, 8.130476262117184660, 54.00000000000000711 ) ) ;
#33377 = PLANE ( 'NONE',  #30106 ) ;
#33378 = DIRECTION ( 'NONE',  ( 1.334402673828313093E-16, 1.000000000000000000, 0.000000000000000000 ) ) ;
#33379 = ORIENTED_EDGE ( 'NONE', *, *, #44876, .F. ) ;
#33380 = VECTOR ( 'NONE', #43513, 1000.000000000000000 ) ;
#33381 = ADVANCED_FACE ( 'NONE', ( #60075 ), #54440, .F. ) ;
#33382 = CARTESIAN_POINT ( 'NONE',  ( 41.09999999999999432, -21.00000000000000000, 13.86939075806900057 ) ) ;
#33383 = CARTESIAN_POINT ( 'NONE',  ( -9.942044687070573872, -2.765062094116047309, 455.0000000000000568 ) ) ;
#33384 = EDGE_CURVE ( 'NONE', #13545, #42109, #43467, .T. ) ;
#33385 = ORIENTED_EDGE ( 'NONE', *, *, #54058, .T. ) ;
#33386 = VERTEX_POINT ( 'NONE', #5658 ) ;
#33387 = EDGE_CURVE ( 'NONE', #31415, #24890, #32536, .T. ) ;
#33388 = ORIENTED_EDGE ( 'NONE', *, *, #57655, .T. ) ;
#33389 = CARTESIAN_POINT ( 'NONE',  ( -11.99351654964683078, -11.19368345035334933, 455.0000000000000568 ) ) ;
#33390 = EDGE_CURVE ( 'NONE', #35406, #27652, #50166, .T. ) ;
#33391 = ADVANCED_FACE ( 'NONE', ( #21904 ), #43822, .F. ) ;
#33392 = LINE ( 'NONE', #15742, #52397 ) ;
#33393 = CARTESIAN_POINT ( 'NONE',  ( 7.806483450353379538, -11.12648345035348996, 455.0000000000000568 ) ) ;
#33394 = EDGE_CURVE ( 'NONE', #16184, #5636, #42252, .T. ) ;
#33395 = EDGE_LOOP ( 'NONE', ( #4022, #10444 ) ) ;
#33396 = VERTEX_POINT ( 'NONE', #26522 ) ;
#33397 = CIRCLE ( 'NONE', #4084, 1.224999999999999423 ) ;
#33398 = ORIENTED_EDGE ( 'NONE', *, *, #66314, .T. ) ;
#33399 = DIRECTION ( 'NONE',  ( 1.000000000000000000, -5.981805089575196197E-17, 0.000000000000000000 ) ) ;
#33400 = ORIENTED_EDGE ( 'NONE', *, *, #65253, .T. ) ;
#33401 = CIRCLE ( 'NONE', #39041, 0.5000000000009302559 ) ;
#33402 = ORIENTED_EDGE ( 'NONE', *, *, #3889, .T. ) ;
#33403 = ORIENTED_EDGE ( 'NONE', *, *, #69062, .T. ) ;
#33404 = ORIENTED_EDGE ( 'NONE', *, *, #61052, .F. ) ;
#33405 = AXIS2_PLACEMENT_3D ( 'NONE', #4844, #64248, #47622 ) ;
#33406 = CARTESIAN_POINT ( 'NONE',  ( 29.25000000000000000, -5.200000000000001066, 26.25000000000000000 ) ) ;
#33408 = EDGE_LOOP ( 'NONE', ( #54381, #59831, #28822, #60421 ) ) ;
#33407 = LINE ( 'NONE', #42622, #14168 ) ;
#33409 = CARTESIAN_POINT ( 'NONE',  ( -11.00000000000000000, -16.64230188589299786, -14.64519951917100116 ) ) ;
#33410 = CIRCLE ( 'NONE', #52597, 3.499999999999056310 ) ;
#33411 = AXIS2_PLACEMENT_3D ( 'NONE', #22822, #21787, #28460 ) ;
#33412 = VECTOR ( 'NONE', #2516, 1000.000000000000000 ) ;
#33413 = DIRECTION ( 'NONE',  ( -1.000000000000000000, 0.000000000000000000, 0.000000000000000000 ) ) ;
#33414 = DIRECTION ( 'NONE',  ( 0.000000000000000000, 0.000000000000000000, -1.000000000000000000 ) ) ;
#33415 = ORIENTED_EDGE ( 'NONE', *, *, #26431, .T. ) ;
#33416 = CONICAL_SURFACE ( 'NONE', #36810, 2.458500000000000796, 1.047019301333029784 ) ;
#33417 = DIRECTION ( 'NONE',  ( 1.000000000000000000, -1.261617073437657735E-14, 0.000000000000000000 ) ) ;
#33418 = LINE ( 'NONE', #55002, #7451 ) ;
#33419 = FACE_OUTER_BOUND ( 'NONE', #42404, .T. ) ;
#33420 = AXIS2_PLACEMENT_3D ( 'NONE', #4116, #68807, #31345 ) ;
#33421 = ORIENTED_EDGE ( 'NONE', *, *, #48780, .T. ) ;
#33422 = FACE_OUTER_BOUND ( 'NONE', #38455, .T. ) ;
#33423 = EDGE_CURVE ( 'NONE', #14823, #961, #65049, .T. ) ;
#33424 = CARTESIAN_POINT ( 'NONE',  ( 10.00000000000000000, 21.00000000000000000, 18.00000000000000355 ) ) ;
#33425 = CARTESIAN_POINT ( 'NONE',  ( 10.05377373788278739, -9.703773737882823269, 54.00000000000000711 ) ) ;
#33426 = VERTEX_POINT ( 'NONE', #16618 ) ;
#33427 = EDGE_CURVE ( 'NONE', #65287, #12110, #59222, .T. ) ;
#33428 = AXIS2_PLACEMENT_3D ( 'NONE', #38146, #6297, #54402 ) ;
#33429 = LINE ( 'NONE', #65603, #64079 ) ;
#33430 = EDGE_CURVE ( 'NONE', #19600, #8140, #48785, .T. ) ;
#33431 = DIRECTION ( 'NONE',  ( 0.000000000000000000, 0.000000000000000000, 1.000000000000000000 ) ) ;
#33432 = DIRECTION ( 'NONE',  ( 4.336808689942043768E-15, 1.000000000000000000, 0.000000000000000000 ) ) ;
#33433 = ADVANCED_FACE ( 'NONE', ( #1046 ), #3, .F. ) ;
#33434 = CARTESIAN_POINT ( 'NONE',  ( -5.779227145995285753, -4.155633711806640207, 54.00000000000000711 ) ) ;
#33435 = DIRECTION ( 'NONE',  ( -1.000000000000000000, 0.000000000000000000, 0.000000000000000000 ) ) ;
#33436 = CARTESIAN_POINT ( 'NONE',  ( 0.000000000000000000, 0.000000000000000000, 0.000000000000000000 ) ) ;
#33437 = SURFACE_STYLE_USAGE ( .BOTH. , #17863 ) ;
#33438 = CARTESIAN_POINT ( 'NONE',  ( 30.00000000000000000, -16.64230188589299786, -14.64519951917100116 ) ) ;
#33439 = VERTEX_POINT ( 'NONE', #344 ) ;
#33440 = DIRECTION ( 'NONE',  ( -1.000000000000000000, 0.000000000000000000, 0.000000000000000000 ) ) ;
#33441 = VECTOR ( 'NONE', #32311, 1000.000000000000000 ) ;
#33442 = LINE ( 'NONE', #43344, #68086 ) ;
#33443 = CARTESIAN_POINT ( 'NONE',  ( -5.098491296477297929, 7.878491296477155181, 195.0000000000000284 ) ) ;
#33444 = CARTESIAN_POINT ( 'NONE',  ( 75.42576880091937142, 0.000000000000000000, 282.4830310981789125 ) ) ;
#33445 = EDGE_LOOP ( 'NONE', ( #21276, #47235, #59030, #48197 ) ) ;
#33446 = CARTESIAN_POINT ( 'NONE',  ( 8.835729544836338434, -8.144523737882822800, 54.00000000000000711 ) ) ;
#33447 = DIRECTION ( 'NONE',  ( -0.7071067811865475727, -0.7071067811865475727, 0.000000000000000000 ) ) ;
#33448 = DIRECTION ( 'NONE',  ( 0.000000000000000000, -0.000000000000000000, 1.000000000000000000 ) ) ;
#33449 = CIRCLE ( 'NONE', #11977, 3.499999999999999556 ) ;
#33450 = DIRECTION ( 'NONE',  ( 0.000000000000000000, -3.673940397442059868E-16, 1.000000000000000000 ) ) ;
#33451 = CARTESIAN_POINT ( 'NONE',  ( 17.51999999999999957, -17.50000000000000000, 26.00000000000000355 ) ) ;
#33452 = EDGE_LOOP ( 'NONE', ( #11214, #65328, #33543, #31164 ) ) ;
#33453 = AXIS2_PLACEMENT_3D ( 'NONE', #49873, #1428, #24033 ) ;
#33454 = EDGE_CURVE ( 'NONE', #29737, #46983, #11286, .T. ) ;
#33455 = AXIS2_PLACEMENT_3D ( 'NONE', #32190, #22288, #59061 ) ;
#33456 = CARTESIAN_POINT ( 'NONE',  ( 3.724485858128679716, 7.394232575409564134, 26.00000000000000711 ) ) ;
#33457 = LINE ( 'NONE', #6236, #51512 ) ;
#33458 = EDGE_LOOP ( 'NONE', ( #12358, #50442, #1677, #58133 ) ) ;
#33459 = VECTOR ( 'NONE', #58831, 1000.000000000000000 ) ;
#33460 = AXIS2_PLACEMENT_3D ( 'NONE', #39625, #23380, #17039 ) ;
#33461 = CIRCLE ( 'NONE', #42505, 2.204799999999997429 ) ;
#33462 = CARTESIAN_POINT ( 'NONE',  ( 176.4833316329832940, -10.00000000000000178, 324.6739988703752715 ) ) ;
#33463 = ORIENTED_EDGE ( 'NONE', *, *, #22335, .T. ) ;
#33464 = PLANE ( 'NONE',  #17598 ) ;
#33465 = VERTEX_POINT ( 'NONE', #65395 ) ;
#33466 = ORIENTED_EDGE ( 'NONE', *, *, #47052, .T. ) ;
#33467 = CARTESIAN_POINT ( 'NONE',  ( -5.993516549646711766, 5.993516549646603409, 455.0000000000000568 ) ) ;
#33468 = ADVANCED_FACE ( 'NONE', ( #42430 ), #59391, .F. ) ;
#33469 = ORIENTED_EDGE ( 'NONE', *, *, #65185, .F. ) ;
#33470 = DIRECTION ( 'NONE',  ( -1.836970198721029934E-16, 1.836970198721036344E-16, -1.000000000000000000 ) ) ;
#33471 = DIRECTION ( 'NONE',  ( -1.000000000000000000, 0.000000000000000000, 0.000000000000000000 ) ) ;
#33472 = FACE_OUTER_BOUND ( 'NONE', #19905, .T. ) ;
#33473 = AXIS2_PLACEMENT_3D ( 'NONE', #56361, #17841, #40451 ) ;
#33474 = ADVANCED_FACE ( 'NONE', ( #22264 ), #16954, .F. ) ;
#33475 = ORIENTED_EDGE ( 'NONE', *, *, #35375, .F. ) ;
#33476 = ORIENTED_EDGE ( 'NONE', *, *, #3767, .F. ) ;
#33477 = PLANE ( 'NONE',  #36922 ) ;
#33478 = LINE ( 'NONE', #55394, #59309 ) ;
#33479 = ORIENTED_EDGE ( 'NONE', *, *, #57126, .F. ) ;
#33480 = EDGE_LOOP ( 'NONE', ( #53083, #65396, #42937, #36175 ) ) ;
#33481 = VERTEX_POINT ( 'NONE', #38523 ) ;
#33482 = LINE ( 'NONE', #49742, #66095 ) ;
#33484 = ORIENTED_EDGE ( 'NONE', *, *, #14237, .F. ) ;
#33483 = DIRECTION ( 'NONE',  ( 0.000000000000000000, 1.000000000000000000, 0.000000000000000000 ) ) ;
#33485 = DIRECTION ( 'NONE',  ( -1.000000000000000000, 0.000000000000000000, 0.000000000000000000 ) ) ;
#33486 = CARTESIAN_POINT ( 'NONE',  ( -3.842976262117327124, -10.31452373788281207, 26.00000000000000000 ) ) ;
#33487 = VERTEX_POINT ( 'NONE', #10260 ) ;
#33488 = AXIS2_PLACEMENT_3D ( 'NONE', #47093, #68666, #26222 ) ;
#33489 = VERTEX_POINT ( 'NONE', #15913 ) ;
#33490 = AXIS2_PLACEMENT_3D ( 'NONE', #50325, #45358, #34752 ) ;
#33491 = CARTESIAN_POINT ( 'NONE',  ( 29.25000000000000000, -5.200000000000001066, -11.75000000000000000 ) ) ;
#33492 = DIRECTION ( 'NONE',  ( 0.000000000000000000, 0.000000000000000000, 1.000000000000000000 ) ) ;
#33493 = CIRCLE ( 'NONE', #64008, 25.39999999999999858 ) ;
#33494 = AXIS2_PLACEMENT_3D ( 'NONE', #6028, #32562, #54127 ) ;
#33495 = VECTOR ( 'NONE', #10828, 1000.000000000000000 ) ;
#33496 = VECTOR ( 'NONE', #67084, 1000.000000000000000 ) ;
#33497 = VECTOR ( 'NONE', #38128, 1000.000000000000000 ) ;
#33498 = CARTESIAN_POINT ( 'NONE',  ( 41.09999999999999432, -14.06939075806900163, 20.80000000000000426 ) ) ;
#33500 = CARTESIAN_POINT ( 'NONE',  ( 10.50000000000000178, 9.690000000000001279, -5.000000000000000000 ) ) ;
#33499 = CIRCLE ( 'NONE', #18969, 3.499999999999999556 ) ;
#33501 = ORIENTED_EDGE ( 'NONE', *, *, #4214, .T. ) ;
#33502 = ORIENTED_EDGE ( 'NONE', *, *, #45326, .F. ) ;
#33503 = EDGE_CURVE ( 'NONE', #30661, #53553, #65733, .T. ) ;
#33504 = CARTESIAN_POINT ( 'NONE',  ( -7.250000000000000888, -8.249999999999998224, -10.50000000000000000 ) ) ;
#33505 = VECTOR ( 'NONE', #19149, 1000.000000000000000 ) ;
#33506 = CYLINDRICAL_SURFACE ( 'NONE', #49934, 24.99999999998784972 ) ;
#33507 = DIRECTION ( 'NONE',  ( 1.356437060717832013E-15, 1.000000000000000000, 0.000000000000000000 ) ) ;
#33508 = DIRECTION ( 'NONE',  ( -0.000000000000000000, 1.000000000000000000, -0.000000000000000000 ) ) ;
#33509 = EDGE_CURVE ( 'NONE', #61702, #20422, #64878, .T. ) ;
#33510 = VECTOR ( 'NONE', #65340, 1000.000000000000000 ) ;
#33511 = DIRECTION ( 'NONE',  ( 1.000000000000000000, -0.000000000000000000, -0.000000000000000000 ) ) ;
#33512 = ORIENTED_EDGE ( 'NONE', *, *, #18044, .T. ) ;
#33513 = CARTESIAN_POINT ( 'NONE',  ( 283.0000000000000568, -20.50000000000000000, -17.00000000000000000 ) ) ;
#33514 = DIRECTION ( 'NONE',  ( -1.000000000000000000, 7.304098846218132892E-15, 0.000000000000000000 ) ) ;
#33515 = CARTESIAN_POINT ( 'NONE',  ( -11.31351654964674402, -4.406483450353330333, 455.0000000000000568 ) ) ;
#33516 = DIRECTION ( 'NONE',  ( 0.000000000000000000, -1.000000000000000000, 0.000000000000000000 ) ) ;
#33517 = PRODUCT_DEFINITION_SHAPE ( 'NONE', 'NONE',  #20553 ) ;
#33518 = AXIS2_PLACEMENT_3D ( 'NONE', #20551, #36833, #58401 ) ;
#33519 = DIRECTION ( 'NONE',  ( -1.836970198721029934E-16, 1.836970198721036590E-16, -1.000000000000000000 ) ) ;
#33520 = FACE_OUTER_BOUND ( 'NONE', #14854, .T. ) ;
#33521 = CARTESIAN_POINT ( 'NONE',  ( -4.459829165594022982, 6.892329165593917395, 26.00000000000000711 ) ) ;
#33522 = ORIENTED_EDGE ( 'NONE', *, *, #28577, .T. ) ;
#33523 = DIRECTION ( 'NONE',  ( 0.7071067811865348052, -0.7071067811865602293, -3.278703137324831017E-30 ) ) ;
#33524 = DIRECTION ( 'NONE',  ( -1.000000000000000000, 0.000000000000000000, 0.000000000000000000 ) ) ;
#33525 = VERTEX_POINT ( 'NONE', #18311 ) ;
#33526 = DIRECTION ( 'NONE',  ( -0.000000000000000000, -0.000000000000000000, -1.000000000000000000 ) ) ;
#33527 = DIRECTION ( 'NONE',  ( 0.7071067811865500152, 0.7071067811865451302, -4.683861624749757595E-31 ) ) ;
#33528 = CARTESIAN_POINT ( 'NONE',  ( 4.740315990920173306, 7.798499376343941414, 455.0000000000000568 ) ) ;
#33529 = ADVANCED_FACE ( 'NONE', ( #11964 ), #17285, .T. ) ;
#33530 = CARTESIAN_POINT ( 'NONE',  ( 4.456444791733522252E-16, 7.450000000000002842, -11.50000000000000000 ) ) ;
#33531 = FACE_OUTER_BOUND ( 'NONE', #38575, .T. ) ;
#33532 = CARTESIAN_POINT ( 'NONE',  ( -8.566576262117260754, 9.689726262117185129, 26.00000000000000711 ) ) ;
#33533 = VERTEX_POINT ( 'NONE', #61440 ) ;
#33534 = CARTESIAN_POINT ( 'NONE',  ( 15.50000000000000000, -0.2000000000000000111, 22.50000000000000000 ) ) ;
#33535 = ORIENTED_EDGE ( 'NONE', *, *, #62305, .T. ) ;
#33536 = CARTESIAN_POINT ( 'NONE',  ( 41.09999999999999432, -14.06939075806901940, -20.80000000000000426 ) ) ;
#33537 = CARTESIAN_POINT ( 'NONE',  ( 11.50000000000000000, -12.00000000000000000, -11.00000000000000000 ) ) ;
#33538 = AXIS2_PLACEMENT_3D ( 'NONE', #33165, #1006, #21864 ) ;
#33539 = CARTESIAN_POINT ( 'NONE',  ( -5.538810540050023157, 7.342976262117183239, 54.00000000000000711 ) ) ;
#33540 = ORIENTED_EDGE ( 'NONE', *, *, #11507, .F. ) ;
#33541 = ORIENTED_EDGE ( 'NONE', *, *, #54144, .F. ) ;
#33542 = CARTESIAN_POINT ( 'NONE',  ( -2.617976262117287956, -6.501044194225499062, 26.00000000000000711 ) ) ;
#33543 = ORIENTED_EDGE ( 'NONE', *, *, #23564, .F. ) ;
#33544 = EDGE_LOOP ( 'NONE', ( #28318, #45207, #37670, #64888 ) ) ;
#33545 = EDGE_CURVE ( 'NONE', #42663, #45572, #13373, .T. ) ;
#33546 = CIRCLE ( 'NONE', #64074, 1.000000000000001776 ) ;
#33547 = DIRECTION ( 'NONE',  ( 1.000000000000000000, 0.000000000000000000, 0.000000000000000000 ) ) ;
#33548 = DIRECTION ( 'NONE',  ( 1.000000000000000000, 0.000000000000000000, 0.000000000000000000 ) ) ;
#33549 = DIRECTION ( 'NONE',  ( -1.836970198721029934E-16, 1.836970198721036590E-16, -1.000000000000000000 ) ) ;
#33550 = EDGE_CURVE ( 'NONE', #67635, #20187, #50842, .T. ) ;
#33551 = ADVANCED_FACE ( 'NONE', ( #8052 ), #22601, .F. ) ;
#33552 = ORIENTED_EDGE ( 'NONE', *, *, #14439, .F. ) ;
#33553 = DIRECTION ( 'NONE',  ( 0.000000000000000000, -2.854859206170826497E-12, 1.000000000000000000 ) ) ;
#33554 = AXIS2_PLACEMENT_3D ( 'NONE', #4132, #58212, #37013 ) ;
#33555 = VECTOR ( 'NONE', #25382, 1000.000000000000000 ) ;
#33557 = DIRECTION ( 'NONE',  ( 1.000000000000000000, -0.000000000000000000, 0.000000000000000000 ) ) ;
#33556 = LINE ( 'NONE', #19033, #60359 ) ;
#33558 = ORIENTED_EDGE ( 'NONE', *, *, #35423, .T. ) ;
#33561 = ORIENTED_EDGE ( 'NONE', *, *, #57472, .T. ) ;
#33560 = EDGE_CURVE ( 'NONE', #67897, #58614, #21966, .T. ) ;
#33559 = DIRECTION ( 'NONE',  ( -0.000000000000000000, 3.673940397442059868E-16, -1.000000000000000000 ) ) ;
#33562 = ORIENTED_EDGE ( 'NONE', *, *, #52399, .T. ) ;
#33563 = EDGE_CURVE ( 'NONE', #53573, #9491, #39876, .T. ) ;
#33564 = CARTESIAN_POINT ( 'NONE',  ( 0.006483450353333613213, -0.006483450353373412106, 195.0000000000000284 ) ) ;
#33565 = ADVANCED_FACE ( 'NONE', ( #44156 ), #6672, .F. ) ;
#33566 = DIRECTION ( 'NONE',  ( -0.4998444328988824181, 0.000000000000000000, 0.8661152018640445593 ) ) ;
#33567 = EDGE_CURVE ( 'NONE', #21827, #10161, #34219, .T. ) ;
#33568 = AXIS2_PLACEMENT_3D ( 'NONE', #34966, #2109, #62538 ) ;
#33569 = PLANE ( 'NONE',  #38224 ) ;
#33570 = ORIENTED_EDGE ( 'NONE', *, *, #50259, .F. ) ;
#33571 = ORIENTED_EDGE ( 'NONE', *, *, #30195, .T. ) ;
#33572 = DIRECTION ( 'NONE',  ( 0.000000000000000000, 1.000000000000000000, 0.000000000000000000 ) ) ;
#33573 = CARTESIAN_POINT ( 'NONE',  ( 39.90000000000000568, -16.96999999999999886, -21.00000000000000000 ) ) ;
#33574 = EDGE_LOOP ( 'NONE', ( #22888, #40868, #49631, #34971 ) ) ;
#33575 = PLANE ( 'NONE',  #17267 ) ;
#33576 = CARTESIAN_POINT ( 'NONE',  ( 8.930623737882843471, 8.566576262117187923, 54.00000000000000711 ) ) ;
#33577 = FACE_OUTER_BOUND ( 'NONE', #49425, .T. ) ;
#33578 = ORIENTED_EDGE ( 'NONE', *, *, #33770, .T. ) ;
#33579 = CARTESIAN_POINT ( 'NONE',  ( 7.250000000000005329, -7.249999999999998224, -26.00000000000001066 ) ) ;
#33580 = EDGE_CURVE ( 'NONE', #51180, #9398, #18668, .T. ) ;
#33581 = DIRECTION ( 'NONE',  ( -1.000000000000000000, 0.000000000000000000, 0.000000000000000000 ) ) ;
#33582 = AXIS2_PLACEMENT_3D ( 'NONE', #40642, #41693, #46293 ) ;
#33584 = ORIENTED_EDGE ( 'NONE', *, *, #42887, .F. ) ;
#33583 = DIRECTION ( 'NONE',  ( 0.000000000000000000, -0.000000000000000000, 1.000000000000000000 ) ) ;
#33586 = EDGE_LOOP ( 'NONE', ( #20924, #51988, #35192, #63845 ) ) ;
#33585 = DIRECTION ( 'NONE',  ( -1.000000000000000000, 0.000000000000000000, 0.000000000000000000 ) ) ;
#33587 = CARTESIAN_POINT ( 'NONE',  ( -11.18999999999999950, -11.18999999999999950, -4.250000000000000000 ) ) ;
#33588 = DIRECTION ( 'NONE',  ( -1.000000000000000000, 0.000000000000000000, 0.000000000000000000 ) ) ;
#33589 = CARTESIAN_POINT ( 'NONE',  ( -8.393516549646697911, -4.396432944014502020, 195.0000000000000284 ) ) ;
#33590 = DIRECTION ( 'NONE',  ( -1.836970198721029934E-16, 1.836970198721036344E-16, -1.000000000000000000 ) ) ;
#33591 = FACE_OUTER_BOUND ( 'NONE', #6272, .T. ) ;
#33592 = VECTOR ( 'NONE', #67505, 1000.000000000000114 ) ;
#33593 = AXIS2_PLACEMENT_3D ( 'NONE', #41245, #14392, #52209 ) ;
#33594 = CIRCLE ( 'NONE', #69759, 3.499999999999054534 ) ;
#33595 = SHAPE_REPRESENTATION ( 'Stepper Motor', ( #45918 ), #55023 ) ;
#33596 = LINE ( 'NONE', #27951, #31527 ) ;
#33597 = VERTEX_POINT ( 'NONE', #1715 ) ;
#33598 = DIRECTION ( 'NONE',  ( 0.000000000000000000, 0.000000000000000000, 1.000000000000000000 ) ) ;
#33599 = CARTESIAN_POINT ( 'NONE',  ( 29.50000000000000355, -11.50000000000100009, 10.50000000000065903 ) ) ;
#33600 = AXIS2_PLACEMENT_3D ( 'NONE', #32933, #22342, #17020 ) ;
#33603 = ORIENTED_EDGE ( 'NONE', *, *, #51451, .F. ) ;
#33602 = PLANE ( 'NONE',  #42342 ) ;
#33601 = VECTOR ( 'NONE', #22715, 1000.000000000000000 ) ;
#33604 = PLANE ( 'NONE',  #23341 ) ;
#33605 = LINE ( 'NONE', #50566, #67941 ) ;
#33606 = AXIS2_PLACEMENT_3D ( 'NONE', #12873, #25260, #68393 ) ;
#33607 = VECTOR ( 'NONE', #69911, 1000.000000000000000 ) ;
#33608 = EDGE_CURVE ( 'NONE', #64355, #40740, #28243, .T. ) ;
#33609 = ORIENTED_EDGE ( 'NONE', *, *, #8092, .F. ) ;
#33610 = DIRECTION ( 'NONE',  ( -0.000000000000000000, -0.000000000000000000, 1.000000000000000000 ) ) ;
#33611 = FACE_OUTER_BOUND ( 'NONE', #43870, .T. ) ;
#33612 = ORIENTED_EDGE ( 'NONE', *, *, #2409, .F. ) ;
#33613 = FACE_OUTER_BOUND ( 'NONE', #22234, .T. ) ;
#33614 = CARTESIAN_POINT ( 'NONE',  ( 4.201500623656052369, 4.727349090213339267, 455.0000000000000568 ) ) ;
#33615 = CARTESIAN_POINT ( 'NONE',  ( -11.99351654964671354, 11.18071654964658990, 195.0000000000000284 ) ) ;
#33616 = ADVANCED_FACE ( 'NONE', ( #34921 ), #40237, .F. ) ;
#33617 = CARTESIAN_POINT ( 'NONE',  ( 27.00000000000000000, 0.000000000000000000, -2.458500000000000796 ) ) ;
#33618 = AXIS2_PLACEMENT_3D ( 'NONE', #4135, #20383, #30298 ) ;
#33619 = FACE_BOUND ( 'NONE', #54590, .T. ) ;
#33620 = ORIENTED_EDGE ( 'NONE', *, *, #10395, .F. ) ;
#33621 = FACE_OUTER_BOUND ( 'NONE', #35661, .T. ) ;
#33622 = VERTEX_POINT ( 'NONE', #67112 ) ;
#33623 = EDGE_CURVE ( 'NONE', #28084, #3378, #29623, .T. ) ;
#33624 = ORIENTED_EDGE ( 'NONE', *, *, #45582, .T. ) ;
#33625 = DIRECTION ( 'NONE',  ( 0.000000000000000000, 0.000000000000000000, 1.000000000000000000 ) ) ;
#33626 = LINE ( 'NONE', #68150, #47819 ) ;
#33627 = ADVANCED_FACE ( 'NONE', ( #28933 ), #50509, .F. ) ;
#33628 = EDGE_CURVE ( 'NONE', #45304, #24526, #68297, .T. ) ;
#33629 = DIRECTION ( 'NONE',  ( -1.000000000000000000, 0.000000000000000000, 0.000000000000000000 ) ) ;
#33630 = CARTESIAN_POINT ( 'NONE',  ( 29.89999999999999858, -0.1999999999911430404, -8.864436962241481021E-12 ) ) ;
#33631 = VERTEX_POINT ( 'NONE', #2412 ) ;
#33632 = ORIENTED_EDGE ( 'NONE', *, *, #2972, .T. ) ;
#33634 = ORIENTED_EDGE ( 'NONE', *, *, #6043, .F. ) ;
#33633 = CARTESIAN_POINT ( 'NONE',  ( 9.690000000000001279, -8.750000000000000000, -5.000000000000000000 ) ) ;
#33635 = VERTEX_POINT ( 'NONE', #23976 ) ;
#33636 = CARTESIAN_POINT ( 'NONE',  ( 5.257023737882801306, 5.242976262117200470, 54.00000000000000711 ) ) ;
#33637 = DIRECTION ( 'NONE',  ( -0.000000000000000000, -0.000000000000000000, 1.000000000000000000 ) ) ;
#33638 = EDGE_CURVE ( 'NONE', #17310, #47121, #58264, .T. ) ;
#33639 = CARTESIAN_POINT ( 'NONE',  ( -8.916576262117340335, -8.580623737882760338, 26.00000000000000000 ) ) ;
#33640 = VECTOR ( 'NONE', #25264, 1000.000000000000000 ) ;
#33641 = DIRECTION ( 'NONE',  ( 1.000000000000000000, 0.000000000000000000, 0.000000000000000000 ) ) ;
#33643 = DIRECTION ( 'NONE',  ( 1.000000000000000000, 0.000000000000000000, 0.000000000000000000 ) ) ;
#33642 = CARTESIAN_POINT ( 'NONE',  ( -7.250000000000000888, 7.450000000000003730, -23.50000000000000000 ) ) ;
#33644 = ORIENTED_EDGE ( 'NONE', *, *, #26825, .T. ) ;
#33646 = VERTEX_POINT ( 'NONE', #41994 ) ;
#33645 = DIRECTION ( 'NONE',  ( -0.4999999999999170108, 1.060575238724965586E-16, -0.8660254037844865582 ) ) ;
#33647 = ORIENTED_EDGE ( 'NONE', *, *, #60427, .F. ) ;
#33648 = EDGE_LOOP ( 'NONE', ( #9196, #25200, #44336, #21288 ) ) ;
#33649 = ADVANCED_FACE ( 'NONE', ( #57206 ), #24687, .F. ) ;
#33650 = CARTESIAN_POINT ( 'NONE',  ( 30.00000000000000000, -9.200000000000120082, 17.30000000000000071 ) ) ;
#33651 = EDGE_CURVE ( 'NONE', #25947, #31047, #20426, .T. ) ;
#33652 = DIRECTION ( 'NONE',  ( -1.000000000000000000, -3.016910393003147986E-15, 0.000000000000000000 ) ) ;
#33653 = FACE_OUTER_BOUND ( 'NONE', #67953, .T. ) ;
#33654 = ORIENTED_EDGE ( 'NONE', *, *, #41406, .F. ) ;
#33655 = VERTEX_POINT ( 'NONE', #68524 ) ;
#33656 = CIRCLE ( 'NONE', #61960, 24.99999999998794920 ) ;
#33657 = VECTOR ( 'NONE', #36606, 1000.000000000000000 ) ;
#33658 = FACE_OUTER_BOUND ( 'NONE', #14346, .T. ) ;
#33659 = LINE ( 'NONE', #40349, #39054 ) ;
#33660 = ORIENTED_EDGE ( 'NONE', *, *, #23597, .F. ) ;
#33661 = ORIENTED_EDGE ( 'NONE', *, *, #6927, .T. ) ;
#33662 = CARTESIAN_POINT ( 'NONE',  ( -9.942044687070573872, -2.765062094116046865, 455.0000000000000568 ) ) ;
#33663 = DIRECTION ( 'NONE',  ( -1.836970198721029934E-16, 1.836970198721036590E-16, -1.000000000000000000 ) ) ;
#33664 = EDGE_LOOP ( 'NONE', ( #5802, #69880, #3693, #36504 ) ) ;
#33665 = AXIS2_PLACEMENT_3D ( 'NONE', #17858, #22815, #44362 ) ;
#33666 = DIRECTION ( 'NONE',  ( 0.000000000000000000, 0.000000000000000000, 1.000000000000000000 ) ) ;
#33667 = EDGE_LOOP ( 'NONE', ( #60282, #1554, #28012, #30162 ) ) ;
#33668 = ORIENTED_EDGE ( 'NONE', *, *, #9058, .F. ) ;
#33669 = DIRECTION ( 'NONE',  ( 0.000000000000000000, 0.000000000000000000, -1.000000000000000000 ) ) ;
#33670 = DIRECTION ( 'NONE',  ( 0.5773502691896291728, 0.5773502691896271743, 0.5773502691896209571 ) ) ;
#33671 = CARTESIAN_POINT ( 'NONE',  ( -15.50000000000000000, -1.037157890325000054, 22.50000000000000000 ) ) ;
#33672 = FACE_OUTER_BOUND ( 'NONE', #56707, .T. ) ;
#33673 = DIRECTION ( 'NONE',  ( 0.000000000000000000, -1.000000000000000000, -0.000000000000000000 ) ) ;
#33674 = EDGE_CURVE ( 'NONE', #8412, #6993, #9474, .T. ) ;
#33675 = CARTESIAN_POINT ( 'NONE',  ( 283.0000000000000568, -38.09999999999885034, -7.900000000002049383 ) ) ;
#33676 = VERTEX_POINT ( 'NONE', #35626 ) ;
#33677 = DIRECTION ( 'NONE',  ( 0.6414496315691537998, -0.7671651518153029814, -2.309356642088714001E-17 ) ) ;
#33678 = ADVANCED_FACE ( 'NONE', ( #46587 ), #19370, .F. ) ;
#33679 = ORIENTED_EDGE ( 'NONE', *, *, #69936, .T. ) ;
#33680 = FACE_OUTER_BOUND ( 'NONE', #12097, .T. ) ;
#33681 = LINE ( 'NONE', #48922, #33441 ) ;
#33683 = ADVANCED_FACE ( 'NONE', ( #40934 ), #63574, .F. ) ;
#33682 = FACE_OUTER_BOUND ( 'NONE', #43952, .T. ) ;
#33684 = DIRECTION ( 'NONE',  ( 0.000000000000000000, 0.000000000000000000, 1.000000000000000000 ) ) ;
#33685 = FACE_OUTER_BOUND ( 'NONE', #54374, .T. ) ;
#33686 = ADVANCED_FACE ( 'NONE', ( #31039 ), #62863, .F. ) ;
#33687 = ORIENTED_EDGE ( 'NONE', *, *, #51159, .T. ) ;
#33688 = EDGE_LOOP ( 'NONE', ( #49583, #54537, #23619, #47140, #25379, #38638 ) ) ;
#33689 = FACE_OUTER_BOUND ( 'NONE', #32264, .T. ) ;
#33690 = EDGE_CURVE ( 'NONE', #20305, #6090, #68163, .T. ) ;
#33691 = CARTESIAN_POINT ( 'NONE',  ( 7.532023737882817649, -6.665817930929303969, 54.00000000000000711 ) ) ;
#33692 = VERTEX_POINT ( 'NONE', #35265 ) ;
#33693 = DIRECTION ( 'NONE',  ( 0.000000000000000000, -0.9921567416492215186, 0.1249999999999996531 ) ) ;
#33694 = ORIENTED_EDGE ( 'NONE', *, *, #12480, .T. ) ;
#33695 = EDGE_CURVE ( 'NONE', #9319, #48333, #7298, .T. ) ;
#33696 = EDGE_LOOP ( 'NONE', ( #18283, #4034, #44672, #44267 ) ) ;
#33697 = EDGE_CURVE ( 'NONE', #37598, #28520, #67125, .T. ) ;
#33698 = AXIS2_PLACEMENT_3D ( 'NONE', #66291, #6880, #13234 ) ;
#33699 = CARTESIAN_POINT ( 'NONE',  ( 275.0000000000000000, -26.50000000000000000, 0.5000000000000000000 ) ) ;
#33700 = FACE_BOUND ( 'NONE', #2073, .T. ) ;
#33701 = EDGE_LOOP ( 'NONE', ( #49952, #18644, #14620, #14413, #61829, #3507, #40243, #21297, #47343 ) ) ;
#33702 = DIRECTION ( 'NONE',  ( -1.000000000000000000, 0.000000000000000000, 0.000000000000000000 ) ) ;
#33703 = DIRECTION ( 'NONE',  ( 0.000000000000000000, 0.7066873191085843997, 0.7075259945833241026 ) ) ;
#33704 = ADVANCED_FACE ( 'NONE', ( #40591 ), #8402, .F. ) ;
#33705 = EDGE_CURVE ( 'NONE', #11614, #8621, #44553, .T. ) ;
#33706 = DIRECTION ( 'NONE',  ( 0.000000000000000000, 0.000000000000000000, 1.000000000000000000 ) ) ;
#33707 = CARTESIAN_POINT ( 'NONE',  ( -5.993516549646711766, 5.993516549646603409, 455.0000000000000568 ) ) ;
#33708 = ORIENTED_EDGE ( 'NONE', *, *, #28704, .F. ) ;
#33710 = VERTEX_POINT ( 'NONE', #30339 ) ;
#33709 = DIRECTION ( 'NONE',  ( -1.000000000000000000, 0.000000000000000000, 0.000000000000000000 ) ) ;
#33711 = EDGE_CURVE ( 'NONE', #29119, #18299, #62491, .T. ) ;
#33712 = AXIS2_PLACEMENT_3D ( 'NONE', #16752, #143, #33004 ) ;
#33713 = CARTESIAN_POINT ( 'NONE',  ( 7.250000000000004441, 7.450000000000001954, -14.50000000000000000 ) ) ;
#33714 = FACE_OUTER_BOUND ( 'NONE', #8680, .T. ) ;
#33715 = FACE_OUTER_BOUND ( 'NONE', #62140, .T. ) ;
#33716 = DIRECTION ( 'NONE',  ( 0.000000000000000000, 0.000000000000000000, -1.000000000000000000 ) ) ;
#33717 = EDGE_LOOP ( 'NONE', ( #36162, #37479, #1159, #37546 ) ) ;
#33718 = FACE_OUTER_BOUND ( 'NONE', #35104, .T. ) ;
#33719 = EDGE_CURVE ( 'NONE', #11562, #49395, #68871, .T. ) ;
#33720 = CARTESIAN_POINT ( 'NONE',  ( 16.89999999999999858, -14.06939075806900163, -20.80000000000000426 ) ) ;
#33721 = EDGE_LOOP ( 'NONE', ( #2496, #14204, #18074, #56494 ) ) ;
#33722 = ORIENTED_EDGE ( 'NONE', *, *, #14439, .T. ) ;
#33723 = ORIENTED_EDGE ( 'NONE', *, *, #33628, .F. ) ;
#33724 = DIRECTION ( 'NONE',  ( -0.000000000000000000, -0.000000000000000000, -1.000000000000000000 ) ) ;
#33725 = EDGE_CURVE ( 'NONE', #13669, #47507, #29876, .T. ) ;
#33726 = CARTESIAN_POINT ( 'NONE',  ( 6.849523737882818430, 10.49297626211719603, 54.00000000000000711 ) ) ;
#33727 = LINE ( 'NONE', #18156, #12317 ) ;
#33728 = EDGE_CURVE ( 'NONE', #46086, #45981, #3123, .T. ) ;
#33729 = CARTESIAN_POINT ( 'NONE',  ( 2.420780051175169145, 8.697938382363084031, 54.00000000000000711 ) ) ;
#33730 = ORIENTED_EDGE ( 'NONE', *, *, #10560, .F. ) ;
#33731 = ORIENTED_EDGE ( 'NONE', *, *, #27702, .T. ) ;
#33732 = ORIENTED_EDGE ( 'NONE', *, *, #64726, .F. ) ;
#33733 = PLANE ( 'NONE',  #18110 ) ;
#33734 = VERTEX_POINT ( 'NONE', #25385 ) ;
#33735 = ORIENTED_EDGE ( 'NONE', *, *, #47380, .T. ) ;
#33736 = VERTEX_POINT ( 'NONE', #1542 ) ;
#33737 = CIRCLE ( 'NONE', #3261, 24.99999999998794920 ) ;
#33738 = ORIENTED_EDGE ( 'NONE', *, *, #68021, .T. ) ;
#33739 = CARTESIAN_POINT ( 'NONE',  ( 4.456444791733522252E-16, 7.450000000000002842, -16.00000000000000000 ) ) ;
#33741 = VERTEX_POINT ( 'NONE', #63923 ) ;
#33740 = CARTESIAN_POINT ( 'NONE',  ( -5.538810540050064901, -7.357023737882800951, 54.00000000000000711 ) ) ;
#33742 = VECTOR ( 'NONE', #6081, 1000.000000000000000 ) ;
#33743 = DIRECTION ( 'NONE',  ( 0.000000000000000000, 0.000000000000000000, 1.000000000000000000 ) ) ;
#33744 = CARTESIAN_POINT ( 'NONE',  ( 7.000000000000000000, -25.60000000000000142, 17.60000000000000142 ) ) ;
#33745 = CARTESIAN_POINT ( 'NONE',  ( -10.49297626211726175, 3.650476262117184234, 54.00000000000000711 ) ) ;
#33746 = ORIENTED_EDGE ( 'NONE', *, *, #28567, .T. ) ;
#33747 = VECTOR ( 'NONE', #63352, 1000.000000000000000 ) ;
#33748 = CARTESIAN_POINT ( 'NONE',  ( 6.657023737882815873, 10.30047626211719880, 26.00000000000000711 ) ) ;
#33749 = DIRECTION ( 'NONE',  ( 0.000000000000000000, 0.000000000000000000, 1.000000000000000000 ) ) ;
#33750 = VECTOR ( 'NONE', #46312, 1000.000000000000000 ) ;
#33751 = CARTESIAN_POINT ( 'NONE',  ( -7.250000000000000000, -7.449999999999998401, -24.00000000000000000 ) ) ;
#33752 = ORIENTED_EDGE ( 'NONE', *, *, #17591, .F. ) ;
#33753 = CARTESIAN_POINT ( 'NONE',  ( 11.78648345035337819, -4.406483450353394282, 195.0000000000000284 ) ) ;
#33755 = VECTOR ( 'NONE', #13310, 1000.000000000000000 ) ;
#33754 = AXIS2_PLACEMENT_3D ( 'NONE', #69184, #4493, #62828 ) ;
#33756 = EDGE_CURVE ( 'NONE', #45382, #37614, #69416, .T. ) ;
#33757 = DIRECTION ( 'NONE',  ( 0.000000000000000000, 0.8346456692913387654, 0.5507872608668551440 ) ) ;
#33758 = CARTESIAN_POINT ( 'NONE',  ( -8.250000000000001776, -7.249999999999998224, -26.00000000000001066 ) ) ;
#33759 = ORIENTED_EDGE ( 'NONE', *, *, #5157, .F. ) ;
#33761 = ADVANCED_FACE ( 'NONE', ( #39031 ), #44325, .T. ) ;
#33760 = CARTESIAN_POINT ( 'NONE',  ( 11.50000000000000000, -12.00000000000000000, -11.03137303340310282 ) ) ;
#33762 = AXIS2_PLACEMENT_3D ( 'NONE', #19151, #56635, #30112 ) ;
#33763 = DIRECTION ( 'NONE',  ( -0.000000000000000000, -0.000000000000000000, -1.000000000000000000 ) ) ;
#33764 = LINE ( 'NONE', #67690, #11072 ) ;
#33765 = EDGE_CURVE ( 'NONE', #54840, #27500, #49114, .T. ) ;
#33766 = ADVANCED_FACE ( 'NONE', ( #17122 ), #23110, .T. ) ;
#33767 = ORIENTED_EDGE ( 'NONE', *, *, #14793, .T. ) ;
#33768 = LINE ( 'NONE', #66639, #32066 ) ;
#33769 = EDGE_CURVE ( 'NONE', #24647, #29693, #60934, .T. ) ;
#33770 = EDGE_CURVE ( 'NONE', #19534, #3474, #38352, .T. ) ;
#33771 = FACE_OUTER_BOUND ( 'NONE', #17304, .T. ) ;
#33772 = FILL_AREA_STYLE ('',( #49692 ) ) ;
#33773 = PLANE ( 'NONE',  #50355 ) ;
#33774 = VERTEX_POINT ( 'NONE', #28412 ) ;
#33775 = CARTESIAN_POINT ( 'NONE',  ( -8.750000000000001776, -7.249999999999998224, -26.00000000000001066 ) ) ;
#33776 = DIRECTION ( 'NONE',  ( -3.491481338843133355E-15, -1.000000000000000000, 0.000000000000000000 ) ) ;
#33777 = DIRECTION ( 'NONE',  ( 1.000000000000000000, 5.013651664672856055E-16, 0.000000000000000000 ) ) ;
#33778 = DIRECTION ( 'NONE',  ( -1.011922027653137735E-14, -1.000000000000000000, 0.000000000000000000 ) ) ;
#33779 = CARTESIAN_POINT ( 'NONE',  ( 7.357023737882784076, 3.834182069070697807, 54.00000000000000711 ) ) ;
#33780 = ORIENTED_EDGE ( 'NONE', *, *, #11192, .F. ) ;
#33781 = LINE ( 'NONE', #60664, #29861 ) ;
#33782 = CARTESIAN_POINT ( 'NONE',  ( -11.47551654964677326, -10.20488345035332145, 195.0000000000000284 ) ) ;
#33783 = CARTESIAN_POINT ( 'NONE',  ( 28.90000000000000213, -0.1999999999911795112, 8.826273045769999343E-12 ) ) ;
#33784 = VECTOR ( 'NONE', #12835, 1000.000000000000000 ) ;
#33785 = DIRECTION ( 'NONE',  ( 1.000000000000000000, -0.000000000000000000, -0.000000000000000000 ) ) ;
#33786 = CARTESIAN_POINT ( 'NONE',  ( -3.650476262117223314, 10.30047626211716683, 54.00000000000000711 ) ) ;
#33787 = VECTOR ( 'NONE', #44737, 1000.000000000000000 ) ;
#33788 = ORIENTED_EDGE ( 'NONE', *, *, #5539, .T. ) ;
#33789 = VECTOR ( 'NONE', #22598, 1000.000000000000000 ) ;
#33790 = CARTESIAN_POINT ( 'NONE',  ( -15.50000000000000000, 0.000000000000000000, -18.50000000000000000 ) ) ;
#33791 = DIRECTION ( 'NONE',  ( 1.000000000000000000, -0.000000000000000000, -0.000000000000000000 ) ) ;
#33792 = EDGE_LOOP ( 'NONE', ( #10935, #14334, #16743, #35786, #16257, #61662, #33620, #27740, #12066, #36889, #69334, #42971, #35121, #16760 ) ) ;
#33793 = AXIS2_PLACEMENT_3D ( 'NONE', #53364, #15180, #31092 ) ;
#33794 = DIRECTION ( 'NONE',  ( 0.000000000000000000, 0.000000000000000000, 1.000000000000000000 ) ) ;
#33795 = VERTEX_POINT ( 'NONE', #12156 ) ;
#33796 = VECTOR ( 'NONE', #21071, 1000.000000000000000 ) ;
#33797 = CARTESIAN_POINT ( 'NONE',  ( 30.00000000000000000, 0.000000000000000000, -27.00000000000000000 ) ) ;
#33798 = ORIENTED_EDGE ( 'NONE', *, *, #55674, .F. ) ;
#33799 = ORIENTED_EDGE ( 'NONE', *, *, #62799, .F. ) ;
#33800 = DIRECTION ( 'NONE',  ( 0.000000000000000000, 0.000000000000000000, 1.000000000000000000 ) ) ;
#33801 = DIRECTION ( 'NONE',  ( -0.000000000000000000, -0.000000000000000000, -1.000000000000000000 ) ) ;
#33802 = AXIS2_PLACEMENT_3D ( 'NONE', #58512, #10062, #31634 ) ;
#33803 = CARTESIAN_POINT ( 'NONE',  ( 275.0000000000000000, -28.95000000000155183, -14.49999999999845990 ) ) ;
#33805 = EDGE_CURVE ( 'NONE', #43137, #3378, #26434, .T. ) ;
#33804 = DIRECTION ( 'NONE',  ( -0.000000000000000000, -0.000000000000000000, 1.000000000000000000 ) ) ;
#33806 = VERTEX_POINT ( 'NONE', #47648 ) ;
#33808 = EDGE_CURVE ( 'NONE', #21629, #23669, #49318, .T. ) ;
#33807 = ORIENTED_EDGE ( 'NONE', *, *, #17685, .F. ) ;
#33809 = DIRECTION ( 'NONE',  ( -1.000000000000000000, 0.000000000000000000, -0.000000000000000000 ) ) ;
#33810 = DIRECTION ( 'NONE',  ( 8.659560562354963673E-17, 0.7071067811865450192, -0.7071067811865500152 ) ) ;
#33811 = ORIENTED_EDGE ( 'NONE', *, *, #60362, .T. ) ;
#33812 = EDGE_LOOP ( 'NONE', ( #49552, #26094, #25468, #9946, #52220 ) ) ;
#33813 = ORIENTED_EDGE ( 'NONE', *, *, #26898, .F. ) ;
#33814 = PLANE ( 'NONE',  #55344 ) ;
#33815 = CARTESIAN_POINT ( 'NONE',  ( 30.00000000000000000, -12.00000000000000000, 11.00000000000000000 ) ) ;
#33817 = VERTEX_POINT ( 'NONE', #44668 ) ;
#33816 = LINE ( 'NONE', #45117, #36060 ) ;
#33818 = LINE ( 'NONE', #55405, #42407 ) ;
#33819 = DIRECTION ( 'NONE',  ( -0.000000000000000000, -0.000000000000000000, 1.000000000000000000 ) ) ;
#33820 = AXIS2_PLACEMENT_3D ( 'NONE', #56089, #12584, #12240 ) ;
#33821 = VERTEX_POINT ( 'NONE', #33389 ) ;
#33822 = VERTEX_POINT ( 'NONE', #895 ) ;
#33823 = CARTESIAN_POINT ( 'NONE',  ( 1.000000000000000000, -16.00000000000000000, 0.000000000000000000 ) ) ;
#33824 = DIRECTION ( 'NONE',  ( 0.7071067811865475727, -0.7071067811865475727, 0.000000000000000000 ) ) ;
#33825 = CARTESIAN_POINT ( 'NONE',  ( -17.00000000000000000, -15.50000000000000000, 19.33772233983200195 ) ) ;
#33826 = CIRCLE ( 'NONE', #16947, 0.2999999999998732569 ) ;
#33827 = CIRCLE ( 'NONE', #3366, 1.000000000000000888 ) ;
#33828 = EDGE_CURVE ( 'NONE', #65032, #32370, #22438, .T. ) ;
#33829 = VECTOR ( 'NONE', #33524, 1000.000000000000000 ) ;
#33830 = CARTESIAN_POINT ( 'NONE',  ( 14.24999999999999822, -0.2715193793361405095, 22.01281590054915327 ) ) ;
#33831 = CARTESIAN_POINT ( 'NONE',  ( 280.0000000000000000, -53.81370849898476649, -16.00000000000000711 ) ) ;
#33832 = VERTEX_POINT ( 'NONE', #21133 ) ;
#33833 = ORIENTED_EDGE ( 'NONE', *, *, #31771, .F. ) ;
#33834 = DIRECTION ( 'NONE',  ( -0.000000000000000000, 1.000000000000000000, -0.000000000000000000 ) ) ;
#33835 = AXIS2_PLACEMENT_3D ( 'NONE', #19331, #40897, #14026 ) ;
#33836 = EDGE_CURVE ( 'NONE', #20610, #28387, #12495, .T. ) ;
#33837 = CARTESIAN_POINT ( 'NONE',  ( 7.852485183456931139, -3.430747519065418860, 455.0000000000000568 ) ) ;
#33838 = DIRECTION ( 'NONE',  ( 0.000000000000000000, 0.5625376724249369076, -0.8267716535433071723 ) ) ;
#33839 = EDGE_CURVE ( 'NONE', #44460, #15622, #31750, .T. ) ;
#33840 = DIRECTION ( 'NONE',  ( 0.000000000000000000, 0.000000000000000000, -1.000000000000000000 ) ) ;
#33841 = CIRCLE ( 'NONE', #28203, 24.99999999998794920 ) ;
#33842 = LINE ( 'NONE', #50800, #55673 ) ;
#33844 = VERTEX_POINT ( 'NONE', #59910 ) ;
#33843 = EDGE_CURVE ( 'NONE', #69756, #9056, #64920, .T. ) ;
#33845 = CARTESIAN_POINT ( 'NONE',  ( 7.450000000000003730, -7.249999999999997335, -25.00000000000000000 ) ) ;
#33846 = EDGE_CURVE ( 'NONE', #45355, #9032, #52973, .T. ) ;
#33847 = DIRECTION ( 'NONE',  ( -0.8660254037844347108, 0.5000000000000068834, 2.509347957447884214E-16 ) ) ;
#33848 = LINE ( 'NONE', #8013, #24387 ) ;
#33849 = VECTOR ( 'NONE', #60570, 1000.000000000000000 ) ;
#33850 = LINE ( 'NONE', #17935, #61542 ) ;
#33851 = EDGE_CURVE ( 'NONE', #66073, #24192, #1648, .T. ) ;
#33852 = DIRECTION ( 'NONE',  ( 1.000000000000000000, 0.000000000000000000, 0.000000000000000000 ) ) ;
#33853 = CARTESIAN_POINT ( 'NONE',  ( -7.813516549646789322, -11.78648345035335865, 195.0000000000000284 ) ) ;
#33854 = AXIS2_PLACEMENT_3D ( 'NONE', #48914, #25962, #134 ) ;
#33855 = VECTOR ( 'NONE', #33810, 1000.000000000000000 ) ;
#33856 = DIRECTION ( 'NONE',  ( -1.000000000000000000, 0.000000000000000000, 0.000000000000000000 ) ) ;
#33857 = ORIENTED_EDGE ( 'NONE', *, *, #59973, .F. ) ;
#33858 = DIRECTION ( 'NONE',  ( 1.000000000000000000, 0.000000000000000000, 0.000000000000000000 ) ) ;
#33859 = LINE ( 'NONE', #6983, #21438 ) ;
#33860 = ORIENTED_EDGE ( 'NONE', *, *, #1445, .T. ) ;
#33861 = DIRECTION ( 'NONE',  ( 0.7071067811865460184, 0.000000000000000000, -0.7071067811865489050 ) ) ;
#33862 = PLANE ( 'NONE',  #768 ) ;
#33863 = CARTESIAN_POINT ( 'NONE',  ( -25.50000000000000355, 0.000000000000000000, 20.87899999999999778 ) ) ;
#33864 = LINE ( 'NONE', #44129, #34300 ) ;
#33865 = CARTESIAN_POINT ( 'NONE',  ( -2.355476262117325525, -9.562023737882830332, 54.00000000000000711 ) ) ;
#33866 = ORIENTED_EDGE ( 'NONE', *, *, #46620, .T. ) ;
#33867 = CARTESIAN_POINT ( 'NONE',  ( 24.00000000000000000, -15.50000000000000000, 19.33772233983200195 ) ) ;
#33868 = VERTEX_POINT ( 'NONE', #28085 ) ;
#33869 = VECTOR ( 'NONE', #56430, 1000.000000000000114 ) ;
#33870 = LINE ( 'NONE', #38506, #1733 ) ;
#33871 = ORIENTED_EDGE ( 'NONE', *, *, #50551, .F. ) ;
#33872 = DIRECTION ( 'NONE',  ( 6.308085367188448025E-15, 1.000000000000000000, 3.673940397442059868E-16 ) ) ;
#33873 = CARTESIAN_POINT ( 'NONE',  ( 28.00000000000000000, -16.64230188589299786, -14.64519951917100116 ) ) ;
#33874 = DIRECTION ( 'NONE',  ( 0.6414496315691645689, 0.7671651518152939886, 0.000000000000000000 ) ) ;
#33875 = VERTEX_POINT ( 'NONE', #43656 ) ;
#33876 = ORIENTED_EDGE ( 'NONE', *, *, #18941, .F. ) ;
#33877 = DIRECTION ( 'NONE',  ( 0.000000000000000000, -0.7046037717806115097, 0.7096009616626348659 ) ) ;
#33878 = VECTOR ( 'NONE', #60924, 1000.000000000000000 ) ;
#33879 = EDGE_LOOP ( 'NONE', ( #38468, #11578, #34495, #40600 ) ) ;
#33880 = ORIENTED_EDGE ( 'NONE', *, *, #22280, .T. ) ;
#33881 = CARTESIAN_POINT ( 'NONE',  ( 9.804883450353409913, 11.07551654964657928, 195.0000000000000284 ) ) ;
#33882 = FACE_OUTER_BOUND ( 'NONE', #4656, .T. ) ;
#33884 = CARTESIAN_POINT ( 'NONE',  ( -6.817976262117321440, -9.737023737882781305, 26.00000000000000000 ) ) ;
#33883 = CIRCLE ( 'NONE', #41826, 0.1749999999999998224 ) ;
#33885 = ORIENTED_EDGE ( 'NONE', *, *, #38588, .F. ) ;
#33886 = EDGE_CURVE ( 'NONE', #50749, #29795, #49642, .T. ) ;
#33887 = VECTOR ( 'NONE', #42831, 1000.000000000000000 ) ;
#33888 = EDGE_CURVE ( 'NONE', #67654, #47898, #1217, .T. ) ;
#33889 = CARTESIAN_POINT ( 'NONE',  ( 10.50000000000000178, 9.690000000000001279, 0.000000000000000000 ) ) ;
#33890 = EDGE_CURVE ( 'NONE', #13397, #25678, #18609, .T. ) ;
#33892 = CARTESIAN_POINT ( 'NONE',  ( -2.355476262117313979, -8.835729544836350868, 26.00000000000000711 ) ) ;
#33891 = CARTESIAN_POINT ( 'NONE',  ( 40.90000000000000568, 0.000000000000000000, 5.000000000000000000 ) ) ;
#33893 = ORIENTED_EDGE ( 'NONE', *, *, #55239, .T. ) ;
#33895 = ORIENTED_EDGE ( 'NONE', *, *, #13272, .T. ) ;
#33894 = DIRECTION ( 'NONE',  ( -1.000000000000000000, 0.000000000000000000, 0.000000000000000000 ) ) ;
#33896 = EDGE_LOOP ( 'NONE', ( #5635, #31848, #58528, #7973 ) ) ;
#33897 = ADVANCED_FACE ( 'NONE', ( #61984 ), #24863, .F. ) ;
#33898 = AXIS2_PLACEMENT_3D ( 'NONE', #9097, #52951, #21112 ) ;
#33900 = AXIS2_PLACEMENT_3D ( 'NONE', #64134, #48544, #31257 ) ;
#33899 = CARTESIAN_POINT ( 'NONE',  ( 4.456444791733522252E-16, 7.450000000000002842, -18.50000000000000000 ) ) ;
#33901 = ORIENTED_EDGE ( 'NONE', *, *, #64693, .F. ) ;
#33902 = CARTESIAN_POINT ( 'NONE',  ( -11.50000000000000000, -12.00000000000000000, 11.03137303340310282 ) ) ;
#33903 = ORIENTED_EDGE ( 'NONE', *, *, #60277, .F. ) ;
#33904 = EDGE_LOOP ( 'NONE', ( #45100, #36161, #46475, #66150 ) ) ;
#33905 = VECTOR ( 'NONE', #45576, 1000.000000000000000 ) ;
#33906 = CARTESIAN_POINT ( 'NONE',  ( -30.00000000000000000, -11.85423089348099879, -9.852125413066602277 ) ) ;
#33907 = DIRECTION ( 'NONE',  ( 0.000000000000000000, 0.000000000000000000, 1.000000000000000000 ) ) ;
#33908 = ORIENTED_EDGE ( 'NONE', *, *, #34332, .F. ) ;
#33909 = LINE ( 'NONE', #54121, #56783 ) ;
#33910 = CARTESIAN_POINT ( 'NONE',  ( 8.406483450353379183, -5.668387132715952959, 195.0000000000000284 ) ) ;
#33911 = DIRECTION ( 'NONE',  ( -1.000000000000000000, 0.000000000000000000, 0.000000000000000000 ) ) ;
#33912 = VERTEX_POINT ( 'NONE', #3294 ) ;
#33913 = CARTESIAN_POINT ( 'NONE',  ( 1.000000000000000000, -21.00000000000000000, 0.000000000000000000 ) ) ;
#33914 = AXIS2_PLACEMENT_3D ( 'NONE', #64463, #55828, #16022 ) ;
#33915 = CARTESIAN_POINT ( 'NONE',  ( 73.57321854994619059, 47.95351654967443977, 15.00000000000000000 ) ) ;
#33917 = ORIENTED_EDGE ( 'NONE', *, *, #35131, .T. ) ;
#33916 = CARTESIAN_POINT ( 'NONE',  ( 15.50000000000000000, -0.4000000000000000222, -25.99999999999999645 ) ) ;
#33919 = VERTEX_POINT ( 'NONE', #8592 ) ;
#33918 = LINE ( 'NONE', #7046, #10892 ) ;
#33920 = CARTESIAN_POINT ( 'NONE',  ( 25.50000000000000355, 0.000000000000000000, -20.24999999999999645 ) ) ;
#33921 = CARTESIAN_POINT ( 'NONE',  ( 290.0000000000000000, -42.00000000000000000, 50.00000000000000000 ) ) ;
#33922 = DIRECTION ( 'NONE',  ( 1.000000000000000000, 0.000000000000000000, 0.000000000000000000 ) ) ;
#33923 = CARTESIAN_POINT ( 'NONE',  ( 275.0000000000000000, -25.60000000000000142, 15.10000000000000142 ) ) ;
#33924 = DIRECTION ( 'NONE',  ( 0.000000000000000000, 0.7071067811865074937, 0.7071067811865876518 ) ) ;
#33925 = EDGE_LOOP ( 'NONE', ( #9672, #63450, #1973, #3404 ) ) ;
#33926 = DIRECTION ( 'NONE',  ( 0.000000000000000000, 0.000000000000000000, -1.000000000000000000 ) ) ;
#33927 = CARTESIAN_POINT ( 'NONE',  ( -9.234937905884020637, 9.942044687070460185, 195.0000000000000284 ) ) ;
#33928 = CIRCLE ( 'NONE', #59891, 4.500000000000190958 ) ;
#33929 = EDGE_CURVE ( 'NONE', #43823, #43603, #7545, .T. ) ;
#33930 = DIRECTION ( 'NONE',  ( 0.000000000000000000, 1.000000000000000000, 1.883909694907254982E-12 ) ) ;
#33932 = EDGE_LOOP ( 'NONE', ( #61798, #27547 ) ) ;
#33931 = LINE ( 'NONE', #2119, #31037 ) ;
#33933 = VECTOR ( 'NONE', #10985, 1000.000000000000000 ) ;
#33934 = CARTESIAN_POINT ( 'NONE',  ( -24.00000000000000000, -16.28999999999999915, 14.50000000000000000 ) ) ;
#33935 = EDGE_CURVE ( 'NONE', #60008, #21483, #34763, .T. ) ;
#33936 = ADVANCED_FACE ( 'NONE', ( #13199 ), #46423, .F. ) ;
#33937 = PLANE ( 'NONE',  #44256 ) ;
#33938 = AXIS2_PLACEMENT_3D ( 'NONE', #13776, #13430, #30399 ) ;
#33939 = EDGE_CURVE ( 'NONE', #4203, #44680, #34057, .T. ) ;
#33940 = ORIENTED_EDGE ( 'NONE', *, *, #16073, .T. ) ;
#33941 = CARTESIAN_POINT ( 'NONE',  ( 8.250000000000005329, 0.000000000000000000, -15.00000000000000000 ) ) ;
#33942 = CARTESIAN_POINT ( 'NONE',  ( -6.817976262117261044, 9.722976262117182245, 26.00000000000000711 ) ) ;
#33943 = EDGE_LOOP ( 'NONE', ( #26196, #44482, #65242, #15629 ) ) ;
#33944 = VECTOR ( 'NONE', #62393, 1000.000000000000000 ) ;
#33945 = CARTESIAN_POINT ( 'NONE',  ( -3.650476262117335668, -10.50702373788282173, 54.00000000000000711 ) ) ;
#33946 = LINE ( 'NONE', #20047, #7496 ) ;
#33947 = DIRECTION ( 'NONE',  ( 0.000000000000000000, 0.000000000000000000, 1.000000000000000000 ) ) ;
#33948 = EDGE_CURVE ( 'NONE', #5787, #65641, #29810, .T. ) ;
#33949 = CARTESIAN_POINT ( 'NONE',  ( 0.000000000000000000, 0.000000000000000000, -30.00000000000001066 ) ) ;
#33950 = EDGE_CURVE ( 'NONE', #63093, #24327, #41117, .T. ) ;
#33951 = CIRCLE ( 'NONE', #58821, 4.000000000000001776 ) ;
#33952 = CARTESIAN_POINT ( 'NONE',  ( 275.2500000000000000, -0.2500000000000000000, -26.75000000000000000 ) ) ;
#33953 = ORIENTED_EDGE ( 'NONE', *, *, #45409, .T. ) ;
#33954 = DIRECTION ( 'NONE',  ( 0.000000000000000000, 0.000000000000000000, 1.000000000000000000 ) ) ;
#33955 = ORIENTED_EDGE ( 'NONE', *, *, #2634, .T. ) ;
#33956 = VERTEX_POINT ( 'NONE', #40055 ) ;
#33957 = CARTESIAN_POINT ( 'NONE',  ( 23.50000000000000000, -5.200000000000001066, 22.50000000000000000 ) ) ;
#33958 = AXIS2_PLACEMENT_3D ( 'NONE', #38478, #60025, #66381 ) ;
#33959 = LINE ( 'NONE', #39274, #29734 ) ;
#33960 =( LENGTH_UNIT ( ) NAMED_UNIT ( * ) SI_UNIT ( .MILLI., .METRE. ) );
#33961 = DIRECTION ( 'NONE',  ( 0.000000000000000000, 1.000000000000000000, 0.000000000000000000 ) ) ;
#33962 = ORIENTED_EDGE ( 'NONE', *, *, #36009, .T. ) ;
#33963 = ORIENTED_EDGE ( 'NONE', *, *, #63737, .T. ) ;
#33964 = FACE_OUTER_BOUND ( 'NONE', #57555, .T. ) ;
#33965 = ORIENTED_EDGE ( 'NONE', *, *, #60498, .F. ) ;
#33966 = CARTESIAN_POINT ( 'NONE',  ( 174.0064834503533575, -29.01119750012555443, 5.000000000000000000 ) ) ;
#33967 = DIRECTION ( 'NONE',  ( -0.000000000000000000, 1.000000000000000000, -0.000000000000000000 ) ) ;
#33968 = CIRCLE ( 'NONE', #43017, 1.000000000000000888 ) ;
#33969 = CARTESIAN_POINT ( 'NONE',  ( 176.4833316329832940, 0.000000000000000000, 278.4149360882130395 ) ) ;
#33970 = FILL_AREA_STYLE ('',( #22355 ) ) ;
#33972 = CARTESIAN_POINT ( 'NONE',  ( -11.50000000000000000, -11.50000000000100009, -10.50000000000065903 ) ) ;
#33971 = LINE ( 'NONE', #51291, #26473 ) ;
#33973 = VERTEX_POINT ( 'NONE', #66595 ) ;
#33975 = ORIENTED_EDGE ( 'NONE', *, *, #16558, .F. ) ;
#33974 = DIRECTION ( 'NONE',  ( 0.000000000000000000, 0.7278708115913771204, 0.6857142857147648929 ) ) ;
#33976 = VERTEX_POINT ( 'NONE', #50677 ) ;
#33977 = ORIENTED_EDGE ( 'NONE', *, *, #11516, .F. ) ;
#33978 = EDGE_CURVE ( 'NONE', #36409, #14259, #19204, .T. ) ;
#33979 = DIRECTION ( 'NONE',  ( 0.000000000000000000, 1.000000000000000000, 0.000000000000000000 ) ) ;
#33980 = AXIS2_PLACEMENT_3D ( 'NONE', #68557, #38712, #31437 ) ;
#33981 = VECTOR ( 'NONE', #22212, 1000.000000000000000 ) ;
#33982 = LINE ( 'NONE', #55568, #58000 ) ;
#33983 = AXIS2_PLACEMENT_3D ( 'NONE', #38636, #64476, #59159 ) ;
#33984 = CARTESIAN_POINT ( 'NONE',  ( -8.000000000000000000, 8.000000000000000000, -1.000000000000000000 ) ) ;
#33985 = ORIENTED_EDGE ( 'NONE', *, *, #40714, .T. ) ;
#33986 = ORIENTED_EDGE ( 'NONE', *, *, #14065, .F. ) ;
#33987 = EDGE_CURVE ( 'NONE', #4186, #39384, #562, .T. ) ;
#33988 = DIRECTION ( 'NONE',  ( 0.000000000000000000, 0.000000000000000000, 1.000000000000000000 ) ) ;
#33989 = DIRECTION ( 'NONE',  ( -1.261617073437657735E-14, -1.000000000000000000, 0.000000000000000000 ) ) ;
#33990 = ORIENTED_EDGE ( 'NONE', *, *, #24043, .T. ) ;
#33991 = AXIS2_PLACEMENT_3D ( 'NONE', #33707, #7169, #66237 ) ;
#33992 = VECTOR ( 'NONE', #22517, 1000.000000000000000 ) ;
#33993 = ORIENTED_EDGE ( 'NONE', *, *, #7613, .T. ) ;
#33994 = FACE_OUTER_BOUND ( 'NONE', #66908, .T. ) ;
#33995 = EDGE_CURVE ( 'NONE', #7460, #55486, #50333, .T. ) ;
#33996 = CARTESIAN_POINT ( 'NONE',  ( 9.562023737882805463, 7.955476262117186614, 54.00000000000000711 ) ) ;
#33997 = ORIENTED_EDGE ( 'NONE', *, *, #23443, .T. ) ;
#33998 = AXIS2_PLACEMENT_3D ( 'NONE', #27636, #54178, #27988 ) ;
#33999 = VECTOR ( 'NONE', #19408, 1000.000000000000000 ) ;
#34000 = CARTESIAN_POINT ( 'NONE',  ( -7.250000000000001776, -7.249999999999998224, -18.50000000000000000 ) ) ;
#34002 = ORIENTED_EDGE ( 'NONE', *, *, #38865, .T. ) ;
#34001 = SURFACE_SIDE_STYLE ('',( #45302 ) ) ;
#34003 = EDGE_LOOP ( 'NONE', ( #24379, #51351, #10216, #38533 ) ) ;
#34005 = DIRECTION ( 'NONE',  ( -0.000000000000000000, -0.000000000000000000, -1.000000000000000000 ) ) ;
#34004 = VECTOR ( 'NONE', #485, 1000.000000000000000 ) ;
#34006 = CARTESIAN_POINT ( 'NONE',  ( 25.50000000000000355, -15.50000000000000000, -24.50000000000000000 ) ) ;
#34007 = DIRECTION ( 'NONE',  ( 0.7671651518152998728, -0.6414496315691575745, 2.309356642088859447E-17 ) ) ;
#34008 = CARTESIAN_POINT ( 'NONE',  ( 7.250000000000004441, 7.450000000000001954, -10.50000000000000000 ) ) ;
#34009 = EDGE_CURVE ( 'NONE', #20348, #36958, #45021, .T. ) ;
#34010 = DIRECTION ( 'NONE',  ( -1.000000000000000000, 0.000000000000000000, 0.000000000000000000 ) ) ;
#34011 = CARTESIAN_POINT ( 'NONE',  ( 39.00000000000000000, -5.250000000000000000, 0.000000000000000000 ) ) ;
#34012 = VERTEX_POINT ( 'NONE', #51380 ) ;
#34013 = CARTESIAN_POINT ( 'NONE',  ( 277.3542486889354564, -20.49999999999999645, -17.00000000000000000 ) ) ;
#34015 = VERTEX_POINT ( 'NONE', #67303 ) ;
#34014 = CARTESIAN_POINT ( 'NONE',  ( 52.83090410532631864, 61.65740854044500452, 0.000000000000000000 ) ) ;
#34016 = CARTESIAN_POINT ( 'NONE',  ( 7.250000000000005329, -7.249999999999998224, -23.50000000000000000 ) ) ;
#34017 = CYLINDRICAL_SURFACE ( 'NONE', #7478, 24.99999999998784972 ) ;
#34018 = CIRCLE ( 'NONE', #36302, 0.1999999999999987899 ) ;
#34019 = EDGE_CURVE ( 'NONE', #27626, #24235, #11843, .T. ) ;
#34020 = LINE ( 'NONE', #17776, #48306 ) ;
#34021 = DIRECTION ( 'NONE',  ( 0.000000000000000000, 1.000000000000000000, 0.000000000000000000 ) ) ;
#34022 = FACE_OUTER_BOUND ( 'NONE', #12828, .T. ) ;
#34023 = VERTEX_POINT ( 'NONE', #66938 ) ;
#34024 = EDGE_LOOP ( 'NONE', ( #66955, #12912, #4383, #31122 ) ) ;
#34025 = DIRECTION ( 'NONE',  ( -0.000000000000000000, 3.673940397442059868E-16, -1.000000000000000000 ) ) ;
#34026 = EDGE_CURVE ( 'NONE', #9337, #69324, #61628, .T. ) ;
#34027 = AXIS2_PLACEMENT_3D ( 'NONE', #54568, #11079, #32646 ) ;
#34028 = DIRECTION ( 'NONE',  ( 1.836970198721029934E-16, 1.836970198721010706E-16, -1.000000000000000000 ) ) ;
#34029 = EDGE_CURVE ( 'NONE', #12098, #9916, #2591, .T. ) ;
#34030 = DIRECTION ( 'NONE',  ( -1.000000000000000000, 0.000000000000000000, -0.000000000000000000 ) ) ;
#34031 = VERTEX_POINT ( 'NONE', #56688 ) ;
#34032 = CARTESIAN_POINT ( 'NONE',  ( 7.000000000000000000, -37.14999999999894698, 8.200000000002349410 ) ) ;
#34033 = ORIENTED_EDGE ( 'NONE', *, *, #14647, .T. ) ;
#34034 = ORIENTED_EDGE ( 'NONE', *, *, #10460, .F. ) ;
#34035 = CYLINDRICAL_SURFACE ( 'NONE', #36961, 3.500000000000114131 ) ;
#34036 = FACE_OUTER_BOUND ( 'NONE', #47463, .T. ) ;
#34037 = ORIENTED_EDGE ( 'NONE', *, *, #33888, .F. ) ;
#34038 = CARTESIAN_POINT ( 'NONE',  ( 4.740315990920131561, -7.811466277050838514, 455.0000000000000568 ) ) ;
#34039 = EDGE_CURVE ( 'NONE', #54700, #9609, #24520, .T. ) ;
#34040 = VECTOR ( 'NONE', #44566, 1000.000000000000000 ) ;
#34041 = LINE ( 'NONE', #48593, #68185 ) ;
#34042 = DIRECTION ( 'NONE',  ( 1.000000000000000000, 0.000000000000000000, 0.000000000000000000 ) ) ;
#34043 = ORIENTED_EDGE ( 'NONE', *, *, #11687, .F. ) ;
#34045 = VERTEX_POINT ( 'NONE', #40778 ) ;
#34044 = CARTESIAN_POINT ( 'NONE',  ( -7.250000000000000000, -7.449999999999998401, -18.50000000000000000 ) ) ;
#34046 = DIRECTION ( 'NONE',  ( -1.000000000000000000, 0.000000000000000000, 0.000000000000000000 ) ) ;
#34047 = DIRECTION ( 'NONE',  ( 1.000000000000000000, -0.000000000000000000, 0.000000000000000000 ) ) ;
#34048 = DIRECTION ( 'NONE',  ( 0.000000000000000000, 1.000000000000000000, 0.000000000000000000 ) ) ;
#34049 = CARTESIAN_POINT ( 'NONE',  ( 283.0000000000000568, -21.00000000000000000, -17.50000000000000000 ) ) ;
#34050 = ORIENTED_EDGE ( 'NONE', *, *, #24276, .F. ) ;
#34051 = DIRECTION ( 'NONE',  ( 0.000000000000000000, 0.000000000000000000, -1.000000000000000000 ) ) ;
#34052 = CYLINDRICAL_SURFACE ( 'NONE', #10443, 0.2000000000000005107 ) ;
#34053 = ORIENTED_EDGE ( 'NONE', *, *, #23080, .T. ) ;
#34054 = VERTEX_POINT ( 'NONE', #13901 ) ;
#34055 = EDGE_CURVE ( 'NONE', #66537, #10509, #33324, .T. ) ;
#34056 = VERTEX_POINT ( 'NONE', #53496 ) ;
#34057 = LINE ( 'NONE', #8238, #52505 ) ;
#34058 = DIRECTION ( 'NONE',  ( 1.000000000000000000, 0.000000000000000000, 0.000000000000000000 ) ) ;
#34059 = EDGE_CURVE ( 'NONE', #15670, #58198, #52088, .T. ) ;
#34060 = LINE ( 'NONE', #29469, #24758 ) ;
#34061 = VECTOR ( 'NONE', #13224, 1000.000000000000000 ) ;
#34062 = ORIENTED_EDGE ( 'NONE', *, *, #40140, .T. ) ;
#34063 = ORIENTED_EDGE ( 'NONE', *, *, #52654, .T. ) ;
#34064 = ORIENTED_EDGE ( 'NONE', *, *, #42882, .F. ) ;
#34065 = ADVANCED_FACE ( 'NONE', ( #20603 ), #9304, .T. ) ;
#34066 = DIRECTION ( 'NONE',  ( 0.000000000000000000, 0.000000000000000000, 1.000000000000000000 ) ) ;
#34067 = ORIENTED_EDGE ( 'NONE', *, *, #47197, .T. ) ;
#34068 = EDGE_CURVE ( 'NONE', #32857, #5665, #61556, .T. ) ;
#34069 = ORIENTED_EDGE ( 'NONE', *, *, #42666, .F. ) ;
#34070 = ORIENTED_EDGE ( 'NONE', *, *, #32527, .T. ) ;
#34071 = ORIENTED_EDGE ( 'NONE', *, *, #48011, .F. ) ;
#34072 = CARTESIAN_POINT ( 'NONE',  ( 10.00000000000000000, 21.00000000000000000, -13.98999642601811999 ) ) ;
#34073 = EDGE_CURVE ( 'NONE', #7012, #54514, #47478, .T. ) ;
#34074 = VECTOR ( 'NONE', #67944, 1000.000000000000000 ) ;
#34076 = ORIENTED_EDGE ( 'NONE', *, *, #10398, .T. ) ;
#34075 = CARTESIAN_POINT ( 'NONE',  ( 11.50000000000000000, -11.50000000000000000, 15.00000000000000000 ) ) ;
#34077 = CARTESIAN_POINT ( 'NONE',  ( 7.450000000000004619, -1.336933437520057563E-15, -13.50000000000000178 ) ) ;
#34078 = PRODUCT_DEFINITION_SHAPE ( 'NONE', 'NONE',  #69993 ) ;
#34079 = CARTESIAN_POINT ( 'NONE',  ( -15.50000000000000000, -0.4000000000000000222, 25.99999999999999645 ) ) ;
#34080 = DIRECTION ( 'NONE',  ( 0.000000000000000000, 0.000000000000000000, 1.000000000000000000 ) ) ;
#34081 = EDGE_CURVE ( 'NONE', #14703, #44963, #52445, .T. ) ;
#34083 = ORIENTED_EDGE ( 'NONE', *, *, #38585, .F. ) ;
#34082 = CARTESIAN_POINT ( 'NONE',  ( -4.173516549646669738, 11.77351654964658678, 455.0000000000000568 ) ) ;
#34084 = EDGE_CURVE ( 'NONE', #39125, #14787, #42354, .T. ) ;
#34085 = ADVANCED_FACE ( 'NONE', ( #21315, #52813 ), #69394, .T. ) ;
#34086 = CARTESIAN_POINT ( 'NONE',  ( -11.11351654964671098, 7.793516549646603231, 455.0000000000000568 ) ) ;
#34088 = EDGE_CURVE ( 'NONE', #30792, #11691, #4370, .T. ) ;
#34087 = AXIS2_PLACEMENT_3D ( 'NONE', #61713, #35178, #56757 ) ;
#34089 = ADVANCED_FACE ( 'NONE', ( #57735 ), #19908, .F. ) ;
#34090 = DIRECTION ( 'NONE',  ( -0.8660254037844510311, -0.4999999999999785727, 0.000000000000000000 ) ) ;
#34091 = DIRECTION ( 'NONE',  ( 0.000000000000000000, 0.000000000000000000, 1.000000000000000000 ) ) ;
#34092 = ORIENTED_EDGE ( 'NONE', *, *, #4511, .T. ) ;
#34093 = CIRCLE ( 'NONE', #3637, 1.929199999999997139 ) ;
#34094 = CARTESIAN_POINT ( 'NONE',  ( 9.404523737882753309, 0.9414762621171547385, 54.00000000000000711 ) ) ;
#34095 = EDGE_CURVE ( 'NONE', #31769, #61959, #48187, .T. ) ;
#34096 = FACE_OUTER_BOUND ( 'NONE', #13364, .T. ) ;
#34097 = CARTESIAN_POINT ( 'NONE',  ( 17.00000000000000000, -15.50000000000000000, 19.33772233983200195 ) ) ;
#34098 = EDGE_CURVE ( 'NONE', #46086, #19854, #53159, .T. ) ;
#34099 = VERTEX_POINT ( 'NONE', #42868 ) ;
#34100 = LINE ( 'NONE', #49000, #24531 ) ;
#34101 = VECTOR ( 'NONE', #67532, 1000.000000000000114 ) ;
#34102 = CARTESIAN_POINT ( 'NONE',  ( -6.486996718459931088, 3.142976262117182173, 54.00000000000000711 ) ) ;
#34103 = CARTESIAN_POINT ( 'NONE',  ( 12.90000000000000213, 13.66939075806899950, 20.80000000000000426 ) ) ;
#34104 = ORIENTED_EDGE ( 'NONE', *, *, #58097, .T. ) ;
#34105 = CARTESIAN_POINT ( 'NONE',  ( 9.804883450353379715, -10.20488345035343336, 195.0000000000000284 ) ) ;
#34106 = CARTESIAN_POINT ( 'NONE',  ( 7.250000000000004441, 7.450000000000001954, -12.00000000000000000 ) ) ;
#34107 = EDGE_CURVE ( 'NONE', #27508, #903, #41479, .T. ) ;
#34108 = FACE_OUTER_BOUND ( 'NONE', #54544, .T. ) ;
#34109 = CARTESIAN_POINT ( 'NONE',  ( -3.593516549646776248, -6.006483450353452547, 455.0000000000000568 ) ) ;
#34110 = ADVANCED_FACE ( 'NONE', ( #68713 ), #47141, .F. ) ;
#34111 = ORIENTED_EDGE ( 'NONE', *, *, #7020, .T. ) ;
#34112 = DIRECTION ( 'NONE',  ( 0.000000000000000000, -3.673940397442059868E-16, 1.000000000000000000 ) ) ;
#34113 = DIRECTION ( 'NONE',  ( 1.836970198721029934E-16, 1.836970198721010706E-16, -1.000000000000000000 ) ) ;
#34114 = CARTESIAN_POINT ( 'NONE',  ( 151.5599459900709860, 0.000000000000000000, 326.8892501111512843 ) ) ;
#34115 = CARTESIAN_POINT ( 'NONE',  ( -8.916576262117358098, -9.703773737882734451, 54.00000000000000711 ) ) ;
#34116 = PLANE ( 'NONE',  #17219 ) ;
#34117 = ORIENTED_EDGE ( 'NONE', *, *, #9041, .F. ) ;
#34118 = DIRECTION ( 'NONE',  ( 0.000000000000000000, 0.000000000000000000, -1.000000000000000000 ) ) ;
#34119 = LINE ( 'NONE', #22499, #55356 ) ;
#34120 = AXIS2_PLACEMENT_3D ( 'NONE', #55363, #69879, #28135 ) ;
#34121 = DIRECTION ( 'NONE',  ( -1.000000000000000000, 5.120954910632640039E-15, 1.881408311965255020E-30 ) ) ;
#34122 = CARTESIAN_POINT ( 'NONE',  ( 6.884529946162100345, -21.00000000000000000, -8.000000000000000000 ) ) ;
#34123 = CARTESIAN_POINT ( 'NONE',  ( 11.78648345035337996, 4.393516549646516722, 455.0000000000000568 ) ) ;
#34124 = AXIS2_PLACEMENT_3D ( 'NONE', #22892, #29221, #61393 ) ;
#34125 = ORIENTED_EDGE ( 'NONE', *, *, #34728, .F. ) ;
#34126 = ORIENTED_EDGE ( 'NONE', *, *, #24597, .T. ) ;
#34127 = LINE ( 'NONE', #18934, #66597 ) ;
#34128 = CARTESIAN_POINT ( 'NONE',  ( 8.900000000000005684, -21.00000000000000000, 13.86939075806900057 ) ) ;
#34129 = ORIENTED_EDGE ( 'NONE', *, *, #69768, .F. ) ;
#34130 = CARTESIAN_POINT ( 'NONE',  ( -7.450000000000001954, 7.250000000000000000, -9.500000000000001776 ) ) ;
#34131 = ORIENTED_EDGE ( 'NONE', *, *, #21267, .F. ) ;
#34132 = VECTOR ( 'NONE', #62326, 1000.000000000000000 ) ;
#34133 = DIRECTION ( 'NONE',  ( -1.000000000000000000, 0.000000000000000000, 0.000000000000000000 ) ) ;
#34134 = EDGE_LOOP ( 'NONE', ( #60871, #30890, #3192, #64804 ) ) ;
#34135 = EDGE_LOOP ( 'NONE', ( #22309, #57223, #68500, #15382 ) ) ;
#34136 = CARTESIAN_POINT ( 'NONE',  ( -3.650476262117335668, -10.50702373788282173, 54.00000000000000711 ) ) ;
#34137 = DIRECTION ( 'NONE',  ( 0.000000000000000000, 0.000000000000000000, 1.000000000000000000 ) ) ;
#34138 = ADVANCED_FACE ( 'NONE', ( #63047 ), #4704, .F. ) ;
#34139 = CARTESIAN_POINT ( 'NONE',  ( -9.404046420174124066, 1.853252480934674651, 195.0000000000000284 ) ) ;
#34140 = LINE ( 'NONE', #44405, #43761 ) ;
#34141 = CIRCLE ( 'NONE', #39794, 0.5000000000000000000 ) ;
#34142 = EDGE_LOOP ( 'NONE', ( #28628, #43074, #63790, #18675, #47574, #47580 ) ) ;
#34143 = ORIENTED_EDGE ( 'NONE', *, *, #46694, .T. ) ;
#34144 = ADVANCED_FACE ( 'NONE', ( #26268 ), #4002, .T. ) ;
#34145 = DIRECTION ( 'NONE',  ( 1.000000000000000000, 0.000000000000000000, 0.000000000000000000 ) ) ;
#34146 = VECTOR ( 'NONE', #52583, 1000.000000000000000 ) ;
#34147 = DIRECTION ( 'NONE',  ( -3.717264591378874374E-15, -1.000000000000000000, 0.000000000000000000 ) ) ;
#34148 = ORIENTED_EDGE ( 'NONE', *, *, #29278, .F. ) ;
#34149 = AXIS2_PLACEMENT_3D ( 'NONE', #41444, #14571, #36485 ) ;
#34150 = EDGE_CURVE ( 'NONE', #6078, #2415, #47824, .T. ) ;
#34151 = EDGE_LOOP ( 'NONE', ( #41617, #41653, #2505, #65992, #67631, #6439 ) ) ;
#34152 = VERTEX_POINT ( 'NONE', #22004 ) ;
#34153 = CARTESIAN_POINT ( 'NONE',  ( -7.603567055985545942, 8.393516549646601987, 455.0000000000000568 ) ) ;
#34154 = AXIS2_PLACEMENT_3D ( 'NONE', #7311, #33511, #6968 ) ;
#34155 = EDGE_CURVE ( 'NONE', #25545, #3194, #32623, .T. ) ;
#34157 = ORIENTED_EDGE ( 'NONE', *, *, #60195, .T. ) ;
#34156 = LINE ( 'NONE', #18597, #10791 ) ;
#34158 = DIRECTION ( 'NONE',  ( -0.000000000000000000, -1.000000000000000000, -0.000000000000000000 ) ) ;
#34159 = VECTOR ( 'NONE', #62978, 1000.000000000000000 ) ;
#34160 = DIRECTION ( 'NONE',  ( -1.000000000000000000, 0.000000000000000000, 0.000000000000000000 ) ) ;
#34161 = ORIENTED_EDGE ( 'NONE', *, *, #11503, .F. ) ;
#34162 = ORIENTED_EDGE ( 'NONE', *, *, #58742, .F. ) ;
#34163 = EDGE_CURVE ( 'NONE', #46020, #58177, #44249, .T. ) ;
#34164 = CARTESIAN_POINT ( 'NONE',  ( -30.00000000000000000, -17.35230188589299871, -15.35019951917099945 ) ) ;
#34165 = DIRECTION ( 'NONE',  ( -0.000000000000000000, -0.000000000000000000, 1.000000000000000000 ) ) ;
#34166 = AXIS2_PLACEMENT_3D ( 'NONE', #12535, #33431, #49685 ) ;
#34167 = DIRECTION ( 'NONE',  ( -1.000000000000000000, 0.000000000000000000, 0.000000000000000000 ) ) ;
#34168 = DIRECTION ( 'NONE',  ( 0.000000000000000000, 0.000000000000000000, 1.000000000000000000 ) ) ;
#34169 = CYLINDRICAL_SURFACE ( 'NONE', #60647, 1.000000000000000888 ) ;
#34171 = VERTEX_POINT ( 'NONE', #49567 ) ;
#34170 = CARTESIAN_POINT ( 'NONE',  ( 41.09999999999999432, 13.66939075806899950, -20.80000000000000426 ) ) ;
#34172 = ORIENTED_EDGE ( 'NONE', *, *, #62612, .T. ) ;
#34173 = AXIS2_PLACEMENT_3D ( 'NONE', #31497, #67914, #35730 ) ;
#34174 = CARTESIAN_POINT ( 'NONE',  ( -7.450000000000001954, -7.249999999999998224, -7.500000000000000000 ) ) ;
#34175 = PLANE ( 'NONE',  #29586 ) ;
#34176 = CARTESIAN_POINT ( 'NONE',  ( 7.500000000000000000, -53.81370849898476649, -20.00000000000000000 ) ) ;
#34177 = CYLINDRICAL_SURFACE ( 'NONE', #10313, 0.5000000000004254375 ) ;
#34178 = CARTESIAN_POINT ( 'NONE',  ( -7.250000000000000888, 7.250000000000001776, -22.00000000000000000 ) ) ;
#34179 = ORIENTED_EDGE ( 'NONE', *, *, #15924, .T. ) ;
#34180 = DIRECTION ( 'NONE',  ( 0.000000000000000000, -3.673940397442059868E-16, 1.000000000000000000 ) ) ;
#34181 = DIRECTION ( 'NONE',  ( 3.510749891857827507E-15, 1.000000000000000000, 0.000000000000000000 ) ) ;
#34182 = ADVANCED_FACE ( 'NONE', ( #21664 ), #32269, .F. ) ;
#34183 = CARTESIAN_POINT ( 'NONE',  ( 7.250000000000004441, 7.450000000000001954, -16.50000000000000000 ) ) ;
#34184 = CARTESIAN_POINT ( 'NONE',  ( 7.250000000000004441, 7.450000000000001954, -7.000000000000000000 ) ) ;
#34185 = EDGE_CURVE ( 'NONE', #27132, #32493, #5752, .T. ) ;
#34186 = AXIS2_PLACEMENT_3D ( 'NONE', #63038, #61977, #62675 ) ;
#34187 = CARTESIAN_POINT ( 'NONE',  ( -6.642976262117323394, -9.912023737882783792, 26.00000000000000000 ) ) ;
#34188 = ADVANCED_FACE ( 'NONE', ( #37931 ), #11385, .T. ) ;
#34189 = DIRECTION ( 'NONE',  ( -0.3479852726768751237, 0.000000000000000000, 0.9375000000000004441 ) ) ;
#34190 = VECTOR ( 'NONE', #31983, 1000.000000000000000 ) ;
#34191 = DIRECTION ( 'NONE',  ( -0.7071067811865460184, -0.7071067811865489050, 0.000000000000000000 ) ) ;
#34192 = ORIENTED_EDGE ( 'NONE', *, *, #5494, .F. ) ;
#34193 = DIRECTION ( 'NONE',  ( 0.000000000000000000, 1.000000000000000000, 0.000000000000000000 ) ) ;
#34194 = CARTESIAN_POINT ( 'NONE',  ( -8.821682069070780230, 7.955476262117183062, 54.00000000000000711 ) ) ;
#34195 = EDGE_LOOP ( 'NONE', ( #18956, #60688, #25818, #11182 ) ) ;
#34196 = DIRECTION ( 'NONE',  ( -1.000000000000000000, 0.000000000000000000, 0.000000000000000000 ) ) ;
#34197 = CYLINDRICAL_SURFACE ( 'NONE', #48040, 0.1749999999999998224 ) ;
#34198 = DIRECTION ( 'NONE',  ( 0.000000000000000000, -1.000000000000000000, 0.000000000000000000 ) ) ;
#34199 = FACE_OUTER_BOUND ( 'NONE', #13094, .T. ) ;
#34200 = CARTESIAN_POINT ( 'NONE',  ( 49.00000000000000000, -14.06939075806900163, -20.80000000000000426 ) ) ;
#34201 = ORIENTED_EDGE ( 'NONE', *, *, #28912, .T. ) ;
#34202 = CARTESIAN_POINT ( 'NONE',  ( 7.250000000000005329, -7.249999999999998224, -19.00000000000000000 ) ) ;
#34203 = EDGE_LOOP ( 'NONE', ( #60948, #65705, #35729, #39259 ) ) ;
#34204 = CYLINDRICAL_SURFACE ( 'NONE', #4037, 4.000000000000000000 ) ;
#34205 = ORIENTED_EDGE ( 'NONE', *, *, #21816, .T. ) ;
#34206 = CARTESIAN_POINT ( 'NONE',  ( 7.000000000000000000, -32.95000000000000284, -13.19999999999999929 ) ) ;
#34207 = CIRCLE ( 'NONE', #15068, 24.99999999998784972 ) ;
#34208 = DIRECTION ( 'NONE',  ( -0.000000000000000000, -0.000000000000000000, -1.000000000000000000 ) ) ;
#34209 = PLANE ( 'NONE',  #9706 ) ;
#34210 = ORIENTED_EDGE ( 'NONE', *, *, #19977, .F. ) ;
#34211 = ORIENTED_EDGE ( 'NONE', *, *, #34829, .F. ) ;
#34212 = AXIS2_PLACEMENT_3D ( 'NONE', #9617, #56036, #20564 ) ;
#34213 = LINE ( 'NONE', #17963, #52039 ) ;
#34214 = VERTEX_POINT ( 'NONE', #26969 ) ;
#34215 = VERTEX_POINT ( 'NONE', #1136 ) ;
#34216 = EDGE_CURVE ( 'NONE', #19389, #15739, #48531, .T. ) ;
#34217 = DIRECTION ( 'NONE',  ( -1.000000000000000000, 0.000000000000000000, 0.000000000000000000 ) ) ;
#34218 = CARTESIAN_POINT ( 'NONE',  ( -7.250000000000000888, -8.249999999999998224, -26.00000000000001066 ) ) ;
#34219 = LINE ( 'NONE', #44492, #34348 ) ;
#34220 = ORIENTED_EDGE ( 'NONE', *, *, #19906, .F. ) ;
#34221 = VECTOR ( 'NONE', #49487, 1000.000000000000000 ) ;
#34222 = EDGE_CURVE ( 'NONE', #64750, #15828, #10694, .T. ) ;
#34223 = CARTESIAN_POINT ( 'NONE',  ( 3.664523737882778853, -10.50702373788281285, 54.00000000000000711 ) ) ;
#34225 = DIRECTION ( 'NONE',  ( 0.7071067811865475727, 0.7071067811865475727, -0.000000000000000000 ) ) ;
#34224 = CARTESIAN_POINT ( 'NONE',  ( 6.872275254348383378, 2.989207322240120313, 54.00000000000000711 ) ) ;
#34226 = ORIENTED_EDGE ( 'NONE', *, *, #34084, .F. ) ;
#34228 = ORIENTED_EDGE ( 'NONE', *, *, #14642, .F. ) ;
#34227 = CARTESIAN_POINT ( 'NONE',  ( -3.667976262117228714, 9.722976262117169810, 54.00000000000000711 ) ) ;
#34229 = EDGE_CURVE ( 'NONE', #27219, #15321, #69462, .T. ) ;
#34230 = EDGE_LOOP ( 'NONE', ( #50164, #21480, #5846, #11084 ) ) ;
#34231 = EDGE_CURVE ( 'NONE', #34255, #32932, #22693, .T. ) ;
#34232 =( NAMED_UNIT ( * ) PLANE_ANGLE_UNIT ( ) SI_UNIT ( $, .RADIAN. ) );
#34233 = EDGE_CURVE ( 'NONE', #5501, #21753, #65823, .T. ) ;
#34234 = EDGE_CURVE ( 'NONE', #4514, #65565, #11720, .T. ) ;
#34235 = CARTESIAN_POINT ( 'NONE',  ( 10.20488345035345290, 9.791916549646566992, 455.0000000000000568 ) ) ;
#34236 = ORIENTED_EDGE ( 'NONE', *, *, #61101, .F. ) ;
#34237 = DIRECTION ( 'NONE',  ( 0.000000000000000000, 0.000000000000000000, 1.000000000000000000 ) ) ;
#34238 = AXIS2_PLACEMENT_3D ( 'NONE', #51616, #67877, #13067 ) ;
#34239 = CIRCLE ( 'NONE', #53518, 0.5249999999999990230 ) ;
#34240 = ADVANCED_FACE ( 'NONE', ( #17379 ), #64452, .T. ) ;
#34241 = FACE_OUTER_BOUND ( 'NONE', #24132, .T. ) ;
#34242 = ORIENTED_EDGE ( 'NONE', *, *, #62939, .F. ) ;
#34243 = VERTEX_POINT ( 'NONE', #804 ) ;
#34244 = CIRCLE ( 'NONE', #64765, 2.000000000000001776 ) ;
#34246 = CARTESIAN_POINT ( 'NONE',  ( 11.50000000000000000, -11.50000000000000000, -15.00000000000000000 ) ) ;
#34245 = AXIS2_PLACEMENT_3D ( 'NONE', #7951, #39774, #45432 ) ;
#34247 = VECTOR ( 'NONE', #32273, 999.9999999999998863 ) ;
#34248 = LINE ( 'NONE', #49836, #31206 ) ;
#34249 = ORIENTED_EDGE ( 'NONE', *, *, #7265, .T. ) ;
#34250 = DIRECTION ( 'NONE',  ( 1.836970198721029934E-16, 1.836970198721010706E-16, -1.000000000000000000 ) ) ;
#34251 = DIRECTION ( 'NONE',  ( -1.000000000000000000, 0.000000000000000000, -0.000000000000000000 ) ) ;
#34252 = AXIS2_PLACEMENT_3D ( 'NONE', #69250, #20806, #37089 ) ;
#34253 = VECTOR ( 'NONE', #28803, 1000.000000000000000 ) ;
#34254 = DIRECTION ( 'NONE',  ( 1.000000000000000000, 0.000000000000000000, 0.000000000000000000 ) ) ;
#34255 = VERTEX_POINT ( 'NONE', #43567 ) ;
#34256 = DIRECTION ( 'NONE',  ( 0.000000000000000000, 0.000000000000000000, -1.000000000000000000 ) ) ;
#34257 = DIRECTION ( 'NONE',  ( 0.000000000000000000, -0.7071067811828075644, 0.7071067811902875810 ) ) ;
#34259 = VERTEX_POINT ( 'NONE', #22363 ) ;
#34258 = CARTESIAN_POINT ( 'NONE',  ( -5.993516549646776603, -6.006483450353426790, 455.0000000000000568 ) ) ;
#34261 = EDGE_LOOP ( 'NONE', ( #25842, #29055, #41, #7392 ) ) ;
#34260 = DIRECTION ( 'NONE',  ( 0.000000000000000000, 3.673940397442059868E-16, -1.000000000000000000 ) ) ;
#34262 = LINE ( 'NONE', #6707, #20082 ) ;
#34263 = LINE ( 'NONE', #2108, #48801 ) ;
#34264 = DIRECTION ( 'NONE',  ( -1.000000000000000000, 0.000000000000000000, 0.000000000000000000 ) ) ;
#34265 = DIRECTION ( 'NONE',  ( 1.000000000000000000, 1.671920889371702854E-15, 0.000000000000000000 ) ) ;
#34266 = LINE ( 'NONE', #50887, #43221 ) ;
#34267 = ORIENTED_EDGE ( 'NONE', *, *, #40199, .T. ) ;
#34268 = CARTESIAN_POINT ( 'NONE',  ( 52.83090410532631864, 0.000000000000000000, 0.000000000000000000 ) ) ;
#34269 = FACE_OUTER_BOUND ( 'NONE', #14630, .T. ) ;
#34270 = FACE_OUTER_BOUND ( 'NONE', #68101, .T. ) ;
#34272 = EDGE_LOOP ( 'NONE', ( #36825, #36096, #55826, #15893, #33767, #2180, #61532, #69313, #17031, #66100, #21283, #52057, #15343, #19490, #899, #21161, #19742, #52083 ) ) ;
#34271 = FACE_BOUND ( 'NONE', #10354, .T. ) ;
#34273 = EDGE_CURVE ( 'NONE', #14139, #52552, #38276, .T. ) ;
#34274 = DIRECTION ( 'NONE',  ( 0.000000000000000000, 1.000000000000000000, 0.000000000000000000 ) ) ;
#34275 = EDGE_CURVE ( 'NONE', #58272, #67938, #48885, .T. ) ;
#34276 = LINE ( 'NONE', #12708, #66810 ) ;
#34277 = EDGE_CURVE ( 'NONE', #36987, #41126, #35569, .T. ) ;
#34278 = VERTEX_POINT ( 'NONE', #43089 ) ;
#34279 = CARTESIAN_POINT ( 'NONE',  ( 9.899999999999998579, 13.66939075806899240, 20.79999999999999361 ) ) ;
#34280 = DIRECTION ( 'NONE',  ( 1.836970198721029934E-16, 1.836970198721010706E-16, -1.000000000000000000 ) ) ;
#34282 = ORIENTED_EDGE ( 'NONE', *, *, #31604, .F. ) ;
#34281 = EDGE_CURVE ( 'NONE', #27811, #18655, #18657, .T. ) ;
#34283 = DIRECTION ( 'NONE',  ( 1.000000000000000000, -0.000000000000000000, -0.000000000000000000 ) ) ;
#34284 = DIRECTION ( 'NONE',  ( 0.000000000000000000, 0.7071067811865475727, -0.7071067811865475727 ) ) ;
#34285 = SURFACE_STYLE_FILL_AREA ( #61159 ) ;
#34286 = CARTESIAN_POINT ( 'NONE',  ( 7.250000000000005329, 7.250000000000000888, -11.50000000000000000 ) ) ;
#34287 = ADVANCED_BREP_SHAPE_REPRESENTATION ( '', ( #44073, #45918 ), #6462 ) ;
#34288 = DIRECTION ( 'NONE',  ( -1.000000000000000000, 0.000000000000000000, 0.000000000000000000 ) ) ;
#34289 = VECTOR ( 'NONE', #12624, 1000.000000000000000 ) ;
#34290 = CIRCLE ( 'NONE', #35458, 0.1999999999999992339 ) ;
#34291 = VERTEX_POINT ( 'NONE', #63271 ) ;
#34292 = CARTESIAN_POINT ( 'NONE',  ( 8.580623737882818958, -8.930623737882855906, 54.00000000000000711 ) ) ;
#34293 = ORIENTED_EDGE ( 'NONE', *, *, #32385, .F. ) ;
#34294 = VERTEX_POINT ( 'NONE', #25442 ) ;
#34295 = DIRECTION ( 'NONE',  ( -1.000000000000000000, 1.671920889371702854E-15, 6.142537696789956391E-31 ) ) ;
#34296 = VECTOR ( 'NONE', #53477, 1000.000000000000000 ) ;
#34297 = AXIS2_PLACEMENT_3D ( 'NONE', #55678, #67345, #6882 ) ;
#34298 = FACE_OUTER_BOUND ( 'NONE', #64557, .T. ) ;
#34299 = AXIS2_PLACEMENT_3D ( 'NONE', #56246, #7448, #1800 ) ;
#34300 = VECTOR ( 'NONE', #49101, 1000.000000000000000 ) ;
#34301 = DIRECTION ( 'NONE',  ( -1.836970198721029934E-16, 1.836970198721036590E-16, -1.000000000000000000 ) ) ;
#34302 = ORIENTED_EDGE ( 'NONE', *, *, #50214, .T. ) ;
#34303 = ORIENTED_EDGE ( 'NONE', *, *, #16394, .F. ) ;
#34304 = CARTESIAN_POINT ( 'NONE',  ( -8.227189898828699555, -1.634292677759815904, 54.00000000000000711 ) ) ;
#34305 = ORIENTED_EDGE ( 'NONE', *, *, #30878, .T. ) ;
#34306 = CARTESIAN_POINT ( 'NONE',  ( 4.201500623656003519, -7.272650909786602114, 195.0000000000000284 ) ) ;
#34307 = CARTESIAN_POINT ( 'NONE',  ( 25.50000000000000355, -17.50000000000000000, -22.50000000000000000 ) ) ;
#34308 = DIRECTION ( 'NONE',  ( -0.000000000000000000, -0.000000000000000000, -1.000000000000000000 ) ) ;
#34309 = VECTOR ( 'NONE', #26608, 1000.000000000000000 ) ;
#34310 = CARTESIAN_POINT ( 'NONE',  ( 7.265214908726123078, -5.393625297349927017, 195.0000000000000284 ) ) ;
#34312 = CARTESIAN_POINT ( 'NONE',  ( 39.90000000000000568, 0.000000000000000000, 5.000000000000000000 ) ) ;
#34311 = LINE ( 'NONE', #40337, #42261 ) ;
#34313 = VERTEX_POINT ( 'NONE', #53028 ) ;
#34315 = ORIENTED_EDGE ( 'NONE', *, *, #58057, .F. ) ;
#34314 = PLANE ( 'NONE',  #60092 ) ;
#34316 = ORIENTED_EDGE ( 'NONE', *, *, #13817, .T. ) ;
#34317 = VERTEX_POINT ( 'NONE', #5283 ) ;
#34318 = ADVANCED_FACE ( 'NONE', ( #31464 ), #48056, .F. ) ;
#34319 = CARTESIAN_POINT ( 'NONE',  ( 8.093267424590464998, -8.711985858128690197, 26.00000000000000000 ) ) ;
#34320 = DIRECTION ( 'NONE',  ( 1.000000000000000000, 0.000000000000000000, 0.000000000000000000 ) ) ;
#34321 = EDGE_CURVE ( 'NONE', #64534, #67047, #27718, .T. ) ;
#34322 = DIRECTION ( 'NONE',  ( 1.836970198721029934E-16, 1.836970198721010706E-16, -1.000000000000000000 ) ) ;
#34323 = ORIENTED_EDGE ( 'NONE', *, *, #28920, .F. ) ;
#34324 = VERTEX_POINT ( 'NONE', #14836 ) ;
#34325 = CIRCLE ( 'NONE', #58079, 3.500000000000000444 ) ;
#34326 = DIRECTION ( 'NONE',  ( 1.000000000000000000, -0.000000000000000000, 0.000000000000000000 ) ) ;
#34327 = LINE ( 'NONE', #7470, #54869 ) ;
#34328 = ORIENTED_EDGE ( 'NONE', *, *, #10064, .T. ) ;
#34329 = ORIENTED_EDGE ( 'NONE', *, *, #15717, .F. ) ;
#34330 = FACE_OUTER_BOUND ( 'NONE', #67036, .T. ) ;
#34331 = CARTESIAN_POINT ( 'NONE',  ( 30.00000000000000000, -11.50000000000100009, 15.00000000000084910 ) ) ;
#34333 = ORIENTED_EDGE ( 'NONE', *, *, #57053, .F. ) ;
#34332 = EDGE_CURVE ( 'NONE', #4441, #19992, #19775, .T. ) ;
#34334 = VECTOR ( 'NONE', #11511, 1000.000000000000000 ) ;
#34335 = VECTOR ( 'NONE', #22364, 1000.000000000000000 ) ;
#34336 = LINE ( 'NONE', #35043, #14430 ) ;
#34338 = ORIENTED_EDGE ( 'NONE', *, *, #17453, .F. ) ;
#34337 = LINE ( 'NONE', #12425, #15942 ) ;
#34339 = ORIENTED_EDGE ( 'NONE', *, *, #67493, .T. ) ;
#34340 = CARTESIAN_POINT ( 'NONE',  ( 283.0000000000000568, -25.50000000000000355, 17.00000000000000000 ) ) ;
#34341 = CARTESIAN_POINT ( 'NONE',  ( -5.242976262117259978, 5.242976262117182706, 54.00000000000000711 ) ) ;
#34342 = VECTOR ( 'NONE', #42068, 1000.000000000000000 ) ;
#34343 = VECTOR ( 'NONE', #15702, 1000.000000000000227 ) ;
#34344 = DIRECTION ( 'NONE',  ( 0.6414496315691617934, -0.7671651518152962090, -2.818519042763987834E-16 ) ) ;
#34345 = CYLINDRICAL_SURFACE ( 'NONE', #10917, 0.1999999999999996503 ) ;
#34346 = LINE ( 'NONE', #28711, #50415 ) ;
#34347 = CARTESIAN_POINT ( 'NONE',  ( 32.89999999999999858, 0.000000000000000000, 2.585923194002694273E-15 ) ) ;
#34348 = VECTOR ( 'NONE', #56503, 1000.000000000000000 ) ;
#34349 = DIRECTION ( 'NONE',  ( -0.000000000000000000, 0.000000000000000000, -1.000000000000000000 ) ) ;
#34350 = EDGE_LOOP ( 'NONE', ( #2861, #42865, #69285, #43979 ) ) ;
#34351 = CARTESIAN_POINT ( 'NONE',  ( -30.00000000000000000, -5.599999999999379696, -26.60000000000059828 ) ) ;
#34353 = ORIENTED_EDGE ( 'NONE', *, *, #30254, .F. ) ;
#34352 = CARTESIAN_POINT ( 'NONE',  ( 10.31452373788281562, -3.664523737882826815, 54.00000000000000711 ) ) ;
#34354 = FACE_OUTER_BOUND ( 'NONE', #52132, .T. ) ;
#34355 = CYLINDRICAL_SURFACE ( 'NONE', #26690, 1.000000000000000888 ) ;
#34356 = CARTESIAN_POINT ( 'NONE',  ( 15.00000000000000000, -26.28355339059299922, 9.766446609406699508 ) ) ;
#34357 = VECTOR ( 'NONE', #41730, 1000.000000000000000 ) ;
#34358 = CARTESIAN_POINT ( 'NONE',  ( -10.03972626211722918, 9.689726262117183353, 26.00000000000000711 ) ) ;
#34359 = CARTESIAN_POINT ( 'NONE',  ( -7.450000000000001954, -7.249999999999998224, -21.00000000000000000 ) ) ;
#34360 = ORIENTED_EDGE ( 'NONE', *, *, #62511, .T. ) ;
#34362 = ORIENTED_EDGE ( 'NONE', *, *, #65506, .F. ) ;
#34361 = EDGE_CURVE ( 'NONE', #33331, #56963, #37111, .T. ) ;
#34363 = FACE_OUTER_BOUND ( 'NONE', #37813, .T. ) ;
#34364 = DIRECTION ( 'NONE',  ( -1.794541526872559352E-16, -1.000000000000000000, 0.000000000000000000 ) ) ;
#34365 = FACE_OUTER_BOUND ( 'NONE', #14520, .T. ) ;
#34366 = VERTEX_POINT ( 'NONE', #47705 ) ;
#34367 = CARTESIAN_POINT ( 'NONE',  ( 11.00000000000000000, -8.959999999999999076, 17.04524521594300523 ) ) ;
#34368 = VERTEX_POINT ( 'NONE', #4925 ) ;
#34369 = EDGE_LOOP ( 'NONE', ( #51674, #13714, #1773, #46649 ) ) ;
#34370 = CARTESIAN_POINT ( 'NONE',  ( 7.969523737882818537, -9.562023737882819674, 54.00000000000000711 ) ) ;
#34371 = CARTESIAN_POINT ( 'NONE',  ( -9.915476262117200790, -0.9555237378827209360, 54.00000000000000711 ) ) ;
#34373 = VERTEX_POINT ( 'NONE', #30746 ) ;
#34372 = ADVANCED_FACE ( 'NONE', ( #26847 ), #42748, .F. ) ;
#34374 = DIRECTION ( 'NONE',  ( 0.000000000000000000, 0.000000000000000000, 1.000000000000000000 ) ) ;
#34375 = VECTOR ( 'NONE', #21450, 1000.000000000000000 ) ;
#34376 = LINE ( 'NONE', #55970, #34296 ) ;
#34377 = ADVANCED_FACE ( 'NONE', ( #68926 ), #64325, .F. ) ;
#34378 = DIRECTION ( 'NONE',  ( 0.000000000000000000, 0.000000000000000000, 1.000000000000000000 ) ) ;
#34379 = EDGE_LOOP ( 'NONE', ( #57826, #65883, #52905, #36233 ) ) ;
#34380 = ORIENTED_EDGE ( 'NONE', *, *, #60966, .T. ) ;
#34382 = ORIENTED_EDGE ( 'NONE', *, *, #31913, .F. ) ;
#34381 = FACE_OUTER_BOUND ( 'NONE', #42797, .T. ) ;
#34383 = ORIENTED_EDGE ( 'NONE', *, *, #22268, .T. ) ;
#34384 = VECTOR ( 'NONE', #66806, 1000.000000000000000 ) ;
#34385 = AXIS2_PLACEMENT_3D ( 'NONE', #42441, #5670, #10970 ) ;
#34386 = LINE ( 'NONE', #28747, #26956 ) ;
#34387 = CARTESIAN_POINT ( 'NONE',  ( 4.961189459950039904, -7.357023737882821379, 54.00000000000000711 ) ) ;
#34388 = DIRECTION ( 'NONE',  ( 0.000000000000000000, -1.000000000000000000, -0.000000000000000000 ) ) ;
#34389 = LINE ( 'NONE', #61620, #60154 ) ;
#34390 = CARTESIAN_POINT ( 'NONE',  ( -8.393516549646779623, -6.344579767990844665, 455.0000000000000568 ) ) ;
#34391 =( GEOMETRIC_REPRESENTATION_CONTEXT ( 3 ) GLOBAL_UNCERTAINTY_ASSIGNED_CONTEXT ( ( #4800 ) ) GLOBAL_UNIT_ASSIGNED_CONTEXT ( ( #66052, #14680, #39190 ) ) REPRESENTATION_CONTEXT ( 'NONE', 'WORKASPACE' ) );
#34392 = PLANE ( 'NONE',  #44290 ) ;
#34393 = ORIENTED_EDGE ( 'NONE', *, *, #9526, .F. ) ;
#34394 = VERTEX_POINT ( 'NONE', #63629 ) ;
#34396 = VERTEX_POINT ( 'NONE', #47004 ) ;
#34395 = AXIS2_PLACEMENT_3D ( 'NONE', #4526, #69578, #6528 ) ;
#34397 = CARTESIAN_POINT ( 'NONE',  ( 280.0000000000000000, -20.49999999999999645, -20.00000000000000000 ) ) ;
#34398 = DIRECTION ( 'NONE',  ( 0.000000000000000000, 0.000000000000000000, 1.000000000000000000 ) ) ;
#34400 = EDGE_CURVE ( 'NONE', #34593, #14316, #36759, .T. ) ;
#34399 = LINE ( 'NONE', #39033, #33784 ) ;
#34401 = EDGE_CURVE ( 'NONE', #14513, #60332, #15880, .T. ) ;
#34402 = VECTOR ( 'NONE', #32295, 1000.000000000000000 ) ;
#34403 = EDGE_LOOP ( 'NONE', ( #34393, #42414, #51895, #17103 ) ) ;
#34404 = VERTEX_POINT ( 'NONE', #9177 ) ;
#34405 = EDGE_CURVE ( 'NONE', #3671, #62585, #68581, .T. ) ;
#34406 = VERTEX_POINT ( 'NONE', #25803 ) ;
#34407 = VECTOR ( 'NONE', #49937, 1000.000000000000000 ) ;
#34408 = CARTESIAN_POINT ( 'NONE',  ( -9.828310488886053520, 1.677516549646603794, 195.0000000000000284 ) ) ;
#34409 = ORIENTED_EDGE ( 'NONE', *, *, #42128, .F. ) ;
#34410 = EDGE_CURVE ( 'NONE', #52575, #43309, #10227, .T. ) ;
#34411 = ORIENTED_EDGE ( 'NONE', *, *, #5633, .T. ) ;
#34413 = ORIENTED_EDGE ( 'NONE', *, *, #22845, .T. ) ;
#34412 = EDGE_CURVE ( 'NONE', #13299, #55616, #47353, .T. ) ;
#34414 = ORIENTED_EDGE ( 'NONE', *, *, #60597, .T. ) ;
#34415 = LINE ( 'NONE', #1560, #1169 ) ;
#34416 = EDGE_CURVE ( 'NONE', #43499, #5667, #59010, .T. ) ;
#34418 = ORIENTED_EDGE ( 'NONE', *, *, #61297, .T. ) ;
#34417 = CYLINDRICAL_SURFACE ( 'NONE', #42444, 1.929199999999998028 ) ;
#34419 = ADVANCED_FACE ( 'NONE', ( #16220 ), #31767, .F. ) ;
#34420 = CARTESIAN_POINT ( 'NONE',  ( 10.00000000000000000, 18.00000000000000355, -21.00000000000000000 ) ) ;
#34421 = DIRECTION ( 'NONE',  ( -1.000000000000000000, 0.000000000000000000, 0.000000000000000000 ) ) ;
#34422 = DIRECTION ( 'NONE',  ( 0.000000000000000000, 0.000000000000000000, 1.000000000000000000 ) ) ;
#34424 = VERTEX_POINT ( 'NONE', #25401 ) ;
#34423 = CARTESIAN_POINT ( 'NONE',  ( -9.547976262117304103, -8.144523737882758851, 54.00000000000000711 ) ) ;
#34425 = ORIENTED_EDGE ( 'NONE', *, *, #1433, .T. ) ;
#34426 = VECTOR ( 'NONE', #63024, 1000.000000000000114 ) ;
#34427 = CARTESIAN_POINT ( 'NONE',  ( -25.50000000000000355, -5.578999999999999737, 20.87900000000000134 ) ) ;
#34428 = CARTESIAN_POINT ( 'NONE',  ( 30.00000000000000000, -9.487228132326899654, 12.50000000000000000 ) ) ;
#34429 = DIRECTION ( 'NONE',  ( -1.000000000000000000, 0.000000000000000000, 0.000000000000000000 ) ) ;
#34430 = ORIENTED_EDGE ( 'NONE', *, *, #54332, .F. ) ;
#34431 = FACE_BOUND ( 'NONE', #11460, .T. ) ;
#34432 = VECTOR ( 'NONE', #50772, 1000.000000000000000 ) ;
#34433 = AXIS2_PLACEMENT_3D ( 'NONE', #31798, #9884, #43424 ) ;
#34435 = DIRECTION ( 'NONE',  ( -0.6414496315691415873, 0.7671651518153131954, 2.309356642089129694E-17 ) ) ;
#34434 = VECTOR ( 'NONE', #54708, 1000.000000000000000 ) ;
#34436 = DIRECTION ( 'NONE',  ( 0.4998444328988824181, 0.000000000000000000, -0.8661152018640445593 ) ) ;
#34437 = ADVANCED_FACE ( 'NONE', ( #32100 ), #59318, .F. ) ;
#34438 = VERTEX_POINT ( 'NONE', #46959 ) ;
#34439 = DIRECTION ( 'NONE',  ( 1.570596175624152093E-15, -1.000000000000000000, 0.000000000000000000 ) ) ;
#34440 = AXIS2_PLACEMENT_3D ( 'NONE', #34926, #19715, #3478 ) ;
#34441 = AXIS2_PLACEMENT_3D ( 'NONE', #29803, #25210, #18485 ) ;
#34442 = FACE_OUTER_BOUND ( 'NONE', #4533, .T. ) ;
#34443 = CARTESIAN_POINT ( 'NONE',  ( -7.250000000000000888, 7.450000000000003730, -19.50000000000000000 ) ) ;
#34444 = EDGE_CURVE ( 'NONE', #41049, #49618, #13053, .T. ) ;
#34445 = ORIENTED_EDGE ( 'NONE', *, *, #27702, .F. ) ;
#34446 = AXIS2_PLACEMENT_3D ( 'NONE', #6441, #5417, #43220 ) ;
#34447 = PLANE ( 'NONE',  #49402 ) ;
#34448 = LINE ( 'NONE', #7592, #60264 ) ;
#34449 =( LENGTH_UNIT ( ) NAMED_UNIT ( * ) SI_UNIT ( .MILLI., .METRE. ) );
#34450 = CARTESIAN_POINT ( 'NONE',  ( 40.90000000000000568, 0.000000000000000000, 3.447897592003593022E-15 ) ) ;
#34451 = CIRCLE ( 'NONE', #42412, 0.7499999999999997780 ) ;
#34452 = EDGE_LOOP ( 'NONE', ( #53774, #28291, #26864, #3202 ) ) ;
#34453 = DIRECTION ( 'NONE',  ( 1.836970198721029934E-16, 1.836970198721010706E-16, -1.000000000000000000 ) ) ;
#34454 = DIRECTION ( 'NONE',  ( -0.000000000000000000, -0.000000000000000000, 1.000000000000000000 ) ) ;
#34455 = CARTESIAN_POINT ( 'NONE',  ( -10.30047626211725031, -3.857023737882713466, 54.00000000000000711 ) ) ;
#34456 = COLOUR_RGB ( '', 0.31764706, 0.68627451, 0.89019608) ;
#34457 = CARTESIAN_POINT ( 'NONE',  ( 0.000000000000000000, 8.750000000000001776, -30.00000000000001066 ) ) ;
#34458 = FACE_OUTER_BOUND ( 'NONE', #66807, .T. ) ;
#34459 = ORIENTED_EDGE ( 'NONE', *, *, #23038, .T. ) ;
#34460 = CARTESIAN_POINT ( 'NONE',  ( 283.0000000000000568, -25.50000000000000355, -14.74860679774999994 ) ) ;
#34461 = CARTESIAN_POINT ( 'NONE',  ( 10.00000000000000000, -18.00000000000000355, -21.00000000000000000 ) ) ;
#34462 = DIRECTION ( 'NONE',  ( 0.000000000000000000, 0.000000000000000000, -1.000000000000000000 ) ) ;
#34463 = LINE ( 'NONE', #52149, #418 ) ;
#34464 = EDGE_CURVE ( 'NONE', #51045, #25235, #9851, .T. ) ;
#34465 = FACE_OUTER_BOUND ( 'NONE', #8045, .T. ) ;
#34466 = ORIENTED_EDGE ( 'NONE', *, *, #5872, .T. ) ;
#34468 = ORIENTED_EDGE ( 'NONE', *, *, #60590, .F. ) ;
#34467 = FACE_OUTER_BOUND ( 'NONE', #25155, .T. ) ;
#34469 = DIRECTION ( 'NONE',  ( -0.5000000000000049960, -0.8660254037844358210, -6.723777587268365305E-17 ) ) ;
#34470 = DIRECTION ( 'NONE',  ( 1.047444401652940007E-14, 1.000000000000000000, 1.836970198721029934E-16 ) ) ;
#34472 = VERTEX_POINT ( 'NONE', #31424 ) ;
#34471 = EDGE_CURVE ( 'NONE', #28850, #40508, #41659, .T. ) ;
#34473 = AXIS2_PLACEMENT_3D ( 'NONE', #5259, #26826, #43070 ) ;
#34474 = EDGE_CURVE ( 'NONE', #32122, #40849, #69510, .T. ) ;
#34475 = CARTESIAN_POINT ( 'NONE',  ( 283.0000000000000568, -26.42999999999999972, 9.412893218813501051 ) ) ;
#34476 = EDGE_CURVE ( 'NONE', #26023, #15117, #20099, .T. ) ;
#34477 = VECTOR ( 'NONE', #27539, 1000.000000000000000 ) ;
#34478 = ORIENTED_EDGE ( 'NONE', *, *, #17230, .F. ) ;
#34479 = EDGE_CURVE ( 'NONE', #14683, #24763, #69236, .T. ) ;
#34480 = EDGE_CURVE ( 'NONE', #701, #57822, #26453, .T. ) ;
#34481 = AXIS2_PLACEMENT_3D ( 'NONE', #51172, #2730, #56822 ) ;
#34482 = PLANE ( 'NONE',  #65073 ) ;
#34483 = ORIENTED_EDGE ( 'NONE', *, *, #45139, .F. ) ;
#34484 = ORIENTED_EDGE ( 'NONE', *, *, #49525, .T. ) ;
#34485 = CARTESIAN_POINT ( 'NONE',  ( 105.8309041053263257, 3.657408540445008960, 10.00000000000000000 ) ) ;
#34486 = CARTESIAN_POINT ( 'NONE',  ( 5.257023737882807524, 7.172176262117201162, 54.00000000000000711 ) ) ;
#34487 = EDGE_CURVE ( 'NONE', #50215, #12761, #6315, .T. ) ;
#34488 = CARTESIAN_POINT ( 'NONE',  ( -7.793516549646712477, 11.31351654964660014, 455.0000000000000568 ) ) ;
#34489 = CARTESIAN_POINT ( 'NONE',  ( 15.50000000000000000, 998.9628421096749662, -22.50000000000000000 ) ) ;
#34490 = VECTOR ( 'NONE', #68017, 1000.000000000000000 ) ;
#34491 = CIRCLE ( 'NONE', #44688, 1.000000000000000000 ) ;
#34492 = AXIS2_PLACEMENT_3D ( 'NONE', #37595, #60177, #11731 ) ;
#34493 = EDGE_CURVE ( 'NONE', #43115, #41827, #37758, .T. ) ;
#34494 = ORIENTED_EDGE ( 'NONE', *, *, #36821, .T. ) ;
#34495 = ORIENTED_EDGE ( 'NONE', *, *, #48959, .F. ) ;
#34496 = PLANE ( 'NONE',  #9806 ) ;
#34497 = EDGE_CURVE ( 'NONE', #2339, #64155, #53726, .T. ) ;
#34498 = CARTESIAN_POINT ( 'NONE',  ( -4.135079735113166954, 3.663616288757006512, 54.00000000000000711 ) ) ;
#34499 = VECTOR ( 'NONE', #16550, 1000.000000000000000 ) ;
#34500 = AXIS2_PLACEMENT_3D ( 'NONE', #27818, #16162, #11875 ) ;
#34501 = VECTOR ( 'NONE', #30780, 1000.000000000000000 ) ;
#34502 = EDGE_LOOP ( 'NONE', ( #48884, #46393, #16639, #56840 ) ) ;
#34503 = ORIENTED_EDGE ( 'NONE', *, *, #22905, .F. ) ;
#34504 = ORIENTED_EDGE ( 'NONE', *, *, #23179, .T. ) ;
#34505 = VECTOR ( 'NONE', #18249, 1000.000000000000000 ) ;
#34506 = DIRECTION ( 'NONE',  ( 0.000000000000000000, -0.000000000000000000, -1.000000000000000000 ) ) ;
#34507 = ADVANCED_FACE ( 'NONE', ( #32464 ), #31056, .T. ) ;
#34509 = ORIENTED_EDGE ( 'NONE', *, *, #36210, .F. ) ;
#34508 = CARTESIAN_POINT ( 'NONE',  ( 11.50000000000000000, -11.70000000000012008, -11.00000000000000000 ) ) ;
#34510 = EDGE_CURVE ( 'NONE', #28681, #20324, #15506, .T. ) ;
#34511 = DIRECTION ( 'NONE',  ( -0.000000000000000000, -0.000000000000000000, -1.000000000000000000 ) ) ;
#34512 = VECTOR ( 'NONE', #49456, 1000.000000000000000 ) ;
#34513 = CARTESIAN_POINT ( 'NONE',  ( 11.19000000000000128, -12.00000000000000000, -4.250000000000000000 ) ) ;
#34514 = ORIENTED_EDGE ( 'NONE', *, *, #68540, .F. ) ;
#34515 = PRESENTATION_LAYER_ASSIGNMENT (  '', '', ( #62800 ) ) ;
#34516 = ORIENTED_EDGE ( 'NONE', *, *, #57417, .F. ) ;
#34517 = DIRECTION ( 'NONE',  ( 0.000000000000000000, 1.000000000000000000, 0.000000000000000000 ) ) ;
#34518 = FACE_OUTER_BOUND ( 'NONE', #35462, .T. ) ;
#34519 = DIRECTION ( 'NONE',  ( 0.000000000000000000, -1.000000000000000000, 0.000000000000000000 ) ) ;
#34520 = DIRECTION ( 'NONE',  ( 0.000000000000000000, 0.000000000000000000, -1.000000000000000000 ) ) ;
#34521 = DIRECTION ( 'NONE',  ( 1.000000000000000000, 0.000000000000000000, 0.000000000000000000 ) ) ;
#34522 = VECTOR ( 'NONE', #23504, 1000.000000000000000 ) ;
#34523 = ORIENTED_EDGE ( 'NONE', *, *, #66667, .T. ) ;
#34524 = ORIENTED_EDGE ( 'NONE', *, *, #18513, .F. ) ;
#34525 = DIRECTION ( 'NONE',  ( 1.920885163218982051E-15, 1.000000000000000000, 1.836970198721033139E-16 ) ) ;
#34526 = CARTESIAN_POINT ( 'NONE',  ( 7.450000000000003730, -7.249999999999997335, -21.50000000000000000 ) ) ;
#34527 = AXIS2_PLACEMENT_3D ( 'NONE', #59974, #48336, #54686 ) ;
#34528 = CARTESIAN_POINT ( 'NONE',  ( 22.90000000000000213, 20.60000000000000142, 13.86939075806900057 ) ) ;
#34529 = ADVANCED_FACE ( 'NONE', ( #42012 ), #47315, .T. ) ;
#34530 = VECTOR ( 'NONE', #46138, 1000.000000000000114 ) ;
#34531 = DIRECTION ( 'NONE',  ( -1.000000000000000000, 0.000000000000000000, 0.000000000000000000 ) ) ;
#34532 = ORIENTED_EDGE ( 'NONE', *, *, #61992, .F. ) ;
#34533 = DIRECTION ( 'NONE',  ( 0.000000000000000000, 0.000000000000000000, 1.000000000000000000 ) ) ;
#34534 = LINE ( 'NONE', #13329, #24824 ) ;
#34535 = EDGE_CURVE ( 'NONE', #55973, #46792, #64287, .T. ) ;
#34536 = DIRECTION ( 'NONE',  ( 0.000000000000000000, 0.000000000000000000, 1.000000000000000000 ) ) ;
#34537 = AXIS2_PLACEMENT_3D ( 'NONE', #58120, #57766, #47509 ) ;
#34538 = VECTOR ( 'NONE', #37363, 1000.000000000000000 ) ;
#34539 = CONICAL_SURFACE ( 'NONE', #67327, 3.233000000000000096, 0.7853981633974362886 ) ;
#34540 = LINE ( 'NONE', #34886, #2165 ) ;
#34541 = DIRECTION ( 'NONE',  ( 1.000000000000000000, -0.000000000000000000, 0.000000000000000000 ) ) ;
#34542 = EDGE_CURVE ( 'NONE', #24957, #56406, #53337, .T. ) ;
#34543 = VECTOR ( 'NONE', #4813, 1000.000000000000000 ) ;
#34544 = VECTOR ( 'NONE', #16342, 1000.000000000000114 ) ;
#34545 = AXIS2_PLACEMENT_3D ( 'NONE', #61102, #50845, #50512 ) ;
#34546 = DIRECTION ( 'NONE',  ( -1.000000000000000000, 0.000000000000000000, 0.000000000000000000 ) ) ;
#34547 = ORIENTED_EDGE ( 'NONE', *, *, #8787, .F. ) ;
#34548 = LINE ( 'NONE', #56134, #28696 ) ;
#34549 = EDGE_CURVE ( 'NONE', #55545, #67463, #5242, .T. ) ;
#34550 = DIRECTION ( 'NONE',  ( 5.120954910632640039E-15, 1.000000000000000000, -0.000000000000000000 ) ) ;
#34551 = ORIENTED_EDGE ( 'NONE', *, *, #14879, .F. ) ;
#34552 = DIRECTION ( 'NONE',  ( -1.000000000000000000, 0.000000000000000000, 0.000000000000000000 ) ) ;
#34553 = FACE_OUTER_BOUND ( 'NONE', #33925, .T. ) ;
#34554 = AXIS2_PLACEMENT_3D ( 'NONE', #23489, #56011, #45041 ) ;
#34555 = DIRECTION ( 'NONE',  ( -1.000000000000000000, 0.000000000000000000, 0.000000000000000000 ) ) ;
#34556 = DIRECTION ( 'NONE',  ( 0.000000000000000000, 0.000000000000000000, 1.000000000000000000 ) ) ;
#34557 = EDGE_CURVE ( 'NONE', #35196, #24794, #55969, .T. ) ;
#34558 = CARTESIAN_POINT ( 'NONE',  ( -18.85410196625000268, -15.50000000000000000, -21.50000000000000000 ) ) ;
#34559 = VERTEX_POINT ( 'NONE', #60003 ) ;
#34560 = DIRECTION ( 'NONE',  ( 1.000000000000000000, -0.000000000000000000, 0.000000000000000000 ) ) ;
#34561 = AXIS2_PLACEMENT_3D ( 'NONE', #29836, #35482, #18890 ) ;
#34562 = ORIENTED_EDGE ( 'NONE', *, *, #60157, .T. ) ;
#34563 = CARTESIAN_POINT ( 'NONE',  ( -24.00000000000000000, -17.00000000000000000, 15.70499999999969809 ) ) ;
#34564 = EDGE_LOOP ( 'NONE', ( #10081, #15933, #13629, #65890 ) ) ;
#34565 = LINE ( 'NONE', #18300, #5462 ) ;
#34566 = ADVANCED_FACE ( 'NONE', ( #28176 ), #49746, .T. ) ;
#34567 = EDGE_CURVE ( 'NONE', #19600, #28340, #5582, .T. ) ;
#34568 = EDGE_CURVE ( 'NONE', #414, #22030, #10804, .T. ) ;
#34569 = DIRECTION ( 'NONE',  ( 0.000000000000000000, 0.000000000000000000, 1.000000000000000000 ) ) ;
#34570 = CARTESIAN_POINT ( 'NONE',  ( -9.791916549646712653, 10.19191654964664018, 195.0000000000000284 ) ) ;
#34571 = VERTEX_POINT ( 'NONE', #27487 ) ;
#34572 = ORIENTED_EDGE ( 'NONE', *, *, #3440, .T. ) ;
#34573 = DIRECTION ( 'NONE',  ( -1.000000000000000000, 0.000000000000000000, 0.000000000000000000 ) ) ;
#34574 = VERTEX_POINT ( 'NONE', #66358 ) ;
#34575 = ORIENTED_EDGE ( 'NONE', *, *, #44102, .F. ) ;
#34576 = EDGE_CURVE ( 'NONE', #32493, #49918, #54712, .T. ) ;
#34577 = FACE_OUTER_BOUND ( 'NONE', #55733, .T. ) ;
#34578 = LINE ( 'NONE', #40590, #44908 ) ;
#34579 = DIRECTION ( 'NONE',  ( 0.000000000000000000, 0.000000000000000000, 1.000000000000000000 ) ) ;
#34580 = MECHANICAL_DESIGN_GEOMETRIC_PRESENTATION_REPRESENTATION (  '', ( #15429 ), #16541 ) ;
#34581 = EDGE_LOOP ( 'NONE', ( #38195, #15262, #8418, #46076 ) ) ;
#34582 = CARTESIAN_POINT ( 'NONE',  ( 20.90000000000000213, 0.000000000000000000, 1.292961597001347137E-15 ) ) ;
#34584 = CARTESIAN_POINT ( 'NONE',  ( 0.5000000000000000000, 18.00000000000000355, 21.00000000000000000 ) ) ;
#34583 = DIRECTION ( 'NONE',  ( 0.000000000000000000, 0.000000000000000000, 1.000000000000000000 ) ) ;
#34585 = EDGE_LOOP ( 'NONE', ( #40774, #24054, #51912, #45745, #13281, #37952, #28180, #18212 ) ) ;
#34587 = ORIENTED_EDGE ( 'NONE', *, *, #1072, .T. ) ;
#34586 = DIRECTION ( 'NONE',  ( -0.000000000000000000, -0.000000000000000000, -1.000000000000000000 ) ) ;
#34588 = ORIENTED_EDGE ( 'NONE', *, *, #5347, .F. ) ;
#34589 = AXIS2_PLACEMENT_3D ( 'NONE', #3515, #68572, #40980 ) ;
#34590 = AXIS2_PLACEMENT_3D ( 'NONE', #68643, #20192, #41753 ) ;
#34591 = CARTESIAN_POINT ( 'NONE',  ( 7.500000000000000000, -53.81370849898476649, -20.00000000000000000 ) ) ;
#34592 = EDGE_CURVE ( 'NONE', #22518, #68972, #981, .T. ) ;
#34593 = VERTEX_POINT ( 'NONE', #12245 ) ;
#34594 = EDGE_CURVE ( 'NONE', #29779, #47728, #48063, .T. ) ;
#34595 = AXIS2_PLACEMENT_3D ( 'NONE', #46453, #15337, #14293 ) ;
#34596 = AXIS2_PLACEMENT_3D ( 'NONE', #13779, #62556, #34986 ) ;
#34597 = AXIS2_PLACEMENT_3D ( 'NONE', #53420, #20879, #21244 ) ;
#34598 = LINE ( 'NONE', #61836, #14486 ) ;
#34599 = CARTESIAN_POINT ( 'NONE',  ( 8.406483450353379183, -7.616533956692325802, 455.0000000000000568 ) ) ;
#34600 = VERTEX_POINT ( 'NONE', #27146 ) ;
#34601 = EDGE_LOOP ( 'NONE', ( #35497, #2813, #69065, #39322 ) ) ;
#34602 = VECTOR ( 'NONE', #16740, 1000.000000000000114 ) ;
#34603 = AXIS2_PLACEMENT_3D ( 'NONE', #61366, #23203, #65982 ) ;
#34604 = FACE_OUTER_BOUND ( 'NONE', #10353, .T. ) ;
#34605 = DIRECTION ( 'NONE',  ( 0.000000000000000000, -1.000000000000000000, 0.000000000000000000 ) ) ;
#34606 = ORIENTED_EDGE ( 'NONE', *, *, #37957, .T. ) ;
#34607 = FACE_OUTER_BOUND ( 'NONE', #28019, .T. ) ;
#34609 = CARTESIAN_POINT ( 'NONE',  ( -7.450000000000001954, 0.000000000000000000, -13.50000000000000178 ) ) ;
#34608 = CIRCLE ( 'NONE', #40268, 0.1750000000000002387 ) ;
#34610 = DIRECTION ( 'NONE',  ( 1.000000000000000000, -0.000000000000000000, 0.000000000000000000 ) ) ;
#34611 = VERTEX_POINT ( 'NONE', #1638 ) ;
#34612 = AXIS2_PLACEMENT_3D ( 'NONE', #47081, #20901, #64060 ) ;
#34613 = CARTESIAN_POINT ( 'NONE',  ( 33.89999999999999858, 3.010794155703768650E-16, -2.458500000000000796 ) ) ;
#34614 = DIRECTION ( 'NONE',  ( -1.000000000000000000, 0.000000000000000000, 0.000000000000000000 ) ) ;
#34616 = EDGE_LOOP ( 'NONE', ( #52787, #30996, #39360, #54168 ) ) ;
#34615 = DIRECTION ( 'NONE',  ( 0.000000000000000000, 0.000000000000000000, -1.000000000000000000 ) ) ;
#34618 = ORIENTED_EDGE ( 'NONE', *, *, #34567, .F. ) ;
#34617 = CARTESIAN_POINT ( 'NONE',  ( 2.544523737882787184, -9.562023737882800134, 54.00000000000000711 ) ) ;
#34619 = DIRECTION ( 'NONE',  ( 1.000000000000000000, -0.000000000000000000, -0.000000000000000000 ) ) ;
#34620 = CYLINDRICAL_SURFACE ( 'NONE', #38645, 1.000000000000000000 ) ;
#34621 = DIRECTION ( 'NONE',  ( -0.000000000000000000, 3.673940397442059868E-16, -1.000000000000000000 ) ) ;
#34622 = DIRECTION ( 'NONE',  ( 0.000000000000000000, -1.000000000000000000, -2.854859206170826497E-12 ) ) ;
#34623 = DIRECTION ( 'NONE',  ( -0.000000000000000000, 3.673940397442059868E-16, -1.000000000000000000 ) ) ;
#34624 = ORIENTED_EDGE ( 'NONE', *, *, #34155, .F. ) ;
#34625 = DIRECTION ( 'NONE',  ( 1.000000000000000000, 0.000000000000000000, 0.000000000000000000 ) ) ;
#34626 = DIRECTION ( 'NONE',  ( 8.480870326997715333E-15, -0.000000000000000000, -1.000000000000000000 ) ) ;
#34627 = FACE_OUTER_BOUND ( 'NONE', #24548, .T. ) ;
#34628 = ADVANCED_FACE ( 'NONE', ( #273 ), #22875, .F. ) ;
#34630 = ORIENTED_EDGE ( 'NONE', *, *, #60856, .T. ) ;
#34629 = CARTESIAN_POINT ( 'NONE',  ( 283.0000000000000568, -42.50000000000000000, 7.500000000000000000 ) ) ;
#34631 = CARTESIAN_POINT ( 'NONE',  ( -8.566576262117349572, -8.930623737882770641, 54.00000000000000711 ) ) ;
#34632 = DIRECTION ( 'NONE',  ( 1.836970198721029934E-16, -1.836970198721036344E-16, 1.000000000000000000 ) ) ;
#34633 = EDGE_CURVE ( 'NONE', #21960, #62934, #17215, .T. ) ;
#34634 = AXIS2_PLACEMENT_3D ( 'NONE', #27161, #63956, #42025 ) ;
#34635 = ORIENTED_EDGE ( 'NONE', *, *, #62189, .F. ) ;
#34636 = FACE_BOUND ( 'NONE', #35532, .T. ) ;
#34637 = EDGE_CURVE ( 'NONE', #45732, #12812, #44767, .T. ) ;
#34638 = DIRECTION ( 'NONE',  ( 0.000000000000000000, 0.000000000000000000, -1.000000000000000000 ) ) ;
#34639 = EDGE_CURVE ( 'NONE', #43197, #46964, #11899, .T. ) ;
#34640 = ORIENTED_EDGE ( 'NONE', *, *, #3002, .T. ) ;
#34641 = CYLINDRICAL_SURFACE ( 'NONE', #49270, 0.1750000000000002387 ) ;
#34642 = CARTESIAN_POINT ( 'NONE',  ( -4.173516549646837603, -11.78648345035344214, 455.0000000000000568 ) ) ;
#34643 = AXIS2_PLACEMENT_3D ( 'NONE', #18985, #66022, #17588 ) ;
#34644 = VECTOR ( 'NONE', #24004, 1000.000000000000000 ) ;
#34645 = CYLINDRICAL_SURFACE ( 'NONE', #64858, 0.2000000000000005107 ) ;
#34646 = EDGE_CURVE ( 'NONE', #45166, #8148, #55072, .T. ) ;
#34647 = EDGE_CURVE ( 'NONE', #52649, #45380, #63862, .T. ) ;
#34648 = FACE_OUTER_BOUND ( 'NONE', #26085, .T. ) ;
#34649 = AXIS2_PLACEMENT_3D ( 'NONE', #68842, #48322, #53633 ) ;
#34651 = DIRECTION ( 'NONE',  ( -0.000000000000000000, -0.000000000000000000, -1.000000000000000000 ) ) ;
#34650 = AXIS2_PLACEMENT_3D ( 'NONE', #67502, #37681, #10452 ) ;
#34652 = EDGE_CURVE ( 'NONE', #31047, #64750, #33134, .T. ) ;
#34653 = ORIENTED_EDGE ( 'NONE', *, *, #31250, .T. ) ;
#34654 = DIRECTION ( 'NONE',  ( 1.000000000000000000, 0.000000000000000000, 0.000000000000000000 ) ) ;
#34655 = VERTEX_POINT ( 'NONE', #17562 ) ;
#34656 = ORIENTED_EDGE ( 'NONE', *, *, #10874, .F. ) ;
#34657 = DIRECTION ( 'NONE',  ( -1.000000000000000000, -2.135044278125301343E-15, -7.844025423732065664E-31 ) ) ;
#34658 = AXIS2_PLACEMENT_3D ( 'NONE', #51862, #66109, #40185 ) ;
#34659 = AXIS2_PLACEMENT_3D ( 'NONE', #11620, #44155, #38188 ) ;
#34660 = AXIS2_PLACEMENT_3D ( 'NONE', #7652, #14004, #62434 ) ;
#34662 = DIRECTION ( 'NONE',  ( -1.000000000000000000, 0.000000000000000000, 0.000000000000000000 ) ) ;
#34661 = CARTESIAN_POINT ( 'NONE',  ( 32.89999999999999858, 20.60000000000000142, -13.86939075806900057 ) ) ;
#34663 = ORIENTED_EDGE ( 'NONE', *, *, #32359, .F. ) ;
#34664 = VERTEX_POINT ( 'NONE', #54372 ) ;
#34665 = CARTESIAN_POINT ( 'NONE',  ( 7.000000000000000000, -26.79000000000000625, 0.000000000000000000 ) ) ;
#34666 = VERTEX_POINT ( 'NONE', #39132 ) ;
#34667 = AXIS2_PLACEMENT_3D ( 'NONE', #1755, #7400, #23666 ) ;
#34668 = CARTESIAN_POINT ( 'NONE',  ( 5.257023737882819070, -5.257023737882825287, 54.00000000000000711 ) ) ;
#34669 = DIRECTION ( 'NONE',  ( -1.203165845134433242E-14, -1.000000000000000000, -1.836970198721014403E-16 ) ) ;
#34670 = CARTESIAN_POINT ( 'NONE',  ( 29.50000000000000355, -11.50000000000100009, -10.50000000000065903 ) ) ;
#34671 = DIRECTION ( 'NONE',  ( 0.000000000000000000, 0.000000000000000000, -1.000000000000000000 ) ) ;
#34673 = CARTESIAN_POINT ( 'NONE',  ( -10.49297626211726175, 6.835476262117182955, 54.00000000000000711 ) ) ;
#34672 = CARTESIAN_POINT ( 'NONE',  ( 30.00000000000000000, -14.04000000000000092, 14.80000000000000071 ) ) ;
#34674 = ORIENTED_EDGE ( 'NONE', *, *, #55251, .F. ) ;
#34676 = VERTEX_POINT ( 'NONE', #60703 ) ;
#34675 = CARTESIAN_POINT ( 'NONE',  ( -8.393516549646712122, 7.603567055985436696, 455.0000000000000568 ) ) ;
#34677 = ORIENTED_EDGE ( 'NONE', *, *, #24203, .F. ) ;
#34678 = EDGE_LOOP ( 'NONE', ( #43839, #19903, #15033, #65998 ) ) ;
#34679 = DIRECTION ( 'NONE',  ( 0.7671651518152939886, -0.6414496315691644579, -2.587583378555133721E-16 ) ) ;
#34680 = EDGE_CURVE ( 'NONE', #21563, #40613, #67281, .T. ) ;
#34681 = CARTESIAN_POINT ( 'NONE',  ( -8.250000000000001776, 0.000000000000000000, -16.00000000000000000 ) ) ;
#34682 = ORIENTED_EDGE ( 'NONE', *, *, #52764, .T. ) ;
#34683 = EDGE_LOOP ( 'NONE', ( #64478, #42002, #20547, #1897 ) ) ;
#34684 = EDGE_CURVE ( 'NONE', #22096, #61056, #33818, .T. ) ;
#34685 = CYLINDRICAL_SURFACE ( 'NONE', #62525, 0.1999999999999996503 ) ;
#34686 = LINE ( 'NONE', #39977, #61592 ) ;
#34687 = ADVANCED_FACE ( 'NONE', ( #6948 ), #50088, .F. ) ;
#34688 = VERTEX_POINT ( 'NONE', #7985 ) ;
#34689 = ADVANCED_FACE ( 'NONE', ( #61741 ), #19648, .F. ) ;
#34690 = ORIENTED_EDGE ( 'NONE', *, *, #57958, .T. ) ;
#34691 = AXIS2_PLACEMENT_3D ( 'NONE', #29770, #28127, #17163 ) ;
#34693 = FACE_OUTER_BOUND ( 'NONE', #61018, .T. ) ;
#34692 = AXIS2_PLACEMENT_3D ( 'NONE', #36635, #29925, #3759 ) ;
#34694 = FACE_OUTER_BOUND ( 'NONE', #59924, .T. ) ;
#34695 = EDGE_LOOP ( 'NONE', ( #15402, #56376 ) ) ;
#34696 = AXIS2_PLACEMENT_3D ( 'NONE', #16065, #9718, #63456 ) ;
#34697 = CIRCLE ( 'NONE', #65223, 4.000000000000000888 ) ;
#34698 = PRODUCT_DEFINITION_FORMATION_WITH_SPECIFIED_SOURCE ( 'ANY', '', #17722, .NOT_KNOWN. ) ;
#34699 = CARTESIAN_POINT ( 'NONE',  ( 9.249999999999998224, -7.848062532927998269, -5.000000000000000000 ) ) ;
#34700 = CARTESIAN_POINT ( 'NONE',  ( -17.00000000000000000, -15.50000000000000000, 14.50000000000000000 ) ) ;
#34702 = ORIENTED_EDGE ( 'NONE', *, *, #53461, .F. ) ;
#34701 = DIRECTION ( 'NONE',  ( 0.6414496315691526895, 0.7671651518153038696, 2.587583378555111534E-16 ) ) ;
#34703 = ORIENTED_EDGE ( 'NONE', *, *, #15466, .F. ) ;
#34704 = DIRECTION ( 'NONE',  ( 1.000000000000000000, -3.491481338843133355E-15, 0.000000000000000000 ) ) ;
#34705 = AXIS2_PLACEMENT_3D ( 'NONE', #35146, #7585, #24561 ) ;
#34706 = CARTESIAN_POINT ( 'NONE',  ( 11.12648345035337627, -9.106483450353492159, 455.0000000000000568 ) ) ;
#34707 = AXIS2_PLACEMENT_3D ( 'NONE', #26433, #16170, #41641 ) ;
#34708 = CARTESIAN_POINT ( 'NONE',  ( 12.00648345035337350, 11.18071654964659345, 195.0000000000000284 ) ) ;
#34709 = LINE ( 'NONE', #7486, #4162 ) ;
#34710 = CARTESIAN_POINT ( 'NONE',  ( 78.77321854994620765, 47.95351654967443977, 43.00000000000000000 ) ) ;
#34711 = CARTESIAN_POINT ( 'NONE',  ( -9.293516549646710700, 10.91351654964659801, 455.0000000000000568 ) ) ;
#34712 = DIRECTION ( 'NONE',  ( -0.000000000000000000, 3.673940397442059868E-16, -1.000000000000000000 ) ) ;
#34713 = VERTEX_POINT ( 'NONE', #29910 ) ;
#34714 = LINE ( 'NONE', #67250, #42793 ) ;
#34716 = VERTEX_POINT ( 'NONE', #45829 ) ;
#34715 = CARTESIAN_POINT ( 'NONE',  ( 11.50000000000000000, -15.97213595500069871, 14.50000000000000000 ) ) ;
#34717 = CIRCLE ( 'NONE', #60711, 1.000000000000000000 ) ;
#34718 = ADVANCED_FACE ( 'NONE', ( #18599 ), #29560, .F. ) ;
#34719 = LINE ( 'NONE', #7839, #519 ) ;
#34720 = FACE_OUTER_BOUND ( 'NONE', #58603, .T. ) ;
#34721 = PLANE ( 'NONE',  #35881 ) ;
#34722 = DIRECTION ( 'NONE',  ( 0.000000000000000000, 0.000000000000000000, 1.000000000000000000 ) ) ;
#34723 = LINE ( 'NONE', #6486, #48419 ) ;
#34724 = ORIENTED_EDGE ( 'NONE', *, *, #13180, .T. ) ;
#34725 = DIRECTION ( 'NONE',  ( -1.836970198721029934E-16, -1.836970198721010706E-16, 1.000000000000000000 ) ) ;
#34726 = ORIENTED_EDGE ( 'NONE', *, *, #15561, .F. ) ;
#34727 = CARTESIAN_POINT ( 'NONE',  ( 8.612468434717241550, -2.005523737882825674, 54.00000000000000711 ) ) ;
#34728 = EDGE_CURVE ( 'NONE', #5750, #48101, #51845, .T. ) ;
#34729 = EDGE_CURVE ( 'NONE', #12276, #11704, #62793, .T. ) ;
#34730 = DIRECTION ( 'NONE',  ( 1.000000000000000000, -1.047444401652940007E-14, 1.836970198721010706E-16 ) ) ;
#34731 = FACE_OUTER_BOUND ( 'NONE', #52861, .T. ) ;
#34732 = EDGE_CURVE ( 'NONE', #11358, #4089, #45468, .T. ) ;
#34733 = ORIENTED_EDGE ( 'NONE', *, *, #14246, .F. ) ;
#34734 = CARTESIAN_POINT ( 'NONE',  ( -4.383466043307968185, -8.406483450353443132, 455.0000000000000568 ) ) ;
#34735 = ORIENTED_EDGE ( 'NONE', *, *, #18131, .T. ) ;
#34736 = VECTOR ( 'NONE', #28052, 1000.000000000000000 ) ;
#34737 = VERTEX_POINT ( 'NONE', #14366 ) ;
#34738 = LINE ( 'NONE', #56313, #41527 ) ;
#34739 = DIRECTION ( 'NONE',  ( 1.000000000000000000, 0.000000000000000000, 0.000000000000000000 ) ) ;
#34740 = ORIENTED_EDGE ( 'NONE', *, *, #12248, .F. ) ;
#34741 = LINE ( 'NONE', #34038, #24301 ) ;
#34742 = FACE_OUTER_BOUND ( 'NONE', #25483, .T. ) ;
#34743 = CARTESIAN_POINT ( 'NONE',  ( -5.993516549646711766, 5.993516549646603409, 455.0000000000000568 ) ) ;
#34744 = VERTEX_POINT ( 'NONE', #2346 ) ;
#34745 = ORIENTED_EDGE ( 'NONE', *, *, #22465, .T. ) ;
#34747 = ORIENTED_EDGE ( 'NONE', *, *, #5135, .F. ) ;
#34746 = CARTESIAN_POINT ( 'NONE',  ( 6.006483450353379716, -6.006483450353490738, 455.0000000000000568 ) ) ;
#34748 = EDGE_LOOP ( 'NONE', ( #36574, #26964, #66872, #66771 ) ) ;
#34749 = AXIS2_PLACEMENT_3D ( 'NONE', #38928, #60487, #33625 ) ;
#34750 = DIRECTION ( 'NONE',  ( -0.7071067811865361374, 0.7071067811865588970, 2.810316974849854557E-30 ) ) ;
#34751 = DIRECTION ( 'NONE',  ( 0.000000000000000000, 0.000000000000000000, 1.000000000000000000 ) ) ;
#34752 = DIRECTION ( 'NONE',  ( -1.156482317317873342E-14, -1.000000000000000000, 0.000000000000000000 ) ) ;
#34753 = FACE_BOUND ( 'NONE', #45482, .T. ) ;
#34754 = VECTOR ( 'NONE', #50190, 1000.000000000000000 ) ;
#34755 = CIRCLE ( 'NONE', #40369, 0.9999999999999991118 ) ;
#34757 = CARTESIAN_POINT ( 'NONE',  ( 146.5599459900709860, 0.000000000000000000, 328.5239988703752942 ) ) ;
#34756 =( GEOMETRIC_REPRESENTATION_CONTEXT ( 3 ) GLOBAL_UNCERTAINTY_ASSIGNED_CONTEXT ( ( #25316 ) ) GLOBAL_UNIT_ASSIGNED_CONTEXT ( ( #43659, #17127, #56342 ) ) REPRESENTATION_CONTEXT ( 'NONE', 'WORKASPACE' ) );
#34758 = LINE ( 'NONE', #7878, #54688 ) ;
#34759 = ORIENTED_EDGE ( 'NONE', *, *, #60777, .T. ) ;
#34760 = ORIENTED_EDGE ( 'NONE', *, *, #4944, .T. ) ;
#34761 = ORIENTED_EDGE ( 'NONE', *, *, #66650, .T. ) ;
#34762 = ORIENTED_EDGE ( 'NONE', *, *, #36754, .T. ) ;
#34763 = LINE ( 'NONE', #2944, #43456 ) ;
#34764 = DIRECTION ( 'NONE',  ( -1.000000000000000000, 3.903627567395476653E-15, 1.836970198721037083E-16 ) ) ;
#34765 = FACE_OUTER_BOUND ( 'NONE', #10019, .T. ) ;
#34766 = VECTOR ( 'NONE', #60210, 1000.000000000000000 ) ;
#34767 = PLANE ( 'NONE',  #9441 ) ;
#34768 = EDGE_LOOP ( 'NONE', ( #55233, #26712, #24484, #59977 ) ) ;
#34769 = ORIENTED_EDGE ( 'NONE', *, *, #42493, .F. ) ;
#34770 = ORIENTED_EDGE ( 'NONE', *, *, #16809, .F. ) ;
#34771 = EDGE_CURVE ( 'NONE', #6534, #14806, #23912, .T. ) ;
#34772 = EDGE_CURVE ( 'NONE', #57470, #47184, #66693, .T. ) ;
#34773 = ADVANCED_FACE ( 'NONE', ( #46177 ), #46523, .T. ) ;
#34774 = LINE ( 'NONE', #51040, #30550 ) ;
#34775 = VERTEX_POINT ( 'NONE', #28857 ) ;
#34776 = ORIENTED_EDGE ( 'NONE', *, *, #25034, .F. ) ;
#34777 = EDGE_CURVE ( 'NONE', #31939, #59906, #67412, .T. ) ;
#34778 = ORIENTED_EDGE ( 'NONE', *, *, #10046, .T. ) ;
#34779 = ORIENTED_EDGE ( 'NONE', *, *, #68591, .F. ) ;
#34780 = CARTESIAN_POINT ( 'NONE',  ( 8.900000000000005684, 13.66939075806899950, 20.80000000000000426 ) ) ;
#34782 = ORIENTED_EDGE ( 'NONE', *, *, #37248, .F. ) ;
#34781 = DIRECTION ( 'NONE',  ( 0.000000000000000000, 1.000000000000000000, 3.673940397442059868E-16 ) ) ;
#34783 = ORIENTED_EDGE ( 'NONE', *, *, #32945, .F. ) ;
#34784 = CARTESIAN_POINT ( 'NONE',  ( -10.50000000000000178, -9.690000000000001279, -4.250000000000000000 ) ) ;
#34785 = CARTESIAN_POINT ( 'NONE',  ( 31.89999999999999858, 0.000000000000000000, 0.000000000000000000 ) ) ;
#34786 = LINE ( 'NONE', #18519, #7596 ) ;
#34787 = MECHANICAL_DESIGN_GEOMETRIC_PRESENTATION_REPRESENTATION (  '', ( #65304 ), #12178 ) ;
#34789 = ORIENTED_EDGE ( 'NONE', *, *, #18273, .T. ) ;
#34788 = DIRECTION ( 'NONE',  ( 1.836970198721029934E-16, -1.836970198721036344E-16, 1.000000000000000000 ) ) ;
#34790 = ORIENTED_EDGE ( 'NONE', *, *, #64436, .F. ) ;
#34791 = CARTESIAN_POINT ( 'NONE',  ( -11.50000000000000000, -11.50000000000000000, -15.00000000000000000 ) ) ;
#34792 = LINE ( 'NONE', #34428, #23250 ) ;
#34793 = FACE_OUTER_BOUND ( 'NONE', #8939, .T. ) ;
#34794 = ORIENTED_EDGE ( 'NONE', *, *, #6861, .F. ) ;
#34795 = CARTESIAN_POINT ( 'NONE',  ( 0.000000000000000000, -7.449999999999998401, -23.00000000000000000 ) ) ;
#34796 = AXIS2_PLACEMENT_3D ( 'NONE', #51548, #33872, #55796 ) ;
#34797 = CARTESIAN_POINT ( 'NONE',  ( 30.00000000000000000, -8.959999999999999076, -12.95475478405700009 ) ) ;
#34798 = CARTESIAN_POINT ( 'NONE',  ( 30.00000000000000000, -11.50000000000082068, -10.20500000000000007 ) ) ;
#34799 = ORIENTED_EDGE ( 'NONE', *, *, #37390, .T. ) ;
#34800 = LINE ( 'NONE', #56377, #22322 ) ;
#34801 = VECTOR ( 'NONE', #54456, 1000.000000000000000 ) ;
#34802 = CARTESIAN_POINT ( 'NONE',  ( 283.0000000000000568, -20.40000000000000213, 17.60000000000000142 ) ) ;
#34803 = VERTEX_POINT ( 'NONE', #8701 ) ;
#34804 = CYLINDRICAL_SURFACE ( 'NONE', #864, 0.1749999999999998224 ) ;
#34805 = PLANE ( 'NONE',  #39019 ) ;
#34806 = PLANE ( 'NONE',  #30011 ) ;
#34807 = EDGE_CURVE ( 'NONE', #68360, #15497, #20954, .T. ) ;
#34808 = VECTOR ( 'NONE', #12451, 1000.000000000000000 ) ;
#34809 = EDGE_CURVE ( 'NONE', #45363, #50155, #62425, .T. ) ;
#34810 = ORIENTED_EDGE ( 'NONE', *, *, #1672, .F. ) ;
#34811 = LINE ( 'NONE', #28462, #62018 ) ;
#34812 = FACE_OUTER_BOUND ( 'NONE', #7354, .T. ) ;
#34813 = EDGE_CURVE ( 'NONE', #40705, #20348, #34857, .T. ) ;
#34814 = LINE ( 'NONE', #18208, #69203 ) ;
#34815 = CARTESIAN_POINT ( 'NONE',  ( 6.358413763958941978, 4.706725378239156932, 26.00000000000000711 ) ) ;
#34816 = DIRECTION ( 'NONE',  ( -1.000000000000000000, 0.000000000000000000, 0.000000000000000000 ) ) ;
#34817 = EDGE_LOOP ( 'NONE', ( #6067, #19635, #63190, #19472, #210 ) ) ;
#34818 = DIRECTION ( 'NONE',  ( 0.000000000000000000, 0.000000000000000000, 1.000000000000000000 ) ) ;
#34819 = CARTESIAN_POINT ( 'NONE',  ( -7.250000000000000888, 8.250000000000001776, -10.00000000000000000 ) ) ;
#34820 = EDGE_CURVE ( 'NONE', #12839, #19794, #12937, .T. ) ;
#34821 = CARTESIAN_POINT ( 'NONE',  ( -29.50000000000000355, -11.50000000000100009, -19.50000000000103739 ) ) ;
#34822 = PRODUCT_DEFINITION ( 'UNKNOWN', '', #18914, #2750 ) ;
#34823 = CARTESIAN_POINT ( 'NONE',  ( 7.000000000000000000, -38.64999999999999858, -15.00000000000000000 ) ) ;
#34824 = EDGE_CURVE ( 'NONE', #38359, #47718, #57135, .T. ) ;
#34825 = CARTESIAN_POINT ( 'NONE',  ( 33.89999999999999858, -0.000000000000000000, -20.80000000000000071 ) ) ;
#34826 = ORIENTED_EDGE ( 'NONE', *, *, #56999, .T. ) ;
#34828 = ORIENTED_EDGE ( 'NONE', *, *, #37897, .F. ) ;
#34827 = DIRECTION ( 'NONE',  ( 0.000000000000000000, 1.000000000000000000, 0.000000000000000000 ) ) ;
#34829 = EDGE_CURVE ( 'NONE', #7825, #41567, #24377, .T. ) ;
#34830 = CARTESIAN_POINT ( 'NONE',  ( 5.668387132715968058, 8.393516549646582448, 455.0000000000000568 ) ) ;
#34831 = DIRECTION ( 'NONE',  ( 0.7071067811865474617, -0.7071067811865474617, 0.000000000000000000 ) ) ;
#34832 = VERTEX_POINT ( 'NONE', #8335 ) ;
#34833 = LINE ( 'NONE', #18938, #37505 ) ;
#34834 = ORIENTED_EDGE ( 'NONE', *, *, #21580, .T. ) ;
#34835 = VECTOR ( 'NONE', #48276, 1000.000000000000000 ) ;
#34836 = LINE ( 'NONE', #66675, #56021 ) ;
#34837 = ORIENTED_EDGE ( 'NONE', *, *, #34680, .T. ) ;
#34838 = EDGE_LOOP ( 'NONE', ( #59995, #23125, #53141, #27323, #480, #15139 ) ) ;
#34839 = DIRECTION ( 'NONE',  ( 1.836970198721029934E-16, 1.836970198721010706E-16, -1.000000000000000000 ) ) ;
#34840 = CARTESIAN_POINT ( 'NONE',  ( -10.91351654964670637, 9.293516549646604119, 455.0000000000000568 ) ) ;
#34841 = AXIS2_PLACEMENT_3D ( 'NONE', #23801, #7532, #41102 ) ;
#34842 = CARTESIAN_POINT ( 'NONE',  ( 0.000000000000000000, -7.449999999999998401, -7.500000000000000000 ) ) ;
#34843 = DIRECTION ( 'NONE',  ( 1.000000000000000000, 0.000000000000000000, 0.000000000000000000 ) ) ;
#34844 = ORIENTED_EDGE ( 'NONE', *, *, #35120, .T. ) ;
#34845 = ORIENTED_EDGE ( 'NONE', *, *, #29459, .T. ) ;
#34846 = DIRECTION ( 'NONE',  ( 0.000000000000000000, 0.000000000000000000, -1.000000000000000000 ) ) ;
#34847 = VECTOR ( 'NONE', #8978, 1000.000000000000000 ) ;
#34848 = LINE ( 'NONE', #67033, #40684 ) ;
#34849 = ORIENTED_EDGE ( 'NONE', *, *, #61631, .F. ) ;
#34850 = VERTEX_POINT ( 'NONE', #24964 ) ;
#34851 = VERTEX_POINT ( 'NONE', #68098 ) ;
#34852 = VECTOR ( 'NONE', #48855, 1000.000000000000000 ) ;
#34853 = DIRECTION ( 'NONE',  ( 1.000000000000000000, 0.000000000000000000, 0.000000000000000000 ) ) ;
#34855 = VERTEX_POINT ( 'NONE', #15417 ) ;
#34854 = LINE ( 'NONE', #1636, #27043 ) ;
#34856 = VECTOR ( 'NONE', #40900, 1000.000000000000114 ) ;
#34857 = LINE ( 'NONE', #13998, #48117 ) ;
#34858 = DIRECTION ( 'NONE',  ( 0.000000000000000000, 0.000000000000000000, 1.000000000000000000 ) ) ;
#34859 = VERTEX_POINT ( 'NONE', #25685 ) ;
#34860 = ORIENTED_EDGE ( 'NONE', *, *, #28657, .F. ) ;
#34861 = ADVANCED_FACE ( 'NONE', ( #47242 ), #36620, .F. ) ;
#34862 = CARTESIAN_POINT ( 'NONE',  ( 25.50000000000000355, 0.000000000000000000, -22.50000000000000000 ) ) ;
#34863 = LINE ( 'NONE', #8710, #69680 ) ;
#34864 = EDGE_CURVE ( 'NONE', #41567, #59591, #9405, .T. ) ;
#34865 = CARTESIAN_POINT ( 'NONE',  ( 29.50000000000000355, -11.50000000000100009, 15.00000000000084910 ) ) ;
#34866 = DIRECTION ( 'NONE',  ( 5.013651664672856055E-16, -1.000000000000000000, -3.673940397442059868E-16 ) ) ;
#34867 = DIRECTION ( 'NONE',  ( 1.000000000000000000, 0.000000000000000000, 0.000000000000000000 ) ) ;
#34868 = EDGE_CURVE ( 'NONE', #46792, #46314, #52544, .T. ) ;
#34870 = ORIENTED_EDGE ( 'NONE', *, *, #68785, .T. ) ;
#34869 = LINE ( 'NONE', #46535, #40064 ) ;
#34871 = ORIENTED_EDGE ( 'NONE', *, *, #9065, .F. ) ;
#34872 = CARTESIAN_POINT ( 'NONE',  ( -7.250000000000001776, -7.249999999999998224, -26.00000000000001066 ) ) ;
#34873 = CYLINDRICAL_SURFACE ( 'NONE', #59518, 1.621000000000000885 ) ;
#34874 = LINE ( 'NONE', #62099, #54507 ) ;
#34875 = DIRECTION ( 'NONE',  ( 0.000000000000000000, 1.000000000000000000, 0.000000000000000000 ) ) ;
#34876 = EDGE_CURVE ( 'NONE', #37791, #16514, #20013, .T. ) ;
#34877 = CIRCLE ( 'NONE', #55249, 0.1749999999999998224 ) ;
#34878 = CARTESIAN_POINT ( 'NONE',  ( 40.90000000000000568, 0.000000000000000000, 3.500000000000000000 ) ) ;
#34879 = ORIENTED_EDGE ( 'NONE', *, *, #50619, .F. ) ;
#34880 = DIRECTION ( 'NONE',  ( -1.836970198721029934E-16, -1.836970198721010706E-16, 1.000000000000000000 ) ) ;
#34881 = DIRECTION ( 'NONE',  ( 0.000000000000000000, 1.000000000000000000, 0.000000000000000000 ) ) ;
#34882 =( NAMED_UNIT ( * ) SI_UNIT ( $, .STERADIAN. ) SOLID_ANGLE_UNIT ( ) );
#34883 = AXIS2_PLACEMENT_3D ( 'NONE', #58076, #21649, #25565 ) ;
#34884 = LINE ( 'NONE', #35229, #7445 ) ;
#34885 = ADVANCED_FACE ( 'NONE', ( #42624, #4804 ), #58191, .F. ) ;
#34886 = CARTESIAN_POINT ( 'NONE',  ( 289.5000000000000000, -42.50000000000000000, 26.50000000000000000 ) ) ;
#34887 = CARTESIAN_POINT ( 'NONE',  ( 40.90000000000000568, 0.000000000000000000, 0.000000000000000000 ) ) ;
#34888 = AXIS2_PLACEMENT_3D ( 'NONE', #19502, #36115, #29755 ) ;
#34889 = DIRECTION ( 'NONE',  ( -0.7071067811865490160, 0.7071067811865461294, 0.000000000000000000 ) ) ;
#34890 = ORIENTED_EDGE ( 'NONE', *, *, #42731, .T. ) ;
#34891 = DIRECTION ( 'NONE',  ( 0.000000000000000000, 0.000000000000000000, 1.000000000000000000 ) ) ;
#34892 = DIRECTION ( 'NONE',  ( 0.000000000000000000, 1.000000000000000000, 0.000000000000000000 ) ) ;
#34893 = VERTEX_POINT ( 'NONE', #41580 ) ;
#34894 = LINE ( 'NONE', #2042, #16524 ) ;
#34895 = CARTESIAN_POINT ( 'NONE',  ( -5.993516549646728642, -6.006483450353378828, 195.0000000000000284 ) ) ;
#34896 = VECTOR ( 'NONE', #9415, 1000.000000000000000 ) ;
#34897 = CARTESIAN_POINT ( 'NONE',  ( 49.00000000000000000, -14.06939075806900163, -20.80000000000000426 ) ) ;
#34898 = LINE ( 'NONE', #40213, #47749 ) ;
#34899 = EDGE_CURVE ( 'NONE', #25493, #33142, #21063, .T. ) ;
#34900 = CARTESIAN_POINT ( 'NONE',  ( 30.90000000000000213, 13.66939075806899240, 20.79999999999999361 ) ) ;
#34901 = ORIENTED_EDGE ( 'NONE', *, *, #11246, .T. ) ;
#34902 = EDGE_CURVE ( 'NONE', #17827, #14810, #69849, .T. ) ;
#34903 = AXIS2_PLACEMENT_3D ( 'NONE', #38735, #59269, #33440 ) ;
#34904 = CARTESIAN_POINT ( 'NONE',  ( 15.00000000000000000, -42.00000000000000000, -15.10000000000000142 ) ) ;
#34905 = EDGE_LOOP ( 'NONE', ( #25993, #13512, #29476, #39941 ) ) ;
#34906 = CARTESIAN_POINT ( 'NONE',  ( 11.00000000000000000, -9.454754784057099570, 17.53999999999999915 ) ) ;
#34907 = VERTEX_POINT ( 'NONE', #4464 ) ;
#34908 = DIRECTION ( 'NONE',  ( -1.000000000000000000, 0.000000000000000000, 0.000000000000000000 ) ) ;
#34909 = AXIS2_PLACEMENT_3D ( 'NONE', #35402, #27774, #56974 ) ;
#34910 = ADVANCED_FACE ( 'NONE', ( #64553 ), #9766, .T. ) ;
#34911 = ORIENTED_EDGE ( 'NONE', *, *, #47864, .T. ) ;
#34912 = CARTESIAN_POINT ( 'NONE',  ( -1.620245201994301665, 8.227189898828640935, 54.00000000000000711 ) ) ;
#34913 = CARTESIAN_POINT ( 'NONE',  ( -3.142976262117286979, -6.501044194225493733, 26.00000000000000711 ) ) ;
#34914 = VERTEX_POINT ( 'NONE', #52913 ) ;
#34915 = ORIENTED_EDGE ( 'NONE', *, *, #28864, .T. ) ;
#34916 = CARTESIAN_POINT ( 'NONE',  ( 11.50000000000000000, -11.50000000000100009, 19.50000000000103739 ) ) ;
#34917 = ORIENTED_EDGE ( 'NONE', *, *, #4244, .F. ) ;
#34918 = ORIENTED_EDGE ( 'NONE', *, *, #17311, .T. ) ;
#34919 = DIRECTION ( 'NONE',  ( 0.000000000000000000, 0.000000000000000000, -1.000000000000000000 ) ) ;
#34920 = CARTESIAN_POINT ( 'NONE',  ( -5.242976262117294617, -7.186223737882800222, 26.00000000000000711 ) ) ;
#34921 = FACE_OUTER_BOUND ( 'NONE', #13013, .T. ) ;
#34922 = AXIS2_PLACEMENT_3D ( 'NONE', #29036, #2510, #61544 ) ;
#34923 = ORIENTED_EDGE ( 'NONE', *, *, #20710, .F. ) ;
#34924 = CARTESIAN_POINT ( 'NONE',  ( 9.703773737882785966, -10.05377373788282469, 54.00000000000000711 ) ) ;
#34926 = CARTESIAN_POINT ( 'NONE',  ( 7.250000000000005329, 7.250000000000000888, -19.50000000000000000 ) ) ;
#34925 = PLANE ( 'NONE',  #29886 ) ;
#34927 = ORIENTED_EDGE ( 'NONE', *, *, #24102, .T. ) ;
#34929 = EDGE_LOOP ( 'NONE', ( #32224, #31030, #69028, #52516 ) ) ;
#34928 = LINE ( 'NONE', #60771, #1481 ) ;
#34930 = ORIENTED_EDGE ( 'NONE', *, *, #53100, .T. ) ;
#34931 = EDGE_CURVE ( 'NONE', #10558, #51495, #51484, .T. ) ;
#34932 = APPLICATION_PROTOCOL_DEFINITION ( 'draft international standard', 'automotive_design', 1998, #10589 ) ;
#34933 = DIRECTION ( 'NONE',  ( 0.000000000000000000, 0.000000000000000000, -1.000000000000000000 ) ) ;
#34934 = VECTOR ( 'NONE', #63194, 1000.000000000000000 ) ;
#34935 = VECTOR ( 'NONE', #68955, 1000.000000000000000 ) ;
#34936 = EDGE_LOOP ( 'NONE', ( #11758, #46490, #54284, #27053 ) ) ;
#34937 = EDGE_CURVE ( 'NONE', #5797, #55172, #52187, .T. ) ;
#34938 = DIRECTION ( 'NONE',  ( -1.000000000000000000, 0.000000000000000000, 0.000000000000000000 ) ) ;
#34939 = DIRECTION ( 'NONE',  ( 1.836970198721029934E-16, 1.836970198721010706E-16, -1.000000000000000000 ) ) ;
#34940 = ORIENTED_EDGE ( 'NONE', *, *, #51424, .F. ) ;
#34941 = ORIENTED_EDGE ( 'NONE', *, *, #13749, .T. ) ;
#34942 = EDGE_CURVE ( 'NONE', #17328, #69660, #57488, .T. ) ;
#34943 = CARTESIAN_POINT ( 'NONE',  ( 9.562023737882814345, -7.969523737882825642, 54.00000000000000711 ) ) ;
#34944 = EDGE_CURVE ( 'NONE', #24837, #11985, #15358, .T. ) ;
#34945 = DIRECTION ( 'NONE',  ( 0.000000000000000000, 0.000000000000000000, 1.000000000000000000 ) ) ;
#34946 = VERTEX_POINT ( 'NONE', #57838 ) ;
#34947 = VECTOR ( 'NONE', #68228, 1000.000000000000227 ) ;
#34948 = DIRECTION ( 'NONE',  ( 0.000000000000000000, 0.000000000000000000, -1.000000000000000000 ) ) ;
#34949 = CARTESIAN_POINT ( 'NONE',  ( 7.250000000000005329, 8.250000000000001776, -26.00000000000001066 ) ) ;
#34950 = ADVANCED_FACE ( 'NONE', ( #42273 ), #63850, .F. ) ;
#34951 = CARTESIAN_POINT ( 'NONE',  ( -7.250000000000000000, -7.449999999999998401, -10.00000000000000000 ) ) ;
#34952 = ORIENTED_EDGE ( 'NONE', *, *, #63401, .T. ) ;
#34953 = CIRCLE ( 'NONE', #48570, 4.000000000000000888 ) ;
#34954 = DIRECTION ( 'NONE',  ( -1.000000000000000000, 0.000000000000000000, 0.000000000000000000 ) ) ;
#34955 = DIRECTION ( 'NONE',  ( -1.000000000000000000, 1.901462112903060228E-14, -1.836970198720995175E-16 ) ) ;
#34956 = EDGE_CURVE ( 'NONE', #18717, #25138, #64211, .T. ) ;
#34958 = EDGE_LOOP ( 'NONE', ( #4710, #9555, #53947, #7561 ) ) ;
#34957 = DIRECTION ( 'NONE',  ( 0.000000000000000000, 0.000000000000000000, 1.000000000000000000 ) ) ;
#34960 = ORIENTED_EDGE ( 'NONE', *, *, #4726, .F. ) ;
#34959 = CARTESIAN_POINT ( 'NONE',  ( -7.250000000000000000, -7.449999999999998401, -17.50000000000000000 ) ) ;
#34961 = EDGE_CURVE ( 'NONE', #47101, #32931, #60517, .T. ) ;
#34962 = CARTESIAN_POINT ( 'NONE',  ( 2.500000000000000000, 3.061616997868383141E-16, -30.00000000000001066 ) ) ;
#34963 = CONICAL_SURFACE ( 'NONE', #23663, 1.621000000000000885, 0.7853981633974518317 ) ;
#34964 = CARTESIAN_POINT ( 'NONE',  ( 283.0000000000000568, -38.15000000000000568, 13.19999999999999929 ) ) ;
#34965 = EDGE_CURVE ( 'NONE', #27411, #69858, #50367, .T. ) ;
#34966 = CARTESIAN_POINT ( 'NONE',  ( -7.250000000000001776, -7.249999999999998224, -11.50000000000000000 ) ) ;
#34967 = EDGE_CURVE ( 'NONE', #35206, #7633, #8568, .T. ) ;
#34968 = EDGE_CURVE ( 'NONE', #64092, #65251, #32378, .T. ) ;
#34969 = FACE_OUTER_BOUND ( 'NONE', #54177, .T. ) ;
#34970 = LINE ( 'NONE', #50554, #59019 ) ;
#34971 = ORIENTED_EDGE ( 'NONE', *, *, #31980, .T. ) ;
#34972 = DIRECTION ( 'NONE',  ( 0.000000000000000000, 0.000000000000000000, -1.000000000000000000 ) ) ;
#34973 = CARTESIAN_POINT ( 'NONE',  ( 39.90000000000000568, 0.000000000000000000, 0.000000000000000000 ) ) ;
#34974 = ADVANCED_FACE ( 'NONE', ( #59593 ), #60267, .T. ) ;
#34975 = CARTESIAN_POINT ( 'NONE',  ( 23.48000000000000043, -15.50000000000000000, -26.00000000000000355 ) ) ;
#34977 = ORIENTED_EDGE ( 'NONE', *, *, #23611, .F. ) ;
#34976 = CARTESIAN_POINT ( 'NONE',  ( -11.31351654964670850, 7.793516549646603231, 455.0000000000000568 ) ) ;
#34978 = DIRECTION ( 'NONE',  ( 0.000000000000000000, 1.000000000000000000, 0.000000000000000000 ) ) ;
#34979 = VECTOR ( 'NONE', #8697, 1000.000000000000000 ) ;
#34980 = CARTESIAN_POINT ( 'NONE',  ( -7.450000000000001954, -7.249999999999998224, -18.00000000000000000 ) ) ;
#34981 = ORIENTED_EDGE ( 'NONE', *, *, #20893, .F. ) ;
#34982 = ORIENTED_EDGE ( 'NONE', *, *, #23779, .T. ) ;
#34983 = LINE ( 'NONE', #29328, #56863 ) ;
#34984 = CYLINDRICAL_SURFACE ( 'NONE', #33938, 24.99999999998789946 ) ;
#34985 = ORIENTED_EDGE ( 'NONE', *, *, #37549, .F. ) ;
#34986 = DIRECTION ( 'NONE',  ( 0.000000000000000000, -0.7084617869615142949, -0.7057491738679528837 ) ) ;
#34987 = CARTESIAN_POINT ( 'NONE',  ( 7.250000000000005329, 7.250000000000000888, -25.50000000000000355 ) ) ;
#34988 = EDGE_CURVE ( 'NONE', #68972, #11705, #4110, .T. ) ;
#34989 = DIRECTION ( 'NONE',  ( -1.000000000000000000, -1.671920889371702657E-15, 0.000000000000000000 ) ) ;
#34990 = AXIS2_PLACEMENT_3D ( 'NONE', #55295, #21726, #11790 ) ;
#34991 = CIRCLE ( 'NONE', #16949, 1.929199999999998028 ) ;
#34992 = ADVANCED_FACE ( 'NONE', ( #44342 ), #38374, .T. ) ;
#34993 = DIRECTION ( 'NONE',  ( -1.000000000000000000, 0.000000000000000000, 0.000000000000000000 ) ) ;
#34994 = VECTOR ( 'NONE', #41616, 1000.000000000000000 ) ;
#34995 = VERTEX_POINT ( 'NONE', #65256 ) ;
#34996 = LINE ( 'NONE', #36051, #46170 ) ;
#34997 = VERTEX_POINT ( 'NONE', #5847 ) ;
#34998 = ORIENTED_EDGE ( 'NONE', *, *, #21935, .T. ) ;
#34999 = AXIS2_PLACEMENT_3D ( 'NONE', #67439, #46547, #41246 ) ;
#35000 = DIRECTION ( 'NONE',  ( 0.000000000000000000, -1.000000000000000000, 0.000000000000000000 ) ) ;
#35001 = CIRCLE ( 'NONE', #46318, 0.1999999999999996503 ) ;
#35002 = LINE ( 'NONE', #56579, #38909 ) ;
#35003 = DIRECTION ( 'NONE',  ( -1.000000000000000000, 0.000000000000000000, 0.000000000000000000 ) ) ;
#35004 = VERTEX_POINT ( 'NONE', #6190 ) ;
#35005 = EDGE_LOOP ( 'NONE', ( #20515, #25267, #46815, #65921 ) ) ;
#35006 = AXIS2_PLACEMENT_3D ( 'NONE', #28428, #2265, #11817 ) ;
#35007 = CARTESIAN_POINT ( 'NONE',  ( -7.250000000000000000, -7.449999999999998401, -13.50000000000000178 ) ) ;
#35008 = ORIENTED_EDGE ( 'NONE', *, *, #52090, .F. ) ;
#35009 = CARTESIAN_POINT ( 'NONE',  ( 29.50000000000000355, -11.50000000000000000, 15.00000000000000000 ) ) ;
#35010 = CARTESIAN_POINT ( 'NONE',  ( -10.50000000000000000, -9.690000000000001279, -4.250000000000000000 ) ) ;
#35011 = ADVANCED_FACE ( 'NONE', ( #22460 ), #5507, .T. ) ;
#35012 = FACE_OUTER_BOUND ( 'NONE', #66523, .T. ) ;
#35013 = DIRECTION ( 'NONE',  ( 0.6414496315691575745, 0.7671651518152999838, 2.587583378555113013E-16 ) ) ;
#35014 = EDGE_LOOP ( 'NONE', ( #1060, #53601, #48900, #69484 ) ) ;
#35015 = CYLINDRICAL_SURFACE ( 'NONE', #48110, 4.500000000000189182 ) ;
#35016 = VECTOR ( 'NONE', #26999, 1000.000000000000000 ) ;
#35017 = AXIS2_PLACEMENT_3D ( 'NONE', #15750, #9395, #42262 ) ;
#35019 = CARTESIAN_POINT ( 'NONE',  ( -7.250000000000000888, 7.250000000000001776, -21.00000000000000000 ) ) ;
#35018 = DIRECTION ( 'NONE',  ( -1.000000000000000000, 1.047444401652940007E-14, -1.836970198721010706E-16 ) ) ;
#35020 = ORIENTED_EDGE ( 'NONE', *, *, #47527, .T. ) ;
#35022 = ORIENTED_EDGE ( 'NONE', *, *, #41907, .F. ) ;
#35021 = CARTESIAN_POINT ( 'NONE',  ( 7.250000000000005329, -7.249999999999998224, -11.50000000000000000 ) ) ;
#35023 = VERTEX_POINT ( 'NONE', #44007 ) ;
#35024 = ORIENTED_EDGE ( 'NONE', *, *, #6047, .T. ) ;
#35025 = DIRECTION ( 'NONE',  ( 0.000000000000000000, 0.000000000000000000, 1.000000000000000000 ) ) ;
#35026 = EDGE_CURVE ( 'NONE', #65806, #41000, #48631, .T. ) ;
#35027 = CARTESIAN_POINT ( 'NONE',  ( 176.4833316329832940, 0.000000000000000000, 280.6301873289890523 ) ) ;
#35028 = CIRCLE ( 'NONE', #24902, 0.1999999999999987899 ) ;
#35029 = ORIENTED_EDGE ( 'NONE', *, *, #61055, .T. ) ;
#35030 = EDGE_LOOP ( 'NONE', ( #23935, #40350, #8222, #11638 ) ) ;
#35031 = EDGE_CURVE ( 'NONE', #24890, #50924, #6545, .T. ) ;
#35032 = PLANE ( 'NONE',  #55724 ) ;
#35033 = EDGE_CURVE ( 'NONE', #8834, #59416, #45824, .T. ) ;
#35034 = DIRECTION ( 'NONE',  ( 0.000000000000000000, 0.000000000000000000, -1.000000000000000000 ) ) ;
#35035 = ORIENTED_EDGE ( 'NONE', *, *, #69160, .T. ) ;
#35036 = ORIENTED_EDGE ( 'NONE', *, *, #65663, .T. ) ;
#35037 = DIRECTION ( 'NONE',  ( -1.836970198721029934E-16, 1.836970198721036344E-16, -1.000000000000000000 ) ) ;
#35038 = ADVANCED_FACE ( 'NONE', ( #43678 ), #22794, .F. ) ;
#35039 = CYLINDRICAL_SURFACE ( 'NONE', #21486, 3.499999999999999556 ) ;
#35040 = AXIS2_PLACEMENT_3D ( 'NONE', #9948, #10982, #36819 ) ;
#35041 = ORIENTED_EDGE ( 'NONE', *, *, #9106, .T. ) ;
#35042 = VECTOR ( 'NONE', #31989, 1000.000000000000000 ) ;
#35043 = CARTESIAN_POINT ( 'NONE',  ( -6.817976262117325881, -9.737023737882786634, 54.00000000000000711 ) ) ;
#35044 = DIRECTION ( 'NONE',  ( -1.000000000000000000, 8.339399738404101090E-15, -1.836970198721014896E-16 ) ) ;
#35045 = VERTEX_POINT ( 'NONE', #55329 ) ;
#35046 = ORIENTED_EDGE ( 'NONE', *, *, #12729, .F. ) ;
#35047 = CIRCLE ( 'NONE', #41830, 1.620999999999997332 ) ;
#35048 = PLANE ( 'NONE',  #9565 ) ;
#35049 = CARTESIAN_POINT ( 'NONE',  ( 7.000000000000000000, -26.50000000000000000, 0.5000000000000000000 ) ) ;
#35050 = CYLINDRICAL_SURFACE ( 'NONE', #21642, 25.39999999999999858 ) ;
#35051 = DIRECTION ( 'NONE',  ( -1.000000000000000000, 0.000000000000000000, 0.000000000000000000 ) ) ;
#35052 = DIRECTION ( 'NONE',  ( -1.000000000000000000, 0.000000000000000000, 0.000000000000000000 ) ) ;
#35053 = CIRCLE ( 'NONE', #10248, 0.8099999999999999423 ) ;
#35054 = EDGE_CURVE ( 'NONE', #18955, #57411, #56027, .T. ) ;
#35055 = CARTESIAN_POINT ( 'NONE',  ( 2.544523737882787184, -9.562023737882791252, 26.00000000000000000 ) ) ;
#35056 = CARTESIAN_POINT ( 'NONE',  ( -2.752095193409374030, 9.942044687070435316, 195.0000000000000284 ) ) ;
#35057 = VERTEX_POINT ( 'NONE', #38036 ) ;
#35058 = PLANE ( 'NONE',  #58655 ) ;
#35060 = ORIENTED_EDGE ( 'NONE', *, *, #6013, .T. ) ;
#35059 = PLANE ( 'NONE',  #3961 ) ;
#35061 = DIRECTION ( 'NONE',  ( 0.000000000000000000, 1.000000000000000000, 0.000000000000000000 ) ) ;
#35062 = CARTESIAN_POINT ( 'NONE',  ( 14.25000000000000000, -2.500000000000000000, -23.22168783648699986 ) ) ;
#35063 = LINE ( 'NONE', #19162, #43810 ) ;
#35064 = DIRECTION ( 'NONE',  ( -0.000000000000000000, -0.000000000000000000, -1.000000000000000000 ) ) ;
#35065 = AXIS2_PLACEMENT_3D ( 'NONE', #53101, #63703, #9963 ) ;
#35066 = DIRECTION ( 'NONE',  ( 1.000000000000000000, 1.570596175624152290E-15, 5.770276737693577136E-31 ) ) ;
#35067 = ORIENTED_EDGE ( 'NONE', *, *, #30204, .F. ) ;
#35068 = PLANE ( 'NONE',  #4955 ) ;
#35069 = ORIENTED_EDGE ( 'NONE', *, *, #19568, .T. ) ;
#35070 = CARTESIAN_POINT ( 'NONE',  ( -9.689999999999999503, -10.50000000000000178, -5.000000000000000000 ) ) ;
#35071 = EDGE_CURVE ( 'NONE', #40323, #29254, #28103, .T. ) ;
#35072 = CARTESIAN_POINT ( 'NONE',  ( 11.12648345035340647, 7.793516549646564151, 455.0000000000000568 ) ) ;
#35073 = EDGE_CURVE ( 'NONE', #33396, #14490, #27063, .T. ) ;
#35074 = DIRECTION ( 'NONE',  ( 0.000000000000000000, 0.000000000000000000, 1.000000000000000000 ) ) ;
#35075 = ORIENTED_EDGE ( 'NONE', *, *, #10077, .F. ) ;
#35076 = CARTESIAN_POINT ( 'NONE',  ( 7.616533956692213003, -8.406483450353491094, 455.0000000000000568 ) ) ;
#35077 = ORIENTED_EDGE ( 'NONE', *, *, #42792, .F. ) ;
#35078 = EDGE_CURVE ( 'NONE', #32135, #47415, #54994, .T. ) ;
#35079 = ORIENTED_EDGE ( 'NONE', *, *, #39865, .F. ) ;
#35080 = FACE_OUTER_BOUND ( 'NONE', #9834, .T. ) ;
#35081 = PLANE ( 'NONE',  #65836 ) ;
#35082 = ORIENTED_EDGE ( 'NONE', *, *, #495, .T. ) ;
#35083 = DIRECTION ( 'NONE',  ( 1.000000000000000000, -0.000000000000000000, -0.000000000000000000 ) ) ;
#35084 = CARTESIAN_POINT ( 'NONE',  ( 7.250000000000005329, -8.249999999999998224, -26.00000000000001066 ) ) ;
#35085 = CARTESIAN_POINT ( 'NONE',  ( -7.250000000000000888, 7.250000000000001776, -23.00000000000000000 ) ) ;
#35086 = ORIENTED_EDGE ( 'NONE', *, *, #3185, .F. ) ;
#35087 = EDGE_LOOP ( 'NONE', ( #23724, #22879, #11870, #35135 ) ) ;
#35088 = AXIS2_PLACEMENT_3D ( 'NONE', #12522, #7216, #40454 ) ;
#35090 = VERTEX_POINT ( 'NONE', #44686 ) ;
#35089 = DIRECTION ( 'NONE',  ( 0.000000000000000000, 0.000000000000000000, 1.000000000000000000 ) ) ;
#35091 = ORIENTED_EDGE ( 'NONE', *, *, #36256, .F. ) ;
#35092 = CIRCLE ( 'NONE', #48643, 25.39999999999999858 ) ;
#35093 = LINE ( 'NONE', #8226, #4403 ) ;
#35094 = CARTESIAN_POINT ( 'NONE',  ( 9.247904806590689475, -9.955011587777349291, 455.0000000000000568 ) ) ;
#35095 = CARTESIAN_POINT ( 'NONE',  ( -7.250000000000000888, 8.250000000000001776, -15.00000000000000000 ) ) ;
#35096 = DIRECTION ( 'NONE',  ( -1.000000000000000000, 0.000000000000000000, 0.000000000000000000 ) ) ;
#35097 = VECTOR ( 'NONE', #14839, 1000.000000000000000 ) ;
#35098 = FACE_OUTER_BOUND ( 'NONE', #41099, .T. ) ;
#35099 = ORIENTED_EDGE ( 'NONE', *, *, #50077, .F. ) ;
#35100 = ORIENTED_EDGE ( 'NONE', *, *, #34107, .F. ) ;
#35101 = VERTEX_POINT ( 'NONE', #17481 ) ;
#35102 = AXIS2_PLACEMENT_3D ( 'NONE', #48594, #26682, #64862 ) ;
#35103 = AXIS2_PLACEMENT_3D ( 'NONE', #67726, #67026, #68434 ) ;
#35104 = EDGE_LOOP ( 'NONE', ( #53396, #52087, #2692, #49946 ) ) ;
#35105 = DIRECTION ( 'NONE',  ( 0.000000000000000000, 0.000000000000000000, -1.000000000000000000 ) ) ;
#35106 = LINE ( 'NONE', #56340, #63711 ) ;
#35107 = VECTOR ( 'NONE', #67634, 1000.000000000000000 ) ;
#35108 =( NAMED_UNIT ( * ) SI_UNIT ( $, .STERADIAN. ) SOLID_ANGLE_UNIT ( ) );
#35109 = ADVANCED_FACE ( 'NONE', ( #60622 ), #12174, .F. ) ;
#35110 = FACE_OUTER_BOUND ( 'NONE', #48241, .T. ) ;
#35111 = ORIENTED_EDGE ( 'NONE', *, *, #60152, .F. ) ;
#35112 = ORIENTED_EDGE ( 'NONE', *, *, #45389, .T. ) ;
#35113 = ORIENTED_EDGE ( 'NONE', *, *, #50402, .T. ) ;
#35115 = CARTESIAN_POINT ( 'NONE',  ( -15.50000000000000000, -5.000000000000000000, -22.50000000000000000 ) ) ;
#35114 = VECTOR ( 'NONE', #25970, 1000.000000000000000 ) ;
#35116 = ORIENTED_EDGE ( 'NONE', *, *, #52389, .T. ) ;
#35117 = ORIENTED_EDGE ( 'NONE', *, *, #16313, .F. ) ;
#35118 = EDGE_CURVE ( 'NONE', #15458, #14694, #16105, .T. ) ;
#35119 = CARTESIAN_POINT ( 'NONE',  ( 11.00000000000000000, -17.14999999999900027, 27.00000000000000000 ) ) ;
#35120 = EDGE_CURVE ( 'NONE', #64293, #4435, #1814, .T. ) ;
#35121 = ORIENTED_EDGE ( 'NONE', *, *, #38569, .T. ) ;
#35122 = EDGE_LOOP ( 'NONE', ( #67322, #25963, #33584, #52743 ) ) ;
#35123 = DIRECTION ( 'NONE',  ( -8.359604446858499085E-15, -1.000000000000000000, 0.000000000000000000 ) ) ;
#35124 = ADVANCED_FACE ( 'NONE', ( #57052 ), #8613, .F. ) ;
#35125 = ADVANCED_FACE ( 'NONE', ( #7210 ), #24885, .F. ) ;
#35127 = ORIENTED_EDGE ( 'NONE', *, *, #55938, .F. ) ;
#35126 = LINE ( 'NONE', #50351, #1741 ) ;
#35128 = ORIENTED_EDGE ( 'NONE', *, *, #38441, .T. ) ;
#35129 = CARTESIAN_POINT ( 'NONE',  ( 40.90000000000000568, -21.00000000000000000, 13.86939075806900057 ) ) ;
#35130 = DIRECTION ( 'NONE',  ( 0.000000000000000000, 0.000000000000000000, 1.000000000000000000 ) ) ;
#35131 = EDGE_CURVE ( 'NONE', #28954, #31270, #18517, .T. ) ;
#35132 = LINE ( 'NONE', #46449, #49370 ) ;
#35134 = ORIENTED_EDGE ( 'NONE', *, *, #23785, .F. ) ;
#35133 = DIRECTION ( 'NONE',  ( 0.000000000000000000, 0.000000000000000000, -1.000000000000000000 ) ) ;
#35135 = ORIENTED_EDGE ( 'NONE', *, *, #24711, .T. ) ;
#35136 = CARTESIAN_POINT ( 'NONE',  ( 4.456444791733522252E-16, 7.450000000000002842, -23.00000000000000000 ) ) ;
#35137 = DIRECTION ( 'NONE',  ( 0.000000000000000000, 0.7071067811865474617, 0.7071067811865474617 ) ) ;
#35138 = DIRECTION ( 'NONE',  ( 0.000000000000000000, 0.000000000000000000, -1.000000000000000000 ) ) ;
#35139 = VECTOR ( 'NONE', #13138, 1000.000000000000000 ) ;
#35140 = VERTEX_POINT ( 'NONE', #28778 ) ;
#35141 = CARTESIAN_POINT ( 'NONE',  ( 8.144523737882817471, -9.562023737882817898, 54.00000000000000711 ) ) ;
#35142 = DIRECTION ( 'NONE',  ( -1.836970198721029934E-16, 1.836970198721036344E-16, -1.000000000000000000 ) ) ;
#35143 = CIRCLE ( 'NONE', #58847, 0.2000000000000005107 ) ;
#35144 = FACE_OUTER_BOUND ( 'NONE', #29769, .T. ) ;
#35145 = EDGE_LOOP ( 'NONE', ( #7219, #35046, #61826, #57328 ) ) ;
#35146 = CARTESIAN_POINT ( 'NONE',  ( 30.00000000000000000, -9.487228132326899654, 12.50000000000000000 ) ) ;
#35147 = LINE ( 'NONE', #63359, #338 ) ;
#35148 = DIRECTION ( 'NONE',  ( 0.000000000000000000, -1.000000000000000000, 0.000000000000000000 ) ) ;
#35149 = VECTOR ( 'NONE', #25372, 1000.000000000000000 ) ;
#35150 = CLOSED_SHELL ( 'NONE', ( #41873, #46296, #34372, #41789, #66577, #48171, #17499, #65356, #41844, #62627, #29065, #9382, #44401, #29788, #25765, #10126, #6002, #27377, #23222, #47680, #35865, #68392, #21179, #28187, #43638, #30096, #45418, #62892, #20108, #32842, #19812 ) ) ;
#35151 = ORIENTED_EDGE ( 'NONE', *, *, #63292, .F. ) ;
#35152 = CARTESIAN_POINT ( 'NONE',  ( -8.250000000000001776, 7.250000000000000888, -16.50000000000000000 ) ) ;
#35153 = DIRECTION ( 'NONE',  ( 0.000000000000000000, 0.000000000000000000, 1.000000000000000000 ) ) ;
#35154 = AXIS2_PLACEMENT_3D ( 'NONE', #8223, #66239, #24147 ) ;
#35155 = VERTEX_POINT ( 'NONE', #39733 ) ;
#35156 = DIRECTION ( 'NONE',  ( 0.000000000000000000, 0.000000000000000000, 1.000000000000000000 ) ) ;
#35157 = DIRECTION ( 'NONE',  ( -1.000000000000000000, 0.000000000000000000, 0.000000000000000000 ) ) ;
#35158 = DIRECTION ( 'NONE',  ( 0.000000000000000000, -1.000000000000000000, 0.000000000000000000 ) ) ;
#35159 = EDGE_CURVE ( 'NONE', #6950, #44516, #68455, .T. ) ;
#35160 = EDGE_CURVE ( 'NONE', #39463, #4089, #66957, .T. ) ;
#35161 = VECTOR ( 'NONE', #55948, 1000.000000000000000 ) ;
#35162 = DIRECTION ( 'NONE',  ( 1.000000000000000000, -1.828336019306068695E-14, 0.000000000000000000 ) ) ;
#35163 = DIRECTION ( 'NONE',  ( 0.000000000000000000, 1.000000000000000000, 0.000000000000000000 ) ) ;
#35164 = VERTEX_POINT ( 'NONE', #61654 ) ;
#35165 = CARTESIAN_POINT ( 'NONE',  ( -7.250000000000000000, -7.449999999999998401, -12.50000000000000000 ) ) ;
#35166 = FACE_OUTER_BOUND ( 'NONE', #23478, .T. ) ;
#35167 = DIRECTION ( 'NONE',  ( 1.000000000000000000, -0.000000000000000000, -0.000000000000000000 ) ) ;
#35168 = EDGE_CURVE ( 'NONE', #11455, #37156, #50353, .T. ) ;
#35169 = CYLINDRICAL_SURFACE ( 'NONE', #39896, 2.000000000000000000 ) ;
#35170 = DIRECTION ( 'NONE',  ( 0.000000000000000000, 0.000000000000000000, 1.000000000000000000 ) ) ;
#35171 = VERTEX_POINT ( 'NONE', #17837 ) ;
#35173 = VERTEX_POINT ( 'NONE', #51401 ) ;
#35172 = CARTESIAN_POINT ( 'NONE',  ( 7.428221114745003462, -3.006483450353490294, 455.0000000000000568 ) ) ;
#35174 = DIRECTION ( 'NONE',  ( 1.000000000000000000, -0.000000000000000000, 0.000000000000000000 ) ) ;
#35175 = CIRCLE ( 'NONE', #54441, 24.99999999998784972 ) ;
#35176 = CARTESIAN_POINT ( 'NONE',  ( -9.942044687070568543, 9.234937905883914055, 195.0000000000000284 ) ) ;
#35177 = ORIENTED_EDGE ( 'NONE', *, *, #23811, .T. ) ;
#35178 = DIRECTION ( 'NONE',  ( -0.000000000000000000, 0.000000000000000000, 1.000000000000000000 ) ) ;
#35179 = ORIENTED_EDGE ( 'NONE', *, *, #2100, .T. ) ;
#35180 = DIRECTION ( 'NONE',  ( -1.000000000000000000, 0.000000000000000000, 0.000000000000000000 ) ) ;
#35181 = ORIENTED_EDGE ( 'NONE', *, *, #445, .F. ) ;
#35182 = VERTEX_POINT ( 'NONE', #60954 ) ;
#35183 = CARTESIAN_POINT ( 'NONE',  ( 22.14589803375000088, -15.50000000000000000, 21.50000000000000000 ) ) ;
#35184 = VECTOR ( 'NONE', #55848, 1000.000000000000000 ) ;
#35185 = CARTESIAN_POINT ( 'NONE',  ( -4.135079735113167843, 3.663616288757005623, 54.00000000000000711 ) ) ;
#35186 = DIRECTION ( 'NONE',  ( 4.745709458399858621E-16, 1.000000000000000000, 1.836970198721035604E-16 ) ) ;
#35187 = CYLINDRICAL_SURFACE ( 'NONE', #29113, 25.39999999999999858 ) ;
#35188 = ORIENTED_EDGE ( 'NONE', *, *, #48734, .F. ) ;
#35189 = ORIENTED_EDGE ( 'NONE', *, *, #993, .F. ) ;
#35190 = CYLINDRICAL_SURFACE ( 'NONE', #34603, 3.499999999999850342 ) ;
#35191 = PLANE ( 'NONE',  #42914 ) ;
#35192 = ORIENTED_EDGE ( 'NONE', *, *, #21022, .T. ) ;
#35193 = ORIENTED_EDGE ( 'NONE', *, *, #39600, .F. ) ;
#35194 = VECTOR ( 'NONE', #47221, 1000.000000000000000 ) ;
#35195 = AXIS2_PLACEMENT_3D ( 'NONE', #26865, #5976, #53388 ) ;
#35196 = VERTEX_POINT ( 'NONE', #34784 ) ;
#35197 = CYLINDRICAL_SURFACE ( 'NONE', #12408, 0.1999999999999987899 ) ;
#35198 = ADVANCED_FACE ( 'NONE', ( #40797 ), #12514, .T. ) ;
#35200 = ORIENTED_EDGE ( 'NONE', *, *, #14701, .T. ) ;
#35199 = LINE ( 'NONE', #66353, #66544 ) ;
#35201 = ADVANCED_FACE ( 'NONE', ( #51052 ), #13222, .T. ) ;
#35202 = DIRECTION ( 'NONE',  ( 1.280238727658158432E-15, 1.000000000000000000, -0.000000000000000000 ) ) ;
#35203 = DIRECTION ( 'NONE',  ( 0.000000000000000000, 0.000000000000000000, 1.000000000000000000 ) ) ;
#35204 = ADVANCED_FACE ( 'NONE', ( #18171 ), #2269, .F. ) ;
#35205 = EDGE_CURVE ( 'NONE', #33956, #24794, #52667, .T. ) ;
#35206 = VERTEX_POINT ( 'NONE', #7908 ) ;
#35207 = EDGE_LOOP ( 'NONE', ( #15152, #19535, #20107, #35591 ) ) ;
#35208 = VECTOR ( 'NONE', #8456, 1000.000000000000000 ) ;
#35209 = DIRECTION ( 'NONE',  ( 0.000000000000000000, 3.673940397442059868E-16, -1.000000000000000000 ) ) ;
#35210 = CARTESIAN_POINT ( 'NONE',  ( 7.500000000000000000, -25.50000000000000355, 20.00000000000000000 ) ) ;
#35211 = LINE ( 'NONE', #39146, #38320 ) ;
#35212 = ADVANCED_FACE ( 'NONE', ( #29484 ), #3321, .F. ) ;
#35213 = DIRECTION ( 'NONE',  ( -1.000000000000000000, 0.000000000000000000, 0.000000000000000000 ) ) ;
#35214 = FACE_OUTER_BOUND ( 'NONE', #10639, .T. ) ;
#35216 = ORIENTED_EDGE ( 'NONE', *, *, #20663, .T. ) ;
#35215 = PLANE ( 'NONE',  #61354 ) ;
#35217 = ORIENTED_EDGE ( 'NONE', *, *, #7310, .T. ) ;
#35218 = CARTESIAN_POINT ( 'NONE',  ( 41.09999999999999432, 21.00000000000000000, 13.98999642601811999 ) ) ;
#35219 = CARTESIAN_POINT ( 'NONE',  ( -7.281754163448141526, 8.000000000000000000, -1.000000000000000000 ) ) ;
#35220 = CARTESIAN_POINT ( 'NONE',  ( -3.663616288757055806, 6.350872789121238426, 54.00000000000000711 ) ) ;
#35221 = CARTESIAN_POINT ( 'NONE',  ( -10.50000000000000178, 9.690000000000001279, 0.000000000000000000 ) ) ;
#35222 = AXIS2_PLACEMENT_3D ( 'NONE', #61780, #45504, #24654 ) ;
#35223 = DIRECTION ( 'NONE',  ( 0.000000000000000000, 0.000000000000000000, 1.000000000000000000 ) ) ;
#35224 = ORIENTED_EDGE ( 'NONE', *, *, #64219, .T. ) ;
#35225 = DIRECTION ( 'NONE',  ( 0.7071067811865475727, 0.7071067811865475727, 2.597868168706480597E-16 ) ) ;
#35226 = DIRECTION ( 'NONE',  ( 0.000000000000000000, 0.000000000000000000, -1.000000000000000000 ) ) ;
#35227 = AXIS2_PLACEMENT_3D ( 'NONE', #27511, #49076, #64308 ) ;
#35228 = SURFACE_STYLE_USAGE ( .BOTH. , #57514 ) ;
#35229 = CARTESIAN_POINT ( 'NONE',  ( 7.000000000000000000, -23.65000000000000568, 12.40000000000000213 ) ) ;
#35230 = CARTESIAN_POINT ( 'NONE',  ( 15.50000000000000000, -1.037157890325000054, -26.50000000000000000 ) ) ;
#35231 = CARTESIAN_POINT ( 'NONE',  ( 8.711985858128686644, 8.079219948824833963, 54.00000000000000711 ) ) ;
#35232 = AXIS2_PLACEMENT_3D ( 'NONE', #45993, #49900, #24070 ) ;
#35233 = CARTESIAN_POINT ( 'NONE',  ( 8.465062094116069247, -4.255011587777252302, 195.0000000000000284 ) ) ;
#35234 = ORIENTED_EDGE ( 'NONE', *, *, #64801, .F. ) ;
#35235 = CARTESIAN_POINT ( 'NONE',  ( 30.00000000000000000, -11.70000000000012008, 10.70000000000011831 ) ) ;
#35236 = DIRECTION ( 'NONE',  ( -1.000000000000000000, 0.000000000000000000, 0.000000000000000000 ) ) ;
#35237 = ORIENTED_EDGE ( 'NONE', *, *, #1363, .T. ) ;
#35238 = FACE_OUTER_BOUND ( 'NONE', #12722, .T. ) ;
#35239 = VECTOR ( 'NONE', #15390, 1000.000000000000000 ) ;
#35240 = DIRECTION ( 'NONE',  ( 0.000000000000000000, 0.000000000000000000, -1.000000000000000000 ) ) ;
#35241 = EDGE_CURVE ( 'NONE', #39718, #55138, #45738, .T. ) ;
#35242 = CARTESIAN_POINT ( 'NONE',  ( 7.250000000000004441, 7.450000000000001954, -13.00000000000000178 ) ) ;
#35243 = PRESENTATION_STYLE_ASSIGNMENT (( #46563 ) ) ;
#35244 = LINE ( 'NONE', #56826, #18094 ) ;
#35245 = ORIENTED_EDGE ( 'NONE', *, *, #57837, .F. ) ;
#35246 = DIRECTION ( 'NONE',  ( -1.000000000000000000, 0.000000000000000000, 0.000000000000000000 ) ) ;
#35247 = CIRCLE ( 'NONE', #53369, 0.5249999999999994671 ) ;
#35248 = VERTEX_POINT ( 'NONE', #56708 ) ;
#35249 = DIRECTION ( 'NONE',  ( -1.000000000000000000, 0.000000000000000000, 0.000000000000000000 ) ) ;
#35250 = DIRECTION ( 'NONE',  ( 0.000000000000000000, -1.901256929667043247E-12, 1.000000000000000000 ) ) ;
#35251 = ORIENTED_EDGE ( 'NONE', *, *, #64283, .F. ) ;
#35252 = LINE ( 'NONE', #12991, #56259 ) ;
#35253 = VECTOR ( 'NONE', #67076, 1000.000000000000000 ) ;
#35254 = EDGE_CURVE ( 'NONE', #56770, #14563, #8256, .T. ) ;
#35255 = ORIENTED_EDGE ( 'NONE', *, *, #36102, .T. ) ;
#35256 = ADVANCED_FACE ( 'NONE', ( #32888 ), #42801, .F. ) ;
#35257 = DIRECTION ( 'NONE',  ( -0.5000000000000129896, -0.8660254037844311581, -2.509347957447868930E-16 ) ) ;
#35258 = VERTEX_POINT ( 'NONE', #69693 ) ;
#35259 = ORIENTED_EDGE ( 'NONE', *, *, #63512, .T. ) ;
#35260 = DIRECTION ( 'NONE',  ( 0.7071067811865474617, 0.7071067811865474617, 0.000000000000000000 ) ) ;
#35261 = ORIENTED_EDGE ( 'NONE', *, *, #2638, .T. ) ;
#35262 = ORIENTED_EDGE ( 'NONE', *, *, #27070, .T. ) ;
#35263 = CARTESIAN_POINT ( 'NONE',  ( -11.00000000000000000, -11.70000000000000284, 12.50000000000000000 ) ) ;
#35264 = CYLINDRICAL_SURFACE ( 'NONE', #13258, 0.1999999999999987899 ) ;
#35265 = CARTESIAN_POINT ( 'NONE',  ( 7.250000000000005329, 8.250000000000001776, -11.50000000000000000 ) ) ;
#35266 = CIRCLE ( 'NONE', #46588, 1.000000000000003553 ) ;
#35267 = ORIENTED_EDGE ( 'NONE', *, *, #50852, .T. ) ;
#35268 = LINE ( 'NONE', #12656, #6364 ) ;
#35270 = CARTESIAN_POINT ( 'NONE',  ( -11.50000000000000000, -12.00000000000000000, 11.03137303340310282 ) ) ;
#35269 = DIRECTION ( 'NONE',  ( 1.000000000000000000, 0.000000000000000000, 0.000000000000000000 ) ) ;
#35271 = ORIENTED_EDGE ( 'NONE', *, *, #44090, .F. ) ;
#35273 = VERTEX_POINT ( 'NONE', #21931 ) ;
#35272 = PLANE ( 'NONE',  #27493 ) ;
#35274 = ORIENTED_EDGE ( 'NONE', *, *, #38629, .F. ) ;
#35275 = SHAPE_DEFINITION_REPRESENTATION ( #21647, #14183 ) ;
#35276 = DIRECTION ( 'NONE',  ( 1.000000000000000000, 0.000000000000000000, 0.000000000000000000 ) ) ;
#35277 = ORIENTED_EDGE ( 'NONE', *, *, #17948, .F. ) ;
#35278 = EDGE_CURVE ( 'NONE', #12942, #66121, #31861, .T. ) ;
#35279 = DIRECTION ( 'NONE',  ( 0.000000000000000000, -1.000000000000000000, 0.000000000000000000 ) ) ;
#35280 = CARTESIAN_POINT ( 'NONE',  ( 8.406483450353356091, 6.331612867284063917, 195.0000000000000284 ) ) ;
#35281 = EDGE_CURVE ( 'NONE', #48070, #2815, #53425, .T. ) ;
#35282 = ORIENTED_EDGE ( 'NONE', *, *, #55303, .T. ) ;
#35283 = ADVANCED_FACE ( 'NONE', ( #21591 ), #64045, .T. ) ;
#35284 = EDGE_LOOP ( 'NONE', ( #10009, #54276, #3186, #65665, #17666, #17780 ) ) ;
#35285 = AXIS2_PLACEMENT_3D ( 'NONE', #63674, #51656, #3918 ) ;
#35286 = DIRECTION ( 'NONE',  ( 0.000000000000000000, 0.000000000000000000, 1.000000000000000000 ) ) ;
#35287 = FACE_OUTER_BOUND ( 'NONE', #57751, .T. ) ;
#35288 = ADVANCED_FACE ( 'NONE', ( #68020 ), #48460, .F. ) ;
#35289 = EDGE_LOOP ( 'NONE', ( #56355, #9098, #14226, #53515, #9006, #7441, #17276, #44903 ) ) ;
#35290 = DIRECTION ( 'NONE',  ( 0.000000000000000000, -3.673940397442059868E-16, 1.000000000000000000 ) ) ;
#35291 = DIRECTION ( 'NONE',  ( 0.000000000000000000, -0.7071067811865475727, 0.7071067811865475727 ) ) ;
#35292 = EDGE_CURVE ( 'NONE', #58614, #37156, #58728, .T. ) ;
#35293 = CARTESIAN_POINT ( 'NONE',  ( 17.00000000000000000, -15.50000000000000000, 14.50000000000000000 ) ) ;
#35294 = ORIENTED_EDGE ( 'NONE', *, *, #62355, .T. ) ;
#35295 = EDGE_CURVE ( 'NONE', #68514, #11420, #65079, .T. ) ;
#35296 = AXIS2_PLACEMENT_3D ( 'NONE', #61793, #13353, #14043 ) ;
#35297 = LINE ( 'NONE', #46618, #14329 ) ;
#35298 = CARTESIAN_POINT ( 'NONE',  ( 30.00000000000000000, -16.28999999999999915, -14.50000000000000000 ) ) ;
#35300 = ORIENTED_EDGE ( 'NONE', *, *, #25751, .T. ) ;
#35299 = LINE ( 'NONE', #56880, #48930 ) ;
#35302 = VERTEX_POINT ( 'NONE', #4978 ) ;
#35301 = CARTESIAN_POINT ( 'NONE',  ( -8.250000000000001776, -7.249999999999998224, -25.50000000000000355 ) ) ;
#35304 = FACE_OUTER_BOUND ( 'NONE', #41953, .T. ) ;
#35303 = VECTOR ( 'NONE', #51441, 1000.000000000000000 ) ;
#35305 = AXIS2_PLACEMENT_3D ( 'NONE', #13348, #56479, #9096 ) ;
#35306 = DIRECTION ( 'NONE',  ( 1.000000000000000000, 0.000000000000000000, 0.000000000000000000 ) ) ;
#35307 = CARTESIAN_POINT ( 'NONE',  ( 30.00000000000000000, -9.199999999999999289, -12.34999999999989839 ) ) ;
#35308 = DIRECTION ( 'NONE',  ( 0.000000000000000000, 0.000000000000000000, 1.000000000000000000 ) ) ;
#35309 = CIRCLE ( 'NONE', #53427, 0.1749999999999998224 ) ;
#35310 = DIRECTION ( 'NONE',  ( 1.000000000000000000, -0.000000000000000000, 0.000000000000000000 ) ) ;
#35311 = VERTEX_POINT ( 'NONE', #14282 ) ;
#35312 = LINE ( 'NONE', #34268, #18801 ) ;
#35313 = DIRECTION ( 'NONE',  ( -1.000000000000000000, 2.602085213965213008E-15, 0.000000000000000000 ) ) ;
#35314 = FACE_OUTER_BOUND ( 'NONE', #45400, .T. ) ;
#35316 = ORIENTED_EDGE ( 'NONE', *, *, #46976, .F. ) ;
#35315 = CYLINDRICAL_SURFACE ( 'NONE', #63852, 4.000000000000000000 ) ;
#35317 = DIRECTION ( 'NONE',  ( 1.836970198721029934E-16, 1.836970198721010706E-16, -1.000000000000000000 ) ) ;
#35318 = AXIS2_PLACEMENT_3D ( 'NONE', #59065, #20188, #26545 ) ;
#35319 = EDGE_CURVE ( 'NONE', #19180, #14864, #45928, .T. ) ;
#35320 = CYLINDRICAL_SURFACE ( 'NONE', #14952, 0.3000000000005393908 ) ;
#35321 = ORIENTED_EDGE ( 'NONE', *, *, #11685, .T. ) ;
#35322 = VERTEX_POINT ( 'NONE', #41140 ) ;
#35323 = PLANE ( 'NONE',  #20735 ) ;
#35324 = DIRECTION ( 'NONE',  ( 1.000000000000000000, 0.000000000000000000, 0.000000000000000000 ) ) ;
#35325 = VECTOR ( 'NONE', #46829, 1000.000000000000000 ) ;
#35326 = EDGE_LOOP ( 'NONE', ( #6113, #16708, #7762, #35634 ) ) ;
#35327 = EDGE_CURVE ( 'NONE', #48708, #37841, #52108, .T. ) ;
#35328 = DIRECTION ( 'NONE',  ( 7.808916176531286882E-15, 1.000000000000000000, 0.000000000000000000 ) ) ;
#35329 = LINE ( 'NONE', #56904, #54704 ) ;
#35330 = AXIS2_PLACEMENT_3D ( 'NONE', #66175, #17739, #55912 ) ;
#35331 = DIRECTION ( 'NONE',  ( -0.000000000000000000, 3.673940397442059868E-16, -1.000000000000000000 ) ) ;
#35332 = EDGE_CURVE ( 'NONE', #1311, #7275, #31, .T. ) ;
#35333 = CARTESIAN_POINT ( 'NONE',  ( 7.450000000000006395, 7.250000000000000888, -8.000000000000000000 ) ) ;
#35334 = ORIENTED_EDGE ( 'NONE', *, *, #59185, .T. ) ;
#35335 = CARTESIAN_POINT ( 'NONE',  ( 7.450000000000003730, -7.249999999999997335, -18.50000000000000000 ) ) ;
#35336 = VERTEX_POINT ( 'NONE', #5344 ) ;
#35337 = LINE ( 'NONE', #56913, #26197 ) ;
#35338 = ORIENTED_EDGE ( 'NONE', *, *, #42090, .F. ) ;
#35339 = DIRECTION ( 'NONE',  ( 0.000000000000000000, 0.000000000000000000, -1.000000000000000000 ) ) ;
#35340 = DIRECTION ( 'NONE',  ( -5.981805089575196197E-17, -1.000000000000000000, 0.000000000000000000 ) ) ;
#35341 = EDGE_CURVE ( 'NONE', #41169, #27481, #16278, .T. ) ;
#35342 = FACE_OUTER_BOUND ( 'NONE', #19190, .T. ) ;
#35343 = ORIENTED_EDGE ( 'NONE', *, *, #5300, .F. ) ;
#35344 = ORIENTED_EDGE ( 'NONE', *, *, #23166, .T. ) ;
#35345 = CARTESIAN_POINT ( 'NONE',  ( 3.430747519065294071, -7.852485183457023510, 455.0000000000000568 ) ) ;
#35346 = ORIENTED_EDGE ( 'NONE', *, *, #60434, .F. ) ;
#35347 = VERTEX_POINT ( 'NONE', #368 ) ;
#35348 = DIRECTION ( 'NONE',  ( 1.000000000000000000, 0.000000000000000000, 0.000000000000000000 ) ) ;
#35349 = DIRECTION ( 'NONE',  ( 1.000000000000000000, -0.000000000000000000, 0.000000000000000000 ) ) ;
#35350 = CONICAL_SURFACE ( 'NONE', #13867, 1732.050807568785558, 1.047197551196574761 ) ;
#35351 = CARTESIAN_POINT ( 'NONE',  ( 25.50000000000000355, -15.50000000000000000, 22.50000000000000000 ) ) ;
#35352 = DIRECTION ( 'NONE',  ( 1.000000000000000000, -1.952517519553884087E-14, 1.836970198720994435E-16 ) ) ;
#35353 = EDGE_CURVE ( 'NONE', #15205, #52522, #59066, .T. ) ;
#35354 = VERTEX_POINT ( 'NONE', #38213 ) ;
#35355 = EDGE_CURVE ( 'NONE', #16502, #29534, #32195, .T. ) ;
#35356 = VECTOR ( 'NONE', #56571, 1000.000000000000227 ) ;
#35357 = CARTESIAN_POINT ( 'NONE',  ( -11.99351654964671354, 7.813516549646603693, 195.0000000000000284 ) ) ;
#35359 = LINE ( 'NONE', #57650, #7452 ) ;
#35358 = CARTESIAN_POINT ( 'NONE',  ( 4.186483450353337687, -11.78648345035347589, 455.0000000000000568 ) ) ;
#35360 = AXIS2_PLACEMENT_3D ( 'NONE', #67705, #56055, #8664 ) ;
#35362 = ORIENTED_EDGE ( 'NONE', *, *, #69062, .F. ) ;
#35361 = AXIS2_PLACEMENT_3D ( 'NONE', #19208, #40433, #61986 ) ;
#35365 = EDGE_CURVE ( 'NONE', #13975, #23202, #69327, .T. ) ;
#35364 = ORIENTED_EDGE ( 'NONE', *, *, #21107, .T. ) ;
#35363 = DIRECTION ( 'NONE',  ( 0.000000000000000000, 0.000000000000000000, 1.000000000000000000 ) ) ;
#35366 = VERTEX_POINT ( 'NONE', #10981 ) ;
#35367 = VERTEX_POINT ( 'NONE', #3672 ) ;
#35368 = EDGE_CURVE ( 'NONE', #62314, #4508, #54122, .T. ) ;
#35369 = EDGE_CURVE ( 'NONE', #2424, #34152, #4157, .T. ) ;
#35370 =( GEOMETRIC_REPRESENTATION_CONTEXT ( 3 ) GLOBAL_UNCERTAINTY_ASSIGNED_CONTEXT ( ( #41576 ) ) GLOBAL_UNIT_ASSIGNED_CONTEXT ( ( #22887, #61045, #55086 ) ) REPRESENTATION_CONTEXT ( 'NONE', 'WORKASPACE' ) );
#35371 = AXIS2_PLACEMENT_3D ( 'NONE', #48312, #219, #10472 ) ;
#35372 = CARTESIAN_POINT ( 'NONE',  ( 283.0000000000000568, -40.30000000000000426, -8.900000000000000355 ) ) ;
#35373 = ADVANCED_FACE ( 'NONE', ( #27932 ), #27581, .T. ) ;
#35374 = CARTESIAN_POINT ( 'NONE',  ( 39.00000000000000000, 0.000000000000000000, 0.000000000000000000 ) ) ;
#35375 = EDGE_CURVE ( 'NONE', #37989, #38190, #54989, .T. ) ;
#35376 = ORIENTED_EDGE ( 'NONE', *, *, #6094, .T. ) ;
#35377 = ORIENTED_EDGE ( 'NONE', *, *, #44000, .F. ) ;
#35378 = EDGE_CURVE ( 'NONE', #55218, #4451, #60098, .T. ) ;
#35379 = LINE ( 'NONE', #4631, #3691 ) ;
#35380 = DIRECTION ( 'NONE',  ( 0.000000000000000000, 0.7084617869628681008, -0.7057491738665939707 ) ) ;
#35381 = VECTOR ( 'NONE', #60830, 999.9999999999998863 ) ;
#35382 = VERTEX_POINT ( 'NONE', #38546 ) ;
#35383 = EDGE_LOOP ( 'NONE', ( #32294, #30687, #63514, #1016 ) ) ;
#35384 = CARTESIAN_POINT ( 'NONE',  ( 7.000000000000000000, -26.50000000000000000, 9.080000000000000071 ) ) ;
#35385 = EDGE_CURVE ( 'NONE', #30244, #53683, #50535, .T. ) ;
#35386 = LINE ( 'NONE', #29739, #10238 ) ;
#35387 = ORIENTED_EDGE ( 'NONE', *, *, #21423, .T. ) ;
#35388 = EDGE_CURVE ( 'NONE', #18763, #3647, #65755, .T. ) ;
#35389 = CARTESIAN_POINT ( 'NONE',  ( -9.690000000000001279, 9.690000000000001279, 0.000000000000000000 ) ) ;
#35390 = CARTESIAN_POINT ( 'NONE',  ( -8.130476262117316111, -8.835729544836294025, 54.00000000000000711 ) ) ;
#35391 = AXIS2_PLACEMENT_3D ( 'NONE', #56737, #35157, #28809 ) ;
#35393 = ORIENTED_EDGE ( 'NONE', *, *, #68265, .F. ) ;
#35392 = SURFACE_STYLE_FILL_AREA ( #14899 ) ;
#35394 = VERTEX_POINT ( 'NONE', #54804 ) ;
#35395 = DIRECTION ( 'NONE',  ( 0.000000000000000000, 0.000000000000000000, 1.000000000000000000 ) ) ;
#35396 = PRESENTATION_STYLE_ASSIGNMENT (( #32478 ) ) ;
#35397 = LINE ( 'NONE', #25519, #39682 ) ;
#35398 = ADVANCED_FACE ( 'NONE', ( #23313 ), #61471, .F. ) ;
#35399 = LINE ( 'NONE', #67243, #3044 ) ;
#35400 = LINE ( 'NONE', #61219, #59464 ) ;
#35401 = DIRECTION ( 'NONE',  ( -0.000000000000000000, 1.000000000000000000, -0.000000000000000000 ) ) ;
#35402 = CARTESIAN_POINT ( 'NONE',  ( 11.50000000000000000, -11.50000000000100009, 15.00000000000084910 ) ) ;
#35403 = ORIENTED_EDGE ( 'NONE', *, *, #9346, .F. ) ;
#35404 = CARTESIAN_POINT ( 'NONE',  ( 146.5599459900709860, 9.000000000000001776, 284.4801873289890182 ) ) ;
#35406 = VERTEX_POINT ( 'NONE', #11993 ) ;
#35405 = CARTESIAN_POINT ( 'NONE',  ( 7.250000000000005329, 8.250000000000001776, -18.50000000000000000 ) ) ;
#35407 = DIRECTION ( 'NONE',  ( 0.4999999999999827360, 0.000000000000000000, -0.8660254037844485886 ) ) ;
#35408 = AXIS2_PLACEMENT_3D ( 'NONE', #13775, #45957, #12710 ) ;
#35409 = VECTOR ( 'NONE', #13284, 1000.000000000000000 ) ;
#35410 = CARTESIAN_POINT ( 'NONE',  ( 30.00000000000000000, -15.46862696659690073, 14.50000000000000000 ) ) ;
#35411 = DIRECTION ( 'NONE',  ( -0.5773502691896257311, -0.5773502691896257311, 0.5773502691896257311 ) ) ;
#35412 = CARTESIAN_POINT ( 'NONE',  ( -7.250000000000000888, 7.250000000000001776, -12.50000000000000000 ) ) ;
#35413 = VECTOR ( 'NONE', #66236, 1000.000000000000000 ) ;
#35414 = DIRECTION ( 'NONE',  ( 1.000000000000000000, 0.000000000000000000, 0.000000000000000000 ) ) ;
#35415 = AXIS2_PLACEMENT_3D ( 'NONE', #46278, #67853, #56539 ) ;
#35416 = ORIENTED_EDGE ( 'NONE', *, *, #57655, .F. ) ;
#35417 = CARTESIAN_POINT ( 'NONE',  ( 280.0000000000000000, -53.81370849898476649, -20.00000000000000000 ) ) ;
#35418 = CARTESIAN_POINT ( 'NONE',  ( 11.75000000000000000, -5.200000000000001066, 60.00000000000000000 ) ) ;
#35419 = EDGE_LOOP ( 'NONE', ( #23141, #45943, #49029, #40580 ) ) ;
#35420 = ADVANCED_FACE ( 'NONE', ( #11647 ), #55152, .T. ) ;
#35421 = AXIS2_PLACEMENT_3D ( 'NONE', #21650, #32948, #432 ) ;
#35422 = CARTESIAN_POINT ( 'NONE',  ( 4.740315990920131561, -7.811466277050838514, 455.0000000000000568 ) ) ;
#35423 = EDGE_CURVE ( 'NONE', #21985, #59322, #67386, .T. ) ;
#35424 = CARTESIAN_POINT ( 'NONE',  ( -17.51999999999999957, -15.50000000000000000, 26.00000000000000355 ) ) ;
#35425 = ORIENTED_EDGE ( 'NONE', *, *, #26010, .F. ) ;
#35426 = CARTESIAN_POINT ( 'NONE',  ( 9.249999999999998224, -7.848062532927998269, 0.000000000000000000 ) ) ;
#35427 = ORIENTED_EDGE ( 'NONE', *, *, #46913, .T. ) ;
#35428 = ADVANCED_FACE ( 'NONE', ( #56189 ), #44514, .F. ) ;
#35429 = ORIENTED_EDGE ( 'NONE', *, *, #42670, .F. ) ;
#35430 = CYLINDRICAL_SURFACE ( 'NONE', #57272, 0.3500000000009988455 ) ;
#35431 = CARTESIAN_POINT ( 'NONE',  ( 7.357023737882778747, 3.834182069070702692, 26.00000000000000711 ) ) ;
#35432 = LINE ( 'NONE', #8567, #22050 ) ;
#35433 = EDGE_CURVE ( 'NONE', #46362, #45646, #30084, .T. ) ;
#35434 = DIRECTION ( 'NONE',  ( 0.000000000000000000, 0.000000000000000000, 1.000000000000000000 ) ) ;
#35435 = EDGE_CURVE ( 'NONE', #10988, #24256, #62839, .T. ) ;
#35436 = LINE ( 'NONE', #2926, #67880 ) ;
#35437 = EDGE_LOOP ( 'NONE', ( #61715, #27906, #5647, #11622, #56949, #38259 ) ) ;
#35438 = ORIENTED_EDGE ( 'NONE', *, *, #47606, .F. ) ;
#35440 = ORIENTED_EDGE ( 'NONE', *, *, #47460, .F. ) ;
#35439 = DIRECTION ( 'NONE',  ( 1.000000000000000000, 0.000000000000000000, 0.000000000000000000 ) ) ;
#35441 = VERTEX_POINT ( 'NONE', #17663 ) ;
#35442 = CARTESIAN_POINT ( 'NONE',  ( -7.250000000000000888, 7.250000000000001776, -23.00000000000000000 ) ) ;
#35443 = DIRECTION ( 'NONE',  ( -0.7071067811865474617, 0.7071067811865474617, 0.000000000000000000 ) ) ;
#35444 = CARTESIAN_POINT ( 'NONE',  ( 15.50000000000129852, -15.50000000000000000, 22.50000000000000000 ) ) ;
#35445 = DIRECTION ( 'NONE',  ( 1.000000000000000000, -5.981805089575194965E-17, 0.000000000000000000 ) ) ;
#35446 = CIRCLE ( 'NONE', #494, 1.000000000000000000 ) ;
#35447 = DIRECTION ( 'NONE',  ( 1.836970198721029934E-16, 1.836970198721010706E-16, -1.000000000000000000 ) ) ;
#35448 = LINE ( 'NONE', #61266, #34132 ) ;
#35449 = VERTEX_POINT ( 'NONE', #60788 ) ;
#35450 = MECHANICAL_DESIGN_GEOMETRIC_PRESENTATION_REPRESENTATION (  '', ( #4992 ), #45640 ) ;
#35451 = EDGE_LOOP ( 'NONE', ( #20679, #36125, #1820, #68858 ) ) ;
#35452 = ORIENTED_EDGE ( 'NONE', *, *, #26774, .T. ) ;
#35453 = EDGE_CURVE ( 'NONE', #13195, #67463, #19942, .T. ) ;
#35454 = EDGE_LOOP ( 'NONE', ( #17885, #23345, #62431, #53941 ) ) ;
#35455 = CARTESIAN_POINT ( 'NONE',  ( 25.50000000000000355, -15.50000000000000000, -22.50000000000000000 ) ) ;
#35456 = DIRECTION ( 'NONE',  ( 8.673617379884030739E-15, 1.000000000000000000, 0.000000000000000000 ) ) ;
#35457 = VECTOR ( 'NONE', #54750, 1000.000000000000000 ) ;
#35459 = DIRECTION ( 'NONE',  ( -3.491481338843133355E-15, -1.000000000000000000, -1.836970198721029934E-16 ) ) ;
#35458 = AXIS2_PLACEMENT_3D ( 'NONE', #65897, #7183, #66256 ) ;
#35460 = VERTEX_POINT ( 'NONE', #12333 ) ;
#35461 = ORIENTED_EDGE ( 'NONE', *, *, #29316, .F. ) ;
#35462 = EDGE_LOOP ( 'NONE', ( #49386, #69154, #55959, #38159 ) ) ;
#35463 = CARTESIAN_POINT ( 'NONE',  ( 10.90000000000000036, -14.06939075806900163, -20.80000000000000426 ) ) ;
#35464 = ORIENTED_EDGE ( 'NONE', *, *, #931, .F. ) ;
#35465 = CIRCLE ( 'NONE', #6162, 24.99999999998794920 ) ;
#35466 = CIRCLE ( 'NONE', #29822, 24.99999999998784972 ) ;
#35467 = VERTEX_POINT ( 'NONE', #33910 ) ;
#35468 = CARTESIAN_POINT ( 'NONE',  ( 39.00000000000000000, -16.96999999999999886, 21.00000000000000000 ) ) ;
#35469 = ORIENTED_EDGE ( 'NONE', *, *, #46609, .F. ) ;
#35470 = VERTEX_POINT ( 'NONE', #50180 ) ;
#35471 = DIRECTION ( 'NONE',  ( -1.000000000000000000, 0.000000000000000000, 0.000000000000000000 ) ) ;
#35472 = CIRCLE ( 'NONE', #11754, 0.9999999999999991118 ) ;
#35473 = ADVANCED_FACE ( 'NONE', ( #1736, #66445 ), #13030, .F. ) ;
#35475 = VERTEX_POINT ( 'NONE', #55835 ) ;
#35474 = CARTESIAN_POINT ( 'NONE',  ( -10.30047626211725031, -3.857023737882713466, 54.00000000000000711 ) ) ;
#35476 = ORIENTED_EDGE ( 'NONE', *, *, #17117, .T. ) ;
#35477 = DIRECTION ( 'NONE',  ( -1.000000000000000000, 0.000000000000000000, 0.000000000000000000 ) ) ;
#35478 = EDGE_CURVE ( 'NONE', #23929, #34893, #7382, .T. ) ;
#35479 = CARTESIAN_POINT ( 'NONE',  ( 152.5922698879801942, -30.42541106249862537, 5.000000000000000000 ) ) ;
#35480 = VECTOR ( 'NONE', #3417, 1000.000000000000000 ) ;
#35481 = CARTESIAN_POINT ( 'NONE',  ( -3.842976262117332453, -10.31452373788281740, 54.00000000000000711 ) ) ;
#35483 = ORIENTED_EDGE ( 'NONE', *, *, #51972, .F. ) ;
#35482 = DIRECTION ( 'NONE',  ( -1.836970198721029934E-16, -1.836970198721010706E-16, 1.000000000000000000 ) ) ;
#35484 = AXIS2_PLACEMENT_3D ( 'NONE', #29804, #51373, #2938 ) ;
#35485 = VERTEX_POINT ( 'NONE', #727 ) ;
#35486 = FACE_OUTER_BOUND ( 'NONE', #32660, .T. ) ;
#35487 = CARTESIAN_POINT ( 'NONE',  ( 9.737023737882816832, -6.832023737882823688, 54.00000000000000711 ) ) ;
#35488 = DIRECTION ( 'NONE',  ( -1.000000000000000000, 0.000000000000000000, 0.000000000000000000 ) ) ;
#35489 = ORIENTED_EDGE ( 'NONE', *, *, #31296, .T. ) ;
#35490 = CARTESIAN_POINT ( 'NONE',  ( 50.83090410532631864, 3.657408540445007628, 2.000000000000000000 ) ) ;
#35491 = LINE ( 'NONE', #47177, #53572 ) ;
#35492 = CARTESIAN_POINT ( 'NONE',  ( 8.250000000000005329, -7.249999999999998224, -8.000000000000000000 ) ) ;
#35493 = ORIENTED_EDGE ( 'NONE', *, *, #2972, .F. ) ;
#35494 = DIRECTION ( 'NONE',  ( 0.000000000000000000, 1.000000000000000000, 0.000000000000000000 ) ) ;
#35495 = PLANE ( 'NONE',  #29474 ) ;
#35496 = CARTESIAN_POINT ( 'NONE',  ( 8.249999999999996447, 8.250000000000001776, 0.000000000000000000 ) ) ;
#35497 = ORIENTED_EDGE ( 'NONE', *, *, #46528, .F. ) ;
#35498 = CARTESIAN_POINT ( 'NONE',  ( 1.690483450353344352, -10.74648345035345720, 455.0000000000000568 ) ) ;
#35499 = FACE_OUTER_BOUND ( 'NONE', #14261, .T. ) ;
#35500 = EDGE_CURVE ( 'NONE', #30976, #55205, #16977, .T. ) ;
#35501 = AXIS2_PLACEMENT_3D ( 'NONE', #19266, #31301, #40832 ) ;
#35502 = AXIS2_PLACEMENT_3D ( 'NONE', #63679, #42091, #51660 ) ;
#35503 = DIRECTION ( 'NONE',  ( -1.000000000000000000, 0.000000000000000000, 0.000000000000000000 ) ) ;
#35504 = ORIENTED_EDGE ( 'NONE', *, *, #47440, .F. ) ;
#35505 = PLANE ( 'NONE',  #38323 ) ;
#35506 = CARTESIAN_POINT ( 'NONE',  ( 17.00000000000000000, -16.64230188589299786, -14.64519951917100116 ) ) ;
#35507 = FACE_OUTER_BOUND ( 'NONE', #14075, .T. ) ;
#35508 = ADVANCED_FACE ( 'NONE', ( #7733 ), #2986, .T. ) ;
#35509 = CARTESIAN_POINT ( 'NONE',  ( -15.50000000000000000, -2.500000000000000000, -23.94337567297399971 ) ) ;
#35510 = FACE_OUTER_BOUND ( 'NONE', #6426, .T. ) ;
#35511 = VECTOR ( 'NONE', #33629, 1000.000000000000000 ) ;
#35512 = ORIENTED_EDGE ( 'NONE', *, *, #11202, .F. ) ;
#35513 = AXIS2_PLACEMENT_3D ( 'NONE', #47950, #20031, #69519 ) ;
#35514 = CARTESIAN_POINT ( 'NONE',  ( -28.00000000000000000, -17.50000000000000000, 15.70499999999969809 ) ) ;
#35515 = DIRECTION ( 'NONE',  ( -0.000000000000000000, -0.000000000000000000, -1.000000000000000000 ) ) ;
#35516 = ADVANCED_FACE ( 'NONE', ( #2439 ), #24356, .F. ) ;
#35517 = EDGE_CURVE ( 'NONE', #7472, #64694, #52726, .T. ) ;
#35518 = DIRECTION ( 'NONE',  ( 0.000000000000000000, 0.000000000000000000, -1.000000000000000000 ) ) ;
#35519 = AXIS2_PLACEMENT_3D ( 'NONE', #2755, #46243, #46944 ) ;
#35520 = EDGE_CURVE ( 'NONE', #15650, #9312, #13395, .T. ) ;
#35521 = CARTESIAN_POINT ( 'NONE',  ( 30.90000000000000213, 3.010794155703768650E-16, -2.458500000000000796 ) ) ;
#35522 = EDGE_CURVE ( 'NONE', #36902, #19691, #56531, .T. ) ;
#35523 = VERTEX_POINT ( 'NONE', #52282 ) ;
#35525 = VERTEX_POINT ( 'NONE', #45927 ) ;
#35524 = DIRECTION ( 'NONE',  ( -0.7071067811865476838, -0.4999999999999997780, 0.4999999999999997780 ) ) ;
#35526 = STYLED_ITEM ( 'NONE', ( #40107 ), #44406 ) ;
#35527 = EDGE_CURVE ( 'NONE', #30476, #53367, #67845, .T. ) ;
#35528 = DIRECTION ( 'NONE',  ( 0.000000000000000000, 1.000000000000000000, 0.000000000000000000 ) ) ;
#35529 = LINE ( 'NONE', #62761, #27844 ) ;
#35530 = AXIS2_PLACEMENT_3D ( 'NONE', #23054, #44608, #12774 ) ;
#35531 = FACE_OUTER_BOUND ( 'NONE', #55905, .T. ) ;
#35532 = EDGE_LOOP ( 'NONE', ( #35338, #28039 ) ) ;
#35533 = CIRCLE ( 'NONE', #44562, 3.500000000000114131 ) ;
#35534 = CYLINDRICAL_SURFACE ( 'NONE', #16052, 0.1999999999999987899 ) ;
#35535 = VERTEX_POINT ( 'NONE', #19053 ) ;
#35536 = ORIENTED_EDGE ( 'NONE', *, *, #59508, .T. ) ;
#35537 = ORIENTED_EDGE ( 'NONE', *, *, #859, .F. ) ;
#35538 = DIRECTION ( 'NONE',  ( 9.912705577010336396E-15, 1.000000000000000000, 0.000000000000000000 ) ) ;
#35539 = DIRECTION ( 'NONE',  ( -0.000000000000000000, 1.000000000000000000, -0.000000000000000000 ) ) ;
#35540 = DIRECTION ( 'NONE',  ( 0.000000000000000000, 0.000000000000000000, 1.000000000000000000 ) ) ;
#35541 = DIRECTION ( 'NONE',  ( -1.000000000000000000, 0.000000000000000000, 0.000000000000000000 ) ) ;
#35542 = VERTEX_POINT ( 'NONE', #19395 ) ;
#35543 = ORIENTED_EDGE ( 'NONE', *, *, #15594, .T. ) ;
#35544 = DIRECTION ( 'NONE',  ( 1.047444401652940007E-14, 1.000000000000000000, 0.000000000000000000 ) ) ;
#35545 = FACE_OUTER_BOUND ( 'NONE', #67491, .T. ) ;
#35546 = ORIENTED_EDGE ( 'NONE', *, *, #62930, .T. ) ;
#35547 = AXIS2_PLACEMENT_3D ( 'NONE', #68412, #25274, #20318 ) ;
#35548 = ORIENTED_EDGE ( 'NONE', *, *, #50003, .F. ) ;
#35549 = ORIENTED_EDGE ( 'NONE', *, *, #19474, .T. ) ;
#35550 = EDGE_LOOP ( 'NONE', ( #54218, #23565, #24683, #68159 ) ) ;
#35551 = CARTESIAN_POINT ( 'NONE',  ( 29.50000000000000355, -12.00000000000000000, 10.52786404500095863 ) ) ;
#35553 = ORIENTED_EDGE ( 'NONE', *, *, #31049, .F. ) ;
#35552 = LINE ( 'NONE', #30618, #12984 ) ;
#35554 = DIRECTION ( 'NONE',  ( 0.000000000000000000, 0.000000000000000000, -1.000000000000000000 ) ) ;
#35555 = EDGE_CURVE ( 'NONE', #3823, #67986, #51935, .T. ) ;
#35556 = AXIS2_PLACEMENT_3D ( 'NONE', #30119, #40730, #30822 ) ;
#35557 = VECTOR ( 'NONE', #52728, 1000.000000000000000 ) ;
#35558 = DIRECTION ( 'NONE',  ( -0.000000000000000000, 3.673940397442059868E-16, -1.000000000000000000 ) ) ;
#35559 = CIRCLE ( 'NONE', #14119, 0.3499999999999996447 ) ;
#35560 = ORIENTED_EDGE ( 'NONE', *, *, #64536, .T. ) ;
#35561 = EDGE_CURVE ( 'NONE', #23661, #5435, #67506, .T. ) ;
#35562 = ORIENTED_EDGE ( 'NONE', *, *, #48521, .T. ) ;
#35563 = EDGE_CURVE ( 'NONE', #17133, #29536, #49335, .T. ) ;
#35564 = AXIS2_PLACEMENT_3D ( 'NONE', #56851, #61825, #24339 ) ;
#35565 = AXIS2_PLACEMENT_3D ( 'NONE', #68605, #63295, #30413 ) ;
#35566 = EDGE_CURVE ( 'NONE', #62792, #26698, #68503, .T. ) ;
#35567 = DIRECTION ( 'NONE',  ( -1.000000000000000000, 0.000000000000000000, 0.000000000000000000 ) ) ;
#35568 = CARTESIAN_POINT ( 'NONE',  ( 17.89999999999999858, -0.000000000000000000, 20.80000000000000426 ) ) ;
#35569 = CIRCLE ( 'NONE', #68351, 1.620999999999997332 ) ;
#35570 = DIRECTION ( 'NONE',  ( 0.000000000000000000, 0.000000000000000000, 1.000000000000000000 ) ) ;
#35571 = AXIS2_PLACEMENT_3D ( 'NONE', #1186, #61239, #55272 ) ;
#35572 = CARTESIAN_POINT ( 'NONE',  ( 5.257023737882819070, -3.157023737882825198, 54.00000000000000711 ) ) ;
#35573 = CARTESIAN_POINT ( 'NONE',  ( 39.00000000000000000, -16.96999999999999886, -21.00000000000000000 ) ) ;
#35574 = ORIENTED_EDGE ( 'NONE', *, *, #16643, .F. ) ;
#35575 = ORIENTED_EDGE ( 'NONE', *, *, #55268, .F. ) ;
#35576 = VECTOR ( 'NONE', #43944, 1000.000000000000000 ) ;
#35577 = CARTESIAN_POINT ( 'NONE',  ( 3.606483450353380249, -4.622483450353491286, 455.0000000000000568 ) ) ;
#35578 = LINE ( 'NONE', #68115, #29009 ) ;
#35579 = CARTESIAN_POINT ( 'NONE',  ( 9.900000000000000355, 0.000000000000000000, 2.154935995002245639E-16 ) ) ;
#35580 = PLANE ( 'NONE',  #5436 ) ;
#35581 = CARTESIAN_POINT ( 'NONE',  ( 16.75000000000000000, -2.500000000000000000, 21.77831216351300014 ) ) ;
#35582 = ORIENTED_EDGE ( 'NONE', *, *, #54951, .F. ) ;
#35583 = CARTESIAN_POINT ( 'NONE',  ( 7.450000000000006395, 7.250000000000000888, -14.50000000000000000 ) ) ;
#35584 = FACE_OUTER_BOUND ( 'NONE', #60627, .T. ) ;
#35585 = LINE ( 'NONE', #15088, #8469 ) ;
#35586 = LINE ( 'NONE', #24996, #43550 ) ;
#35587 = EDGE_CURVE ( 'NONE', #54124, #56837, #34608, .T. ) ;
#35588 = CARTESIAN_POINT ( 'NONE',  ( -7.250000000000000888, 7.450000000000003730, -10.50000000000000000 ) ) ;
#35589 = CARTESIAN_POINT ( 'NONE',  ( 275.0000000000000000, -40.30000000000000426, 8.900000000000000355 ) ) ;
#35590 = CARTESIAN_POINT ( 'NONE',  ( 49.00000000000000000, -0.2000000000089119934, 8.909539772616881237E-12 ) ) ;
#35591 = ORIENTED_EDGE ( 'NONE', *, *, #26767, .T. ) ;
#35592 = DIRECTION ( 'NONE',  ( 0.000000000000000000, 0.000000000000000000, -1.000000000000000000 ) ) ;
#35593 = DIRECTION ( 'NONE',  ( 0.000000000000000000, -1.000000000000000000, 0.000000000000000000 ) ) ;
#35594 = AXIS2_PLACEMENT_3D ( 'NONE', #1361, #65381, #44476 ) ;
#35595 = ORIENTED_EDGE ( 'NONE', *, *, #36587, .F. ) ;
#35596 = CARTESIAN_POINT ( 'NONE',  ( -6.344366288193421077, -4.720772854004749775, 54.00000000000000711 ) ) ;
#35597 = CARTESIAN_POINT ( 'NONE',  ( 4.406483450353340103, -11.32648345035347681, 455.0000000000000568 ) ) ;
#35598 = LINE ( 'NONE', #46562, #16346 ) ;
#35599 = CIRCLE ( 'NONE', #26592, 0.1999999999999987899 ) ;
#35600 = DIRECTION ( 'NONE',  ( -1.836970198721029934E-16, 1.836970198721036590E-16, -1.000000000000000000 ) ) ;
#35601 = ADVANCED_FACE ( 'NONE', ( #14094 ), #8798, .T. ) ;
#35602 = VERTEX_POINT ( 'NONE', #25063 ) ;
#35603 = CARTESIAN_POINT ( 'NONE',  ( 7.000000000000000000, -21.00000000000000000, 0.000000000000000000 ) ) ;
#35604 = VECTOR ( 'NONE', #67321, 1000.000000000000000 ) ;
#35605 = VECTOR ( 'NONE', #59350, 1000.000000000000000 ) ;
#35606 = VECTOR ( 'NONE', #25941, 1000.000000000000000 ) ;
#35607 = EDGE_LOOP ( 'NONE', ( #1734, #23216, #3292, #12304 ) ) ;
#35608 = EDGE_CURVE ( 'NONE', #22607, #62442, #41667, .T. ) ;
#35609 = CARTESIAN_POINT ( 'NONE',  ( -29.50000000000000355, -11.50000000000000000, 15.00000000000000000 ) ) ;
#35610 = PLANE ( 'NONE',  #17532 ) ;
#35611 = ORIENTED_EDGE ( 'NONE', *, *, #69723, .T. ) ;
#35612 = CARTESIAN_POINT ( 'NONE',  ( 10.09643294401453417, 2.893516549646536262, 455.0000000000000568 ) ) ;
#35613 = AXIS2_PLACEMENT_3D ( 'NONE', #30685, #58610, #68863 ) ;
#35614 = ORIENTED_EDGE ( 'NONE', *, *, #67993, .T. ) ;
#35615 = AXIS2_PLACEMENT_3D ( 'NONE', #69593, #10188, #10882 ) ;
#35616 = CARTESIAN_POINT ( 'NONE',  ( 4.255011587777218551, -8.465062094116168723, 455.0000000000000568 ) ) ;
#35617 = VERTEX_POINT ( 'NONE', #50870 ) ;
#35618 = EDGE_LOOP ( 'NONE', ( #66126, #60868, #20844, #55491 ) ) ;
#35619 = LINE ( 'NONE', #29975, #22709 ) ;
#35620 = VERTEX_POINT ( 'NONE', #14460 ) ;
#35621 = ORIENTED_EDGE ( 'NONE', *, *, #33886, .T. ) ;
#35622 = ADVANCED_FACE ( 'NONE', ( #36013 ), #57583, .F. ) ;
#35623 = CARTESIAN_POINT ( 'NONE',  ( -8.916576262117260399, 8.916576262117214213, 54.00000000000000711 ) ) ;
#35624 = CARTESIAN_POINT ( 'NONE',  ( -8.916576262117258622, 10.03972626211718477, 54.00000000000000711 ) ) ;
#35625 = VECTOR ( 'NONE', #69641, 1000.000000000000000 ) ;
#35626 = CARTESIAN_POINT ( 'NONE',  ( -30.00000000000000000, -14.33999999999999986, -14.50000000000000000 ) ) ;
#35627 = VERTEX_POINT ( 'NONE', #9149 ) ;
#35628 = CIRCLE ( 'NONE', #45781, 3.232999999999965901 ) ;
#35629 = DIRECTION ( 'NONE',  ( 0.000000000000000000, -0.7071067811865474617, -0.7071067811865474617 ) ) ;
#35631 = FACE_OUTER_BOUND ( 'NONE', #60334, .T. ) ;
#35630 = DIRECTION ( 'NONE',  ( 1.000000000000000000, 0.000000000000000000, 0.000000000000000000 ) ) ;
#35632 = ORIENTED_EDGE ( 'NONE', *, *, #41819, .T. ) ;
#35634 = ORIENTED_EDGE ( 'NONE', *, *, #44661, .T. ) ;
#35633 = CARTESIAN_POINT ( 'NONE',  ( 34.89999999999999858, -0.2000000000089119934, -8.913009219568841313E-12 ) ) ;
#35635 = ORIENTED_EDGE ( 'NONE', *, *, #36287, .T. ) ;
#35636 = PRODUCT_CONTEXT ( 'NONE', #56227, 'mechanical' ) ;
#35637 = LINE ( 'NONE', #30354, #11885 ) ;
#35639 = VERTEX_POINT ( 'NONE', #3843 ) ;
#35638 = LINE ( 'NONE', #67833, #17277 ) ;
#35640 = DIRECTION ( 'NONE',  ( 0.000000000000000000, 0.000000000000000000, -1.000000000000000000 ) ) ;
#35641 = DIRECTION ( 'NONE',  ( -0.000000000000000000, -0.000000000000000000, -1.000000000000000000 ) ) ;
#35642 = ORIENTED_EDGE ( 'NONE', *, *, #35690, .F. ) ;
#35643 = CIRCLE ( 'NONE', #60485, 0.1750000000000002387 ) ;
#35644 = EDGE_LOOP ( 'NONE', ( #31156, #13471 ) ) ;
#35645 = EDGE_CURVE ( 'NONE', #28489, #43571, #25412, .T. ) ;
#35646 = CYLINDRICAL_SURFACE ( 'NONE', #51577, 24.99999999998784972 ) ;
#35647 = AXIS2_PLACEMENT_3D ( 'NONE', #23535, #13273, #7620 ) ;
#35648 = VERTEX_POINT ( 'NONE', #32114 ) ;
#35649 = EDGE_CURVE ( 'NONE', #17758, #11032, #15159, .T. ) ;
#35650 = CARTESIAN_POINT ( 'NONE',  ( -29.25000000000000000, -5.000000000000000000, 26.25000000000000000 ) ) ;
#35651 = DIRECTION ( 'NONE',  ( 1.053224967557347660E-14, 1.000000000000000000, 0.000000000000000000 ) ) ;
#35652 = CIRCLE ( 'NONE', #46915, 2.204799999999997429 ) ;
#35653 = DIRECTION ( 'NONE',  ( -1.000000000000000000, 0.000000000000000000, 0.000000000000000000 ) ) ;
#35654 = EDGE_LOOP ( 'NONE', ( #36788, #60076, #9943, #27041 ) ) ;
#35655 = CIRCLE ( 'NONE', #41316, 1.399999999999998579 ) ;
#35656 = VECTOR ( 'NONE', #36855, 1000.000000000000000 ) ;
#35657 = AXIS2_PLACEMENT_3D ( 'NONE', #20529, #4632, #8871 ) ;
#35658 = CARTESIAN_POINT ( 'NONE',  ( -7.342976262117259623, 5.538810540049946773, 26.00000000000000711 ) ) ;
#35659 = CARTESIAN_POINT ( 'NONE',  ( -6.835476262117260227, 10.49297626211718359, 54.00000000000000711 ) ) ;
#35661 = EDGE_LOOP ( 'NONE', ( #255, #57038, #33212, #68719 ) ) ;
#35660 = DIRECTION ( 'NONE',  ( -0.000000000000000000, 1.000000000000000000, -0.000000000000000000 ) ) ;
#35663 = ORIENTED_EDGE ( 'NONE', *, *, #32304, .T. ) ;
#35662 = DIRECTION ( 'NONE',  ( 0.000000000000000000, 0.000000000000000000, 1.000000000000000000 ) ) ;
#35664 = CARTESIAN_POINT ( 'NONE',  ( 7.969523737882818537, -9.737023737882809726, 26.00000000000000000 ) ) ;
#35665 = CIRCLE ( 'NONE', #57129, 0.2000000000000005107 ) ;
#35666 = VECTOR ( 'NONE', #36795, 1000.000000000000000 ) ;
#35667 = CARTESIAN_POINT ( 'NONE',  ( 10.92648345035337520, -2.906483450353491094, 455.0000000000000568 ) ) ;
#35668 = CARTESIAN_POINT ( 'NONE',  ( -7.955476262117259445, 9.722976262117178692, 54.00000000000000711 ) ) ;
#35669 = DIRECTION ( 'NONE',  ( 0.000000000000000000, 0.000000000000000000, -1.000000000000000000 ) ) ;
#35670 = VECTOR ( 'NONE', #65918, 1000.000000000000000 ) ;
#35671 = EDGE_CURVE ( 'NONE', #47415, #6609, #25778, .T. ) ;
#35672 = CARTESIAN_POINT ( 'NONE',  ( 8.606483450353380249, -7.616533956692325802, 455.0000000000000568 ) ) ;
#35673 = ORIENTED_EDGE ( 'NONE', *, *, #27494, .T. ) ;
#35674 = CARTESIAN_POINT ( 'NONE',  ( 283.0000000000000568, -38.64999999999999858, 15.00000000000000000 ) ) ;
#35675 = DIRECTION ( 'NONE',  ( -1.000000000000000000, 0.000000000000000000, 0.000000000000000000 ) ) ;
#35676 = CARTESIAN_POINT ( 'NONE',  ( 25.57999999999999829, 0.000000000000000000, 0.000000000000000000 ) ) ;
#35678 = ORIENTED_EDGE ( 'NONE', *, *, #18406, .T. ) ;
#35677 = CYLINDRICAL_SURFACE ( 'NONE', #23143, 3.499999999999850342 ) ;
#35679 = PRODUCT ( 'Part2', 'Part2', '', ( #2769 ) ) ;
#35680 = AXIS2_PLACEMENT_3D ( 'NONE', #53379, #48412, #6313 ) ;
#35681 = DIRECTION ( 'NONE',  ( 7.808916176531286882E-15, 1.000000000000000000, -0.000000000000000000 ) ) ;
#35682 = CARTESIAN_POINT ( 'NONE',  ( 11.90000000000000036, -21.00000000000000000, 13.86939075806900057 ) ) ;
#35683 = ORIENTED_EDGE ( 'NONE', *, *, #41686, .T. ) ;
#35684 = CARTESIAN_POINT ( 'NONE',  ( 7.811466277050774565, 7.259684009079793832, 455.0000000000000568 ) ) ;
#35685 = CARTESIAN_POINT ( 'NONE',  ( 8.406483450353398723, 5.655420232009111814, 455.0000000000000568 ) ) ;
#35686 = ORIENTED_EDGE ( 'NONE', *, *, #45330, .T. ) ;
#35687 = PLANE ( 'NONE',  #54805 ) ;
#35688 = DIRECTION ( 'NONE',  ( 0.000000000000000000, 1.000000000000000000, 0.000000000000000000 ) ) ;
#35689 = DIRECTION ( 'NONE',  ( -1.671920889371702657E-15, 1.000000000000000000, 3.673940397442059868E-16 ) ) ;
#35690 = EDGE_CURVE ( 'NONE', #21517, #44259, #64632, .T. ) ;
#35691 = CARTESIAN_POINT ( 'NONE',  ( 6.884529946162100345, -21.00000000000000000, 0.000000000000000000 ) ) ;
#35692 = VERTEX_POINT ( 'NONE', #43065 ) ;
#35693 = EDGE_CURVE ( 'NONE', #41134, #62844, #4213, .T. ) ;
#35694 = DIRECTION ( 'NONE',  ( -1.836970198721029934E-16, 1.836970198721036590E-16, -1.000000000000000000 ) ) ;
#35695 = VERTEX_POINT ( 'NONE', #31435 ) ;
#35696 = EDGE_LOOP ( 'NONE', ( #63369, #40453, #22025, #1097, #26517, #10405, #25576, #20135 ) ) ;
#35697 = EDGE_CURVE ( 'NONE', #11798, #6104, #21164, .T. ) ;
#35698 = VECTOR ( 'NONE', #51334, 1000.000000000000000 ) ;
#35699 = VERTEX_POINT ( 'NONE', #48026 ) ;
#35700 = CARTESIAN_POINT ( 'NONE',  ( 7.250000000000005329, 8.250000000000001776, -26.00000000000001066 ) ) ;
#35701 = EDGE_CURVE ( 'NONE', #46404, #3061, #7396, .T. ) ;
#35702 = AXIS2_PLACEMENT_3D ( 'NONE', #21378, #22081, #64523 ) ;
#35703 = DIRECTION ( 'NONE',  ( 1.000000000000000000, 0.000000000000000000, 0.000000000000000000 ) ) ;
#35704 = VECTOR ( 'NONE', #58861, 1000.000000000000114 ) ;
#35706 = EDGE_CURVE ( 'NONE', #56861, #56386, #23366, .T. ) ;
#35705 = AXIS2_PLACEMENT_3D ( 'NONE', #66620, #56016, #50702 ) ;
#35707 = FACE_OUTER_BOUND ( 'NONE', #62319, .T. ) ;
#35708 = ORIENTED_EDGE ( 'NONE', *, *, #69472, .T. ) ;
#35709 = EDGE_CURVE ( 'NONE', #50275, #62585, #15517, .T. ) ;
#35710 = EDGE_LOOP ( 'NONE', ( #40378, #26188, #62026, #42208 ) ) ;
#35711 = DIRECTION ( 'NONE',  ( -1.000000000000000000, 0.000000000000000000, 0.000000000000000000 ) ) ;
#35713 = ORIENTED_EDGE ( 'NONE', *, *, #41114, .F. ) ;
#35712 = EDGE_CURVE ( 'NONE', #58904, #35825, #4896, .T. ) ;
#35714 = ORIENTED_EDGE ( 'NONE', *, *, #66446, .T. ) ;
#35715 = CIRCLE ( 'NONE', #32356, 0.5999999999999989786 ) ;
#35716 = VECTOR ( 'NONE', #7422, 1000.000000000000000 ) ;
#35717 = VECTOR ( 'NONE', #18334, 1000.000000000000000 ) ;
#35718 = LINE ( 'NONE', #25119, #46200 ) ;
#35719 = LINE ( 'NONE', #57293, #14384 ) ;
#35720 = DIRECTION ( 'NONE',  ( 0.000000000000000000, 1.000000000000000000, 0.000000000000000000 ) ) ;
#35721 = DIRECTION ( 'NONE',  ( -1.000000000000000000, 0.000000000000000000, 0.000000000000000000 ) ) ;
#35722 = VERTEX_POINT ( 'NONE', #9497 ) ;
#35723 = DIRECTION ( 'NONE',  ( -1.000000000000000000, 0.000000000000000000, 0.000000000000000000 ) ) ;
#35724 = AXIS2_PLACEMENT_3D ( 'NONE', #11080, #48913, #27685 ) ;
#35725 = AXIS2_PLACEMENT_3D ( 'NONE', #51292, #18768, #45991 ) ;
#35726 = VECTOR ( 'NONE', #15134, 1000.000000000000000 ) ;
#35728 = CARTESIAN_POINT ( 'NONE',  ( -2.277516549646816379, -9.841277389592805847, 455.0000000000000568 ) ) ;
#35727 = CARTESIAN_POINT ( 'NONE',  ( 283.0000000000000568, -31.30000000000095284, -12.19999999999906315 ) ) ;
#35729 = ORIENTED_EDGE ( 'NONE', *, *, #66010, .F. ) ;
#35731 = ORIENTED_EDGE ( 'NONE', *, *, #26139, .T. ) ;
#35730 = DIRECTION ( 'NONE',  ( 0.000000000000000000, 0.000000000000000000, 1.000000000000000000 ) ) ;
#35732 = ORIENTED_EDGE ( 'NONE', *, *, #49581, .F. ) ;
#35733 = ORIENTED_EDGE ( 'NONE', *, *, #66074, .T. ) ;
#35734 = AXIS2_PLACEMENT_3D ( 'NONE', #28962, #1067, #17306 ) ;
#35735 = CYLINDRICAL_SURFACE ( 'NONE', #23097, 2.215251240775983899 ) ;
#35736 =( BOUNDED_CURVE ( )  B_SPLINE_CURVE ( 3, ( #42214, #62727, #58130, #15002 ),
 .UNSPECIFIED., .F., .F. ) 
 B_SPLINE_CURVE_WITH_KNOTS ( ( 4, 4 ),
 ( 3.864326901403208669, 4.037257447447657910 ),
 .UNSPECIFIED. ) 
 CURVE ( )  GEOMETRIC_REPRESENTATION_ITEM ( )  RATIONAL_B_SPLINE_CURVE ( ( 1.000000000000000000, 0.9975094710839674805, 0.9975094710839674805, 1.000000000000000000 ) ) 
 REPRESENTATION_ITEM ( '' )  );
#35737 = AXIS2_PLACEMENT_3D ( 'NONE', #2272, #56017, #44691 ) ;
#35738 = DIRECTION ( 'NONE',  ( -1.000000000000000000, 0.000000000000000000, 0.000000000000000000 ) ) ;
#35739 = ORIENTED_EDGE ( 'NONE', *, *, #69529, .F. ) ;
#35740 = VERTEX_POINT ( 'NONE', #53345 ) ;
#35741 = DIRECTION ( 'NONE',  ( 0.000000000000000000, 0.7071067811865496822, -0.7071067811865454633 ) ) ;
#35742 = CYLINDRICAL_SURFACE ( 'NONE', #19871, 1.399999999999998579 ) ;
#35743 = VERTEX_POINT ( 'NONE', #52999 ) ;
#35744 = ORIENTED_EDGE ( 'NONE', *, *, #32334, .T. ) ;
#35745 = CARTESIAN_POINT ( 'NONE',  ( 29.25000000000000000, -5.200000000000001066, 11.75000000000000000 ) ) ;
#35746 = DIRECTION ( 'NONE',  ( -0.000000000000000000, 1.000000000000000000, -0.000000000000000000 ) ) ;
#35747 = ORIENTED_EDGE ( 'NONE', *, *, #18779, .T. ) ;
#35748 = DIRECTION ( 'NONE',  ( 0.000000000000000000, 0.000000000000000000, 1.000000000000000000 ) ) ;
#35749 = DIRECTION ( 'NONE',  ( -1.836970198721029934E-16, 1.836970198721036344E-16, -1.000000000000000000 ) ) ;
#35750 = VECTOR ( 'NONE', #41774, 1000.000000000000000 ) ;
#35752 = ORIENTED_EDGE ( 'NONE', *, *, #42722, .F. ) ;
#35751 = CARTESIAN_POINT ( 'NONE',  ( 146.5599459900709860, 9.000000000000001776, 320.8239988703753056 ) ) ;
#35753 = ORIENTED_EDGE ( 'NONE', *, *, #22456, .F. ) ;
#35754 = CARTESIAN_POINT ( 'NONE',  ( -11.00000000000000000, -13.54524521594299991, 17.53999999999999915 ) ) ;
#35755 = EDGE_CURVE ( 'NONE', #17475, #9246, #5334, .T. ) ;
#35756 = VECTOR ( 'NONE', #57498, 1000.000000000000000 ) ;
#35757 = CARTESIAN_POINT ( 'NONE',  ( -7.813516549646711162, 11.99351654964660341, 455.0000000000000568 ) ) ;
#35758 = LINE ( 'NONE', #39659, #56081 ) ;
#35759 = CARTESIAN_POINT ( 'NONE',  ( 33.89999999999999858, 20.60000000000000142, 13.86939075806899702 ) ) ;
#35760 = DIRECTION ( 'NONE',  ( -0.7671651518152998728, 0.6414496315691575745, 0.000000000000000000 ) ) ;
#35761 = AXIS2_PLACEMENT_3D ( 'NONE', #19071, #55517, #23334 ) ;
#35762 = CIRCLE ( 'NONE', #12086, 0.2000000000000005107 ) ;
#35763 = ADVANCED_FACE ( 'NONE', ( #31067 ), #9863, .F. ) ;
#35764 = CARTESIAN_POINT ( 'NONE',  ( 2.420780051175169145, 8.697938382363084031, 54.00000000000000711 ) ) ;
#35765 = ORIENTED_EDGE ( 'NONE', *, *, #69683, .T. ) ;
#35766 = CARTESIAN_POINT ( 'NONE',  ( -29.50000000000000355, -11.50000000000100009, 15.00000000000084910 ) ) ;
#35768 = ORIENTED_EDGE ( 'NONE', *, *, #69137, .T. ) ;
#35767 = FACE_OUTER_BOUND ( 'NONE', #14354, .T. ) ;
#35769 = AXIS2_PLACEMENT_3D ( 'NONE', #44040, #17519, #66651 ) ;
#35771 = FACE_OUTER_BOUND ( 'NONE', #30898, .T. ) ;
#35770 = VECTOR ( 'NONE', #33572, 1000.000000000000000 ) ;
#35772 = DIRECTION ( 'NONE',  ( 0.000000000000000000, 0.000000000000000000, 1.000000000000000000 ) ) ;
#35773 = EDGE_CURVE ( 'NONE', #30052, #49314, #20798, .T. ) ;
#35774 = LINE ( 'NONE', #47095, #56628 ) ;
#35775 = VECTOR ( 'NONE', #35052, 1000.000000000000000 ) ;
#35776 = VECTOR ( 'NONE', #36071, 1000.000000000000000 ) ;
#35777 = VERTEX_POINT ( 'NONE', #42716 ) ;
#35778 = CARTESIAN_POINT ( 'NONE',  ( 12.00000000000000178, -11.18999999999999950, 0.000000000000000000 ) ) ;
#35779 = DIRECTION ( 'NONE',  ( -1.000000000000000000, 0.000000000000000000, 0.000000000000000000 ) ) ;
#35780 = EDGE_CURVE ( 'NONE', #25974, #38025, #26822, .T. ) ;
#35781 = ORIENTED_EDGE ( 'NONE', *, *, #67095, .T. ) ;
#35782 = VECTOR ( 'NONE', #42021, 1000.000000000000000 ) ;
#35783 =( NAMED_UNIT ( * ) SI_UNIT ( $, .STERADIAN. ) SOLID_ANGLE_UNIT ( ) );
#35784 = VECTOR ( 'NONE', #24810, 1000.000000000000000 ) ;
#35785 = PLANE ( 'NONE',  #34149 ) ;
#35786 = ORIENTED_EDGE ( 'NONE', *, *, #24133, .F. ) ;
#35787 = EDGE_CURVE ( 'NONE', #6189, #27468, #69602, .T. ) ;
#35788 = LINE ( 'NONE', #52414, #67730 ) ;
#35789 = ORIENTED_EDGE ( 'NONE', *, *, #23877, .T. ) ;
#35790 = ORIENTED_EDGE ( 'NONE', *, *, #24853, .F. ) ;
#35791 = DIRECTION ( 'NONE',  ( -0.000000000000000000, 3.673940397442059868E-16, -1.000000000000000000 ) ) ;
#35792 = CARTESIAN_POINT ( 'NONE',  ( 2.706483450353418085, 10.08346604330775875, 455.0000000000000568 ) ) ;
#35793 = CARTESIAN_POINT ( 'NONE',  ( 39.90000000000000568, 0.000000000000000000, 0.000000000000000000 ) ) ;
#35794 = DIRECTION ( 'NONE',  ( 0.000000000000000000, 0.000000000000000000, -1.000000000000000000 ) ) ;
#35795 = CARTESIAN_POINT ( 'NONE',  ( -8.130476262117259267, 8.821682069070703847, 26.00000000000000711 ) ) ;
#35796 = ORIENTED_EDGE ( 'NONE', *, *, #30306, .T. ) ;
#35797 = EDGE_CURVE ( 'NONE', #59188, #60382, #68900, .T. ) ;
#35798 = ORIENTED_EDGE ( 'NONE', *, *, #7310, .F. ) ;
#35800 = ORIENTED_EDGE ( 'NONE', *, *, #56025, .T. ) ;
#35799 = DIRECTION ( 'NONE',  ( 1.836970198721029934E-16, 1.836970198721010706E-16, -1.000000000000000000 ) ) ;
#35802 = ORIENTED_EDGE ( 'NONE', *, *, #68790, .T. ) ;
#35801 = EDGE_CURVE ( 'NONE', #69217, #28788, #10540, .T. ) ;
#35803 = CARTESIAN_POINT ( 'NONE',  ( -5.993516549646776603, -6.006483450353426790, 455.0000000000000568 ) ) ;
#35804 = DIRECTION ( 'NONE',  ( -1.000000000000000000, 0.000000000000000000, 0.000000000000000000 ) ) ;
#35805 = CARTESIAN_POINT ( 'NONE',  ( 11.12648345035331587, 2.893516549646573566, 195.0000000000000284 ) ) ;
#35806 = FACE_BOUND ( 'NONE', #18322, .T. ) ;
#35807 = COLOUR_RGB ( '', 0.08235294, 0.09019608, 0.10196078) ;
#35808 = DIRECTION ( 'NONE',  ( -1.000000000000000000, 0.000000000000000000, 0.000000000000000000 ) ) ;
#35809 = PLANE ( 'NONE',  #49033 ) ;
#35810 = ORIENTED_EDGE ( 'NONE', *, *, #2097, .T. ) ;
#35811 = ORIENTED_EDGE ( 'NONE', *, *, #25833, .F. ) ;
#35812 = VERTEX_POINT ( 'NONE', #69244 ) ;
#35813 = VECTOR ( 'NONE', #31066, 1000.000000000000000 ) ;
#35814 = AXIS2_PLACEMENT_3D ( 'NONE', #21518, #16572, #48395 ) ;
#35815 = VECTOR ( 'NONE', #3155, 1000.000000000000000 ) ;
#35816 = VERTEX_POINT ( 'NONE', #69935 ) ;
#35817 = DIRECTION ( 'NONE',  ( -1.000000000000000000, 8.339399738404101090E-15, -1.836970198721014896E-16 ) ) ;
#35818 = CARTESIAN_POINT ( 'NONE',  ( -3.842976262117332453, -10.31452373788281740, 54.00000000000000711 ) ) ;
#35819 = DIRECTION ( 'NONE',  ( 1.000000000000000000, 0.000000000000000000, 0.000000000000000000 ) ) ;
#35820 = VECTOR ( 'NONE', #41173, 1000.000000000000000 ) ;
#35821 = AXIS2_PLACEMENT_3D ( 'NONE', #19048, #31688, #26726 ) ;
#35822 = CARTESIAN_POINT ( 'NONE',  ( -5.779227145995285753, 4.141586236041028712, 26.00000000000000711 ) ) ;
#35823 = PRODUCT_DEFINITION_FORMATION_WITH_SPECIFIED_SOURCE ( 'ANY', '', #26723, .NOT_KNOWN. ) ;
#35824 = VERTEX_POINT ( 'NONE', #64296 ) ;
#35825 = VERTEX_POINT ( 'NONE', #15850 ) ;
#35826 = ORIENTED_EDGE ( 'NONE', *, *, #20850, .T. ) ;
#35827 = FACE_OUTER_BOUND ( 'NONE', #62500, .T. ) ;
#35828 = VECTOR ( 'NONE', #26737, 1000.000000000000000 ) ;
#35829 = CIRCLE ( 'NONE', #61764, 0.8099999999999999423 ) ;
#35830 = ORIENTED_EDGE ( 'NONE', *, *, #26146, .F. ) ;
#35831 = VERTEX_POINT ( 'NONE', #37425 ) ;
#35832 = PLANE ( 'NONE',  #2858 ) ;
#35833 = ORIENTED_EDGE ( 'NONE', *, *, #6154, .T. ) ;
#35834 = EDGE_CURVE ( 'NONE', #50705, #51075, #58984, .T. ) ;
#35835 = ORIENTED_EDGE ( 'NONE', *, *, #20407, .F. ) ;
#35836 = CARTESIAN_POINT ( 'NONE',  ( 40.90000000000000568, 4.286263797015736595E-16, -3.500000000000000000 ) ) ;
#35838 = ORIENTED_EDGE ( 'NONE', *, *, #44572, .T. ) ;
#35837 = DIRECTION ( 'NONE',  ( 1.000000000000000000, 0.000000000000000000, 0.000000000000000000 ) ) ;
#35839 = EDGE_LOOP ( 'NONE', ( #57976, #61109, #19246, #23959 ) ) ;
#35840 = ADVANCED_FACE ( 'NONE', ( #39478 ), #59680, .T. ) ;
#35841 = CARTESIAN_POINT ( 'NONE',  ( 275.0000000000000000, -21.00000000000000000, 17.50000000000000000 ) ) ;
#35842 = VECTOR ( 'NONE', #23328, 1000.000000000000000 ) ;
#35843 = LINE ( 'NONE', #31266, #28416 ) ;
#35844 = CARTESIAN_POINT ( 'NONE',  ( -4.393516549646671265, 11.31351654964658771, 455.0000000000000568 ) ) ;
#35845 = ADVANCED_FACE ( 'NONE', ( #65675 ), #39142, .F. ) ;
#35847 = EDGE_LOOP ( 'NONE', ( #17268, #3808, #46766, #6064, #54523, #46387, #23290, #31892 ) ) ;
#35846 = DIRECTION ( 'NONE',  ( 0.000000000000000000, -0.7046037717806115097, -0.7096009616626348659 ) ) ;
#35848 = ORIENTED_EDGE ( 'NONE', *, *, #13141, .T. ) ;
#35849 = CYLINDRICAL_SURFACE ( 'NONE', #34537, 0.5000000000079367624 ) ;
#35850 = EDGE_CURVE ( 'NONE', #9996, #23638, #53886, .T. ) ;
#35851 = CARTESIAN_POINT ( 'NONE',  ( 7.450000000000003730, -7.249999999999997335, -12.00000000000000000 ) ) ;
#35852 = CARTESIAN_POINT ( 'NONE',  ( 9.306483450353372433, 10.91351654964661044, 195.0000000000000284 ) ) ;
#35853 = CARTESIAN_POINT ( 'NONE',  ( 6.006483450353379716, -6.006483450353490738, 455.0000000000000568 ) ) ;
#35854 = ADVANCED_FACE ( 'NONE', ( #66368 ), #60349, .F. ) ;
#35855 = ORIENTED_EDGE ( 'NONE', *, *, #64139, .F. ) ;
#35856 = DIRECTION ( 'NONE',  ( 1.836970198721029934E-16, 1.836970198721010706E-16, -1.000000000000000000 ) ) ;
#35857 = PLANE ( 'NONE',  #21913 ) ;
#35858 = VECTOR ( 'NONE', #145, 1000.000000000000000 ) ;
#35859 = ORIENTED_EDGE ( 'NONE', *, *, #49192, .T. ) ;
#35860 = EDGE_CURVE ( 'NONE', #47318, #61277, #22882, .T. ) ;
#35861 = LINE ( 'NONE', #8639, #25704 ) ;
#35862 = EDGE_CURVE ( 'NONE', #69570, #60745, #28866, .T. ) ;
#35863 = LINE ( 'NONE', #13943, #38526 ) ;
#35864 = CARTESIAN_POINT ( 'NONE',  ( 8.750000000000005329, 0.000000000000000000, -26.00000000000001066 ) ) ;
#35865 = ADVANCED_FACE ( 'NONE', ( #17222 ), #65018, .T. ) ;
#35866 = EDGE_CURVE ( 'NONE', #26202, #5400, #39161, .T. ) ;
#35867 = ORIENTED_EDGE ( 'NONE', *, *, #40585, .F. ) ;
#35868 = AXIS2_PLACEMENT_3D ( 'NONE', #27847, #16890, #64631 ) ;
#35869 = AXIS2_PLACEMENT_3D ( 'NONE', #62449, #24993, #26055 ) ;
#35870 = AXIS2_PLACEMENT_3D ( 'NONE', #61757, #13316, #6624 ) ;
#35871 = DIRECTION ( 'NONE',  ( -3.491481338843133355E-15, -1.000000000000000000, -1.836970198721029934E-16 ) ) ;
#35872 = DIRECTION ( 'NONE',  ( 1.000000000000000000, -1.047444401652939849E-14, 0.000000000000000000 ) ) ;
#35873 = EDGE_CURVE ( 'NONE', #96, #27729, #50447, .T. ) ;
#35874 = CIRCLE ( 'NONE', #2000, 1.000000000000000000 ) ;
#35875 = AXIS2_PLACEMENT_3D ( 'NONE', #23411, #55582, #18084 ) ;
#35876 = CARTESIAN_POINT ( 'NONE',  ( -11.31351654964671027, 7.593516549646603941, 455.0000000000000568 ) ) ;
#35877 = VERTEX_POINT ( 'NONE', #2009 ) ;
#35878 = LINE ( 'NONE', #9715, #57534 ) ;
#35879 = CARTESIAN_POINT ( 'NONE',  ( -7.793516549646829716, -11.32648345035340576, 455.0000000000000568 ) ) ;
#35880 = CARTESIAN_POINT ( 'NONE',  ( -11.00000000000000000, -17.50000000000000000, -15.70500000000000007 ) ) ;
#35881 = AXIS2_PLACEMENT_3D ( 'NONE', #7841, #18812, #24822 ) ;
#35882 = DIRECTION ( 'NONE',  ( 0.000000000000000000, 0.000000000000000000, 1.000000000000000000 ) ) ;
#35883 = VECTOR ( 'NONE', #259, 1000.000000000000114 ) ;
#35884 = DIRECTION ( 'NONE',  ( -0.000000000000000000, -0.000000000000000000, -1.000000000000000000 ) ) ;
#35885 = EDGE_CURVE ( 'NONE', #30319, #59322, #28186, .T. ) ;
#35886 = ORIENTED_EDGE ( 'NONE', *, *, #38386, .F. ) ;
#35887 = DIRECTION ( 'NONE',  ( -1.000000000000000000, 0.000000000000000000, 0.000000000000000000 ) ) ;
#35888 = CYLINDRICAL_SURFACE ( 'NONE', #28242, 1.000000000000000888 ) ;
#35889 = CYLINDRICAL_SURFACE ( 'NONE', #65065, 1.000000000000000000 ) ;
#35890 = FACE_OUTER_BOUND ( 'NONE', #46239, .T. ) ;
#35891 = APPLICATION_CONTEXT ( 'automotive_design' ) ;
#35892 = CARTESIAN_POINT ( 'NONE',  ( -9.093516549646817992, -10.09643294401455904, 455.0000000000000568 ) ) ;
#35893 = ADVANCED_FACE ( 'NONE', ( #60011 ), #33141, .T. ) ;
#35894 = ORIENTED_EDGE ( 'NONE', *, *, #17650, .F. ) ;
#35896 = VERTEX_POINT ( 'NONE', #54725 ) ;
#35895 = CARTESIAN_POINT ( 'NONE',  ( -11.18999999999999950, 11.18999999999999950, -4.250000000000000000 ) ) ;
#35897 = EDGE_CURVE ( 'NONE', #33105, #47162, #32420, .T. ) ;
#35898 = VECTOR ( 'NONE', #17925, 1000.000000000000000 ) ;
#35899 = LINE ( 'NONE', #57454, #22593 ) ;
#35900 = CARTESIAN_POINT ( 'NONE',  ( 10.05377373788278739, -9.703773737882814387, 26.00000000000000000 ) ) ;
#35901 = LINE ( 'NONE', #52159, #16107 ) ;
#35902 = ORIENTED_EDGE ( 'NONE', *, *, #3455, .F. ) ;
#35903 = CARTESIAN_POINT ( 'NONE',  ( 7.000000000000000000, -20.50000000000000000, -13.00000000000000178 ) ) ;
#35904 = ORIENTED_EDGE ( 'NONE', *, *, #58330, .F. ) ;
#35905 = ORIENTED_EDGE ( 'NONE', *, *, #41642, .F. ) ;
#35906 = ORIENTED_EDGE ( 'NONE', *, *, #3430, .F. ) ;
#35907 = VERTEX_POINT ( 'NONE', #45125 ) ;
#35908 = LINE ( 'NONE', #9384, #56568 ) ;
#35909 = DIRECTION ( 'NONE',  ( -1.836970198721029934E-16, 1.836970198721036590E-16, -1.000000000000000000 ) ) ;
#35910 = CARTESIAN_POINT ( 'NONE',  ( -8.393516549646712122, 4.383466043307770121, 455.0000000000000568 ) ) ;
#35911 = LINE ( 'NONE', #50761, #21218 ) ;
#35912 = EDGE_CURVE ( 'NONE', #1047, #59678, #54379, .T. ) ;
#35913 = COLOUR_RGB ( '', 0.40784314, 0.44705882, 0.49803922) ;
#35914 = ORIENTED_EDGE ( 'NONE', *, *, #44456, .T. ) ;
#35915 = ORIENTED_EDGE ( 'NONE', *, *, #17808, .T. ) ;
#35916 = CARTESIAN_POINT ( 'NONE',  ( -5.538810540050064901, -7.357023737882800951, 54.00000000000000711 ) ) ;
#35917 = FACE_OUTER_BOUND ( 'NONE', #66264, .T. ) ;
#35918 = VERTEX_POINT ( 'NONE', #16891 ) ;
#35919 = ORIENTED_EDGE ( 'NONE', *, *, #27735, .T. ) ;
#35920 = ORIENTED_EDGE ( 'NONE', *, *, #35278, .F. ) ;
#35921 = ORIENTED_EDGE ( 'NONE', *, *, #7935, .F. ) ;
#35922 = CARTESIAN_POINT ( 'NONE',  ( 7.250000000000005329, -7.449999999999998401, -25.00000000000000000 ) ) ;
#35923 = UNCERTAINTY_MEASURE_WITH_UNIT (LENGTH_MEASURE( 1.000000000000000082E-05 ), #397, 'distance_accuracy_value', 'NONE');
#35925 = ORIENTED_EDGE ( 'NONE', *, *, #4415, .F. ) ;
#35924 = CARTESIAN_POINT ( 'NONE',  ( -25.50000000000000355, -15.12100000000000044, -20.87900000000000134 ) ) ;
#35926 = CIRCLE ( 'NONE', #52912, 3.300000002979700753 ) ;
#35927 = EDGE_CURVE ( 'NONE', #17187, #59026, #49427, .T. ) ;
#35928 = DIRECTION ( 'NONE',  ( -1.000000000000000000, 0.000000000000000000, 0.000000000000000000 ) ) ;
#35929 = FACE_OUTER_BOUND ( 'NONE', #33114, .T. ) ;
#35930 = ORIENTED_EDGE ( 'NONE', *, *, #66831, .F. ) ;
#35931 = EDGE_CURVE ( 'NONE', #15613, #15881, #3036, .T. ) ;
#35932 = ORIENTED_EDGE ( 'NONE', *, *, #27444, .F. ) ;
#35933 = CIRCLE ( 'NONE', #66409, 0.5000000000079367624 ) ;
#35934 = EDGE_CURVE ( 'NONE', #22077, #51741, #50094, .T. ) ;
#35935 = ADVANCED_FACE ( 'NONE', ( #62085 ), #19312, .T. ) ;
#35936 = FACE_OUTER_BOUND ( 'NONE', #30510, .T. ) ;
#35937 = ADVANCED_FACE ( 'NONE', ( #35936 ), #13311, .F. ) ;
#35938 = EDGE_CURVE ( 'NONE', #2849, #43744, #62804, .T. ) ;
#35939 = CARTESIAN_POINT ( 'NONE',  ( 28.00000000000000000, -17.35230188589299871, 15.35019951917099945 ) ) ;
#35940 = AXIS2_PLACEMENT_3D ( 'NONE', #47183, #68751, #58504 ) ;
#35941 = DIRECTION ( 'NONE',  ( 1.000000000000000000, 0.000000000000000000, 0.000000000000000000 ) ) ;
#35942 = FACE_OUTER_BOUND ( 'NONE', #4630, .T. ) ;
#35943 =( NAMED_UNIT ( * ) SI_UNIT ( $, .STERADIAN. ) SOLID_ANGLE_UNIT ( ) );
#35944 = ORIENTED_EDGE ( 'NONE', *, *, #65826, .F. ) ;
#35945 = CARTESIAN_POINT ( 'NONE',  ( 15.50000000000000000, -5.000000000000000000, -22.50000000000000000 ) ) ;
#35946 = DIRECTION ( 'NONE',  ( -3.491481338843133355E-15, -1.000000000000000000, -1.836970198721029934E-16 ) ) ;
#35947 = CARTESIAN_POINT ( 'NONE',  ( 289.2330000000000041, 0.000000000000000000, 0.000000000000000000 ) ) ;
#35948 = CARTESIAN_POINT ( 'NONE',  ( -3.142976262117292308, -6.501044194225499062, 54.00000000000000711 ) ) ;
#35949 = LINE ( 'NONE', #14389, #68095 ) ;
#35950 = ORIENTED_EDGE ( 'NONE', *, *, #55497, .T. ) ;
#35951 = DIRECTION ( 'NONE',  ( 0.000000000000000000, 0.000000000000000000, -1.000000000000000000 ) ) ;
#35952 = DIRECTION ( 'NONE',  ( -1.000000000000000000, 1.901462112903059913E-14, -1.836970198720994682E-16 ) ) ;
#35953 = LINE ( 'NONE', #68486, #60411 ) ;
#35954 = FACE_OUTER_BOUND ( 'NONE', #48670, .T. ) ;
#35955 = CARTESIAN_POINT ( 'NONE',  ( 0.5000000000000000000, -42.00000000000000000, -27.00000000000000000 ) ) ;
#35956 = DIRECTION ( 'NONE',  ( 0.000000000000000000, 0.000000000000000000, -1.000000000000000000 ) ) ;
#35957 = PLANE ( 'NONE',  #25648 ) ;
#35958 = CARTESIAN_POINT ( 'NONE',  ( -6.344366288193410419, 5.779227145995219139, 54.00000000000000711 ) ) ;
#35959 = ORIENTED_EDGE ( 'NONE', *, *, #15237, .T. ) ;
#35960 = LINE ( 'NONE', #52587, #15200 ) ;
#35961 = CARTESIAN_POINT ( 'NONE',  ( 7.250000000000005329, 8.250000000000001776, -10.50000000000000000 ) ) ;
#35962 = ORIENTED_EDGE ( 'NONE', *, *, #60009, .F. ) ;
#35963 = DIRECTION ( 'NONE',  ( -1.349135440953254805E-14, -1.000000000000000000, 0.000000000000000000 ) ) ;
#35964 = CARTESIAN_POINT ( 'NONE',  ( 49.00000000000000000, 20.60000000000000142, -13.86939075806900057 ) ) ;
#35965 = CARTESIAN_POINT ( 'NONE',  ( -7.250000000000001776, -7.249999999999998224, -12.00000000000000000 ) ) ;
#35966 = FACE_OUTER_BOUND ( 'NONE', #62988, .T. ) ;
#35967 = DIRECTION ( 'NONE',  ( 0.000000000000000000, 0.000000000000000000, -1.000000000000000000 ) ) ;
#35968 = ORIENTED_EDGE ( 'NONE', *, *, #36241, .T. ) ;
#35969 = VECTOR ( 'NONE', #44654, 1000.000000000000000 ) ;
#35970 = DIRECTION ( 'NONE',  ( -1.000000000000000000, 0.000000000000000000, 0.000000000000000000 ) ) ;
#35971 = ADVANCED_FACE ( 'NONE', ( #61382 ), #40876, .F. ) ;
#35972 = ORIENTED_EDGE ( 'NONE', *, *, #13190, .F. ) ;
#35973 = DIRECTION ( 'NONE',  ( 1.000000000000000000, -1.260948829465470062E-14, 0.000000000000000000 ) ) ;
#35974 = CARTESIAN_POINT ( 'NONE',  ( 8.250000000000005329, 0.000000000000000000, -9.000000000000001776 ) ) ;
#35975 = ORIENTED_EDGE ( 'NONE', *, *, #25001, .F. ) ;
#35976 = EDGE_CURVE ( 'NONE', #21925, #68361, #34863, .T. ) ;
#35977 = DIRECTION ( 'NONE',  ( 0.000000000000000000, 0.000000000000000000, 1.000000000000000000 ) ) ;
#35978 = VECTOR ( 'NONE', #38381, 1000.000000000000000 ) ;
#35979 = LINE ( 'NONE', #23368, #2452 ) ;
#35980 = ORIENTED_EDGE ( 'NONE', *, *, #916, .F. ) ;
#35981 = LINE ( 'NONE', #47641, #66105 ) ;
#35982 = EDGE_LOOP ( 'NONE', ( #30839, #59570, #41389, #16336 ) ) ;
#35983 = ORIENTED_EDGE ( 'NONE', *, *, #24711, .F. ) ;
#35984 = CARTESIAN_POINT ( 'NONE',  ( 283.0000000000000568, -20.40000000000000213, -12.40000000000000213 ) ) ;
#35985 = ORIENTED_EDGE ( 'NONE', *, *, #46134, .F. ) ;
#35986 = VERTEX_POINT ( 'NONE', #29210 ) ;
#35987 = CYLINDRICAL_SURFACE ( 'NONE', #53106, 0.2000000000000005107 ) ;
#35988 = PLANE ( 'NONE',  #47153 ) ;
#35989 = DIRECTION ( 'NONE',  ( 0.000000000000000000, 0.000000000000000000, 1.000000000000000000 ) ) ;
#35990 = ORIENTED_EDGE ( 'NONE', *, *, #54459, .T. ) ;
#35991 = CYLINDRICAL_SURFACE ( 'NONE', #721, 0.7500000000000006661 ) ;
#35993 = DIRECTION ( 'NONE',  ( -0.7071067811865474617, 0.000000000000000000, -0.7071067811865474617 ) ) ;
#35992 = DIRECTION ( 'NONE',  ( 0.000000000000000000, 0.7071067811865474617, 0.7071067811865474617 ) ) ;
#35994 = EDGE_LOOP ( 'NONE', ( #61594, #14656, #63774, #55053, #37476, #30607 ) ) ;
#35996 = ORIENTED_EDGE ( 'NONE', *, *, #7262, .T. ) ;
#35995 = PLANE ( 'NONE',  #24045 ) ;
#35997 = EDGE_LOOP ( 'NONE', ( #69477, #63489, #27744, #50934 ) ) ;
#35998 = PRODUCT_CONTEXT ( 'NONE', #21429, 'mechanical' ) ;
#35999 = DIRECTION ( 'NONE',  ( 0.000000000000000000, -1.000000000000000000, -1.880440247955360336E-12 ) ) ;
#36001 = ORIENTED_EDGE ( 'NONE', *, *, #50264, .T. ) ;
#36000 = DIRECTION ( 'NONE',  ( 0.000000000000000000, 0.6857142857146703019, -0.7278708115914659382 ) ) ;
#36002 = ADVANCED_FACE ( 'NONE', ( #7994 ), #18971, .F. ) ;
#36003 = CARTESIAN_POINT ( 'NONE',  ( 7.900000000000000355, 18.00000000000000355, 21.00000000000000000 ) ) ;
#36004 = PLANE ( 'NONE',  #66682 ) ;
#36005 = EDGE_LOOP ( 'NONE', ( #33282, #19321, #42263, #22846 ) ) ;
#36006 = EDGE_LOOP ( 'NONE', ( #56504, #40515, #62785, #68944 ) ) ;
#36007 = DIRECTION ( 'NONE',  ( 0.000000000000000000, 0.000000000000000000, 1.000000000000000000 ) ) ;
#36008 = EDGE_CURVE ( 'NONE', #50581, #66792, #17715, .T. ) ;
#36009 = EDGE_CURVE ( 'NONE', #19769, #47162, #45475, .T. ) ;
#36010 = VERTEX_POINT ( 'NONE', #56789 ) ;
#36011 = AXIS2_PLACEMENT_3D ( 'NONE', #43658, #525, #16090 ) ;
#36012 = DIRECTION ( 'NONE',  ( -1.836970198721029934E-16, 1.836970198721036344E-16, -1.000000000000000000 ) ) ;
#36013 = FACE_OUTER_BOUND ( 'NONE', #20783, .T. ) ;
#36014 = ADVANCED_FACE ( 'NONE', ( #34518 ), #12945, .F. ) ;
#36015 = CARTESIAN_POINT ( 'NONE',  ( -6.486996718459931088, 2.617976262117183150, 54.00000000000000711 ) ) ;
#36016 = EDGE_CURVE ( 'NONE', #51904, #18299, #40174, .T. ) ;
#36017 = ORIENTED_EDGE ( 'NONE', *, *, #12922, .T. ) ;
#36018 = AXIS2_PLACEMENT_3D ( 'NONE', #36880, #59127, #36505 ) ;
#36019 = EDGE_CURVE ( 'NONE', #31134, #28450, #56100, .T. ) ;
#36020 = CARTESIAN_POINT ( 'NONE',  ( 7.606483450353380249, -11.32648345035348925, 455.0000000000000568 ) ) ;
#36021 = CARTESIAN_POINT ( 'NONE',  ( 11.00000000000000000, -11.50000000000000000, 15.00000000000000000 ) ) ;
#36022 = VERTEX_POINT ( 'NONE', #2694 ) ;
#36024 = EDGE_LOOP ( 'NONE', ( #26088, #63204, #24908, #17883 ) ) ;
#36023 = DIRECTION ( 'NONE',  ( 0.000000000000000000, 3.673940397442059868E-16, -1.000000000000000000 ) ) ;
#36025 = LINE ( 'NONE', #46627, #28353 ) ;
#36026 = VECTOR ( 'NONE', #2538, 1000.000000000000000 ) ;
#36027 = LINE ( 'NONE', #46282, #39776 ) ;
#36028 = CARTESIAN_POINT ( 'NONE',  ( 4.046023737882794791, 3.142976262117205266, 54.00000000000000711 ) ) ;
#36029 = CARTESIAN_POINT ( 'NONE',  ( 8.250000000000005329, -8.249999999999998224, -26.00000000000001066 ) ) ;
#36030 = CARTESIAN_POINT ( 'NONE',  ( 31.89999999999999858, -0.000000000000000000, -20.80000000000000071 ) ) ;
#36031 = ORIENTED_EDGE ( 'NONE', *, *, #14633, .T. ) ;
#36032 = DIRECTION ( 'NONE',  ( 0.5773502691896257311, -0.5773502691896258421, -0.5773502691896257311 ) ) ;
#36033 = CARTESIAN_POINT ( 'NONE',  ( 111.9257688011041836, 10.00000000000000000, 281.4830310981151911 ) ) ;
#36034 = CARTESIAN_POINT ( 'NONE',  ( -10.19191654964685689, -10.20488345035338362, 455.0000000000000568 ) ) ;
#36036 = AXIS2_PLACEMENT_3D ( 'NONE', #50783, #46182, #61381 ) ;
#36035 = VECTOR ( 'NONE', #17596, 1000.000000000000000 ) ;
#36038 = ORIENTED_EDGE ( 'NONE', *, *, #23247, .T. ) ;
#36037 = DIRECTION ( 'NONE',  ( 0.000000000000000000, 0.000000000000000000, 1.000000000000000000 ) ) ;
#36039 = CARTESIAN_POINT ( 'NONE',  ( 7.250000000000005329, -7.249999999999998224, -30.00000000000001066 ) ) ;
#36040 = FACE_OUTER_BOUND ( 'NONE', #44605, .T. ) ;
#36041 = VECTOR ( 'NONE', #32577, 1000.000000000000000 ) ;
#36042 = ORIENTED_EDGE ( 'NONE', *, *, #20663, .F. ) ;
#36043 = DIRECTION ( 'NONE',  ( 1.000000000000000000, 0.000000000000000000, 0.000000000000000000 ) ) ;
#36044 = CARTESIAN_POINT ( 'NONE',  ( 4.456444791733522252E-16, 7.450000000000002842, -21.50000000000000000 ) ) ;
#36045 = VERTEX_POINT ( 'NONE', #8345 ) ;
#36046 = DIRECTION ( 'NONE',  ( 0.000000000000000000, 0.000000000000000000, -1.000000000000000000 ) ) ;
#36047 = CYLINDRICAL_SURFACE ( 'NONE', #69339, 5.000000000000004441 ) ;
#36048 = CARTESIAN_POINT ( 'NONE',  ( 39.00000000000000000, 0.000000000000000000, 0.000000000000000000 ) ) ;
#36049 = DIRECTION ( 'NONE',  ( -1.000000000000000000, 0.000000000000000000, 0.000000000000000000 ) ) ;
#36050 = ORIENTED_EDGE ( 'NONE', *, *, #50933, .T. ) ;
#36051 = CARTESIAN_POINT ( 'NONE',  ( 8.580623737882845603, 8.916576262117189344, 54.00000000000000711 ) ) ;
#36052 = EDGE_LOOP ( 'NONE', ( #774, #34770, #40396, #952 ) ) ;
#36053 = VERTEX_POINT ( 'NONE', #24273 ) ;
#36054 = ORIENTED_EDGE ( 'NONE', *, *, #65583, .F. ) ;
#36055 = ADVANCED_FACE ( 'NONE', ( #25324 ), #24976, .F. ) ;
#36056 = EDGE_CURVE ( 'NONE', #21095, #67352, #28847, .T. ) ;
#36057 = CYLINDRICAL_SURFACE ( 'NONE', #24625, 0.5000000000023371305 ) ;
#36058 = EDGE_CURVE ( 'NONE', #2766, #16233, #20998, .T. ) ;
#36059 = EDGE_CURVE ( 'NONE', #47155, #7800, #3408, .T. ) ;
#36060 = VECTOR ( 'NONE', #61374, 1000.000000000000000 ) ;
#36061 = CARTESIAN_POINT ( 'NONE',  ( 26.90000000000000213, 0.000000000000000000, -2.285366197183106074 ) ) ;
#36062 = CARTESIAN_POINT ( 'NONE',  ( -11.50000000000000000, -11.50000000000100009, -15.00000000000084910 ) ) ;
#36063 = ORIENTED_EDGE ( 'NONE', *, *, #16110, .F. ) ;
#36064 = ORIENTED_EDGE ( 'NONE', *, *, #28571, .T. ) ;
#36065 = DIRECTION ( 'NONE',  ( 0.000000000000000000, 0.000000000000000000, 1.000000000000000000 ) ) ;
#36066 = CIRCLE ( 'NONE', #43988, 0.5999999999999998668 ) ;
#36067 = ORIENTED_EDGE ( 'NONE', *, *, #61454, .T. ) ;
#36068 = AXIS2_PLACEMENT_3D ( 'NONE', #52711, #52344, #42775 ) ;
#36069 = ORIENTED_EDGE ( 'NONE', *, *, #11588, .F. ) ;
#36070 = FACE_OUTER_BOUND ( 'NONE', #45693, .T. ) ;
#36071 = DIRECTION ( 'NONE',  ( 1.901462112903059913E-14, 1.000000000000000000, 1.836970198721045958E-16 ) ) ;
#36072 = DIRECTION ( 'NONE',  ( 1.836970198721029934E-16, 1.836970198721010706E-16, -1.000000000000000000 ) ) ;
#36073 = LINE ( 'NONE', #29711, #10544 ) ;
#36074 = ORIENTED_EDGE ( 'NONE', *, *, #4196, .T. ) ;
#36075 = AXIS2_PLACEMENT_3D ( 'NONE', #13418, #67526, #61488 ) ;
#36076 = CARTESIAN_POINT ( 'NONE',  ( -9.690000000000001279, -9.750000000000001776, -5.000000000000000000 ) ) ;
#36078 = DIRECTION ( 'NONE',  ( -1.836970198721029934E-16, -1.836970198721010706E-16, 1.000000000000000000 ) ) ;
#36077 = CARTESIAN_POINT ( 'NONE',  ( 9.703773737882785966, -8.930623737882845248, 26.00000000000000000 ) ) ;
#36079 = VERTEX_POINT ( 'NONE', #19654 ) ;
#36081 = VERTEX_POINT ( 'NONE', #41226 ) ;
#36080 = CARTESIAN_POINT ( 'NONE',  ( -15.50000000000000000, 998.9628421096749662, -22.50000000000000000 ) ) ;
#36082 = ORIENTED_EDGE ( 'NONE', *, *, #22324, .T. ) ;
#36083 = VECTOR ( 'NONE', #35570, 1000.000000000000000 ) ;
#36084 = PLANE ( 'NONE',  #64909 ) ;
#36085 = AXIS2_PLACEMENT_3D ( 'NONE', #21007, #1189, #5464 ) ;
#36086 = CARTESIAN_POINT ( 'NONE',  ( 0.5000000000000000000, 21.00000000000000000, 18.00000000000000355 ) ) ;
#36087 = ORIENTED_EDGE ( 'NONE', *, *, #57659, .F. ) ;
#36088 = ORIENTED_EDGE ( 'NONE', *, *, #18982, .F. ) ;
#36089 = VECTOR ( 'NONE', #32450, 1000.000000000000000 ) ;
#36090 = CARTESIAN_POINT ( 'NONE',  ( -2.530476262117320907, -9.562023737882823227, 26.00000000000000711 ) ) ;
#36091 = DIRECTION ( 'NONE',  ( 0.000000000000000000, 1.000000000000000000, 0.000000000000000000 ) ) ;
#36092 = EDGE_LOOP ( 'NONE', ( #14299, #39719, #55620, #59282 ) ) ;
#36093 = EDGE_LOOP ( 'NONE', ( #20651, #46238, #65895, #8926 ) ) ;
#36094 = DIRECTION ( 'NONE',  ( 0.000000000000000000, -0.000000000000000000, 1.000000000000000000 ) ) ;
#36095 = CARTESIAN_POINT ( 'NONE',  ( -6.331612867284244217, -8.406483450353421816, 455.0000000000000568 ) ) ;
#36096 = ORIENTED_EDGE ( 'NONE', *, *, #54295, .T. ) ;
#36097 = ADVANCED_FACE ( 'NONE', ( #47592 ), #10803, .F. ) ;
#36098 = ADVANCED_FACE ( 'NONE', ( #20369 ), #33416, .F. ) ;
#36099 = CARTESIAN_POINT ( 'NONE',  ( 41.09999999999999432, -21.00000000000000000, 13.86939075806900057 ) ) ;
#36100 = VECTOR ( 'NONE', #54286, 1000.000000000000000 ) ;
#36101 = CARTESIAN_POINT ( 'NONE',  ( -4.193516549646831848, -11.12648345035344377, 455.0000000000000568 ) ) ;
#36102 = EDGE_CURVE ( 'NONE', #4470, #62021, #56020, .T. ) ;
#36104 = ORIENTED_EDGE ( 'NONE', *, *, #54064, .F. ) ;
#36103 = CARTESIAN_POINT ( 'NONE',  ( -9.689726262117227762, 8.566576262117216345, 54.00000000000000711 ) ) ;
#36105 = VERTEX_POINT ( 'NONE', #42280 ) ;
#36106 = DIRECTION ( 'NONE',  ( -1.000000000000000000, 0.000000000000000000, 0.000000000000000000 ) ) ;
#36107 = EDGE_CURVE ( 'NONE', #19393, #55229, #15424, .T. ) ;
#36108 = DIRECTION ( 'NONE',  ( -1.920292680692490463E-14, -1.000000000000000000, -1.836970198721045958E-16 ) ) ;
#36109 = DIRECTION ( 'NONE',  ( 0.000000000000000000, 0.000000000000000000, -1.000000000000000000 ) ) ;
#36110 = DIRECTION ( 'NONE',  ( 0.000000000000000000, -1.000000000000000000, 0.000000000000000000 ) ) ;
#36111 = DIRECTION ( 'NONE',  ( 0.000000000000000000, 3.673940397442059868E-16, -1.000000000000000000 ) ) ;
#36112 = EDGE_CURVE ( 'NONE', #33102, #66383, #4051, .T. ) ;
#36113 = CARTESIAN_POINT ( 'NONE',  ( -11.00000000000000000, -11.85423089348099879, 9.852125413066602277 ) ) ;
#36114 = ORIENTED_EDGE ( 'NONE', *, *, #28905, .F. ) ;
#36115 = DIRECTION ( 'NONE',  ( -0.7071067811865462405, 0.7071067811865487940, 0.000000000000000000 ) ) ;
#36116 = AXIS2_PLACEMENT_3D ( 'NONE', #3027, #45091, #7255 ) ;
#36117 = ADVANCED_FACE ( 'NONE', ( #15070 ), #58201, .F. ) ;
#36118 = AXIS2_PLACEMENT_3D ( 'NONE', #32443, #43378, #33471 ) ;
#36120 = ORIENTED_EDGE ( 'NONE', *, *, #35934, .F. ) ;
#36119 = PLANE ( 'NONE',  #48074 ) ;
#36121 = PLANE ( 'NONE',  #2807 ) ;
#36122 = FACE_OUTER_BOUND ( 'NONE', #52891, .T. ) ;
#36123 = CARTESIAN_POINT ( 'NONE',  ( 7.450000000000006395, 7.250000000000000888, -9.500000000000001776 ) ) ;
#36124 = CIRCLE ( 'NONE', #66606, 0.5999999999999989786 ) ;
#36125 = ORIENTED_EDGE ( 'NONE', *, *, #10129, .F. ) ;
#36126 = CARTESIAN_POINT ( 'NONE',  ( 4.720772854004775532, -4.155633711806681063, 54.00000000000000711 ) ) ;
#36127 = LINE ( 'NONE', #30830, #24919 ) ;
#36128 = EDGE_LOOP ( 'NONE', ( #60770, #32265, #21319, #55105 ) ) ;
#36129 = CARTESIAN_POINT ( 'NONE',  ( 30.00000000000000000, -5.200000000000001066, 11.75000000000000000 ) ) ;
#36130 = SURFACE_SIDE_STYLE ('',( #41786 ) ) ;
#36131 = VECTOR ( 'NONE', #4339, 1000.000000000000000 ) ;
#36132 = DIRECTION ( 'NONE',  ( -1.000000000000000000, 0.000000000000000000, 0.000000000000000000 ) ) ;
#36133 = ORIENTED_EDGE ( 'NONE', *, *, #48481, .F. ) ;
#36134 = CARTESIAN_POINT ( 'NONE',  ( 7.250000000000005329, -7.249999999999998224, -26.00000000000001066 ) ) ;
#36135 = ORIENTED_EDGE ( 'NONE', *, *, #43405, .F. ) ;
#36136 = ORIENTED_EDGE ( 'NONE', *, *, #3423, .T. ) ;
#36137 = FACE_OUTER_BOUND ( 'NONE', #6465, .T. ) ;
#36138 = AXIS2_PLACEMENT_3D ( 'NONE', #34347, #6474, #60197 ) ;
#36139 = DIRECTION ( 'NONE',  ( 1.000000000000000000, 0.000000000000000000, 0.000000000000000000 ) ) ;
#36140 = VECTOR ( 'NONE', #26355, 1000.000000000000000 ) ;
#36141 = CARTESIAN_POINT ( 'NONE',  ( -11.50000000000000000, -11.50000000000000000, 15.00000000000000000 ) ) ;
#36142 = EDGE_CURVE ( 'NONE', #58160, #17842, #8564, .T. ) ;
#36143 = LINE ( 'NONE', #63733, #54720 ) ;
#36144 = DIRECTION ( 'NONE',  ( 0.000000000000000000, 0.000000000000000000, -1.000000000000000000 ) ) ;
#36145 = ORIENTED_EDGE ( 'NONE', *, *, #38437, .F. ) ;
#36146 = ORIENTED_EDGE ( 'NONE', *, *, #65826, .T. ) ;
#36148 = ORIENTED_EDGE ( 'NONE', *, *, #17667, .F. ) ;
#36147 = DIRECTION ( 'NONE',  ( -0.7071067811865398012, 0.7071067811865552333, 2.597868168706484541E-16 ) ) ;
#36149 = VERTEX_POINT ( 'NONE', #48294 ) ;
#36150 =( BOUNDED_CURVE ( )  B_SPLINE_CURVE ( 3, ( #6990, #44818, #65711, #1024 ),
 .UNSPECIFIED., .F., .F. ) 
 B_SPLINE_CURVE_WITH_KNOTS ( ( 4, 4 ),
 ( 3.141592653589793116, 4.712388980384689674 ),
 .UNSPECIFIED. ) 
 CURVE ( )  GEOMETRIC_REPRESENTATION_ITEM ( )  RATIONAL_B_SPLINE_CURVE ( ( 1.000000000000000000, 0.8047378541243649375, 0.8047378541243649375, 1.000000000000000000 ) ) 
 REPRESENTATION_ITEM ( '' )  );
#36151 = DIRECTION ( 'NONE',  ( -0.000000000000000000, -0.000000000000000000, -1.000000000000000000 ) ) ;
#36152 = CARTESIAN_POINT ( 'NONE',  ( 8.250000000000005329, -7.249999999999998224, -10.00000000000000000 ) ) ;
#36153 = DIRECTION ( 'NONE',  ( 3.304235192336781428E-15, 1.000000000000000000, 0.000000000000000000 ) ) ;
#36154 = CIRCLE ( 'NONE', #21473, 0.2000000000000005107 ) ;
#36155 = DIRECTION ( 'NONE',  ( 0.000000000000000000, 0.000000000000000000, 1.000000000000000000 ) ) ;
#36156 = LINE ( 'NONE', #69386, #17551 ) ;
#36157 = ADVANCED_FACE ( 'NONE', ( #21414 ), #69855, .F. ) ;
#36158 = DIRECTION ( 'NONE',  ( 1.000000000000000000, 0.000000000000000000, 0.000000000000000000 ) ) ;
#36159 = ORIENTED_EDGE ( 'NONE', *, *, #52892, .F. ) ;
#36160 = ORIENTED_EDGE ( 'NONE', *, *, #17801, .T. ) ;
#36161 = ORIENTED_EDGE ( 'NONE', *, *, #19737, .F. ) ;
#36162 = ORIENTED_EDGE ( 'NONE', *, *, #14652, .F. ) ;
#36163 = ADVANCED_FACE ( 'NONE', ( #27069 ), #63861, .F. ) ;
#36164 = DIRECTION ( 'NONE',  ( -0.000000000000000000, 1.000000000000000000, -0.000000000000000000 ) ) ;
#36165 = CARTESIAN_POINT ( 'NONE',  ( 34.89999999999999858, -21.00000000000001421, -13.86939075806900945 ) ) ;
#36166 = VECTOR ( 'NONE', #43842, 1000.000000000000114 ) ;
#36167 = CARTESIAN_POINT ( 'NONE',  ( -16.33757311576526305, -0.3152598339554828488, 23.45980260912095616 ) ) ;
#36168 = VECTOR ( 'NONE', #15724, 1000.000000000000000 ) ;
#36169 = VERTEX_POINT ( 'NONE', #36997 ) ;
#36170 = EDGE_LOOP ( 'NONE', ( #25807, #2525, #15632, #44421 ) ) ;
#36171 = ORIENTED_EDGE ( 'NONE', *, *, #58635, .T. ) ;
#36172 = AXIS2_PLACEMENT_3D ( 'NONE', #6895, #49008, #65938 ) ;
#36173 = FACE_OUTER_BOUND ( 'NONE', #31356, .T. ) ;
#36174 = ORIENTED_EDGE ( 'NONE', *, *, #22543, .F. ) ;
#36175 = ORIENTED_EDGE ( 'NONE', *, *, #23179, .F. ) ;
#36176 = DIRECTION ( 'NONE',  ( -0.000000000000000000, -0.000000000000000000, -1.000000000000000000 ) ) ;
#36177 = EDGE_CURVE ( 'NONE', #39630, #10108, #64560, .T. ) ;
#36178 = ORIENTED_EDGE ( 'NONE', *, *, #32201, .F. ) ;
#36179 = VECTOR ( 'NONE', #21882, 1000.000000000000000 ) ;
#36180 = ORIENTED_EDGE ( 'NONE', *, *, #65320, .F. ) ;
#36181 = CARTESIAN_POINT ( 'NONE',  ( 6.619341603356846626, 4.734785091273825408, 455.0000000000000568 ) ) ;
#36182 = AXIS2_PLACEMENT_3D ( 'NONE', #28349, #66530, #1826 ) ;
#36184 = ORIENTED_EDGE ( 'NONE', *, *, #61539, .F. ) ;
#36183 = LINE ( 'NONE', #15327, #34490 ) ;
#36185 = VERTEX_POINT ( 'NONE', #58565 ) ;
#36186 = FACE_OUTER_BOUND ( 'NONE', #8334, .T. ) ;
#36187 = EDGE_CURVE ( 'NONE', #17538, #46187, #35665, .T. ) ;
#36188 = CARTESIAN_POINT ( 'NONE',  ( 18.85410196625000268, -17.50000000000000000, 21.50000000000000000 ) ) ;
#36190 = VERTEX_POINT ( 'NONE', #10115 ) ;
#36189 = DIRECTION ( 'NONE',  ( 1.836970198721029934E-16, 1.836970198721010706E-16, -1.000000000000000000 ) ) ;
#36191 = VERTEX_POINT ( 'NONE', #5512 ) ;
#36192 = VECTOR ( 'NONE', #26919, 1000.000000000000000 ) ;
#36193 = CARTESIAN_POINT ( 'NONE',  ( 15.29686605390242704, -0.2715358723600077573, 21.17390376548697972 ) ) ;
#36194 = VECTOR ( 'NONE', #40787, 1000.000000000000000 ) ;
#36195 = ADVANCED_FACE ( 'NONE', ( #52555 ), #25690, .F. ) ;
#36196 = PLANE ( 'NONE',  #21593 ) ;
#36197 = DIRECTION ( 'NONE',  ( -1.000000000000000000, 0.000000000000000000, 0.000000000000000000 ) ) ;
#36198 = DIRECTION ( 'NONE',  ( -1.000000000000000000, 0.000000000000000000, 0.000000000000000000 ) ) ;
#36199 = EDGE_CURVE ( 'NONE', #48129, #40508, #41585, .T. ) ;
#36200 = EDGE_LOOP ( 'NONE', ( #46753, #23616, #1212, #34789 ) ) ;
#36201 = CARTESIAN_POINT ( 'NONE',  ( 7.532023737882801662, 6.651770455163677376, 26.00000000000000711 ) ) ;
#36202 = EDGE_CURVE ( 'NONE', #53301, #2050, #45633, .T. ) ;
#36203 = PLANE ( 'NONE',  #3900 ) ;
#36204 = CARTESIAN_POINT ( 'NONE',  ( 6.358413763958968623, -5.793274621760850174, 26.00000000000000711 ) ) ;
#36205 = AXIS2_PLACEMENT_3D ( 'NONE', #64127, #46778, #25587 ) ;
#36206 = ORIENTED_EDGE ( 'NONE', *, *, #36878, .T. ) ;
#36207 = CARTESIAN_POINT ( 'NONE',  ( 11.08848345035337424, 11.47551654964657608, 195.0000000000000284 ) ) ;
#36208 = LINE ( 'NONE', #19950, #35114 ) ;
#36209 = CARTESIAN_POINT ( 'NONE',  ( -9.722976262117258628, 6.817976262117182884, 26.00000000000000711 ) ) ;
#36210 = EDGE_CURVE ( 'NONE', #29126, #50794, #19879, .T. ) ;
#36211 = ORIENTED_EDGE ( 'NONE', *, *, #21737, .F. ) ;
#36212 = FACE_OUTER_BOUND ( 'NONE', #38520, .T. ) ;
#36213 = AXIS2_PLACEMENT_3D ( 'NONE', #15519, #22468, #69604 ) ;
#36214 = CARTESIAN_POINT ( 'NONE',  ( -15.50000000000000000, -2.500000000000000000, -21.05662432702600029 ) ) ;
#36215 = AXIS2_PLACEMENT_3D ( 'NONE', #16982, #33241, #39231 ) ;
#36216 = CARTESIAN_POINT ( 'NONE',  ( 8.250000000000005329, 8.250000000000001776, -26.00000000000001066 ) ) ;
#36217 = EDGE_LOOP ( 'NONE', ( #60575, #39939, #2075, #68057 ) ) ;
#36218 = CARTESIAN_POINT ( 'NONE',  ( 49.00000000000000000, -0.2000000000089119934, -8.913009219568841313E-12 ) ) ;
#36219 = EDGE_CURVE ( 'NONE', #14260, #5244, #55337, .T. ) ;
#36220 = CARTESIAN_POINT ( 'NONE',  ( 10.20488345035345468, 10.19191654964656735, 455.0000000000000568 ) ) ;
#36221 = CARTESIAN_POINT ( 'NONE',  ( 15.00000000000000000, -20.40000000000000213, 12.40000000000000213 ) ) ;
#36222 = CIRCLE ( 'NONE', #14780, 1.000000000000000000 ) ;
#36223 = CARTESIAN_POINT ( 'NONE',  ( -8.593516549646745162, -4.396432944014545541, 455.0000000000000568 ) ) ;
#36224 = CARTESIAN_POINT ( 'NONE',  ( 8.689999999999999503, -9.750000000000001776, -7.000000000000000000 ) ) ;
#36225 = ORIENTED_EDGE ( 'NONE', *, *, #4604, .F. ) ;
#36226 = CARTESIAN_POINT ( 'NONE',  ( -8.250000000000001776, 7.250000000000000888, -19.50000000000000000 ) ) ;
#36227 = CYLINDRICAL_SURFACE ( 'NONE', #61031, 1.000000000000001776 ) ;
#36228 = CARTESIAN_POINT ( 'NONE',  ( 3.848229544836323512, -7.357023737882812497, 54.00000000000000711 ) ) ;
#36229 = CIRCLE ( 'NONE', #45245, 0.1999999999999987899 ) ;
#36230 = VECTOR ( 'NONE', #68866, 1000.000000000000114 ) ;
#36231 = EDGE_CURVE ( 'NONE', #5578, #50, #59411, .T. ) ;
#36232 = DIRECTION ( 'NONE',  ( -0.000000000000000000, -0.000000000000000000, -1.000000000000000000 ) ) ;
#36233 = ORIENTED_EDGE ( 'NONE', *, *, #15147, .T. ) ;
#36235 = ORIENTED_EDGE ( 'NONE', *, *, #51031, .T. ) ;
#36234 = CARTESIAN_POINT ( 'NONE',  ( -5.380658396643315022, -4.747751991980679875, 455.0000000000000568 ) ) ;
#36236 = EDGE_CURVE ( 'NONE', #8968, #13785, #17844, .T. ) ;
#36237 = CARTESIAN_POINT ( 'NONE',  ( 6.006483450353379716, -8.211283450353395352, 195.0000000000000284 ) ) ;
#36238 = DIRECTION ( 'NONE',  ( -1.000000000000000000, 0.000000000000000000, 0.000000000000000000 ) ) ;
#36239 = DIRECTION ( 'NONE',  ( -1.000000000000000000, 0.000000000000000000, -0.000000000000000000 ) ) ;
#36240 = ORIENTED_EDGE ( 'NONE', *, *, #6497, .T. ) ;
#36241 = EDGE_CURVE ( 'NONE', #46689, #69904, #16814, .T. ) ;
#36242 = AXIS2_PLACEMENT_3D ( 'NONE', #22557, #17236, #60364 ) ;
#36243 = DIRECTION ( 'NONE',  ( 0.7671651518153006499, -0.6414496315691565753, -2.356647714346250026E-16 ) ) ;
#36244 = CARTESIAN_POINT ( 'NONE',  ( -8.227189898828699555, -1.634292677759815904, 54.00000000000000711 ) ) ;
#36245 = EDGE_CURVE ( 'NONE', #57618, #49327, #11830, .T. ) ;
#36246 = EDGE_LOOP ( 'NONE', ( #2313, #6540, #14242, #38107 ) ) ;
#36247 = VERTEX_POINT ( 'NONE', #28111 ) ;
#36248 = VERTEX_POINT ( 'NONE', #38379 ) ;
#36249 = ADVANCED_FACE ( 'NONE', ( #6551 ), #23138, .F. ) ;
#36250 = CARTESIAN_POINT ( 'NONE',  ( 37.90000000000000568, -21.00000000000001421, -13.86939075806900945 ) ) ;
#36251 = PLANE ( 'NONE',  #53564 ) ;
#36252 = FACE_OUTER_BOUND ( 'NONE', #54132, .T. ) ;
#36253 =( NAMED_UNIT ( * ) PLANE_ANGLE_UNIT ( ) SI_UNIT ( $, .RADIAN. ) );
#36254 = VECTOR ( 'NONE', #16186, 1000.000000000000000 ) ;
#36255 = VERTEX_POINT ( 'NONE', #12523 ) ;
#36256 = EDGE_CURVE ( 'NONE', #67352, #52963, #48991, .T. ) ;
#36257 = ORIENTED_EDGE ( 'NONE', *, *, #64605, .F. ) ;
#36258 = CYLINDRICAL_SURFACE ( 'NONE', #26757, 0.5000000000079367624 ) ;
#36259 = ADVANCED_FACE ( 'NONE', ( #49675 ), #59934, .F. ) ;
#36260 = DIRECTION ( 'NONE',  ( -0.000000000000000000, -0.000000000000000000, -1.000000000000000000 ) ) ;
#36261 = ORIENTED_EDGE ( 'NONE', *, *, #62466, .F. ) ;
#36262 = EDGE_CURVE ( 'NONE', #52784, #32281, #49345, .T. ) ;
#36263 = VERTEX_POINT ( 'NONE', #64904 ) ;
#36264 = EDGE_CURVE ( 'NONE', #37820, #67667, #6305, .T. ) ;
#36265 = EDGE_CURVE ( 'NONE', #11916, #3912, #65592, .T. ) ;
#36266 = ORIENTED_EDGE ( 'NONE', *, *, #16106, .F. ) ;
#36267 = VERTEX_POINT ( 'NONE', #6876 ) ;
#36268 = CARTESIAN_POINT ( 'NONE',  ( 11.00000000000000000, -11.50000000000100009, -10.50000000000065903 ) ) ;
#36269 = VECTOR ( 'NONE', #34007, 999.9999999999998863 ) ;
#36271 = ORIENTED_EDGE ( 'NONE', *, *, #31648, .F. ) ;
#36270 = CARTESIAN_POINT ( 'NONE',  ( 15.00000000000000000, -21.00000000000000000, -4.000000000000000000 ) ) ;
#36272 = EDGE_CURVE ( 'NONE', #28438, #25974, #17149, .T. ) ;
#36273 = CARTESIAN_POINT ( 'NONE',  ( 49.00000000000000000, 0.000000000000000000, 0.000000000000000000 ) ) ;
#36274 = AXIS2_PLACEMENT_3D ( 'NONE', #3590, #25864, #57675 ) ;
#36275 = FACE_OUTER_BOUND ( 'NONE', #66395, .T. ) ;
#36276 = EDGE_CURVE ( 'NONE', #50090, #59591, #5212, .T. ) ;
#36277 = ORIENTED_EDGE ( 'NONE', *, *, #24666, .T. ) ;
#36278 = CIRCLE ( 'NONE', #13556, 4.000000000000001776 ) ;
#36279 = ORIENTED_EDGE ( 'NONE', *, *, #26095, .F. ) ;
#36280 = EDGE_CURVE ( 'NONE', #43574, #33481, #17488, .T. ) ;
#36281 = AXIS2_PLACEMENT_3D ( 'NONE', #28741, #13529, #44649 ) ;
#36282 = CIRCLE ( 'NONE', #47591, 1.449999999999996403 ) ;
#36283 = CARTESIAN_POINT ( 'NONE',  ( 27.00000000000000000, 0.000000000000000000, 0.000000000000000000 ) ) ;
#36284 = EDGE_CURVE ( 'NONE', #11420, #68516, #33418, .T. ) ;
#36285 = DIRECTION ( 'NONE',  ( 0.000000000000000000, 0.000000000000000000, -1.000000000000000000 ) ) ;
#36286 = ORIENTED_EDGE ( 'NONE', *, *, #16812, .T. ) ;
#36287 = EDGE_CURVE ( 'NONE', #64473, #8910, #1242, .T. ) ;
#36288 = DIRECTION ( 'NONE',  ( 0.000000000000000000, 1.000000000000000000, 0.000000000000000000 ) ) ;
#36289 = CARTESIAN_POINT ( 'NONE',  ( 3.003254798005743353, 6.858227778582815404, 54.00000000000000711 ) ) ;
#36290 = ORIENTED_EDGE ( 'NONE', *, *, #67542, .T. ) ;
#36291 = LINE ( 'NONE', #37350, #12444 ) ;
#36292 = DIRECTION ( 'NONE',  ( 0.000000000000000000, 0.000000000000000000, -1.000000000000000000 ) ) ;
#36293 = AXIS2_PLACEMENT_3D ( 'NONE', #17083, #54930, #6485 ) ;
#36294 = LINE ( 'NONE', #67765, #36421 ) ;
#36295 = LINE ( 'NONE', #14386, #63003 ) ;
#36296 = FACE_OUTER_BOUND ( 'NONE', #12998, .T. ) ;
#36297 = ORIENTED_EDGE ( 'NONE', *, *, #21066, .F. ) ;
#36298 = DIRECTION ( 'NONE',  ( 0.000000000000000000, 0.6666666666652433237, -0.7453559925012029908 ) ) ;
#36299 = DIRECTION ( 'NONE',  ( 0.000000000000000000, 1.000000000000000000, 0.000000000000000000 ) ) ;
#36300 = PLANE ( 'NONE',  #50224 ) ;
#36301 = DIRECTION ( 'NONE',  ( 0.000000000000000000, 1.000000000000000000, 0.000000000000000000 ) ) ;
#36302 = AXIS2_PLACEMENT_3D ( 'NONE', #17143, #11823, #33413 ) ;
#36303 = LINE ( 'NONE', #31377, #8927 ) ;
#36304 = DIRECTION ( 'NONE',  ( -0.9375000000000006661, 0.000000000000000000, 0.3479852726768744020 ) ) ;
#36305 = DIRECTION ( 'NONE',  ( -0.7071067811865500152, -0.7071067811865451302, 4.683861624749757595E-31 ) ) ;
#36306 = DIRECTION ( 'NONE',  ( -1.836970198721029934E-16, 1.836970198721036590E-16, -1.000000000000000000 ) ) ;
#36307 = ORIENTED_EDGE ( 'NONE', *, *, #68604, .T. ) ;
#36308 = CARTESIAN_POINT ( 'NONE',  ( 15.00000000000000000, -26.42999999999999972, -9.412893218813501051 ) ) ;
#36309 = DIRECTION ( 'NONE',  ( 0.000000000000000000, -1.000000000000000000, 0.000000000000000000 ) ) ;
#36310 = EDGE_LOOP ( 'NONE', ( #35663, #39855, #69127, #64744 ) ) ;
#36311 = DIRECTION ( 'NONE',  ( 1.836970198721029934E-16, 1.836970198721010706E-16, -1.000000000000000000 ) ) ;
#36312 = CARTESIAN_POINT ( 'NONE',  ( -8.249999999999996447, -7.848062532927998269, -1.000000000000000000 ) ) ;
#36313 = CARTESIAN_POINT ( 'NONE',  ( -5.538810540050023157, 7.342976262117183239, 54.00000000000000711 ) ) ;
#36314 = CYLINDRICAL_SURFACE ( 'NONE', #40721, 1.000000000000000000 ) ;
#36315 = VECTOR ( 'NONE', #29312, 1000.000000000000000 ) ;
#36316 = ORIENTED_EDGE ( 'NONE', *, *, #48808, .F. ) ;
#36317 = ADVANCED_FACE ( 'NONE', ( #12182 ), #22116, .F. ) ;
#36318 = ORIENTED_EDGE ( 'NONE', *, *, #1363, .F. ) ;
#36319 = CYLINDRICAL_SURFACE ( 'NONE', #5592, 1.000000000000000000 ) ;
#36320 = DIRECTION ( 'NONE',  ( -0.7071067811865463515, -0.7071067811865487940, 0.000000000000000000 ) ) ;
#36321 = VERTEX_POINT ( 'NONE', #28441 ) ;
#36322 = ADVANCED_FACE ( 'NONE', ( #50012 ), #39743, .F. ) ;
#36323 = CARTESIAN_POINT ( 'NONE',  ( 3.157023737882819425, -4.046023737882816107, 26.00000000000000711 ) ) ;
#36324 = DIRECTION ( 'NONE',  ( 1.000000000000000000, -0.000000000000000000, -0.000000000000000000 ) ) ;
#36325 = EDGE_CURVE ( 'NONE', #7579, #20433, #19586, .T. ) ;
#36326 = ORIENTED_EDGE ( 'NONE', *, *, #68616, .T. ) ;
#36327 = AXIS2_PLACEMENT_3D ( 'NONE', #67189, #7782, #12384 ) ;
#36328 = CLOSED_SHELL ( 'NONE', ( #2052, #32075, #36722, #33468, #16543, #50220, #68748, #11565, #68702, #48077, #17986, #23567 ) ) ;
#36329 = DIRECTION ( 'NONE',  ( 0.7071067811865474617, 0.7071067811865474617, 0.000000000000000000 ) ) ;
#36330 = ORIENTED_EDGE ( 'NONE', *, *, #47581, .F. ) ;
#36331 = EDGE_CURVE ( 'NONE', #46858, #61120, #23841, .T. ) ;
#36332 = EDGE_LOOP ( 'NONE', ( #68981, #61469 ) ) ;
#36333 = CARTESIAN_POINT ( 'NONE',  ( 1.690483450353418959, 10.73351654964659652, 455.0000000000000568 ) ) ;
#36334 = ORIENTED_EDGE ( 'NONE', *, *, #54722, .F. ) ;
#36335 = EDGE_LOOP ( 'NONE', ( #44069, #36877, #42672, #49596 ) ) ;
#36336 = CARTESIAN_POINT ( 'NONE',  ( 7.450000000000006395, 7.250000000000000888, -22.00000000000000000 ) ) ;
#36337 = PLANE ( 'NONE',  #34707 ) ;
#36338 = CARTESIAN_POINT ( 'NONE',  ( 6.006483450353401921, 5.993516549646582092, 455.0000000000000568 ) ) ;
#36339 = ORIENTED_EDGE ( 'NONE', *, *, #41605, .F. ) ;
#36340 = CARTESIAN_POINT ( 'NONE',  ( -7.250000000000000888, 7.250000000000001776, -26.00000000000001066 ) ) ;
#36341 = CIRCLE ( 'NONE', #29610, 3.499999999999849454 ) ;
#36343 = DIRECTION ( 'NONE',  ( -1.000000000000000000, 0.000000000000000000, 0.000000000000000000 ) ) ;
#36342 = LINE ( 'NONE', #20431, #16918 ) ;
#36344 = VERTEX_POINT ( 'NONE', #19239 ) ;
#36346 = ORIENTED_EDGE ( 'NONE', *, *, #53545, .F. ) ;
#36345 = CARTESIAN_POINT ( 'NONE',  ( 30.00000000000000000, -5.599999999999999645, -27.00000000000000000 ) ) ;
#36347 = ORIENTED_EDGE ( 'NONE', *, *, #2896, .T. ) ;
#36348 = ADVANCED_FACE ( 'NONE', ( #67677 ), #23498, .T. ) ;
#36349 = APPLICATION_PROTOCOL_DEFINITION ( 'draft international standard', 'automotive_design', 1998, #61160 ) ;
#36350 = LINE ( 'NONE', #19040, #18648 ) ;
#36352 = ORIENTED_EDGE ( 'NONE', *, *, #48560, .F. ) ;
#36351 = DIRECTION ( 'NONE',  ( 0.000000000000000000, 0.000000000000000000, -1.000000000000000000 ) ) ;
#36353 = CARTESIAN_POINT ( 'NONE',  ( -8.750000000000001776, 7.250000000000000000, -30.00000000000001066 ) ) ;
#36354 = CARTESIAN_POINT ( 'NONE',  ( 16.89999999999999858, -0.1999999999911795112, 8.826273045769999343E-12 ) ) ;
#36355 = VECTOR ( 'NONE', #23490, 1000.000000000000000 ) ;
#36356 = ORIENTED_EDGE ( 'NONE', *, *, #26395, .F. ) ;
#36357 = VERTEX_POINT ( 'NONE', #57062 ) ;
#36358 = CARTESIAN_POINT ( 'NONE',  ( 49.00000000000000000, -0.2000000000089119934, -8.913009219568841313E-12 ) ) ;
#36359 = VECTOR ( 'NONE', #67446, 1000.000000000000000 ) ;
#36360 = ORIENTED_EDGE ( 'NONE', *, *, #9151, .F. ) ;
#36361 = CARTESIAN_POINT ( 'NONE',  ( 22.14589803375000088, -15.50000000000000000, -21.50000000000000000 ) ) ;
#36362 = DIRECTION ( 'NONE',  ( -1.000000000000000000, 0.000000000000000000, 0.000000000000000000 ) ) ;
#36363 = LINE ( 'NONE', #56532, #43028 ) ;
#36364 = VECTOR ( 'NONE', #66379, 1000.000000000000114 ) ;
#36365 = ADVANCED_FACE ( 'NONE', ( #12863 ), #24551, .F. ) ;
#36366 = ORIENTED_EDGE ( 'NONE', *, *, #58715, .T. ) ;
#36367 = EDGE_CURVE ( 'NONE', #27925, #25470, #49224, .T. ) ;
#36368 = FACE_OUTER_BOUND ( 'NONE', #42064, .T. ) ;
#36369 = LINE ( 'NONE', #30723, #8869 ) ;
#36372 = VERTEX_POINT ( 'NONE', #13230 ) ;
#36371 = EDGE_CURVE ( 'NONE', #23372, #21475, #29841, .T. ) ;
#36370 = CARTESIAN_POINT ( 'NONE',  ( -25.50000000000000355, -5.200000000000001066, 22.50000000000000000 ) ) ;
#36374 = VERTEX_POINT ( 'NONE', #61667 ) ;
#36373 = DIRECTION ( 'NONE',  ( 0.000000000000000000, 1.000000000000000000, 0.000000000000000000 ) ) ;
#36375 = CIRCLE ( 'NONE', #13806, 0.4000000000000010214 ) ;
#36376 = DIRECTION ( 'NONE',  ( 0.000000000000000000, 1.000000000000000000, 0.000000000000000000 ) ) ;
#36377 = DIRECTION ( 'NONE',  ( -0.000000000000000000, -0.000000000000000000, -1.000000000000000000 ) ) ;
#36378 = CARTESIAN_POINT ( 'NONE',  ( -9.293516549646827940, -10.92648345035338764, 455.0000000000000568 ) ) ;
#36379 = VECTOR ( 'NONE', #7261, 1000.000000000000000 ) ;
#36380 = CARTESIAN_POINT ( 'NONE',  ( -15.50000000000000000, -0.4000000000000000222, 22.50000000000000000 ) ) ;
#36381 = CARTESIAN_POINT ( 'NONE',  ( -8.697938382363185283, -8.093267424590415260, 54.00000000000000711 ) ) ;
#36382 = EDGE_LOOP ( 'NONE', ( #47654, #7304, #56694, #21948 ) ) ;
#36383 = DIRECTION ( 'NONE',  ( -1.000000000000000000, 0.000000000000000000, 0.000000000000000000 ) ) ;
#36384 = CARTESIAN_POINT ( 'NONE',  ( 4.740315990920173306, 7.798499376343941414, 455.0000000000000568 ) ) ;
#36385 = AXIS2_PLACEMENT_3D ( 'NONE', #23617, #18306, #45175 ) ;
#36386 =( LENGTH_UNIT ( ) NAMED_UNIT ( * ) SI_UNIT ( .MILLI., .METRE. ) );
#36388 = ORIENTED_EDGE ( 'NONE', *, *, #2138, .F. ) ;
#36387 = CARTESIAN_POINT ( 'NONE',  ( 2.765062094116041980, -9.955011587777324422, 455.0000000000000568 ) ) ;
#36389 = DIRECTION ( 'NONE',  ( 1.000000000000000000, 1.671920889371702854E-15, 6.142537696789956391E-31 ) ) ;
#36390 = VECTOR ( 'NONE', #33184, 1000.000000000000114 ) ;
#36391 = DIRECTION ( 'NONE',  ( 0.000000000000000000, -1.000000000000000000, 0.000000000000000000 ) ) ;
#36392 = VECTOR ( 'NONE', #22232, 1000.000000000000000 ) ;
#36393 = DIRECTION ( 'NONE',  ( 0.000000000000000000, 0.000000000000000000, 1.000000000000000000 ) ) ;
#36394 = ORIENTED_EDGE ( 'NONE', *, *, #12999, .T. ) ;
#36395 = PLANE ( 'NONE',  #27554 ) ;
#36396 = CARTESIAN_POINT ( 'NONE',  ( 7.250000000000005329, 7.250000000000000888, -26.00000000000001066 ) ) ;
#36397 = ORIENTED_EDGE ( 'NONE', *, *, #15102, .T. ) ;
#36398 = SURFACE_STYLE_USAGE ( .BOTH. , #45683 ) ;
#36399 = CARTESIAN_POINT ( 'NONE',  ( -9.750000000000001776, 9.690000000000001279, -5.000000000000000000 ) ) ;
#36400 = DIRECTION ( 'NONE',  ( -0.000000000000000000, -0.000000000000000000, -1.000000000000000000 ) ) ;
#36401 = FACE_OUTER_BOUND ( 'NONE', #59062, .T. ) ;
#36402 = EDGE_CURVE ( 'NONE', #54090, #49938, #34792, .T. ) ;
#36403 = DIRECTION ( 'NONE',  ( 8.673617379884087537E-15, 1.000000000000000000, 0.000000000000000000 ) ) ;
#36404 = ORIENTED_EDGE ( 'NONE', *, *, #55581, .T. ) ;
#36405 = CARTESIAN_POINT ( 'NONE',  ( 7.450000000000004619, -1.336933437520057563E-15, -10.00000000000000000 ) ) ;
#36406 = ORIENTED_EDGE ( 'NONE', *, *, #28485, .T. ) ;
#36407 = DIRECTION ( 'NONE',  ( 1.000000000000000000, 0.000000000000000000, 0.000000000000000000 ) ) ;
#36408 = ORIENTED_EDGE ( 'NONE', *, *, #64693, .T. ) ;
#36409 = VERTEX_POINT ( 'NONE', #35852 ) ;
#36410 = ADVANCED_FACE ( 'NONE', ( #7918 ), #50708, .F. ) ;
#36411 = DIRECTION ( 'NONE',  ( 0.000000000000000000, 0.000000000000000000, 1.000000000000000000 ) ) ;
#36412 = EDGE_CURVE ( 'NONE', #64953, #41781, #28785, .T. ) ;
#36413 = AXIS2_PLACEMENT_3D ( 'NONE', #6581, #65619, #54671 ) ;
#36414 = EDGE_CURVE ( 'NONE', #34152, #44259, #7577, .T. ) ;
#36415 = DIRECTION ( 'NONE',  ( 0.000000000000000000, 1.000000000000000000, 0.000000000000000000 ) ) ;
#36416 = CARTESIAN_POINT ( 'NONE',  ( 25.50000000000000355, 0.000000000000000000, 22.50000000000000000 ) ) ;
#36417 = ORIENTED_EDGE ( 'NONE', *, *, #48821, .F. ) ;
#36418 = EDGE_CURVE ( 'NONE', #22125, #10176, #41325, .T. ) ;
#36419 = VERTEX_POINT ( 'NONE', #67337 ) ;
#36420 = ADVANCED_FACE ( 'NONE', ( #18894 ), #41149, .F. ) ;
#36421 = VECTOR ( 'NONE', #45847, 1000.000000000000000 ) ;
#36422 = CARTESIAN_POINT ( 'NONE',  ( -6.500000000000002665, -6.500000000000002665, 0.000000000000000000 ) ) ;
#36423 = ORIENTED_EDGE ( 'NONE', *, *, #44320, .F. ) ;
#36424 = ORIENTED_EDGE ( 'NONE', *, *, #36883, .T. ) ;
#36425 = DIRECTION ( 'NONE',  ( 0.000000000000000000, 0.000000000000000000, 1.000000000000000000 ) ) ;
#36426 = DIRECTION ( 'NONE',  ( 0.000000000000000000, 0.000000000000000000, 1.000000000000000000 ) ) ;
#36427 = CARTESIAN_POINT ( 'NONE',  ( -11.00000000000000000, -11.10796162543699950, -9.102987789146602893 ) ) ;
#36428 = EDGE_CURVE ( 'NONE', #51826, #31741, #8268, .T. ) ;
#36429 = VERTEX_POINT ( 'NONE', #56717 ) ;
#36430 = CARTESIAN_POINT ( 'NONE',  ( -8.916576262117260399, 8.916576262117214213, 26.00000000000000711 ) ) ;
#36432 = DIRECTION ( 'NONE',  ( 1.000000000000000000, -5.981805089575194965E-17, 0.000000000000000000 ) ) ;
#36431 = DIRECTION ( 'NONE',  ( 0.000000000000000000, 0.000000000000000000, -1.000000000000000000 ) ) ;
#36433 = ORIENTED_EDGE ( 'NONE', *, *, #17626, .T. ) ;
#36435 = VERTEX_POINT ( 'NONE', #51411 ) ;
#36434 = CARTESIAN_POINT ( 'NONE',  ( 8.750000000000005329, -7.249999999999997335, -30.00000000000001066 ) ) ;
#36436 = ORIENTED_EDGE ( 'NONE', *, *, #16425, .T. ) ;
#36437 = DIRECTION ( 'NONE',  ( 1.000000000000000000, -5.981805089575196197E-17, 0.000000000000000000 ) ) ;
#36438 = CARTESIAN_POINT ( 'NONE',  ( 5.257023737882819070, -4.032023737882826531, 54.00000000000000711 ) ) ;
#36439 = VECTOR ( 'NONE', #63118, 1000.000000000000000 ) ;
#36440 = EDGE_LOOP ( 'NONE', ( #13252, #9909, #10228, #23339 ) ) ;
#36441 = ORIENTED_EDGE ( 'NONE', *, *, #9694, .F. ) ;
#36442 = VECTOR ( 'NONE', #2643, 999.9999999999998863 ) ;
#36444 = PLANE ( 'NONE',  #66916 ) ;
#36443 = VECTOR ( 'NONE', #8557, 1000.000000000000000 ) ;
#36445 = DIRECTION ( 'NONE',  ( 0.000000000000000000, 1.000000000000000000, 0.000000000000000000 ) ) ;
#36446 = ORIENTED_EDGE ( 'NONE', *, *, #53912, .T. ) ;
#36447 = EDGE_LOOP ( 'NONE', ( #3896, #20176, #58941, #31177 ) ) ;
#36448 = FACE_OUTER_BOUND ( 'NONE', #25662, .T. ) ;
#36449 = VECTOR ( 'NONE', #57600, 1000.000000000000000 ) ;
#36450 = DIRECTION ( 'NONE',  ( -1.000000000000000000, 0.000000000000000000, 0.000000000000000000 ) ) ;
#36451 = ORIENTED_EDGE ( 'NONE', *, *, #57319, .F. ) ;
#36452 = ADVANCED_FACE ( 'NONE', ( #13931 ), #8628, .T. ) ;
#36453 = DIRECTION ( 'NONE',  ( 0.000000000000000000, 1.000000000000000000, 0.000000000000000000 ) ) ;
#36454 = DIRECTION ( 'NONE',  ( 0.000000000000000000, -0.7071067811865475727, -0.7071067811865475727 ) ) ;
#36457 = ORIENTED_EDGE ( 'NONE', *, *, #16391, .T. ) ;
#36456 = EDGE_CURVE ( 'NONE', #3551, #45925, #20632, .T. ) ;
#36455 = PRESENTATION_STYLE_ASSIGNMENT (( #56962 ) ) ;
#36459 = EDGE_LOOP ( 'NONE', ( #31544, #6440, #53322, #8785 ) ) ;
#36458 = DIRECTION ( 'NONE',  ( 0.000000000000000000, -1.000000000000000000, 0.000000000000000000 ) ) ;
#36460 = ADVANCED_FACE ( 'NONE', ( #58122 ), #53189, .F. ) ;
#36461 = CARTESIAN_POINT ( 'NONE',  ( 49.00000000000000000, 20.60000000000000142, -13.86939075806900057 ) ) ;
#36462 = CARTESIAN_POINT ( 'NONE',  ( -5.242976262117280406, -5.257023737882805747, 54.00000000000000711 ) ) ;
#36463 = AXIS2_PLACEMENT_3D ( 'NONE', #5807, #16763, #53904 ) ;
#36464 = CARTESIAN_POINT ( 'NONE',  ( 0.000000000000000000, 8.250000000000001776, -8.500000000000000000 ) ) ;
#36465 = LINE ( 'NONE', #69341, #1913 ) ;
#36466 = ADVANCED_FACE ( 'NONE', ( #47513 ), #4039, .T. ) ;
#36467 = PLANE ( 'NONE',  #35065 ) ;
#36468 = DIRECTION ( 'NONE',  ( -1.794541526872559352E-16, -1.000000000000000000, 0.000000000000000000 ) ) ;
#36469 = AXIS2_PLACEMENT_3D ( 'NONE', #62504, #39304, #807 ) ;
#36470 = VERTEX_POINT ( 'NONE', #37611 ) ;
#36471 = CARTESIAN_POINT ( 'NONE',  ( -7.250000000000000888, 7.450000000000003730, -25.00000000000000000 ) ) ;
#36473 = ORIENTED_EDGE ( 'NONE', *, *, #42717, .F. ) ;
#36472 = DIRECTION ( 'NONE',  ( 1.000000000000000000, 0.000000000000000000, 0.000000000000000000 ) ) ;
#36474 = DIRECTION ( 'NONE',  ( -1.000000000000000000, 3.491481338843132961E-15, 1.836970198721036344E-16 ) ) ;
#36475 = CARTESIAN_POINT ( 'NONE',  ( -11.00000000000000000, -11.10796162543699950, 9.102987789146602893 ) ) ;
#36476 = FACE_OUTER_BOUND ( 'NONE', #61839, .T. ) ;
#36477 = AXIS2_PLACEMENT_3D ( 'NONE', #34227, #8059, #12314 ) ;
#36478 = PLANE ( 'NONE',  #38574 ) ;
#36479 = ORIENTED_EDGE ( 'NONE', *, *, #24624, .T. ) ;
#36480 = LINE ( 'NONE', #64416, #45551 ) ;
#36481 = CARTESIAN_POINT ( 'NONE',  ( 6.006483450353379716, -6.006483450353394815, 195.0000000000000284 ) ) ;
#36482 = ORIENTED_EDGE ( 'NONE', *, *, #56447, .T. ) ;
#36483 = LINE ( 'NONE', #7934, #11929 ) ;
#36484 = FILL_AREA_STYLE ('',( #48152 ) ) ;
#36485 = DIRECTION ( 'NONE',  ( 0.000000000000000000, 0.000000000000000000, -1.000000000000000000 ) ) ;
#36486 = VECTOR ( 'NONE', #1801, 1000.000000000000000 ) ;
#36487 = ORIENTED_EDGE ( 'NONE', *, *, #64040, .F. ) ;
#36488 = CARTESIAN_POINT ( 'NONE',  ( 6.006483450353379716, -6.006483450353394815, 195.0000000000000284 ) ) ;
#36489 = VERTEX_POINT ( 'NONE', #63431 ) ;
#36490 = ORIENTED_EDGE ( 'NONE', *, *, #31211, .F. ) ;
#36491 = AXIS2_PLACEMENT_3D ( 'NONE', #20655, #26672, #42580 ) ;
#36492 = DIRECTION ( 'NONE',  ( -3.491481338843133355E-15, -1.000000000000000000, -1.836970198721029934E-16 ) ) ;
#36493 = FACE_OUTER_BOUND ( 'NONE', #63286, .T. ) ;
#36494 = FACE_OUTER_BOUND ( 'NONE', #3853, .T. ) ;
#36495 = VECTOR ( 'NONE', #47624, 1000.000000000000000 ) ;
#36496 = LINE ( 'NONE', #53139, #25337 ) ;
#36497 = VECTOR ( 'NONE', #68121, 1000.000000000000000 ) ;
#36498 = CARTESIAN_POINT ( 'NONE',  ( 9.306483450353379538, -10.09643294401465852, 455.0000000000000568 ) ) ;
#36499 = ORIENTED_EDGE ( 'NONE', *, *, #33828, .T. ) ;
#36500 = VERTEX_POINT ( 'NONE', #30903 ) ;
#36501 = ADVANCED_FACE ( 'NONE', ( #31276 ), #9691, .T. ) ;
#36503 = ORIENTED_EDGE ( 'NONE', *, *, #53507, .T. ) ;
#36502 = DIRECTION ( 'NONE',  ( 0.000000000000000000, 1.000000000000000000, 0.000000000000000000 ) ) ;
#36504 = ORIENTED_EDGE ( 'NONE', *, *, #4293, .T. ) ;
#36505 = DIRECTION ( 'NONE',  ( 0.000000000000000000, 0.000000000000000000, 1.000000000000000000 ) ) ;
#36506 = DIRECTION ( 'NONE',  ( 0.000000000000000000, 0.000000000000000000, -1.000000000000000000 ) ) ;
#36507 = EDGE_CURVE ( 'NONE', #391, #27141, #14993, .T. ) ;
#36508 = CARTESIAN_POINT ( 'NONE',  ( 8.900000000000005684, 20.60000000000000142, -13.86939075806900057 ) ) ;
#36509 = DIRECTION ( 'NONE',  ( 1.836970198721029934E-16, -1.836970198721036344E-16, 1.000000000000000000 ) ) ;
#36511 = LINE ( 'NONE', #68708, #42504 ) ;
#36510 = FACE_BOUND ( 'NONE', #61269, .T. ) ;
#36512 = CIRCLE ( 'NONE', #8281, 1.929199999999998916 ) ;
#36513 = ORIENTED_EDGE ( 'NONE', *, *, #26313, .T. ) ;
#36514 = VERTEX_POINT ( 'NONE', #52117 ) ;
#36515 = ORIENTED_EDGE ( 'NONE', *, *, #12682, .F. ) ;
#36516 = ORIENTED_EDGE ( 'NONE', *, *, #31267, .F. ) ;
#36517 = CARTESIAN_POINT ( 'NONE',  ( -25.49999999999869971, -15.50000000000000000, -22.50000000000000000 ) ) ;
#36518 = CIRCLE ( 'NONE', #15071, 3.499999999999999556 ) ;
#36519 = CARTESIAN_POINT ( 'NONE',  ( 15.00000000000000000, -23.65000000000000568, 12.40000000000000213 ) ) ;
#36520 = DIRECTION ( 'NONE',  ( 1.000000000000000000, 0.000000000000000000, 0.000000000000000000 ) ) ;
#36521 = EDGE_CURVE ( 'NONE', #10593, #2943, #58308, .T. ) ;
#36522 = LINE ( 'NONE', #31928, #63672 ) ;
#36523 = ORIENTED_EDGE ( 'NONE', *, *, #63443, .T. ) ;
#36524 = ORIENTED_EDGE ( 'NONE', *, *, #23273, .F. ) ;
#36525 = ORIENTED_EDGE ( 'NONE', *, *, #8424, .F. ) ;
#36526 = VECTOR ( 'NONE', #45901, 1000.000000000000000 ) ;
#36527 = DIRECTION ( 'NONE',  ( 0.000000000000000000, 0.000000000000000000, 1.000000000000000000 ) ) ;
#36528 = ORIENTED_EDGE ( 'NONE', *, *, #25253, .F. ) ;
#36529 = ORIENTED_EDGE ( 'NONE', *, *, #46795, .F. ) ;
#36530 = CARTESIAN_POINT ( 'NONE',  ( -17.24945551514599984, -15.50000000000000000, 25.53140320652400064 ) ) ;
#36531 = ORIENTED_EDGE ( 'NONE', *, *, #4552, .F. ) ;
#36532 = ORIENTED_EDGE ( 'NONE', *, *, #29304, .F. ) ;
#36533 = DIRECTION ( 'NONE',  ( 0.000000000000000000, 1.000000000000000000, 0.000000000000000000 ) ) ;
#36535 = EDGE_LOOP ( 'NONE', ( #54816, #50538, #34126, #39121 ) ) ;
#36534 = CARTESIAN_POINT ( 'NONE',  ( 7.000000000000000000, -37.61196062927500350, 8.008708659369300875 ) ) ;
#36536 = ORIENTED_EDGE ( 'NONE', *, *, #23325, .T. ) ;
#36537 = VECTOR ( 'NONE', #32228, 1000.000000000000000 ) ;
#36539 = CARTESIAN_POINT ( 'NONE',  ( 7.250000000000005329, 8.250000000000001776, -26.00000000000001066 ) ) ;
#36538 = AXIS2_PLACEMENT_3D ( 'NONE', #59653, #59985, #60682 ) ;
#36540 = CARTESIAN_POINT ( 'NONE',  ( -8.513516549646713116, 11.29351654964659701, 194.9999952000000292 ) ) ;
#36543 = ORIENTED_EDGE ( 'NONE', *, *, #18031, .T. ) ;
#36542 = EDGE_CURVE ( 'NONE', #56320, #3551, #4398, .T. ) ;
#36541 = CARTESIAN_POINT ( 'NONE',  ( 41.09999999999999432, -14.06939075806901940, -20.80000000000000426 ) ) ;
#36545 = ORIENTED_EDGE ( 'NONE', *, *, #55332, .F. ) ;
#36544 = CIRCLE ( 'NONE', #33151, 5.000000000000000000 ) ;
#36546 = DIRECTION ( 'NONE',  ( 4.121462285523434951E-16, 1.000000000000000000, 3.673940397442059868E-16 ) ) ;
#36547 = MECHANICAL_DESIGN_GEOMETRIC_PRESENTATION_REPRESENTATION (  '', ( #64768 ), #38802 ) ;
#36548 = CIRCLE ( 'NONE', #6071, 8.300000000000002487 ) ;
#36549 = DIRECTION ( 'NONE',  ( -1.836970198721029934E-16, -1.836970198721010706E-16, 1.000000000000000000 ) ) ;
#36550 = LINE ( 'NONE', #42203, #56066 ) ;
#36551 = EDGE_CURVE ( 'NONE', #44628, #21397, #47173, .T. ) ;
#36552 = CARTESIAN_POINT ( 'NONE',  ( 7.250000000000004441, 7.450000000000001954, -8.000000000000000000 ) ) ;
#36553 = CIRCLE ( 'NONE', #15109, 8.000000000000001776 ) ;
#36554 = ORIENTED_EDGE ( 'NONE', *, *, #49780, .T. ) ;
#36555 = DIRECTION ( 'NONE',  ( -1.000000000000000000, 0.000000000000000000, 0.000000000000000000 ) ) ;
#36556 = FACE_OUTER_BOUND ( 'NONE', #6785, .T. ) ;
#36557 = CARTESIAN_POINT ( 'NONE',  ( -16.75000000000000000, -2.500000000000000000, -21.77831216351300014 ) ) ;
#36558 = DIRECTION ( 'NONE',  ( 0.000000000000000000, 1.000000000000000000, 0.000000000000000000 ) ) ;
#36559 = DIRECTION ( 'NONE',  ( -1.000000000000000000, 0.000000000000000000, 0.000000000000000000 ) ) ;
#36560 = ADVANCED_FACE ( 'NONE', ( #64483 ), #15695, .F. ) ;
#36561 = CYLINDRICAL_SURFACE ( 'NONE', #35940, 0.1999999999999987899 ) ;
#36562 = ORIENTED_EDGE ( 'NONE', *, *, #10308, .F. ) ;
#36563 = EDGE_CURVE ( 'NONE', #67923, #27113, #15404, .T. ) ;
#36564 = CARTESIAN_POINT ( 'NONE',  ( 11.48848345035334617, -10.20488345035343336, 195.0000000000000284 ) ) ;
#36565 = PLANE ( 'NONE',  #58206 ) ;
#36566 = LINE ( 'NONE', #31291, #48563 ) ;
#36567 = ORIENTED_EDGE ( 'NONE', *, *, #18323, .T. ) ;
#36568 = PLANE ( 'NONE',  #8980 ) ;
#36569 = LINE ( 'NONE', #3350, #49047 ) ;
#36570 = CARTESIAN_POINT ( 'NONE',  ( 37.90000000000000568, 0.000000000000000000, 0.000000000000000000 ) ) ;
#36571 = AXIS2_PLACEMENT_3D ( 'NONE', #62740, #8995, #52496 ) ;
#36572 = LINE ( 'NONE', #10748, #53917 ) ;
#36573 = CARTESIAN_POINT ( 'NONE',  ( 8.250000000000005329, -7.249999999999998224, -13.00000000000000178 ) ) ;
#36574 = ORIENTED_EDGE ( 'NONE', *, *, #36756, .F. ) ;
#36575 = DIRECTION ( 'NONE',  ( 0.000000000000000000, 0.000000000000000000, -1.000000000000000000 ) ) ;
#36576 = DIRECTION ( 'NONE',  ( -1.836970198721029934E-16, 1.836970198721036590E-16, -1.000000000000000000 ) ) ;
#36577 = FACE_OUTER_BOUND ( 'NONE', #19228, .T. ) ;
#36578 = CYLINDRICAL_SURFACE ( 'NONE', #55716, 4.000000000000000000 ) ;
#36579 = DIRECTION ( 'NONE',  ( -0.7671651518153105309, 0.6414496315691445849, 2.356647714346206145E-16 ) ) ;
#36580 = ORIENTED_EDGE ( 'NONE', *, *, #21988, .F. ) ;
#36582 = EDGE_LOOP ( 'NONE', ( #69807, #34790 ) ) ;
#36581 = DIRECTION ( 'NONE',  ( -1.000000000000000000, 0.000000000000000000, 0.000000000000000000 ) ) ;
#36583 = EDGE_CURVE ( 'NONE', #36864, #4457, #36550, .T. ) ;
#36584 = AXIS2_PLACEMENT_3D ( 'NONE', #36761, #30398, #4584 ) ;
#36585 = AXIS2_PLACEMENT_3D ( 'NONE', #14349, #46504, #68079 ) ;
#36586 = CARTESIAN_POINT ( 'NONE',  ( -1.620245201994373385, -8.241237374594328813, 54.00000000000000711 ) ) ;
#36587 = EDGE_CURVE ( 'NONE', #47575, #20267, #41509, .T. ) ;
#36588 = CARTESIAN_POINT ( 'NONE',  ( 11.50000000000000000, -11.50000000000000000, 11.00000000000000000 ) ) ;
#36589 = DIRECTION ( 'NONE',  ( -4.956352788505168198E-15, -1.000000000000000000, 0.000000000000000000 ) ) ;
#36590 = ORIENTED_EDGE ( 'NONE', *, *, #1847, .T. ) ;
#36591 = EDGE_CURVE ( 'NONE', #20264, #51421, #63785, .T. ) ;
#36592 = CARTESIAN_POINT ( 'NONE',  ( 283.0000000000000568, -32.95000000000000284, 13.19999999999999929 ) ) ;
#36593 = VECTOR ( 'NONE', #18472, 1000.000000000000000 ) ;
#36594 = CARTESIAN_POINT ( 'NONE',  ( -11.75000000000000000, -5.000000000000000000, -23.89194109070750471 ) ) ;
#36595 = AXIS2_PLACEMENT_3D ( 'NONE', #65270, #923, #17153 ) ;
#36596 = EDGE_CURVE ( 'NONE', #67938, #53770, #25607, .T. ) ;
#36597 = ORIENTED_EDGE ( 'NONE', *, *, #51834, .T. ) ;
#36598 = VERTEX_POINT ( 'NONE', #5081 ) ;
#36599 = ADVANCED_FACE ( 'NONE', ( #10039 ), #31614, .T. ) ;
#36601 = ORIENTED_EDGE ( 'NONE', *, *, #49305, .T. ) ;
#36600 = CIRCLE ( 'NONE', #20799, 0.1749999999999998224 ) ;
#36602 = EDGE_CURVE ( 'NONE', #28757, #13195, #31955, .T. ) ;
#36603 = CARTESIAN_POINT ( 'NONE',  ( 8.241237374594247100, 1.620245201994230611, 54.00000000000000711 ) ) ;
#36604 = ADVANCED_FACE ( 'NONE', ( #21342 ), #22036, .F. ) ;
#36605 = DIRECTION ( 'NONE',  ( -1.000000000000000000, 0.000000000000000000, 0.000000000000000000 ) ) ;
#36606 = DIRECTION ( 'NONE',  ( -1.836970198721029934E-16, 1.836970198721036590E-16, -1.000000000000000000 ) ) ;
#36607 = ORIENTED_EDGE ( 'NONE', *, *, #14252, .T. ) ;
#36608 = ORIENTED_EDGE ( 'NONE', *, *, #39908, .T. ) ;
#36609 = CARTESIAN_POINT ( 'NONE',  ( 15.50000000000000000, -0.2038245569916610489, 21.05662432702600029 ) ) ;
#36610 = AXIS2_PLACEMENT_3D ( 'NONE', #25571, #64109, #36158 ) ;
#36611 = CARTESIAN_POINT ( 'NONE',  ( 17.24945551514599984, -17.50000000000000000, 25.53140320652400064 ) ) ;
#36612 = ORIENTED_EDGE ( 'NONE', *, *, #51938, .F. ) ;
#36613 = ORIENTED_EDGE ( 'NONE', *, *, #14559, .F. ) ;
#36614 = ORIENTED_EDGE ( 'NONE', *, *, #11194, .F. ) ;
#36615 = ORIENTED_EDGE ( 'NONE', *, *, #59645, .T. ) ;
#36616 = LINE ( 'NONE', #25315, #3403 ) ;
#36617 = UNCERTAINTY_MEASURE_WITH_UNIT (LENGTH_MEASURE( 1.000000000000000082E-05 ), #51449, 'distance_accuracy_value', 'NONE');
#36619 = ORIENTED_EDGE ( 'NONE', *, *, #15675, .T. ) ;
#36618 = FACE_OUTER_BOUND ( 'NONE', #35005, .T. ) ;
#36620 = CYLINDRICAL_SURFACE ( 'NONE', #5218, 0.2999999999994933941 ) ;
#36621 = CARTESIAN_POINT ( 'NONE',  ( 49.00000000000000000, -0.2000000000089119934, -8.913009219568841313E-12 ) ) ;
#36622 = EDGE_CURVE ( 'NONE', #14877, #66251, #6362, .T. ) ;
#36623 = CARTESIAN_POINT ( 'NONE',  ( -3.834182069070823040, -7.357023737882818715, 54.00000000000000711 ) ) ;
#36624 = EDGE_LOOP ( 'NONE', ( #4794, #61379, #52096, #51199 ) ) ;
#36625 = AXIS2_PLACEMENT_3D ( 'NONE', #31635, #26320, #27368 ) ;
#36626 = ORIENTED_EDGE ( 'NONE', *, *, #55740, .F. ) ;
#36627 = CIRCLE ( 'NONE', #6147, 0.3999999999999993006 ) ;
#36628 = EDGE_CURVE ( 'NONE', #57897, #36105, #48162, .T. ) ;
#36629 = CARTESIAN_POINT ( 'NONE',  ( 10.20488345035345645, 11.07551654964652954, 455.0000000000000568 ) ) ;
#36630 = CARTESIAN_POINT ( 'NONE',  ( 0.5000000000000000000, -21.00000000000000000, 18.00000000000000355 ) ) ;
#36631 = ORIENTED_EDGE ( 'NONE', *, *, #58058, .F. ) ;
#36632 = CIRCLE ( 'NONE', #44541, 24.99999999998789946 ) ;
#36633 = AXIS2_PLACEMENT_3D ( 'NONE', #39299, #7462, #44948 ) ;
#36634 = CYLINDRICAL_SURFACE ( 'NONE', #8542, 0.1999999999999987899 ) ;
#36635 = CARTESIAN_POINT ( 'NONE',  ( 23.90000000000000213, -0.2000000000089119934, -8.913009219568841313E-12 ) ) ;
#36636 = DIRECTION ( 'NONE',  ( 0.000000000000000000, 0.000000000000000000, -1.000000000000000000 ) ) ;
#36637 = ORIENTED_EDGE ( 'NONE', *, *, #15210, .F. ) ;
#36638 = DIRECTION ( 'NONE',  ( -1.000000000000000000, 0.000000000000000000, 0.000000000000000000 ) ) ;
#36639 = DIRECTION ( 'NONE',  ( 0.000000000000000000, 1.000000000000000000, 0.000000000000000000 ) ) ;
#36640 = VECTOR ( 'NONE', #4961, 1000.000000000000000 ) ;
#36641 = CIRCLE ( 'NONE', #63765, 0.5000000000001357803 ) ;
#36643 = CIRCLE ( 'NONE', #33268, 0.3499999999999996447 ) ;
#36642 = PLANE ( 'NONE',  #37600 ) ;
#36644 = FACE_OUTER_BOUND ( 'NONE', #20586, .T. ) ;
#36645 = AXIS2_PLACEMENT_3D ( 'NONE', #13718, #19030, #56845 ) ;
#36646 = EDGE_CURVE ( 'NONE', #11146, #54627, #49277, .T. ) ;
#36647 = CARTESIAN_POINT ( 'NONE',  ( -30.00000000000000000, -5.599999999999999645, 9.000000000000001776 ) ) ;
#36648 = VERTEX_POINT ( 'NONE', #49932 ) ;
#36649 = PLANE ( 'NONE',  #51670 ) ;
#36650 = CARTESIAN_POINT ( 'NONE',  ( 7.000000000000000000, -32.45000000000000995, -15.00000000000000000 ) ) ;
#36651 = DIRECTION ( 'NONE',  ( -0.000000000000000000, 0.000000000000000000, 1.000000000000000000 ) ) ;
#36652 = CARTESIAN_POINT ( 'NONE',  ( 7.450000000000006395, 7.250000000000000888, -23.50000000000000000 ) ) ;
#36653 = ORIENTED_EDGE ( 'NONE', *, *, #7997, .F. ) ;
#36654 = AXIS2_PLACEMENT_3D ( 'NONE', #52034, #35395, #36106 ) ;
#36655 = DIRECTION ( 'NONE',  ( 0.000000000000000000, 0.000000000000000000, 1.000000000000000000 ) ) ;
#36656 = ADVANCED_FACE ( 'NONE', ( #49260 ), #65851, .T. ) ;
#36657 = CARTESIAN_POINT ( 'NONE',  ( 283.0000000000000568, -42.50000000000000000, -14.49999999999903899 ) ) ;
#36659 = EDGE_CURVE ( 'NONE', #14927, #63906, #52661, .T. ) ;
#36658 = CIRCLE ( 'NONE', #6180, 3.499999999999040323 ) ;
#36660 = DIRECTION ( 'NONE',  ( -0.000000000000000000, -0.000000000000000000, -1.000000000000000000 ) ) ;
#36661 = DIRECTION ( 'NONE',  ( 1.000000000000000000, -0.000000000000000000, 0.000000000000000000 ) ) ;
#36662 = ORIENTED_EDGE ( 'NONE', *, *, #61252, .T. ) ;
#36663 = CARTESIAN_POINT ( 'NONE',  ( 14.66242688423474583, -0.3152598339554803508, 23.45980260912095616 ) ) ;
#36664 = PLANE ( 'NONE',  #154 ) ;
#36665 = EDGE_CURVE ( 'NONE', #33912, #5044, #22391, .T. ) ;
#36666 = DIRECTION ( 'NONE',  ( -1.000000000000000000, 0.000000000000000000, 0.000000000000000000 ) ) ;
#36667 = EDGE_CURVE ( 'NONE', #16772, #65595, #6472, .T. ) ;
#36668 = ADVANCED_FACE ( 'NONE', ( #37958 ), #64828, .T. ) ;
#36669 = DIRECTION ( 'NONE',  ( 0.000000000000000000, -0.1111111111108840643, -0.9938079899999319178 ) ) ;
#36670 = CARTESIAN_POINT ( 'NONE',  ( -7.250000000000001776, -7.249999999999998224, -13.50000000000000178 ) ) ;
#36671 = CARTESIAN_POINT ( 'NONE',  ( -8.598420958951683346, 1.991476262117183316, 26.00000000000000711 ) ) ;
#36672 = CARTESIAN_POINT ( 'NONE',  ( 11.08848345035334404, -9.804883450353528929, 455.0000000000000568 ) ) ;
#36673 = ORIENTED_EDGE ( 'NONE', *, *, #61955, .F. ) ;
#36674 = EDGE_CURVE ( 'NONE', #56714, #34394, #18765, .T. ) ;
#36675 = ORIENTED_EDGE ( 'NONE', *, *, #40958, .T. ) ;
#36676 = LINE ( 'NONE', #15806, #47379 ) ;
#36677 = EDGE_CURVE ( 'NONE', #37252, #26529, #32647, .T. ) ;
#36678 = CARTESIAN_POINT ( 'NONE',  ( -15.08757311576351690, -0.3152598339557960427, 23.70526090033903444 ) ) ;
#36679 = ORIENTED_EDGE ( 'NONE', *, *, #56120, .F. ) ;
#36680 = VECTOR ( 'NONE', #58693, 1000.000000000000000 ) ;
#36681 = CARTESIAN_POINT ( 'NONE',  ( -11.07551654964683330, -11.48848345035333907, 455.0000000000000568 ) ) ;
#36682 = EDGE_CURVE ( 'NONE', #17779, #51662, #59168, .T. ) ;
#36683 = CARTESIAN_POINT ( 'NONE',  ( 11.00000000000000000, -17.50000000000000000, 60.00000000000000000 ) ) ;
#36684 = AXIS2_PLACEMENT_3D ( 'NONE', #24305, #6653, #39512 ) ;
#36685 = ORIENTED_EDGE ( 'NONE', *, *, #33503, .F. ) ;
#36686 = DIRECTION ( 'NONE',  ( 1.000000000000000000, 0.000000000000000000, 0.000000000000000000 ) ) ;
#36687 = EDGE_LOOP ( 'NONE', ( #9586, #28081, #58700, #8331, #66638, #50958, #7765, #4 ) ) ;
#36688 = VERTEX_POINT ( 'NONE', #1165 ) ;
#36690 = EDGE_CURVE ( 'NONE', #10380, #68245, #11416, .T. ) ;
#36689 = FACE_OUTER_BOUND ( 'NONE', #11808, .T. ) ;
#36691 = ORIENTED_EDGE ( 'NONE', *, *, #61585, .F. ) ;
#36692 = EDGE_CURVE ( 'NONE', #1993, #69377, #53497, .T. ) ;
#36693 = DIRECTION ( 'NONE',  ( 0.000000000000000000, -1.000000000000000000, 0.000000000000000000 ) ) ;
#36694 = CARTESIAN_POINT ( 'NONE',  ( 275.0000000000000000, -42.00000000000000000, -26.50000000000000000 ) ) ;
#36695 = AXIS2_PLACEMENT_3D ( 'NONE', #36845, #11336, #15626 ) ;
#36696 = AXIS2_PLACEMENT_3D ( 'NONE', #49142, #48103, #10274 ) ;
#36697 = DIRECTION ( 'NONE',  ( 0.000000000000000000, 0.000000000000000000, -1.000000000000000000 ) ) ;
#36698 = ORIENTED_EDGE ( 'NONE', *, *, #58301, .F. ) ;
#36699 = CARTESIAN_POINT ( 'NONE',  ( -7.250000000000000888, 8.250000000000001776, -13.00000000000000178 ) ) ;
#36701 = DIRECTION ( 'NONE',  ( -0.000000000000000000, -0.000000000000000000, -1.000000000000000000 ) ) ;
#36700 = CARTESIAN_POINT ( 'NONE',  ( 7.811466277050736373, -7.272650909786632312, 195.0000000000000284 ) ) ;
#36702 = CIRCLE ( 'NONE', #45710, 0.06000000000000102474 ) ;
#36703 = ORIENTED_EDGE ( 'NONE', *, *, #69159, .F. ) ;
#36704 = ORIENTED_EDGE ( 'NONE', *, *, #6823, .F. ) ;
#36705 = EDGE_CURVE ( 'NONE', #23856, #63336, #21691, .T. ) ;
#36706 = ORIENTED_EDGE ( 'NONE', *, *, #57389, .F. ) ;
#36708 = EDGE_LOOP ( 'NONE', ( #2714, #34220, #532, #3050 ) ) ;
#36707 = ITEM_DEFINED_TRANSFORMATION ( 'NONE', 'NONE', #32408,  #49371 ) ;
#36709 = AXIS2_PLACEMENT_3D ( 'NONE', #63986, #58331, #53374 ) ;
#36710 = FACE_BOUND ( 'NONE', #7913, .T. ) ;
#36712 = VERTEX_POINT ( 'NONE', #133 ) ;
#36711 = DIRECTION ( 'NONE',  ( 1.000000000000000000, -5.981805089575194965E-17, 0.000000000000000000 ) ) ;
#36713 = DIRECTION ( 'NONE',  ( -0.6414496315691526895, -0.7671651518153038696, 0.000000000000000000 ) ) ;
#36714 = VECTOR ( 'NONE', #49009, 1000.000000000000000 ) ;
#36715 = DIRECTION ( 'NONE',  ( 1.000000000000000000, 0.000000000000000000, 0.000000000000000000 ) ) ;
#36717 = ORIENTED_EDGE ( 'NONE', *, *, #49004, .T. ) ;
#36716 = VECTOR ( 'NONE', #54913, 1000.000000000000000 ) ;
#36718 = ORIENTED_EDGE ( 'NONE', *, *, #43010, .T. ) ;
#36719 = COLOUR_RGB ( '', 0.09019608, 0.27058824, 0.51372549) ;
#36720 = DIRECTION ( 'NONE',  ( -1.000000000000000000, 0.000000000000000000, 0.000000000000000000 ) ) ;
#36721 = ORIENTED_EDGE ( 'NONE', *, *, #39298, .T. ) ;
#36722 = ADVANCED_FACE ( 'NONE', ( #44614 ), #17073, .F. ) ;
#36723 = FACE_OUTER_BOUND ( 'NONE', #57666, .T. ) ;
#36724 = CARTESIAN_POINT ( 'NONE',  ( -7.450000000000001954, 7.250000000000000000, -12.50000000000000000 ) ) ;
#36725 = DIRECTION ( 'NONE',  ( -1.000000000000000000, 0.000000000000000000, 0.000000000000000000 ) ) ;
#36726 = ORIENTED_EDGE ( 'NONE', *, *, #41853, .F. ) ;
#36727 = EDGE_CURVE ( 'NONE', #42288, #60085, #28366, .T. ) ;
#36728 = CYLINDRICAL_SURFACE ( 'NONE', #9684, 0.5249999999999990230 ) ;
#36729 = LINE ( 'NONE', #19744, #32400 ) ;
#36731 = EDGE_LOOP ( 'NONE', ( #16652, #8382, #54470, #21113 ) ) ;
#36730 = LINE ( 'NONE', #52289, #23898 ) ;
#36733 = VERTEX_POINT ( 'NONE', #40000 ) ;
#36732 = CARTESIAN_POINT ( 'NONE',  ( 17.00000000000000000, -16.28999999999999915, 14.50000000000000000 ) ) ;
#36734 = ADVANCED_FACE ( 'NONE', ( #12779 ), #3243, .T. ) ;
#36735 = CARTESIAN_POINT ( 'NONE',  ( 25.57999999999999829, 3.010794155703768650E-16, -2.458500000000000796 ) ) ;
#36736 = FACE_OUTER_BOUND ( 'NONE', #54646, .T. ) ;
#36737 = EDGE_CURVE ( 'NONE', #4384, #43288, #10903, .T. ) ;
#36738 = CIRCLE ( 'NONE', #35547, 0.5000000000079367624 ) ;
#36739 = LINE ( 'NONE', #25425, #32477 ) ;
#36740 = LINE ( 'NONE', #37096, #13672 ) ;
#36741 = VECTOR ( 'NONE', #65027, 1000.000000000000000 ) ;
#36742 = EDGE_CURVE ( 'NONE', #10806, #26444, #51692, .T. ) ;
#36743 = LINE ( 'NONE', #42037, #36449 ) ;
#36744 = ORIENTED_EDGE ( 'NONE', *, *, #20276, .T. ) ;
#36745 = CARTESIAN_POINT ( 'NONE',  ( -11.11351654964671098, 7.793516549646603231, 455.0000000000000568 ) ) ;
#36746 = LINE ( 'NONE', #53705, #10192 ) ;
#36748 = VERTEX_POINT ( 'NONE', #24464 ) ;
#36747 = CYLINDRICAL_SURFACE ( 'NONE', #10792, 3.499999999999853895 ) ;
#36749 = CIRCLE ( 'NONE', #48048, 1.500000000000001332 ) ;
#36750 = VECTOR ( 'NONE', #305, 1000.000000000000000 ) ;
#36751 = VECTOR ( 'NONE', #63222, 1000.000000000000000 ) ;
#36752 = DIRECTION ( 'NONE',  ( -1.000000000000000000, 0.000000000000000000, 0.000000000000000000 ) ) ;
#36753 = DIRECTION ( 'NONE',  ( 1.000000000000000000, -0.000000000000000000, -0.000000000000000000 ) ) ;
#36754 = EDGE_CURVE ( 'NONE', #62419, #13697, #45310, .T. ) ;
#36755 = DIRECTION ( 'NONE',  ( -0.000000000000000000, 3.673940397442059868E-16, -1.000000000000000000 ) ) ;
#36756 = EDGE_CURVE ( 'NONE', #49922, #32098, #34346, .T. ) ;
#36757 = VECTOR ( 'NONE', #3819, 1000.000000000000000 ) ;
#36758 = CIRCLE ( 'NONE', #68344, 0.5000000000001362244 ) ;
#36759 = LINE ( 'NONE', #57959, #25449 ) ;
#36760 = ORIENTED_EDGE ( 'NONE', *, *, #37152, .F. ) ;
#36761 = CARTESIAN_POINT ( 'NONE',  ( -2.406732575409671337, -8.711985858128709737, 54.00000000000000711 ) ) ;
#36762 = DIRECTION ( 'NONE',  ( 1.000000000000000000, 0.000000000000000000, 0.000000000000000000 ) ) ;
#36763 = ORIENTED_EDGE ( 'NONE', *, *, #859, .T. ) ;
#36764 = CARTESIAN_POINT ( 'NONE',  ( 40.90000000000000568, -21.00000000000000000, 13.86939075806900057 ) ) ;
#36765 = EDGE_CURVE ( 'NONE', #32155, #5314, #35400, .T. ) ;
#36766 = ADVANCED_FACE ( 'NONE', ( #50632 ), #13494, .T. ) ;
#36767 = CYLINDRICAL_SURFACE ( 'NONE', #67209, 8.000000000000000000 ) ;
#36768 = AXIS2_PLACEMENT_3D ( 'NONE', #63938, #58972, #57923 ) ;
#36769 = CARTESIAN_POINT ( 'NONE',  ( -16.75000000000000000, -2.500000000000000000, 23.22168783648699986 ) ) ;
#36770 = FACE_OUTER_BOUND ( 'NONE', #67355, .T. ) ;
#36771 = EDGE_CURVE ( 'NONE', #35602, #56028, #66879, .T. ) ;
#36772 = DIRECTION ( 'NONE',  ( 1.000000000000000000, 0.000000000000000000, 0.000000000000000000 ) ) ;
#36773 = VECTOR ( 'NONE', #23158, 1000.000000000000000 ) ;
#36774 = ORIENTED_EDGE ( 'NONE', *, *, #61997, .F. ) ;
#36775 = ORIENTED_EDGE ( 'NONE', *, *, #16896, .F. ) ;
#36776 = CARTESIAN_POINT ( 'NONE',  ( 8.241237374594303944, -1.634292677759877410, 26.00000000000000711 ) ) ;
#36777 = ORIENTED_EDGE ( 'NONE', *, *, #43846, .T. ) ;
#36778 = ORIENTED_EDGE ( 'NONE', *, *, #34510, .T. ) ;
#36779 = AXIS2_PLACEMENT_3D ( 'NONE', #38902, #53, #26923 ) ;
#36780 = DIRECTION ( 'NONE',  ( 1.000000000000000000, 0.000000000000000000, -8.994862468027880808E-15 ) ) ;
#36781 = CARTESIAN_POINT ( 'NONE',  ( 7.900000000000000355, -21.00000000000000000, -18.00000000000000355 ) ) ;
#36782 = CARTESIAN_POINT ( 'NONE',  ( -8.393516549646712122, 6.331612867284047041, 455.0000000000000568 ) ) ;
#36783 = ORIENTED_EDGE ( 'NONE', *, *, #50860, .F. ) ;
#36784 = ORIENTED_EDGE ( 'NONE', *, *, #67406, .T. ) ;
#36786 = EDGE_CURVE ( 'NONE', #53128, #40022, #29404, .T. ) ;
#36785 = CARTESIAN_POINT ( 'NONE',  ( 7.532023737882806103, 6.651770455163672047, 54.00000000000000711 ) ) ;
#36787 = ORIENTED_EDGE ( 'NONE', *, *, #69806, .T. ) ;
#36788 = ORIENTED_EDGE ( 'NONE', *, *, #10808, .T. ) ;
#36789 = EDGE_CURVE ( 'NONE', #42345, #25681, #61663, .T. ) ;
#36790 = CARTESIAN_POINT ( 'NONE',  ( 0.000000000000000000, -8.249999999999998224, -25.50000000000000355 ) ) ;
#36791 = DIRECTION ( 'NONE',  ( 0.000000000000000000, -0.1111111111108840643, -0.9938079899999319178 ) ) ;
#36792 = CARTESIAN_POINT ( 'NONE',  ( -30.00000000000000000, -11.50000000000100009, 15.00000000000084910 ) ) ;
#36793 = CIRCLE ( 'NONE', #54851, 3.499999999999056310 ) ;
#36794 = ORIENTED_EDGE ( 'NONE', *, *, #6881, .F. ) ;
#36795 = DIRECTION ( 'NONE',  ( -1.794541526872559352E-16, -1.000000000000000000, 0.000000000000000000 ) ) ;
#36797 = LINE ( 'NONE', #15226, #10652 ) ;
#36796 = CARTESIAN_POINT ( 'NONE',  ( 7.250000000000005329, 7.250000000000000888, -26.00000000000001066 ) ) ;
#36798 = ORIENTED_EDGE ( 'NONE', *, *, #6122, .T. ) ;
#36800 = ORIENTED_EDGE ( 'NONE', *, *, #51811, .F. ) ;
#36799 = LINE ( 'NONE', #8860, #8194 ) ;
#36801 = VECTOR ( 'NONE', #51182, 1000.000000000000000 ) ;
#36802 = VERTEX_POINT ( 'NONE', #50280 ) ;
#36803 = AXIS2_PLACEMENT_3D ( 'NONE', #17524, #22150, #28817 ) ;
#36804 = CARTESIAN_POINT ( 'NONE',  ( 17.89999999999999858, -21.00000000000000000, 13.86939075806900057 ) ) ;
#36805 = AXIS2_PLACEMENT_3D ( 'NONE', #34075, #40794, #4387 ) ;
#36806 = AXIS2_PLACEMENT_3D ( 'NONE', #19332, #39837, #3088 ) ;
#36808 = FACE_OUTER_BOUND ( 'NONE', #1479, .T. ) ;
#36807 = CIRCLE ( 'NONE', #31153, 0.1749999999999998224 ) ;
#36809 = VERTEX_POINT ( 'NONE', #55592 ) ;
#36810 = AXIS2_PLACEMENT_3D ( 'NONE', #36283, #53606, #26378 ) ;
#36811 = AXIS2_PLACEMENT_3D ( 'NONE', #44064, #5902, #6594 ) ;
#36812 = VECTOR ( 'NONE', #49896, 1000.000000000000000 ) ;
#36813 = CARTESIAN_POINT ( 'NONE',  ( 283.0000000000000568, -25.60000000000000142, 15.10000000000000142 ) ) ;
#36814 = DIRECTION ( 'NONE',  ( 0.000000000000000000, 0.000000000000000000, 1.000000000000000000 ) ) ;
#36815 = VERTEX_POINT ( 'NONE', #13140 ) ;
#36816 = ORIENTED_EDGE ( 'NONE', *, *, #69354, .F. ) ;
#36817 = LINE ( 'NONE', #59418, #29676 ) ;
#36818 = AXIS2_PLACEMENT_3D ( 'NONE', #55746, #50775, #13301 ) ;
#36819 = DIRECTION ( 'NONE',  ( 0.000000000000000000, 0.000000000000000000, -1.000000000000000000 ) ) ;
#36820 = ORIENTED_EDGE ( 'NONE', *, *, #63392, .T. ) ;
#36821 = EDGE_CURVE ( 'NONE', #57153, #61785, #36867, .T. ) ;
#36822 = FACE_OUTER_BOUND ( 'NONE', #40051, .T. ) ;
#36823 = PLANE ( 'NONE',  #47534 ) ;
#36825 = ORIENTED_EDGE ( 'NONE', *, *, #14521, .F. ) ;
#36824 = DIRECTION ( 'NONE',  ( 0.000000000000000000, 0.000000000000000000, -1.000000000000000000 ) ) ;
#36826 = VECTOR ( 'NONE', #27520, 1000.000000000000000 ) ;
#36828 = VERTEX_POINT ( 'NONE', #12433 ) ;
#36827 = CARTESIAN_POINT ( 'NONE',  ( -11.47551654964682122, -10.20488345035336941, 455.0000000000000568 ) ) ;
#36829 = EDGE_CURVE ( 'NONE', #43764, #29937, #18093, .T. ) ;
#36830 = DIRECTION ( 'NONE',  ( 0.000000000000000000, 0.000000000000000000, -1.000000000000000000 ) ) ;
#36831 = DIRECTION ( 'NONE',  ( -1.000000000000000000, 0.000000000000000000, 0.000000000000000000 ) ) ;
#36832 = EDGE_CURVE ( 'NONE', #55425, #47809, #51324, .T. ) ;
#36833 = DIRECTION ( 'NONE',  ( -0.7671651518152962090, 0.6414496315691619044, 0.000000000000000000 ) ) ;
#36834 = ADVANCED_FACE ( 'NONE', ( #29066 ), #67244, .F. ) ;
#36835 = DIRECTION ( 'NONE',  ( 1.000000000000000000, -3.491481338843132961E-15, 0.000000000000000000 ) ) ;
#36836 = CARTESIAN_POINT ( 'NONE',  ( 283.0000000000000568, -30.80000000000000071, -12.20000000000000107 ) ) ;
#36837 = EDGE_CURVE ( 'NONE', #43499, #21463, #50979, .T. ) ;
#36838 = EDGE_CURVE ( 'NONE', #36344, #34855, #22213, .T. ) ;
#36839 = CARTESIAN_POINT ( 'NONE',  ( 7.450000000000004619, -1.336933437520057563E-15, -12.00000000000000000 ) ) ;
#36840 = EDGE_LOOP ( 'NONE', ( #31806, #7351, #31427, #42244 ) ) ;
#36841 = DIRECTION ( 'NONE',  ( 0.000000000000000000, 0.000000000000000000, 1.000000000000000000 ) ) ;
#36842 = ADVANCED_BREP_SHAPE_REPRESENTATION ( '', ( #65930, #45918 ), #25755 ) ;
#36844 = ORIENTED_EDGE ( 'NONE', *, *, #57211, .F. ) ;
#36843 = CARTESIAN_POINT ( 'NONE',  ( 7.450000000000004619, -1.336933437520057563E-15, -24.50000000000000000 ) ) ;
#36845 = CARTESIAN_POINT ( 'NONE',  ( 30.00000000000000000, -9.200000000000120082, 17.30000000000000071 ) ) ;
#36846 = FACE_BOUND ( 'NONE', #23752, .T. ) ;
#36847 = CARTESIAN_POINT ( 'NONE',  ( 8.750000000000005329, 7.250000000000000888, -30.00000000000001066 ) ) ;
#36848 = AXIS2_PLACEMENT_3D ( 'NONE', #62806, #14377, #35941 ) ;
#36849 = LINE ( 'NONE', #64078, #5866 ) ;
#36850 = CIRCLE ( 'NONE', #25534, 0.4999999999991867061 ) ;
#36851 = ORIENTED_EDGE ( 'NONE', *, *, #68107, .F. ) ;
#36852 = LINE ( 'NONE', #20567, #30891 ) ;
#36853 = DIRECTION ( 'NONE',  ( -1.000000000000000000, 0.000000000000000000, 0.000000000000000000 ) ) ;
#36854 = EDGE_LOOP ( 'NONE', ( #8500, #25720 ) ) ;
#36855 = DIRECTION ( 'NONE',  ( -1.836970198721029934E-16, 1.836970198721036590E-16, -1.000000000000000000 ) ) ;
#36856 = AXIS2_PLACEMENT_3D ( 'NONE', #60577, #49960, #1521 ) ;
#36857 = DIRECTION ( 'NONE',  ( -1.000000000000000000, 2.309061475090597584E-14, 0.000000000000000000 ) ) ;
#36858 = CIRCLE ( 'NONE', #17645, 1.399999999999999245 ) ;
#36859 = AXIS2_PLACEMENT_3D ( 'NONE', #34450, #47103, #52407 ) ;
#36860 = CIRCLE ( 'NONE', #48156, 4.000000000000000888 ) ;
#36861 = CARTESIAN_POINT ( 'NONE',  ( -10.73351654964671198, 1.077516549646603483, 455.0000000000000568 ) ) ;
#36862 = ORIENTED_EDGE ( 'NONE', *, *, #34019, .T. ) ;
#36863 = DIRECTION ( 'NONE',  ( 0.000000000000000000, 0.000000000000000000, -1.000000000000000000 ) ) ;
#36864 = VERTEX_POINT ( 'NONE', #30109 ) ;
#36865 = VERTEX_POINT ( 'NONE', #61932 ) ;
#36866 = CARTESIAN_POINT ( 'NONE',  ( -7.450000000000001954, 7.250000000000000000, -10.50000000000000000 ) ) ;
#36868 = FACE_OUTER_BOUND ( 'NONE', #57245, .T. ) ;
#36867 = CIRCLE ( 'NONE', #45862, 1.929199999999998028 ) ;
#36869 = AXIS2_PLACEMENT_3D ( 'NONE', #29270, #46246, #7710 ) ;
#36870 = CARTESIAN_POINT ( 'NONE',  ( 15.90000000000000036, -0.000000000000000000, 20.80000000000000426 ) ) ;
#36871 = DIRECTION ( 'NONE',  ( 0.000000000000000000, 0.000000000000000000, -1.000000000000000000 ) ) ;
#36872 = DIRECTION ( 'NONE',  ( 0.000000000000000000, 0.000000000000000000, 1.000000000000000000 ) ) ;
#36873 = ORIENTED_EDGE ( 'NONE', *, *, #40367, .T. ) ;
#36874 = EDGE_LOOP ( 'NONE', ( #10187, #37334, #48568, #18405 ) ) ;
#36876 = ORIENTED_EDGE ( 'NONE', *, *, #48346, .F. ) ;
#36875 = FACE_OUTER_BOUND ( 'NONE', #52644, .T. ) ;
#36877 = ORIENTED_EDGE ( 'NONE', *, *, #39736, .F. ) ;
#36878 = EDGE_CURVE ( 'NONE', #40309, #41587, #24811, .T. ) ;
#36879 = AXIS2_PLACEMENT_3D ( 'NONE', #51058, #7573, #45393 ) ;
#36880 = CARTESIAN_POINT ( 'NONE',  ( 25.50000000000000355, -5.578999999999999737, 22.50000000000000000 ) ) ;
#36881 = CARTESIAN_POINT ( 'NONE',  ( 14.50000000000000000, -0.5000000000000000000, -27.00000000000000000 ) ) ;
#36882 = CARTESIAN_POINT ( 'NONE',  ( -15.50000000000000000, -5.000000000000000000, 22.50000000000000000 ) ) ;
#36883 = EDGE_CURVE ( 'NONE', #10391, #47005, #51582, .T. ) ;
#36884 = CARTESIAN_POINT ( 'NONE',  ( -7.798499376344062206, -4.740315990920112021, 195.0000000000000284 ) ) ;
#36886 = DIRECTION ( 'NONE',  ( -1.000000000000000000, 0.000000000000000000, 0.000000000000000000 ) ) ;
#36885 = LINE ( 'NONE', #14257, #53585 ) ;
#36887 = VERTEX_POINT ( 'NONE', #68295 ) ;
#36888 = ORIENTED_EDGE ( 'NONE', *, *, #51576, .T. ) ;
#36889 = ORIENTED_EDGE ( 'NONE', *, *, #19087, .F. ) ;
#36890 = DIRECTION ( 'NONE',  ( 1.000000000000000000, 0.000000000000000000, 0.000000000000000000 ) ) ;
#36891 = CARTESIAN_POINT ( 'NONE',  ( -5.655420232009250370, 8.393516549646600211, 455.0000000000000568 ) ) ;
#36892 =( NAMED_UNIT ( * ) PLANE_ANGLE_UNIT ( ) SI_UNIT ( $, .RADIAN. ) );
#36893 = CARTESIAN_POINT ( 'NONE',  ( -2.406732575409671337, -8.711985858128709737, 54.00000000000000711 ) ) ;
#36894 = ORIENTED_EDGE ( 'NONE', *, *, #59583, .F. ) ;
#36895 = ORIENTED_EDGE ( 'NONE', *, *, #16992, .F. ) ;
#36896 = VECTOR ( 'NONE', #65194, 1000.000000000000000 ) ;
#36897 = ORIENTED_EDGE ( 'NONE', *, *, #54086, .F. ) ;
#36898 = PLANE ( 'NONE',  #36205 ) ;
#36899 = VERTEX_POINT ( 'NONE', #3597 ) ;
#36900 = AXIS2_PLACEMENT_3D ( 'NONE', #3369, #25653, #46495 ) ;
#36901 = DIRECTION ( 'NONE',  ( -1.000000000000000000, 0.000000000000000000, 0.000000000000000000 ) ) ;
#36902 = VERTEX_POINT ( 'NONE', #35759 ) ;
#36903 = ORIENTED_EDGE ( 'NONE', *, *, #47130, .T. ) ;
#36904 = VECTOR ( 'NONE', #12690, 1000.000000000000114 ) ;
#36905 = LINE ( 'NONE', #48205, #66663 ) ;
#36907 = ORIENTED_EDGE ( 'NONE', *, *, #24974, .T. ) ;
#36906 = LINE ( 'NONE', #4026, #51470 ) ;
#36908 = ORIENTED_EDGE ( 'NONE', *, *, #16369, .T. ) ;
#36909 = AXIS2_PLACEMENT_3D ( 'NONE', #51085, #56739, #35162 ) ;
#36910 = VECTOR ( 'NONE', #38161, 1000.000000000000000 ) ;
#36911 = EDGE_CURVE ( 'NONE', #68975, #52878, #41762, .T. ) ;
#36912 = CIRCLE ( 'NONE', #16615, 0.9999999999999991118 ) ;
#36913 = CARTESIAN_POINT ( 'NONE',  ( -6.822336235477446387, 4.135079735113101229, 54.00000000000000711 ) ) ;
#36914 = AXIS2_PLACEMENT_3D ( 'NONE', #3385, #46160, #67732 ) ;
#36915 = CARTESIAN_POINT ( 'NONE',  ( 5.393625297349900372, -7.265214908726134624, 195.0000000000000284 ) ) ;
#36917 = EDGE_LOOP ( 'NONE', ( #67476, #3908, #53847, #35902 ) ) ;
#36916 = DIRECTION ( 'NONE',  ( 1.000000000000000000, 0.000000000000000000, 0.000000000000000000 ) ) ;
#36918 = ORIENTED_EDGE ( 'NONE', *, *, #64918, .T. ) ;
#36919 = CARTESIAN_POINT ( 'NONE',  ( 7.450000000000004619, -1.336933437520057563E-15, -22.50000000000000000 ) ) ;
#36920 = VECTOR ( 'NONE', #6711, 1000.000000000000000 ) ;
#36921 = CARTESIAN_POINT ( 'NONE',  ( 15.08757311576526128, -0.3152598339554890106, 21.29473909965996015 ) ) ;
#36922 = AXIS2_PLACEMENT_3D ( 'NONE', #55060, #59306, #54359 ) ;
#36923 = DIRECTION ( 'NONE',  ( 0.000000000000000000, 0.000000000000000000, 1.000000000000000000 ) ) ;
#36924 = DIRECTION ( 'NONE',  ( -1.000000000000000000, 0.000000000000000000, 0.000000000000000000 ) ) ;
#36925 = CARTESIAN_POINT ( 'NONE',  ( 7.900000000000000355, -0.2000000000000000111, 0.000000000000000000 ) ) ;
#36926 = AXIS2_PLACEMENT_3D ( 'NONE', #30007, #8430, #46971 ) ;
#36927 = EDGE_CURVE ( 'NONE', #56572, #27049, #64062, .T. ) ;
#36928 = EDGE_CURVE ( 'NONE', #1307, #5466, #19496, .T. ) ;
#36929 = VERTEX_POINT ( 'NONE', #42115 ) ;
#36930 = CARTESIAN_POINT ( 'NONE',  ( -3.593516549646742497, -7.428221114745029219, 195.0000000000000284 ) ) ;
#36931 = VERTEX_POINT ( 'NONE', #26213 ) ;
#36932 = AXIS2_PLACEMENT_3D ( 'NONE', #40373, #61931, #8889 ) ;
#36933 = DIRECTION ( 'NONE',  ( 0.000000000000000000, 0.000000000000000000, 1.000000000000000000 ) ) ;
#36934 = FACE_OUTER_BOUND ( 'NONE', #33121, .T. ) ;
#36935 = EDGE_CURVE ( 'NONE', #9829, #47150, #17711, .T. ) ;
#36936 = DIRECTION ( 'NONE',  ( 0.000000000000000000, 0.000000000000000000, 1.000000000000000000 ) ) ;
#36937 = DIRECTION ( 'NONE',  ( 0.7071067811865411334, -0.7071067811865539010, -2.597868168706484541E-16 ) ) ;
#36938 = CARTESIAN_POINT ( 'NONE',  ( 0.000000000000000000, -7.449999999999998401, -19.50000000000000000 ) ) ;
#36939 = ORIENTED_EDGE ( 'NONE', *, *, #31398, .T. ) ;
#36940 = DIRECTION ( 'NONE',  ( 0.000000000000000000, -0.000000000000000000, 1.000000000000000000 ) ) ;
#36941 = LINE ( 'NONE', #489, #66122 ) ;
#36942 = PLANE ( 'NONE',  #56412 ) ;
#36943 = VERTEX_POINT ( 'NONE', #19848 ) ;
#36944 = CARTESIAN_POINT ( 'NONE',  ( -3.650476262117335668, -10.50702373788282173, 54.00000000000000711 ) ) ;
#36945 = DIRECTION ( 'NONE',  ( -0.7071067811865550112, -0.7071067811865401342, 0.000000000000000000 ) ) ;
#36946 = CARTESIAN_POINT ( 'NONE',  ( 78.77321854994620765, 47.95351654967443977, 25.00000000000000000 ) ) ;
#36947 = CARTESIAN_POINT ( 'NONE',  ( 46.39999999999999858, 21.00000000000000000, -1.750000000000000222 ) ) ;
#36948 = CYLINDRICAL_SURFACE ( 'NONE', #19544, 0.1999999999999987899 ) ;
#36949 = ORIENTED_EDGE ( 'NONE', *, *, #69768, .T. ) ;
#36950 = CARTESIAN_POINT ( 'NONE',  ( 6.006483450353379716, -6.006483450353490738, 455.0000000000000568 ) ) ;
#36951 = CARTESIAN_POINT ( 'NONE',  ( -11.31351654964669784, -4.406483450353282372, 195.0000000000000284 ) ) ;
#36952 = AXIS2_PLACEMENT_3D ( 'NONE', #48381, #21503, #21169 ) ;
#36953 = DIRECTION ( 'NONE',  ( 0.000000000000000000, -0.7084617869623469621, -0.7057491738671168857 ) ) ;
#36954 = AXIS2_PLACEMENT_3D ( 'NONE', #39834, #60725, #6636 ) ;
#36955 = AXIS2_PLACEMENT_3D ( 'NONE', #23318, #22968, #44518 ) ;
#36956 = CARTESIAN_POINT ( 'NONE',  ( 11.50000000000000000, -11.50000000000000000, -15.00000000000000000 ) ) ;
#36957 = DIRECTION ( 'NONE',  ( 0.5000000000000004441, -0.8660254037844382635, 0.000000000000000000 ) ) ;
#36958 = VERTEX_POINT ( 'NONE', #41062 ) ;
#36960 = ORIENTED_EDGE ( 'NONE', *, *, #50523, .F. ) ;
#36959 = CARTESIAN_POINT ( 'NONE',  ( 30.00000000000000000, -14.04000000000000092, -17.04524521594300523 ) ) ;
#36961 = AXIS2_PLACEMENT_3D ( 'NONE', #16411, #50310, #54947 ) ;
#36962 = AXIS2_PLACEMENT_3D ( 'NONE', #44690, #45740, #55665 ) ;
#36963 = PLANE ( 'NONE',  #60937 ) ;
#36964 = DIRECTION ( 'NONE',  ( 1.280238727658158432E-15, 1.000000000000000000, -0.000000000000000000 ) ) ;
#36965 = DIRECTION ( 'NONE',  ( 0.000000000000000000, 1.000000000000000000, 0.000000000000000000 ) ) ;
#36966 = ORIENTED_EDGE ( 'NONE', *, *, #22849, .T. ) ;
#36967 = EDGE_CURVE ( 'NONE', #6666, #29645, #4206, .T. ) ;
#36968 = EDGE_CURVE ( 'NONE', #63525, #36419, #52037, .T. ) ;
#36969 = ADVANCED_FACE ( 'NONE', ( #9962 ), #52386, .F. ) ;
#36970 = AXIS2_PLACEMENT_3D ( 'NONE', #69520, #69864, #21425 ) ;
#36971 = FACE_OUTER_BOUND ( 'NONE', #48898, .T. ) ;
#36972 = LINE ( 'NONE', #33383, #62362 ) ;
#36973 = VERTEX_POINT ( 'NONE', #8890 ) ;
#36974 = EDGE_LOOP ( 'NONE', ( #61019, #24469, #45996, #39464 ) ) ;
#36975 = ADVANCED_FACE ( 'NONE', ( #14907 ), #68993, .F. ) ;
#36976 = ORIENTED_EDGE ( 'NONE', *, *, #6814, .T. ) ;
#36977 = DIRECTION ( 'NONE',  ( 3.717264591378875951E-15, 1.000000000000000000, 0.000000000000000000 ) ) ;
#36978 = FACE_OUTER_BOUND ( 'NONE', #4900, .T. ) ;
#36979 = CARTESIAN_POINT ( 'NONE',  ( 39.00000000000000000, 0.000000000000000000, 0.000000000000000000 ) ) ;
#36980 = AXIS2_PLACEMENT_3D ( 'NONE', #50550, #2451, #18011 ) ;
#36981 = ORIENTED_EDGE ( 'NONE', *, *, #56592, .F. ) ;
#36982 = ORIENTED_EDGE ( 'NONE', *, *, #37142, .T. ) ;
#36983 = CARTESIAN_POINT ( 'NONE',  ( -7.793516549646781755, -11.12648345035335851, 195.0000000000000284 ) ) ;
#36984 = EDGE_LOOP ( 'NONE', ( #69487, #14704, #21508, #64518 ) ) ;
#36985 = EDGE_LOOP ( 'NONE', ( #57509, #49521, #4972, #21522 ) ) ;
#36986 = ORIENTED_EDGE ( 'NONE', *, *, #34009, .F. ) ;
#36987 = VERTEX_POINT ( 'NONE', #63701 ) ;
#36988 = DIRECTION ( 'NONE',  ( -1.836970198721029934E-16, 1.836970198721036590E-16, -1.000000000000000000 ) ) ;
#36990 = EDGE_LOOP ( 'NONE', ( #45379, #68884, #22717, #18177 ) ) ;
#36989 = LINE ( 'NONE', #3745, #61541 ) ;
#36991 = CARTESIAN_POINT ( 'NONE',  ( 30.00000000000000000, -10.85999999999999943, 9.000000000000001776 ) ) ;
#36992 = DIRECTION ( 'NONE',  ( 0.7071067811865474617, -0.7071067811865474617, 0.000000000000000000 ) ) ;
#36993 = CARTESIAN_POINT ( 'NONE',  ( 12.00000000000000000, 11.18999999999999950, 0.000000000000000000 ) ) ;
#36994 = AXIS2_PLACEMENT_3D ( 'NONE', #10057, #69096, #46816 ) ;
#36995 = VERTEX_POINT ( 'NONE', #3949 ) ;
#36996 = ORIENTED_EDGE ( 'NONE', *, *, #30606, .F. ) ;
#36997 = CARTESIAN_POINT ( 'NONE',  ( 18.89999999999999858, -14.06939075806902117, -20.80000000000000426 ) ) ;
#36998 = VECTOR ( 'NONE', #46384, 1000.000000000000000 ) ;
#36999 = AXIS2_PLACEMENT_3D ( 'NONE', #64565, #5518, #27075 ) ;
#37000 = CARTESIAN_POINT ( 'NONE',  ( -28.00000000000000000, -17.50000000000000000, 15.70500000000000007 ) ) ;
#37001 = VERTEX_POINT ( 'NONE', #47082 ) ;
#37002 = EDGE_CURVE ( 'NONE', #65543, #2608, #24481, .T. ) ;
#37003 = VECTOR ( 'NONE', #23363, 1000.000000000000000 ) ;
#37004 = CIRCLE ( 'NONE', #43754, 0.4999999999945519691 ) ;
#37005 = CARTESIAN_POINT ( 'NONE',  ( -8.250000000000001776, -8.249999999999998224, -26.00000000000001066 ) ) ;
#37006 = ORIENTED_EDGE ( 'NONE', *, *, #16000, .T. ) ;
#37007 = DIRECTION ( 'NONE',  ( 0.000000000000000000, 0.000000000000000000, 1.000000000000000000 ) ) ;
#37008 = EDGE_CURVE ( 'NONE', #40597, #29083, #36465, .T. ) ;
#37009 = EDGE_CURVE ( 'NONE', #42510, #6950, #25871, .T. ) ;
#37010 = FILL_AREA_STYLE ('',( #63867 ) ) ;
#37011 = ORIENTED_EDGE ( 'NONE', *, *, #29392, .T. ) ;
#37012 = DIRECTION ( 'NONE',  ( 0.000000000000000000, -1.000000000000000000, 0.000000000000000000 ) ) ;
#37013 = DIRECTION ( 'NONE',  ( 0.7671651518153029814, 0.6414496315691537998, 0.000000000000000000 ) ) ;
#37014 = CIRCLE ( 'NONE', #28013, 0.5000000000023371305 ) ;
#37015 = CIRCLE ( 'NONE', #6522, 24.99999999998789946 ) ;
#37016 = DIRECTION ( 'NONE',  ( 0.000000000000000000, 0.7071067811865480168, 0.7071067811865470176 ) ) ;
#37017 = EDGE_CURVE ( 'NONE', #32897, #34396, #4650, .T. ) ;
#37018 = DIRECTION ( 'NONE',  ( -1.678252938371784572E-14, -1.000000000000000000, -1.836970198721041520E-16 ) ) ;
#37019 = DIRECTION ( 'NONE',  ( -0.000000000000000000, 3.673940397442059868E-16, -1.000000000000000000 ) ) ;
#37020 = ADVANCED_FACE ( 'NONE', ( #15259 ), #52755, .F. ) ;
#37021 = ORIENTED_EDGE ( 'NONE', *, *, #24085, .F. ) ;
#37022 = LINE ( 'NONE', #26393, #6507 ) ;
#37023 = CARTESIAN_POINT ( 'NONE',  ( -6.642976262117260333, 10.30047626211718104, 54.00000000000000711 ) ) ;
#37024 = EDGE_CURVE ( 'NONE', #60715, #63093, #58402, .T. ) ;
#37025 = CARTESIAN_POINT ( 'NONE',  ( -7.250000000000000888, 7.250000000000001776, -11.00000000000000000 ) ) ;
#37026 = VECTOR ( 'NONE', #37018, 1000.000000000000000 ) ;
#37027 = VERTEX_POINT ( 'NONE', #10299 ) ;
#37028 = FACE_OUTER_BOUND ( 'NONE', #36990, .T. ) ;
#37029 = FACE_BOUND ( 'NONE', #53006, .T. ) ;
#37030 = CARTESIAN_POINT ( 'NONE',  ( 283.0000000000000568, -39.80000000000000426, -12.69999999999999929 ) ) ;
#37031 = CARTESIAN_POINT ( 'NONE',  ( 11.75000000000000000, -5.000000000000000000, -21.10805890929250239 ) ) ;
#37032 = VERTEX_POINT ( 'NONE', #54137 ) ;
#37033 = DIRECTION ( 'NONE',  ( -0.5773502691896257311, -0.5773502691896257311, 0.5773502691896257311 ) ) ;
#37034 = DIRECTION ( 'NONE',  ( -1.000000000000000000, 0.000000000000000000, 0.000000000000000000 ) ) ;
#37035 = DIRECTION ( 'NONE',  ( -0.000000000000000000, -0.000000000000000000, -1.000000000000000000 ) ) ;
#37036 = CARTESIAN_POINT ( 'NONE',  ( -11.00000000000000000, -5.599999999999999645, -9.000000000000001776 ) ) ;
#37037 = SURFACE_STYLE_USAGE ( .BOTH. , #21799 ) ;
#37038 = DIRECTION ( 'NONE',  ( 0.000000000000000000, 0.000000000000000000, 1.000000000000000000 ) ) ;
#37039 = EDGE_LOOP ( 'NONE', ( #1618, #65512, #46822, #66286 ) ) ;
#37040 = ORIENTED_EDGE ( 'NONE', *, *, #39226, .T. ) ;
#37041 = CARTESIAN_POINT ( 'NONE',  ( -6.642976262117328723, -9.912023737882789121, 54.00000000000000711 ) ) ;
#37042 = DIRECTION ( 'NONE',  ( 0.000000000000000000, -0.000000000000000000, -1.000000000000000000 ) ) ;
#37043 = AXIS2_PLACEMENT_3D ( 'NONE', #66562, #55609, #40019 ) ;
#37044 = VERTEX_POINT ( 'NONE', #48832 ) ;
#37045 = CARTESIAN_POINT ( 'NONE',  ( 15.50000000000000000, -2.500000000000000000, -23.94337567297399971 ) ) ;
#37046 = DIRECTION ( 'NONE',  ( 0.000000000000000000, 0.000000000000000000, -1.000000000000000000 ) ) ;
#37047 = VERTEX_POINT ( 'NONE', #21944 ) ;
#37048 = CARTESIAN_POINT ( 'NONE',  ( -7.250000000000000888, 8.750000000000001776, -30.00000000000001066 ) ) ;
#37049 = VERTEX_POINT ( 'NONE', #387 ) ;
#37050 = EDGE_LOOP ( 'NONE', ( #40495, #45266, #16533, #46417 ) ) ;
#37051 = DIRECTION ( 'NONE',  ( 0.000000000000000000, -1.000000000000000000, 0.000000000000000000 ) ) ;
#37052 = ORIENTED_EDGE ( 'NONE', *, *, #57253, .F. ) ;
#37053 = VECTOR ( 'NONE', #60062, 1000.000000000000000 ) ;
#37054 = PLANE ( 'NONE',  #49693 ) ;
#37055 = DIRECTION ( 'NONE',  ( -1.000000000000000000, 0.000000000000000000, 0.000000000000000000 ) ) ;
#37056 = CARTESIAN_POINT ( 'NONE',  ( 49.00000000000000000, -0.2000000000089119934, 8.909539772616881237E-12 ) ) ;
#37057 = EDGE_LOOP ( 'NONE', ( #38688, #23006, #69913, #37339 ) ) ;
#37058 = EDGE_LOOP ( 'NONE', ( #60494, #20882, #69304, #23907 ) ) ;
#37059 = CARTESIAN_POINT ( 'NONE',  ( -7.394232575409614761, 3.710438382363058896, 54.00000000000000711 ) ) ;
#37060 = AXIS2_PLACEMENT_3D ( 'NONE', #22619, #28597, #28952 ) ;
#37061 = CIRCLE ( 'NONE', #6410, 0.1999999999999996503 ) ;
#37063 = DIRECTION ( 'NONE',  ( -0.7071067811865391350, 0.7071067811865560104, 1.750285133459120294E-30 ) ) ;
#37062 = DIRECTION ( 'NONE',  ( 8.673617379884051249E-15, 1.000000000000000000, 0.000000000000000000 ) ) ;
#37064 = EDGE_CURVE ( 'NONE', #40926, #35986, #56114, .T. ) ;
#37065 = VERTEX_POINT ( 'NONE', #65092 ) ;
#37066 = ORIENTED_EDGE ( 'NONE', *, *, #42090, .T. ) ;
#37068 = VERTEX_POINT ( 'NONE', #28283 ) ;
#37067 = CONTEXT_DEPENDENT_SHAPE_REPRESENTATION ( #25991, #15994 ) ;
#37069 = EDGE_CURVE ( 'NONE', #27061, #40434, #46, .T. ) ;
#37070 = DIRECTION ( 'NONE',  ( 0.000000000000000000, 0.000000000000000000, 1.000000000000000000 ) ) ;
#37072 = ORIENTED_EDGE ( 'NONE', *, *, #69732, .F. ) ;
#37071 = DIRECTION ( 'NONE',  ( 1.000000000000000000, -6.308085367188448025E-15, 0.000000000000000000 ) ) ;
#37073 = AXIS2_PLACEMENT_3D ( 'NONE', #18193, #60973, #28454 ) ;
#37074 = CARTESIAN_POINT ( 'NONE',  ( 11.48848345035334617, -11.08848345035349148, 455.0000000000000568 ) ) ;
#37075 = DIRECTION ( 'NONE',  ( 0.000000000000000000, 0.000000000000000000, 1.000000000000000000 ) ) ;
#37076 = EDGE_LOOP ( 'NONE', ( #27722, #57133, #35255, #52208 ) ) ;
#37077 = ADVANCED_FACE ( 'NONE', ( #16656 ), #65434, .T. ) ;
#37078 = EDGE_LOOP ( 'NONE', ( #28826, #3459, #32437, #18188 ) ) ;
#37079 = CARTESIAN_POINT ( 'NONE',  ( -7.250000000000000888, 8.250000000000001776, -7.500000000000000000 ) ) ;
#37080 = EDGE_CURVE ( 'NONE', #40018, #43115, #43162, .T. ) ;
#37081 = ORIENTED_EDGE ( 'NONE', *, *, #60929, .F. ) ;
#37082 = DIRECTION ( 'NONE',  ( 0.000000000000000000, 0.000000000000000000, 1.000000000000000000 ) ) ;
#37083 = DIRECTION ( 'NONE',  ( -1.000000000000000000, 1.334402673828312846E-16, 0.000000000000000000 ) ) ;
#37084 = PLANE ( 'NONE',  #58844 ) ;
#37085 = VERTEX_POINT ( 'NONE', #27265 ) ;
#37086 = CARTESIAN_POINT ( 'NONE',  ( -2.617976262117251540, 6.486996718459834277, 54.00000000000000711 ) ) ;
#37087 = FACE_OUTER_BOUND ( 'NONE', #54979, .T. ) ;
#37088 = ADVANCED_FACE ( 'NONE', ( #10636 ), #22640, .F. ) ;
#37090 = ORIENTED_EDGE ( 'NONE', *, *, #61191, .T. ) ;
#37089 = DIRECTION ( 'NONE',  ( 0.000000000000000000, 0.000000000000000000, -1.000000000000000000 ) ) ;
#37092 = ORIENTED_EDGE ( 'NONE', *, *, #19130, .F. ) ;
#37091 = CARTESIAN_POINT ( 'NONE',  ( -7.955476262117317177, -8.835729544836295801, 54.00000000000000711 ) ) ;
#37093 = FACE_OUTER_BOUND ( 'NONE', #5425, .T. ) ;
#37094 = CARTESIAN_POINT ( 'NONE',  ( -6.858227778582845602, -3.003254798005714488, 54.00000000000000711 ) ) ;
#37095 = CARTESIAN_POINT ( 'NONE',  ( -11.47551654964667733, 10.19191654964664018, 195.0000000000000284 ) ) ;
#37096 = CARTESIAN_POINT ( 'NONE',  ( 30.00000000000000000, -5.599999999999999645, 27.00000000000000000 ) ) ;
#37097 = CARTESIAN_POINT ( 'NONE',  ( 41.09999999999999432, -14.06939075806900163, 20.80000000000000426 ) ) ;
#37098 = EDGE_CURVE ( 'NONE', #68282, #21718, #47096, .T. ) ;
#37099 = ORIENTED_EDGE ( 'NONE', *, *, #31049, .T. ) ;
#37100 = CARTESIAN_POINT ( 'NONE',  ( -10.19191654964671301, 11.47551654964660450, 455.0000000000000568 ) ) ;
#37101 = DIRECTION ( 'NONE',  ( 0.000000000000000000, -1.000000000000000000, 0.000000000000000000 ) ) ;
#37103 = EDGE_CURVE ( 'NONE', #1387, #19218, #18815, .T. ) ;
#37102 = LINE ( 'NONE', #15873, #43575 ) ;
#37104 = CIRCLE ( 'NONE', #6600, 0.5000000000079367624 ) ;
#37106 = VERTEX_POINT ( 'NONE', #16293 ) ;
#37105 = DIRECTION ( 'NONE',  ( 1.000000000000000000, 0.000000000000000000, 0.000000000000000000 ) ) ;
#37107 = PLANE ( 'NONE',  #42579 ) ;
#37108 = LINE ( 'NONE', #15878, #20191 ) ;
#37109 = DIRECTION ( 'NONE',  ( 1.000000000000000000, -0.000000000000000000, -0.000000000000000000 ) ) ;
#37110 = AXIS2_PLACEMENT_3D ( 'NONE', #57936, #25418, #49347 ) ;
#37111 = LINE ( 'NONE', #4238, #6213 ) ;
#37112 = ORIENTED_EDGE ( 'NONE', *, *, #52189, .F. ) ;
#37113 = LINE ( 'NONE', #20483, #8347 ) ;
#37114 = DIRECTION ( 'NONE',  ( 0.000000000000000000, 1.000000000000000000, 0.000000000000000000 ) ) ;
#37115 = ADVANCED_FACE ( 'NONE', ( #11326 ), #37869, .F. ) ;
#37116 = VERTEX_POINT ( 'NONE', #32574 ) ;
#37117 = CARTESIAN_POINT ( 'NONE',  ( -7.250000000000000888, 7.450000000000003730, -11.50000000000000000 ) ) ;
#37118 = LINE ( 'NONE', #9896, #66089 ) ;
#37119 = CARTESIAN_POINT ( 'NONE',  ( 8.406483450353379183, -6.344579767990935260, 455.0000000000000568 ) ) ;
#37120 = CARTESIAN_POINT ( 'NONE',  ( -6.835476262117334834, -10.50702373788278798, 54.00000000000000711 ) ) ;
#37121 = AXIS2_PLACEMENT_3D ( 'NONE', #33348, #54934, #56299 ) ;
#37122 = DIRECTION ( 'NONE',  ( -1.000000000000000000, 0.000000000000000000, 0.000000000000000000 ) ) ;
#37123 = ORIENTED_EDGE ( 'NONE', *, *, #41959, .F. ) ;
#37124 = ORIENTED_EDGE ( 'NONE', *, *, #27290, .T. ) ;
#37125 = FACE_OUTER_BOUND ( 'NONE', #10679, .T. ) ;
#37126 = EDGE_LOOP ( 'NONE', ( #46220, #21072, #34879, #61989 ) ) ;
#37127 = ORIENTED_EDGE ( 'NONE', *, *, #35355, .T. ) ;
#37128 = PLANE ( 'NONE',  #922 ) ;
#37129 = EDGE_CURVE ( 'NONE', #67310, #1682, #65768, .T. ) ;
#37130 = CARTESIAN_POINT ( 'NONE',  ( -7.450000000000001954, -7.249999999999998224, -22.00000000000000000 ) ) ;
#37131 = DIRECTION ( 'NONE',  ( 0.000000000000000000, -1.000000000000000000, 0.000000000000000000 ) ) ;
#37132 = ORIENTED_EDGE ( 'NONE', *, *, #39393, .F. ) ;
#37133 = ORIENTED_EDGE ( 'NONE', *, *, #23918, .T. ) ;
#37134 = DIRECTION ( 'NONE',  ( 0.7142857142857395036, 0.000000000000000000, 0.6998542122237394469 ) ) ;
#37135 = ORIENTED_EDGE ( 'NONE', *, *, #17891, .F. ) ;
#37136 = EDGE_CURVE ( 'NONE', #41339, #3133, #44191, .T. ) ;
#37137 = EDGE_LOOP ( 'NONE', ( #30865, #62833, #66439, #52019 ) ) ;
#37138 = DIRECTION ( 'NONE',  ( -0.000000000000000000, 1.000000000000000000, 3.673940397442059868E-16 ) ) ;
#37139 = DIRECTION ( 'NONE',  ( 0.000000000000000000, 1.000000000000000000, 0.000000000000000000 ) ) ;
#37140 = DIRECTION ( 'NONE',  ( 0.000000000000000000, 0.000000000000000000, -1.000000000000000000 ) ) ;
#37141 = ORIENTED_EDGE ( 'NONE', *, *, #14654, .T. ) ;
#37142 = EDGE_CURVE ( 'NONE', #47575, #31468, #27860, .T. ) ;
#37143 = CARTESIAN_POINT ( 'NONE',  ( -7.450000000000001954, 0.000000000000000000, -14.50000000000000000 ) ) ;
#37145 = CARTESIAN_POINT ( 'NONE',  ( -8.393516549646722780, -5.668387132715892562, 195.0000000000000284 ) ) ;
#37144 = LINE ( 'NONE', #9569, #46799 ) ;
#37146 = ORIENTED_EDGE ( 'NONE', *, *, #59856, .F. ) ;
#37147 = EDGE_CURVE ( 'NONE', #16300, #25227, #16991, .T. ) ;
#37149 = ORIENTED_EDGE ( 'NONE', *, *, #33297, .T. ) ;
#37148 = DIRECTION ( 'NONE',  ( 0.000000000000000000, 0.000000000000000000, 1.000000000000000000 ) ) ;
#37150 = VERTEX_POINT ( 'NONE', #54825 ) ;
#37151 = CIRCLE ( 'NONE', #57461, 0.5000000000079362072 ) ;
#37152 = EDGE_CURVE ( 'NONE', #14703, #38244, #59082, .T. ) ;
#37153 = DIRECTION ( 'NONE',  ( 0.000000000000000000, 0.000000000000000000, -1.000000000000000000 ) ) ;
#37154 = AXIS2_PLACEMENT_3D ( 'NONE', #52799, #48176, #15652 ) ;
#37155 = CARTESIAN_POINT ( 'NONE',  ( -8.598420958951683346, 1.466476262117183182, 54.00000000000000711 ) ) ;
#37156 = VERTEX_POINT ( 'NONE', #49514 ) ;
#37157 = EDGE_CURVE ( 'NONE', #26529, #56381, #17324, .T. ) ;
#37158 = EDGE_CURVE ( 'NONE', #10775, #21736, #64399, .T. ) ;
#37159 = VECTOR ( 'NONE', #58834, 1000.000000000000000 ) ;
#37160 = DIRECTION ( 'NONE',  ( 1.000000000000000000, 0.000000000000000000, 0.000000000000000000 ) ) ;
#37161 = DIRECTION ( 'NONE',  ( -1.794541526872559352E-16, -1.000000000000000000, 0.000000000000000000 ) ) ;
#37162 = EDGE_CURVE ( 'NONE', #64619, #8221, #14341, .T. ) ;
#37163 = ORIENTED_EDGE ( 'NONE', *, *, #52228, .F. ) ;
#37164 = EDGE_CURVE ( 'NONE', #43746, #33525, #18979, .T. ) ;
#37165 = EDGE_CURVE ( 'NONE', #14678, #58971, #62812, .T. ) ;
#37166 = VERTEX_POINT ( 'NONE', #46539 ) ;
#37167 = CIRCLE ( 'NONE', #6652, 0.5999999999999998668 ) ;
#37168 = CARTESIAN_POINT ( 'NONE',  ( 0.000000000000000000, -7.449999999999998401, -15.50000000000000000 ) ) ;
#37169 = CARTESIAN_POINT ( 'NONE',  ( 283.0000000000000568, -20.50000000000000000, 13.00000000000000178 ) ) ;
#37170 = DIRECTION ( 'NONE',  ( 1.836970198721029934E-16, -1.836970198721036344E-16, 1.000000000000000000 ) ) ;
#37171 = ORIENTED_EDGE ( 'NONE', *, *, #990, .T. ) ;
#37172 = EDGE_CURVE ( 'NONE', #18065, #52249, #40261, .T. ) ;
#37173 = AXIS2_PLACEMENT_3D ( 'NONE', #23588, #8016, #45151 ) ;
#37174 = LINE ( 'NONE', #19486, #61696 ) ;
#37175 = DIRECTION ( 'NONE',  ( 1.000000000000000000, 0.000000000000000000, 0.000000000000000000 ) ) ;
#37177 = VERTEX_POINT ( 'NONE', #8724 ) ;
#37176 = DIRECTION ( 'NONE',  ( 1.000000000000000000, -0.000000000000000000, 0.000000000000000000 ) ) ;
#37179 = ORIENTED_EDGE ( 'NONE', *, *, #16190, .T. ) ;
#37178 = DIRECTION ( 'NONE',  ( 1.000000000000000000, 0.000000000000000000, 0.000000000000000000 ) ) ;
#37180 = LINE ( 'NONE', #10296, #62138 ) ;
#37181 = CIRCLE ( 'NONE', #4423, 0.5000000000001357803 ) ;
#37182 = DIRECTION ( 'NONE',  ( 0.000000000000000000, 1.000000000000000000, 0.000000000000000000 ) ) ;
#37183 = DIRECTION ( 'NONE',  ( 0.000000000000000000, 1.000000000000000000, 8.604228440837611257E-13 ) ) ;
#37184 = DIRECTION ( 'NONE',  ( -0.000000000000000000, 3.673940397442059868E-16, -1.000000000000000000 ) ) ;
#37185 = LINE ( 'NONE', #5362, #31673 ) ;
#37186 = CARTESIAN_POINT ( 'NONE',  ( -9.942044687070527687, -2.765062094115999347, 195.0000000000000284 ) ) ;
#37187 = ADVANCED_FACE ( 'NONE', ( #40538 ), #30296, .T. ) ;
#37188 = ORIENTED_EDGE ( 'NONE', *, *, #36276, .F. ) ;
#37189 = DIRECTION ( 'NONE',  ( -0.4998444328988824181, 0.000000000000000000, 0.8661152018640445593 ) ) ;
#37192 = ORIENTED_EDGE ( 'NONE', *, *, #7332, .T. ) ;
#37191 = EDGE_CURVE ( 'NONE', #11281, #15650, #45846, .T. ) ;
#37190 =( LENGTH_UNIT ( ) NAMED_UNIT ( * ) SI_UNIT ( .MILLI., .METRE. ) );
#37193 = CARTESIAN_POINT ( 'NONE',  ( 275.0000000000000000, -32.95000000000000284, 14.50000000000000000 ) ) ;
#37194 = FACE_OUTER_BOUND ( 'NONE', #23426, .T. ) ;
#37195 = DIRECTION ( 'NONE',  ( 0.7671651518153105309, -0.6414496315691445849, 0.000000000000000000 ) ) ;
#37196 = ORIENTED_EDGE ( 'NONE', *, *, #10090, .F. ) ;
#37197 = CARTESIAN_POINT ( 'NONE',  ( 7.250000000000004441, 7.450000000000001954, -11.00000000000000000 ) ) ;
#37198 = FACE_OUTER_BOUND ( 'NONE', #47246, .T. ) ;
#37199 = ORIENTED_EDGE ( 'NONE', *, *, #46151, .F. ) ;
#37200 = CIRCLE ( 'NONE', #22501, 0.3999999999999993006 ) ;
#37201 = DIRECTION ( 'NONE',  ( -1.000000000000000000, 0.000000000000000000, 0.000000000000000000 ) ) ;
#37202 = CARTESIAN_POINT ( 'NONE',  ( 11.90000000000000036, -14.06939075806900874, 20.80000000000001137 ) ) ;
#37203 = VECTOR ( 'NONE', #64689, 1000.000000000000000 ) ;
#37204 = LINE ( 'NONE', #50131, #64832 ) ;
#37205 = EDGE_LOOP ( 'NONE', ( #65581, #28820, #62938, #26780, #2186 ) ) ;
#37206 = LINE ( 'NONE', #48158, #13518 ) ;
#37207 = VERTEX_POINT ( 'NONE', #46190 ) ;
#37208 = VERTEX_POINT ( 'NONE', #29930 ) ;
#37209 = AXIS2_PLACEMENT_3D ( 'NONE', #57422, #30555, #52122 ) ;
#37210 = LINE ( 'NONE', #9277, #66356 ) ;
#37211 = CARTESIAN_POINT ( 'NONE',  ( -7.250000000000001776, -7.249999999999998224, -19.50000000000000000 ) ) ;
#37212 = AXIS2_PLACEMENT_3D ( 'NONE', #6791, #28365, #42219 ) ;
#37213 = FACE_OUTER_BOUND ( 'NONE', #11315, .T. ) ;
#37214 = LINE ( 'NONE', #59811, #69044 ) ;
#37215 = ORIENTED_EDGE ( 'NONE', *, *, #35054, .F. ) ;
#37216 = ORIENTED_EDGE ( 'NONE', *, *, #55114, .F. ) ;
#37218 = ORIENTED_EDGE ( 'NONE', *, *, #39286, .T. ) ;
#37217 = DIRECTION ( 'NONE',  ( 0.000000000000000000, 1.000000000000000000, 0.000000000000000000 ) ) ;
#37219 = EDGE_LOOP ( 'NONE', ( #17027, #33198 ) ) ;
#37220 = EDGE_CURVE ( 'NONE', #34688, #391, #46893, .T. ) ;
#37221 = DIRECTION ( 'NONE',  ( 1.836970198721029934E-16, 1.836970198721010706E-16, -1.000000000000000000 ) ) ;
#37222 = CARTESIAN_POINT ( 'NONE',  ( -10.49297626211726175, 6.835476262117182955, 54.00000000000000711 ) ) ;
#37223 = DIRECTION ( 'NONE',  ( 0.000000000000000000, -0.7071067811865460184, -0.7071067811865489050 ) ) ;
#37224 = ADVANCED_FACE ( 'NONE', ( #24986 ), #34873, .F. ) ;
#37225 = CYLINDRICAL_SURFACE ( 'NONE', #5162, 0.1999999999999996503 ) ;
#37226 = VECTOR ( 'NONE', #28417, 1000.000000000000000 ) ;
#37228 = CARTESIAN_POINT ( 'NONE',  ( -30.00000000000000000, -11.10796162543699950, -9.102987789146602893 ) ) ;
#37227 = CARTESIAN_POINT ( 'NONE',  ( 39.90000000000000568, 0.000000000000000000, 0.000000000000000000 ) ) ;
#37229 = ORIENTED_EDGE ( 'NONE', *, *, #20268, .T. ) ;
#37230 = ADVANCED_FACE ( 'NONE', ( #9422 ), #13671, .T. ) ;
#37231 = ORIENTED_EDGE ( 'NONE', *, *, #22390, .F. ) ;
#37232 = VERTEX_POINT ( 'NONE', #35219 ) ;
#37233 = ORIENTED_EDGE ( 'NONE', *, *, #4202, .T. ) ;
#37234 = CARTESIAN_POINT ( 'NONE',  ( -7.250000000000000000, -7.449999999999998401, -11.50000000000000000 ) ) ;
#37235 = EDGE_CURVE ( 'NONE', #20433, #66152, #35578, .T. ) ;
#37236 = CARTESIAN_POINT ( 'NONE',  ( -5.242976262117275077, -5.257023737882800418, 26.00000000000000711 ) ) ;
#37237 = DIRECTION ( 'NONE',  ( 0.000000000000000000, 0.000000000000000000, 1.000000000000000000 ) ) ;
#37238 = CARTESIAN_POINT ( 'NONE',  ( 7.357023737882817827, -3.848229544836346605, 54.00000000000000711 ) ) ;
#37239 = VECTOR ( 'NONE', #69685, 1000.000000000000000 ) ;
#37240 = ORIENTED_EDGE ( 'NONE', *, *, #43339, .T. ) ;
#37241 = ORIENTED_EDGE ( 'NONE', *, *, #48482, .T. ) ;
#37242 = ORIENTED_EDGE ( 'NONE', *, *, #67945, .F. ) ;
#37243 = CYLINDRICAL_SURFACE ( 'NONE', #10223, 1.224999999999998757 ) ;
#37244 = ORIENTED_EDGE ( 'NONE', *, *, #34937, .T. ) ;
#37245 = DIRECTION ( 'NONE',  ( -1.047444401652940007E-14, -1.000000000000000000, -1.836970198721029934E-16 ) ) ;
#37246 = CARTESIAN_POINT ( 'NONE',  ( 21.90000000000000213, 20.60000000000000142, -13.86939075806900057 ) ) ;
#37247 = ORIENTED_EDGE ( 'NONE', *, *, #8550, .T. ) ;
#37248 = EDGE_CURVE ( 'NONE', #24345, #6900, #49852, .T. ) ;
#37249 = ORIENTED_EDGE ( 'NONE', *, *, #16604, .F. ) ;
#37250 = CARTESIAN_POINT ( 'NONE',  ( -11.11351654964680336, -9.106483450353373144, 455.0000000000000568 ) ) ;
#37252 = VERTEX_POINT ( 'NONE', #25336 ) ;
#37251 = DIRECTION ( 'NONE',  ( 0.000000000000000000, 1.000000000000000000, -0.000000000000000000 ) ) ;
#37253 = CIRCLE ( 'NONE', #12320, 0.3499999999999611200 ) ;
#37254 = ORIENTED_EDGE ( 'NONE', *, *, #27325, .F. ) ;
#37255 = DIRECTION ( 'NONE',  ( -0.000000000000000000, -0.000000000000000000, 1.000000000000000000 ) ) ;
#37257 = ORIENTED_EDGE ( 'NONE', *, *, #19561, .F. ) ;
#37256 = CARTESIAN_POINT ( 'NONE',  ( 0.000000000000000000, 0.000000000000000000, -3.233000000000000096 ) ) ;
#37258 = ORIENTED_EDGE ( 'NONE', *, *, #3572, .T. ) ;
#37259 = VECTOR ( 'NONE', #34626, 1000.000000000000000 ) ;
#37260 = CARTESIAN_POINT ( 'NONE',  ( -11.07551654964678711, -11.48848345035328933, 195.0000000000000284 ) ) ;
#37261 = DIRECTION ( 'NONE',  ( -1.000000000000000000, 0.000000000000000000, 0.000000000000000000 ) ) ;
#37262 = FACE_OUTER_BOUND ( 'NONE', #57851, .T. ) ;
#37263 = CARTESIAN_POINT ( 'NONE',  ( 13.90000000000000036, -0.000000000000000000, 20.80000000000000426 ) ) ;
#37264 = VECTOR ( 'NONE', #50222, 1000.000000000000000 ) ;
#37265 = DIRECTION ( 'NONE',  ( -1.000000000000000000, 0.000000000000000000, 0.000000000000000000 ) ) ;
#37266 = ADVANCED_FACE ( 'NONE', ( #29575 ), #8355, .F. ) ;
#37267 = EDGE_LOOP ( 'NONE', ( #45039, #20925, #15053, #7200 ) ) ;
#37268 = FACE_BOUND ( 'NONE', #23085, .T. ) ;
#37269 = VECTOR ( 'NONE', #9274, 1000.000000000000000 ) ;
#37271 = ORIENTED_EDGE ( 'NONE', *, *, #11354, .F. ) ;
#37270 = ADVANCED_FACE ( 'NONE', ( #63163 ), #40887, .F. ) ;
#37272 = DIRECTION ( 'NONE',  ( -0.000000000000000000, -0.000000000000000000, -1.000000000000000000 ) ) ;
#37273 = SURFACE_STYLE_FILL_AREA ( #52481 ) ;
#37274 = EDGE_CURVE ( 'NONE', #19077, #62836, #57155, .T. ) ;
#37275 = DIRECTION ( 'NONE',  ( 1.000000000000000000, 0.000000000000000000, 0.000000000000000000 ) ) ;
#37276 = CARTESIAN_POINT ( 'NONE',  ( 4.206483450353341702, -11.32648345035347504, 455.0000000000000568 ) ) ;
#37277 = AXIS2_PLACEMENT_3D ( 'NONE', #45752, #35488, #20289 ) ;
#37278 = CARTESIAN_POINT ( 'NONE',  ( 36.90000000000000568, -0.1999999999911430404, -8.864436962241481021E-12 ) ) ;
#37279 = EDGE_LOOP ( 'NONE', ( #41979, #25406, #29386, #39616 ) ) ;
#37280 = DIRECTION ( 'NONE',  ( 0.000000000000000000, 0.000000000000000000, -1.000000000000000000 ) ) ;
#37281 =( NAMED_UNIT ( * ) PLANE_ANGLE_UNIT ( ) SI_UNIT ( $, .RADIAN. ) );
#37282 = EDGE_LOOP ( 'NONE', ( #1423, #60426, #3904, #15578, #23710 ) ) ;
#37283 = VECTOR ( 'NONE', #5503, 1000.000000000000000 ) ;
#37284 = FACE_OUTER_BOUND ( 'NONE', #62690, .T. ) ;
#37285 = CARTESIAN_POINT ( 'NONE',  ( 1.690483450353351458, -9.841277389592800517, 455.0000000000000568 ) ) ;
#37286 = DIRECTION ( 'NONE',  ( 0.000000000000000000, 1.000000000000000000, 0.000000000000000000 ) ) ;
#37287 = DIRECTION ( 'NONE',  ( 1.836970198721029934E-16, 1.836970198721010706E-16, -1.000000000000000000 ) ) ;
#37288 = DIRECTION ( 'NONE',  ( 1.000000000000000000, 0.000000000000000000, 0.000000000000000000 ) ) ;
#37289 = ORIENTED_EDGE ( 'NONE', *, *, #48084, .F. ) ;
#37290 = PLANE ( 'NONE',  #7326 ) ;
#37291 = DIRECTION ( 'NONE',  ( -1.000000000000000000, 7.751221965937476285E-17, 0.000000000000000000 ) ) ;
#37292 = CARTESIAN_POINT ( 'NONE',  ( 111.9257688011037146, 10.00000000000000000, 335.4830310981152479 ) ) ;
#37293 = LINE ( 'NONE', #4075, #69308 ) ;
#37294 = CARTESIAN_POINT ( 'NONE',  ( -8.821682069070780230, 2.355476262117184305, 26.00000000000000711 ) ) ;
#37295 = ORIENTED_EDGE ( 'NONE', *, *, #65957, .F. ) ;
#37296 = CIRCLE ( 'NONE', #41768, 1.000000000000000888 ) ;
#37298 = ORIENTED_EDGE ( 'NONE', *, *, #52172, .F. ) ;
#37297 = CARTESIAN_POINT ( 'NONE',  ( -7.250000000000000888, -8.249999999999998224, -26.00000000000001066 ) ) ;
#37299 = EDGE_CURVE ( 'NONE', #32112, #16139, #43760, .T. ) ;
#37300 = AXIS2_PLACEMENT_3D ( 'NONE', #58152, #63460, #9722 ) ;
#37301 = DIRECTION ( 'NONE',  ( -0.000000000000000000, 3.673940397442059868E-16, -1.000000000000000000 ) ) ;
#37302 = DIRECTION ( 'NONE',  ( -0.8660254037844510311, -0.4999999999999785727, 0.000000000000000000 ) ) ;
#37303 = LINE ( 'NONE', #27385, #69197 ) ;
#37304 = ORIENTED_EDGE ( 'NONE', *, *, #56465, .T. ) ;
#37305 = VECTOR ( 'NONE', #59002, 1000.000000000000000 ) ;
#37306 = DIRECTION ( 'NONE',  ( 0.000000000000000000, 1.000000000000000000, 0.000000000000000000 ) ) ;
#37307 = DIRECTION ( 'NONE',  ( 0.000000000000000000, 0.000000000000000000, -1.000000000000000000 ) ) ;
#37308 = EDGE_CURVE ( 'NONE', #17145, #67710, #38126, .T. ) ;
#37309 = ORIENTED_EDGE ( 'NONE', *, *, #7271, .F. ) ;
#37310 = ORIENTED_EDGE ( 'NONE', *, *, #59524, .T. ) ;
#37311 = EDGE_CURVE ( 'NONE', #59150, #10667, #51637, .T. ) ;
#37312 = CIRCLE ( 'NONE', #44046, 1.449999999999999956 ) ;
#37313 = ORIENTED_EDGE ( 'NONE', *, *, #49079, .F. ) ;
#37314 = EDGE_CURVE ( 'NONE', #44206, #37330, #69170, .T. ) ;
#37315 = EDGE_CURVE ( 'NONE', #43050, #12421, #58914, .T. ) ;
#37316 = CIRCLE ( 'NONE', #3381, 0.7499999999999997780 ) ;
#37317 = CYLINDRICAL_SURFACE ( 'NONE', #19618, 1.000000000000000000 ) ;
#37318 = VECTOR ( 'NONE', #44559, 1000.000000000000114 ) ;
#37319 = CARTESIAN_POINT ( 'NONE',  ( 7.250000000000005329, 7.250000000000000888, -23.00000000000000000 ) ) ;
#37320 = CARTESIAN_POINT ( 'NONE',  ( 0.000000000000000000, -20.50000000000002487, -17.79289321881347163 ) ) ;
#37321 = EDGE_CURVE ( 'NONE', #33225, #61431, #52568, .T. ) ;
#37322 = ORIENTED_EDGE ( 'NONE', *, *, #63032, .T. ) ;
#37323 = EDGE_LOOP ( 'NONE', ( #57195, #5238, #16449, #49392, #38657, #34799, #4597, #10937 ) ) ;
#37325 = DIRECTION ( 'NONE',  ( -0.9375000000000004441, 0.000000000000000000, 0.3479852726768752902 ) ) ;
#37324 = VECTOR ( 'NONE', #57599, 1000.000000000000000 ) ;
#37326 = AXIS2_PLACEMENT_3D ( 'NONE', #24614, #56425, #2338 ) ;
#37327 = ORIENTED_EDGE ( 'NONE', *, *, #42837, .F. ) ;
#37328 = ORIENTED_EDGE ( 'NONE', *, *, #10872, .T. ) ;
#37329 = ORIENTED_EDGE ( 'NONE', *, *, #43353, .T. ) ;
#37330 = VERTEX_POINT ( 'NONE', #16477 ) ;
#37331 = DIRECTION ( 'NONE',  ( 0.000000000000000000, 0.000000000000000000, -1.000000000000000000 ) ) ;
#37332 = UNCERTAINTY_MEASURE_WITH_UNIT (LENGTH_MEASURE( 1.000000000000000082E-05 ), #67173, 'distance_accuracy_value', 'NONE');
#37334 = ORIENTED_EDGE ( 'NONE', *, *, #68431, .F. ) ;
#37333 = LINE ( 'NONE', #32026, #2856 ) ;
#37335 = CARTESIAN_POINT ( 'NONE',  ( -7.342976262117253405, -3.848229544836288429, 54.00000000000000711 ) ) ;
#37336 = DIRECTION ( 'NONE',  ( -1.000000000000000000, -0.000000000000000000, -0.000000000000000000 ) ) ;
#37337 = AXIS2_PLACEMENT_3D ( 'NONE', #48196, #28600, #5055 ) ;
#37338 = DIRECTION ( 'NONE',  ( 1.000000000000000000, 0.000000000000000000, 0.000000000000000000 ) ) ;
#37339 = ORIENTED_EDGE ( 'NONE', *, *, #25741, .T. ) ;
#37340 = CARTESIAN_POINT ( 'NONE',  ( -8.821682069070780230, 2.530476262117183683, 26.00000000000000711 ) ) ;
#37341 = DIRECTION ( 'NONE',  ( 3.491481338843132961E-15, 1.000000000000000000, 1.836970198721029934E-16 ) ) ;
#37342 = AXIS2_PLACEMENT_3D ( 'NONE', #55578, #28694, #50269 ) ;
#37343 = VERTEX_POINT ( 'NONE', #63527 ) ;
#37344 = EDGE_CURVE ( 'NONE', #11005, #48516, #30988, .T. ) ;
#37345 = VECTOR ( 'NONE', #62270, 1000.000000000000000 ) ;
#37346 = CARTESIAN_POINT ( 'NONE',  ( 12.00648345035340903, 7.813516549646560172, 455.0000000000000568 ) ) ;
#37347 = DIRECTION ( 'NONE',  ( 0.7071067811865451302, -0.7071067811865500152, -2.597868168706484048E-16 ) ) ;
#37348 = ORIENTED_EDGE ( 'NONE', *, *, #13042, .T. ) ;
#37349 = EDGE_CURVE ( 'NONE', #54143, #28681, #31320, .T. ) ;
#37350 = CARTESIAN_POINT ( 'NONE',  ( 7.250000000000005329, 8.250000000000001776, -26.00000000000001066 ) ) ;
#37351 = LINE ( 'NONE', #32396, #32468 ) ;
#37352 = EDGE_CURVE ( 'NONE', #59223, #19699, #31365, .T. ) ;
#37353 = FACE_OUTER_BOUND ( 'NONE', #54513, .T. ) ;
#37354 = DIRECTION ( 'NONE',  ( 0.000000000000000000, -0.9938079899998859545, 0.1111111111112941946 ) ) ;
#37355 = EDGE_CURVE ( 'NONE', #54387, #50275, #63871, .T. ) ;
#37356 = VECTOR ( 'NONE', #17877, 1000.000000000000000 ) ;
#37357 = CARTESIAN_POINT ( 'NONE',  ( -8.130476262117324993, -9.562023737882769936, 54.00000000000000711 ) ) ;
#37358 = ORIENTED_EDGE ( 'NONE', *, *, #2709, .F. ) ;
#37359 = DIRECTION ( 'NONE',  ( -1.000000000000000000, 0.000000000000000000, 0.000000000000000000 ) ) ;
#37360 = DIRECTION ( 'NONE',  ( -0.000000000000000000, -0.000000000000000000, -1.000000000000000000 ) ) ;
#37361 = DIRECTION ( 'NONE',  ( 1.000000000000000000, -2.990116172375847553E-15, -1.836970198721035357E-16 ) ) ;
#37362 = VECTOR ( 'NONE', #67709, 1000.000000000000000 ) ;
#37363 = DIRECTION ( 'NONE',  ( 1.000000000000000000, 0.000000000000000000, 0.000000000000000000 ) ) ;
#37364 = ORIENTED_EDGE ( 'NONE', *, *, #20942, .F. ) ;
#37365 = DIRECTION ( 'NONE',  ( -4.956352788505168198E-15, -1.000000000000000000, 0.000000000000000000 ) ) ;
#37366 = CARTESIAN_POINT ( 'NONE',  ( 41.09999999999999432, -21.00000000000000000, -13.86939075806900057 ) ) ;
#37367 = CIRCLE ( 'NONE', #46381, 24.99999999998784972 ) ;
#37368 = CARTESIAN_POINT ( 'NONE',  ( -17.51999999999999957, -15.50000000000000000, -26.00000000000000355 ) ) ;
#37369 = FACE_OUTER_BOUND ( 'NONE', #12391, .T. ) ;
#37370 = ORIENTED_EDGE ( 'NONE', *, *, #1445, .F. ) ;
#37371 = DIRECTION ( 'NONE',  ( -1.000000000000000000, 0.000000000000000000, 0.000000000000000000 ) ) ;
#37372 = CARTESIAN_POINT ( 'NONE',  ( 283.0000000000000568, -39.79999999999954952, 8.900000000000419575 ) ) ;
#37373 = DIRECTION ( 'NONE',  ( -2.135044278125299371E-15, 1.000000000000000000, -0.000000000000000000 ) ) ;
#37374 = DIRECTION ( 'NONE',  ( -1.000000000000000000, 0.000000000000000000, 0.000000000000000000 ) ) ;
#37375 =( NAMED_UNIT ( * ) PLANE_ANGLE_UNIT ( ) SI_UNIT ( $, .RADIAN. ) );
#37376 = DIRECTION ( 'NONE',  ( 0.000000000000000000, 0.000000000000000000, 1.000000000000000000 ) ) ;
#37377 = ORIENTED_EDGE ( 'NONE', *, *, #45644, .T. ) ;
#37378 = ORIENTED_EDGE ( 'NONE', *, *, #49912, .F. ) ;
#37379 = LINE ( 'NONE', #42321, #30418 ) ;
#37380 = AXIS2_PLACEMENT_3D ( 'NONE', #42710, #37761, #31425 ) ;
#37381 = CARTESIAN_POINT ( 'NONE',  ( -5.242976262117259978, 5.242976262117182706, 26.00000000000000711 ) ) ;
#37382 = ORIENTED_EDGE ( 'NONE', *, *, #17282, .F. ) ;
#37383 = DIRECTION ( 'NONE',  ( 0.000000000000000000, 0.9760787414516886029, 0.2174173187353931058 ) ) ;
#37384 = CARTESIAN_POINT ( 'NONE',  ( -29.50000000000000355, -11.50000000000100009, -10.50000000000065903 ) ) ;
#37385 = VERTEX_POINT ( 'NONE', #15433 ) ;
#37386 = CARTESIAN_POINT ( 'NONE',  ( -3.593516549646712299, 4.609516549646604844, 195.0000000000000284 ) ) ;
#37387 = EDGE_LOOP ( 'NONE', ( #22524, #39531, #628, #34425 ) ) ;
#37388 = ORIENTED_EDGE ( 'NONE', *, *, #29459, .F. ) ;
#37389 = DIRECTION ( 'NONE',  ( -1.000000000000000000, 0.000000000000000000, 0.000000000000000000 ) ) ;
#37390 = EDGE_CURVE ( 'NONE', #25369, #7124, #20033, .T. ) ;
#37391 = AXIS2_PLACEMENT_3D ( 'NONE', #44349, #60628, #17843 ) ;
#37392 = EDGE_LOOP ( 'NONE', ( #53663, #58726, #9289, #30770 ) ) ;
#37393 = DIRECTION ( 'NONE',  ( -1.000000000000000000, 0.000000000000000000, 0.000000000000000000 ) ) ;
#37394 = CARTESIAN_POINT ( 'NONE',  ( -6.817976262117322328, -9.912023737882780239, 26.00000000000000000 ) ) ;
#37395 = CARTESIAN_POINT ( 'NONE',  ( -5.993516549646711766, 5.993516549646603409, 195.0000000000000284 ) ) ;
#37396 = PRESENTATION_LAYER_ASSIGNMENT (  '', '', ( #10287 ) ) ;
#37397 = ADVANCED_FACE ( 'NONE', ( #53965 ), #47602, .T. ) ;
#37398 = ADVANCED_FACE ( 'NONE', ( #48650 ), #21776, .F. ) ;
#37399 = ORIENTED_EDGE ( 'NONE', *, *, #58860, .T. ) ;
#37400 = VERTEX_POINT ( 'NONE', #31704 ) ;
#37401 = VECTOR ( 'NONE', #21531, 1000.000000000000000 ) ;
#37402 = FACE_OUTER_BOUND ( 'NONE', #28680, .T. ) ;
#37404 = LINE ( 'NONE', #31044, #24321 ) ;
#37403 = CARTESIAN_POINT ( 'NONE',  ( 11.78648345035337819, -7.606483450353493936, 455.0000000000000568 ) ) ;
#37405 = ORIENTED_EDGE ( 'NONE', *, *, #1447, .T. ) ;
#37406 = ORIENTED_EDGE ( 'NONE', *, *, #41654, .F. ) ;
#37407 = CIRCLE ( 'NONE', #15955, 1.399999999999998579 ) ;
#37408 = AXIS2_PLACEMENT_3D ( 'NONE', #52526, #19288, #35538 ) ;
#37410 = EDGE_LOOP ( 'NONE', ( #29371, #46245, #2240, #29295 ) ) ;
#37409 = PRODUCT_CONTEXT ( 'NONE', #52631, 'mechanical' ) ;
#37411 = DIRECTION ( 'NONE',  ( -1.000000000000000000, 0.000000000000000000, 0.000000000000000000 ) ) ;
#37412 = EDGE_CURVE ( 'NONE', #51741, #22546, #43332, .T. ) ;
#37414 = ORIENTED_EDGE ( 'NONE', *, *, #41599, .F. ) ;
#37413 = LINE ( 'NONE', #58628, #10529 ) ;
#37415 = AXIS2_PLACEMENT_3D ( 'NONE', #15296, #36502, #62316 ) ;
#37416 = DIRECTION ( 'NONE',  ( -1.000000000000000000, 0.000000000000000000, 0.000000000000000000 ) ) ;
#37417 = AXIS2_PLACEMENT_3D ( 'NONE', #45224, #51235, #57246 ) ;
#37418 = DIRECTION ( 'NONE',  ( 0.000000000000000000, 0.000000000000000000, 1.000000000000000000 ) ) ;
#37419 = VERTEX_POINT ( 'NONE', #26388 ) ;
#37420 = EDGE_LOOP ( 'NONE', ( #1130, #55219, #43497, #57988 ) ) ;
#37421 = AXIS2_PLACEMENT_3D ( 'NONE', #20997, #5456, #32657 ) ;
#37422 = CARTESIAN_POINT ( 'NONE',  ( 7.000000000000000000, -38.65000000000095781, 14.49999999999903899 ) ) ;
#37423 = ORIENTED_EDGE ( 'NONE', *, *, #21992, .F. ) ;
#37424 = CARTESIAN_POINT ( 'NONE',  ( 15.00000000000000000, -26.42999999999999972, -9.412893218813501051 ) ) ;
#37425 = CARTESIAN_POINT ( 'NONE',  ( -11.00000000000000000, -5.200000000000001066, -26.59999999999999787 ) ) ;
#37426 = CARTESIAN_POINT ( 'NONE',  ( 10.31452373788281562, -6.849523737882823760, 54.00000000000000711 ) ) ;
#37427 = ORIENTED_EDGE ( 'NONE', *, *, #580, .T. ) ;
#37428 = FACE_OUTER_BOUND ( 'NONE', #40150, .T. ) ;
#37429 = CARTESIAN_POINT ( 'NONE',  ( 7.250000000000004441, 7.450000000000001954, -23.50000000000000000 ) ) ;
#37430 = AXIS2_PLACEMENT_3D ( 'NONE', #36621, #26725, #41928 ) ;
#37432 = VERTEX_POINT ( 'NONE', #9783 ) ;
#37431 = CARTESIAN_POINT ( 'NONE',  ( 2.906483450353420928, 11.11351654964658842, 455.0000000000000568 ) ) ;
#37433 = VERTEX_POINT ( 'NONE', #41948 ) ;
#37434 = DIRECTION ( 'NONE',  ( 0.7071067811865401342, -0.7071067811865550112, -1.355854680848614216E-30 ) ) ;
#37435 = DIRECTION ( 'NONE',  ( -2.891205793294683355E-15, -1.000000000000000000, 0.000000000000000000 ) ) ;
#37436 = DIRECTION ( 'NONE',  ( -0.000000000000000000, -0.000000000000000000, -1.000000000000000000 ) ) ;
#37437 = DIRECTION ( 'NONE',  ( 0.000000000000000000, -1.000000000000000000, 0.000000000000000000 ) ) ;
#37438 = EDGE_CURVE ( 'NONE', #58190, #33133, #5520, .T. ) ;
#37439 = CARTESIAN_POINT ( 'NONE',  ( 11.32648345035337911, 4.193516549646524538, 455.0000000000000568 ) ) ;
#37440 = VERTEX_POINT ( 'NONE', #59257 ) ;
#37441 = DIRECTION ( 'NONE',  ( -0.000000000000000000, 0.000000000000000000, -1.000000000000000000 ) ) ;
#37442 = DIRECTION ( 'NONE',  ( 0.000000000000000000, -3.673940397442059868E-16, 1.000000000000000000 ) ) ;
#37443 = VECTOR ( 'NONE', #52473, 1000.000000000000000 ) ;
#37444 =( NAMED_UNIT ( * ) PLANE_ANGLE_UNIT ( ) SI_UNIT ( $, .RADIAN. ) );
#37446 = EDGE_LOOP ( 'NONE', ( #52051, #53560, #44157, #38179 ) ) ;
#37445 = DIRECTION ( 'NONE',  ( 0.000000000000000000, 0.000000000000000000, 1.000000000000000000 ) ) ;
#37447 = PRODUCT ( 'HOLDING PLATE', 'HOLDING PLATE', '', ( #25763 ) ) ;
#37448 = AXIS2_PLACEMENT_3D ( 'NONE', #55159, #7391, #6703 ) ;
#37449 = PLANE ( 'NONE',  #24559 ) ;
#37450 = CARTESIAN_POINT ( 'NONE',  ( 7.000000000000000000, -39.79999999999905214, 12.19999999999906315 ) ) ;
#37451 = CARTESIAN_POINT ( 'NONE',  ( -8.750000000000003553, 7.750000000000001776, 0.000000000000000000 ) ) ;
#37452 = EDGE_CURVE ( 'NONE', #61368, #51358, #21158, .T. ) ;
#37453 = DIRECTION ( 'NONE',  ( -1.000000000000000000, 0.000000000000000000, 0.000000000000000000 ) ) ;
#37454 = EDGE_LOOP ( 'NONE', ( #51707, #42423, #55146, #48571 ) ) ;
#37455 = LINE ( 'NONE', #59362, #45601 ) ;
#37456 = DIRECTION ( 'NONE',  ( 0.000000000000000000, -0.7071067811828075644, 0.7071067811902875810 ) ) ;
#37457 = EDGE_LOOP ( 'NONE', ( #58355, #32972, #23891, #52890 ) ) ;
#37458 = DIRECTION ( 'NONE',  ( 1.000000000000000000, 0.000000000000000000, 0.000000000000000000 ) ) ;
#37459 = VECTOR ( 'NONE', #37559, 1000.000000000000000 ) ;
#37460 = CLOSED_SHELL ( 'NONE', ( #11585, #30836, #44700, #60281, #55413, #25649 ) ) ;
#37461 = LINE ( 'NONE', #54418, #3025 ) ;
#37462 = CARTESIAN_POINT ( 'NONE',  ( 9.562023737882812569, -2.369523737882815784, 26.00000000000000711 ) ) ;
#37463 = EDGE_CURVE ( 'NONE', #57937, #7800, #10465, .T. ) ;
#37464 = PLANE ( 'NONE',  #50799 ) ;
#37465 = DIRECTION ( 'NONE',  ( -0.000000000000000000, 0.000000000000000000, -1.000000000000000000 ) ) ;
#37466 = VERTEX_POINT ( 'NONE', #15776 ) ;
#37467 = ORIENTED_EDGE ( 'NONE', *, *, #38294, .F. ) ;
#37468 = CARTESIAN_POINT ( 'NONE',  ( -6.822336235477446387, 6.350872789121265072, 54.00000000000000711 ) ) ;
#37469 = ORIENTED_EDGE ( 'NONE', *, *, #61058, .T. ) ;
#37470 = ORIENTED_EDGE ( 'NONE', *, *, #31819, .T. ) ;
#37471 = CARTESIAN_POINT ( 'NONE',  ( -9.942044687070573872, -2.765062094116046865, 455.0000000000000568 ) ) ;
#37472 = CIRCLE ( 'NONE', #25043, 0.1999999999999992339 ) ;
#37473 = CARTESIAN_POINT ( 'NONE',  ( 283.0000000000000568, -32.95000000000000284, 13.19999999999999929 ) ) ;
#37474 = CARTESIAN_POINT ( 'NONE',  ( 15.50000000000000000, -0.1999999999999999556, -22.50000000000000000 ) ) ;
#37475 = ORIENTED_EDGE ( 'NONE', *, *, #34400, .T. ) ;
#37476 = ORIENTED_EDGE ( 'NONE', *, *, #8366, .T. ) ;
#37477 = CARTESIAN_POINT ( 'NONE',  ( -7.250000000000001776, -7.249999999999998224, -26.00000000000001066 ) ) ;
#37478 = ORIENTED_EDGE ( 'NONE', *, *, #7030, .F. ) ;
#37479 = ORIENTED_EDGE ( 'NONE', *, *, #10270, .T. ) ;
#37480 = EDGE_CURVE ( 'NONE', #55046, #65427, #37351, .T. ) ;
#37481 = DIRECTION ( 'NONE',  ( 1.047444401652939849E-14, 1.000000000000000000, 1.836970198721029934E-16 ) ) ;
#37482 = CARTESIAN_POINT ( 'NONE',  ( 10.00000000000000000, 18.00000000000000355, -21.00000000000000000 ) ) ;
#37483 = DIRECTION ( 'NONE',  ( 1.000000000000000000, -0.000000000000000000, 0.000000000000000000 ) ) ;
#37484 = AXIS2_PLACEMENT_3D ( 'NONE', #7909, #34421, #56015 ) ;
#37485 = ADVANCED_FACE ( 'NONE', ( #64568 ), #53615, .F. ) ;
#37486 = EDGE_CURVE ( 'NONE', #49938, #64845, #43693, .T. ) ;
#37487 = ORIENTED_EDGE ( 'NONE', *, *, #48386, .T. ) ;
#37488 = CARTESIAN_POINT ( 'NONE',  ( -7.250000000000000888, 7.450000000000003730, -10.00000000000000000 ) ) ;
#37490 = CARTESIAN_POINT ( 'NONE',  ( -7.250000000000000888, 8.250000000000001776, -23.00000000000000000 ) ) ;
#37489 = CARTESIAN_POINT ( 'NONE',  ( 10.20488345035340849, 11.47551654964657786, 195.0000000000000284 ) ) ;
#37491 = VERTEX_POINT ( 'NONE', #22126 ) ;
#37494 = ORIENTED_EDGE ( 'NONE', *, *, #44886, .T. ) ;
#37493 = EDGE_CURVE ( 'NONE', #12012, #37614, #34100, .T. ) ;
#37492 = CARTESIAN_POINT ( 'NONE',  ( -17.00000000000000000, -15.50000000000000000, 19.33772233983200195 ) ) ;
#37495 = VERTEX_POINT ( 'NONE', #6207 ) ;
#37496 = ADVANCED_FACE ( 'NONE', ( #45061 ), #11839, .F. ) ;
#37497 = EDGE_CURVE ( 'NONE', #30184, #43815, #11494, .T. ) ;
#37498 = FACE_OUTER_BOUND ( 'NONE', #55476, .T. ) ;
#37499 = EDGE_CURVE ( 'NONE', #18067, #9829, #33429, .T. ) ;
#37500 = CARTESIAN_POINT ( 'NONE',  ( -9.689999999999999503, -9.750000000000001776, -4.250000000000000000 ) ) ;
#37501 = ORIENTED_EDGE ( 'NONE', *, *, #26485, .T. ) ;
#37502 = DIRECTION ( 'NONE',  ( 0.000000000000000000, 0.000000000000000000, -1.000000000000000000 ) ) ;
#37503 = DIRECTION ( 'NONE',  ( 0.000000000000000000, 0.000000000000000000, -1.000000000000000000 ) ) ;
#37504 = ORIENTED_EDGE ( 'NONE', *, *, #41521, .F. ) ;
#37505 = VECTOR ( 'NONE', #14342, 1000.000000000000000 ) ;
#37506 = VECTOR ( 'NONE', #60059, 1000.000000000000000 ) ;
#37507 = ORIENTED_EDGE ( 'NONE', *, *, #31773, .F. ) ;
#37508 = DIRECTION ( 'NONE',  ( -1.000000000000000000, 0.000000000000000000, 0.000000000000000000 ) ) ;
#37509 = DIRECTION ( 'NONE',  ( -1.836970198721029934E-16, 1.836970198721036344E-16, -1.000000000000000000 ) ) ;
#37510 = DIRECTION ( 'NONE',  ( 2.135044278125299371E-15, -1.000000000000000000, 0.000000000000000000 ) ) ;
#37511 = ORIENTED_EDGE ( 'NONE', *, *, #28926, .T. ) ;
#37512 = VECTOR ( 'NONE', #41636, 1000.000000000000000 ) ;
#37513 = PLANE ( 'NONE',  #24466 ) ;
#37514 = EDGE_CURVE ( 'NONE', #3076, #30690, #49353, .T. ) ;
#37515 = CYLINDRICAL_SURFACE ( 'NONE', #26092, 4.500000000000189182 ) ;
#37517 = ORIENTED_EDGE ( 'NONE', *, *, #39218, .T. ) ;
#37516 = CARTESIAN_POINT ( 'NONE',  ( 39.00000000000000000, 0.000000000000000000, 0.000000000000000000 ) ) ;
#37519 = ORIENTED_EDGE ( 'NONE', *, *, #13480, .F. ) ;
#37518 = DIRECTION ( 'NONE',  ( -0.000000000000000000, -0.000000000000000000, -1.000000000000000000 ) ) ;
#37521 = DIRECTION ( 'NONE',  ( 0.000000000000000000, 0.000000000000000000, 1.000000000000000000 ) ) ;
#37520 = VECTOR ( 'NONE', #45152, 1000.000000000000000 ) ;
#37522 = CARTESIAN_POINT ( 'NONE',  ( 7.250000000000005329, -8.249999999999998224, -24.50000000000000000 ) ) ;
#37523 = CARTESIAN_POINT ( 'NONE',  ( -24.00000000000000000, -17.50000000000000000, 15.70499999999969809 ) ) ;
#37524 = DIRECTION ( 'NONE',  ( 0.000000000000000000, 1.000000000000000000, 0.000000000000000000 ) ) ;
#37525 = EDGE_CURVE ( 'NONE', #48981, #48595, #12190, .T. ) ;
#37526 = CARTESIAN_POINT ( 'NONE',  ( 10.50000000000000178, 9.690000000000001279, -4.250000000000000000 ) ) ;
#37527 = DIRECTION ( 'NONE',  ( -1.000000000000000000, 0.000000000000000000, 0.000000000000000000 ) ) ;
#37528 = EDGE_LOOP ( 'NONE', ( #56777, #47064, #29549, #40259 ) ) ;
#37529 = CARTESIAN_POINT ( 'NONE',  ( 10.50702373788281818, -9.795823737882813020, 54.00000000000000711 ) ) ;
#37530 = EDGE_CURVE ( 'NONE', #29693, #63246, #12534, .T. ) ;
#37532 = VERTEX_POINT ( 'NONE', #11157 ) ;
#37531 = LINE ( 'NONE', #32580, #67237 ) ;
#37534 = ORIENTED_EDGE ( 'NONE', *, *, #31211, .T. ) ;
#37533 = LINE ( 'NONE', #32223, #63801 ) ;
#37535 = CARTESIAN_POINT ( 'NONE',  ( -24.00000000000000000, -17.35230188589299871, 15.35019951917099945 ) ) ;
#37536 = CARTESIAN_POINT ( 'NONE',  ( 1.480523737882788238, -9.404523737882794165, 54.00000000000000711 ) ) ;
#37537 = ORIENTED_EDGE ( 'NONE', *, *, #19407, .T. ) ;
#37538 = DIRECTION ( 'NONE',  ( -1.000000000000000000, 0.000000000000000000, 0.000000000000000000 ) ) ;
#37539 = CARTESIAN_POINT ( 'NONE',  ( -7.250000000000000888, -8.249999999999998224, -26.00000000000001066 ) ) ;
#37540 = ORIENTED_EDGE ( 'NONE', *, *, #987, .F. ) ;
#37541 = DIRECTION ( 'NONE',  ( -1.000000000000000000, 0.000000000000000000, 0.000000000000000000 ) ) ;
#37542 = CARTESIAN_POINT ( 'NONE',  ( 0.000000000000000000, 0.000000000000000000, -10.00000000000000000 ) ) ;
#37543 = CARTESIAN_POINT ( 'NONE',  ( -11.00000000000000000, -12.00000000000000000, -11.03137303340310282 ) ) ;
#37544 = EDGE_CURVE ( 'NONE', #21483, #47295, #8725, .T. ) ;
#37545 = VECTOR ( 'NONE', #24724, 1000.000000000000114 ) ;
#37546 = ORIENTED_EDGE ( 'NONE', *, *, #34055, .F. ) ;
#37547 = CARTESIAN_POINT ( 'NONE',  ( -7.250000000000000888, 7.250000000000001776, -26.00000000000001066 ) ) ;
#37548 = VERTEX_POINT ( 'NONE', #926 ) ;
#37549 = EDGE_CURVE ( 'NONE', #14678, #17991, #17156, .T. ) ;
#37550 = ORIENTED_EDGE ( 'NONE', *, *, #2890, .T. ) ;
#37551 = AXIS2_PLACEMENT_3D ( 'NONE', #42086, #69311, #52008 ) ;
#37552 = EDGE_CURVE ( 'NONE', #26707, #15366, #38388, .T. ) ;
#37553 = CARTESIAN_POINT ( 'NONE',  ( -28.00000000000000000, -17.35230188589299871, 15.35019951917099945 ) ) ;
#37554 = DIRECTION ( 'NONE',  ( 1.034072152899299800E-14, 1.000000000000000000, 0.000000000000000000 ) ) ;
#37555 = EDGE_CURVE ( 'NONE', #57481, #67199, #28451, .T. ) ;
#37556 = ADVANCED_FACE ( 'NONE', ( #28121 ), #49684, .F. ) ;
#37557 = ADVANCED_FACE ( 'NONE', ( #50375 ), #32726, .T. ) ;
#37558 = CARTESIAN_POINT ( 'NONE',  ( 32.89999999999999858, -14.06939075806900874, 20.80000000000001137 ) ) ;
#37559 = DIRECTION ( 'NONE',  ( -1.000000000000000000, 0.000000000000000000, 0.000000000000000000 ) ) ;
#37560 = ORIENTED_EDGE ( 'NONE', *, *, #55165, .T. ) ;
#37561 = ORIENTED_EDGE ( 'NONE', *, *, #20103, .F. ) ;
#37563 = ORIENTED_EDGE ( 'NONE', *, *, #10739, .F. ) ;
#37562 = CARTESIAN_POINT ( 'NONE',  ( -6.817976262117327657, -9.912023737882785568, 54.00000000000000711 ) ) ;
#37564 = EDGE_CURVE ( 'NONE', #42141, #56866, #53924, .T. ) ;
#37565 = ORIENTED_EDGE ( 'NONE', *, *, #54771, .F. ) ;
#37566 = CARTESIAN_POINT ( 'NONE',  ( 7.450000000000004619, -1.336933437520057563E-15, -7.500000000000000000 ) ) ;
#37567 = CIRCLE ( 'NONE', #28497, 0.5250000000000003553 ) ;
#37568 = DIRECTION ( 'NONE',  ( 1.000000000000000000, -0.000000000000000000, 0.000000000000000000 ) ) ;
#37569 = ADVANCED_FACE ( 'NONE', ( #17501 ), #39072, .F. ) ;
#37570 = CARTESIAN_POINT ( 'NONE',  ( -29.50000000000000355, -11.50000000000100009, -19.50000000000103739 ) ) ;
#37571 = ADVANCED_FACE ( 'NONE', ( #23506 ), #66635, .F. ) ;
#37572 = VECTOR ( 'NONE', #57957, 1000.000000000000000 ) ;
#37573 = LINE ( 'NONE', #19901, #22066 ) ;
#37575 = DIRECTION ( 'NONE',  ( -0.7071067811865514585, -0.7071067811865435759, -2.597868168706465806E-16 ) ) ;
#37574 = FACE_OUTER_BOUND ( 'NONE', #10999, .T. ) ;
#37576 = CIRCLE ( 'NONE', #25141, 1.000000000000000888 ) ;
#37577 = VERTEX_POINT ( 'NONE', #40463 ) ;
#37579 = ORIENTED_EDGE ( 'NONE', *, *, #38098, .F. ) ;
#37578 = CARTESIAN_POINT ( 'NONE',  ( -11.75000000000000000, -5.000000000000000000, 26.25000000000000000 ) ) ;
#37580 = ORIENTED_EDGE ( 'NONE', *, *, #2025, .T. ) ;
#37581 = ORIENTED_EDGE ( 'NONE', *, *, #59732, .F. ) ;
#37582 = CARTESIAN_POINT ( 'NONE',  ( -6.817976262117261044, 9.722976262117182245, 26.00000000000000711 ) ) ;
#37583 = AXIS2_PLACEMENT_3D ( 'NONE', #33162, #32817, #21180 ) ;
#37584 = EDGE_CURVE ( 'NONE', #54936, #24780, #46120, .T. ) ;
#37585 = DIRECTION ( 'NONE',  ( -0.000000000000000000, 3.673940397442059868E-16, -1.000000000000000000 ) ) ;
#37587 = ADVANCED_FACE ( 'NONE', ( #29503 ), #41159, .T. ) ;
#37586 = DIRECTION ( 'NONE',  ( 0.000000000000000000, 0.000000000000000000, 1.000000000000000000 ) ) ;
#37588 = CARTESIAN_POINT ( 'NONE',  ( -11.07551654964667520, 11.07551654964660237, 455.0000000000000568 ) ) ;
#37589 = VERTEX_POINT ( 'NONE', #2630 ) ;
#37590 = ORIENTED_EDGE ( 'NONE', *, *, #3698, .F. ) ;
#37591 = EDGE_LOOP ( 'NONE', ( #47111, #15407, #7838, #48980 ) ) ;
#37592 = CARTESIAN_POINT ( 'NONE',  ( 26.90000000000000213, 0.000000000000000000, 0.000000000000000000 ) ) ;
#37593 = ORIENTED_EDGE ( 'NONE', *, *, #31157, .F. ) ;
#37594 = CARTESIAN_POINT ( 'NONE',  ( 3.606483450353397568, 4.609516549646590633, 455.0000000000000568 ) ) ;
#37595 = CARTESIAN_POINT ( 'NONE',  ( 7.000000000000000000, -20.40000000000000213, -12.40000000000000213 ) ) ;
#37596 = VECTOR ( 'NONE', #29868, 1000.000000000000000 ) ;
#37597 = VERTEX_POINT ( 'NONE', #40816 ) ;
#37598 = VERTEX_POINT ( 'NONE', #51071 ) ;
#37599 = DIRECTION ( 'NONE',  ( 0.000000000000000000, 1.000000000000000000, 0.000000000000000000 ) ) ;
#37600 = AXIS2_PLACEMENT_3D ( 'NONE', #41950, #9784, #47604 ) ;
#37601 = FACE_OUTER_BOUND ( 'NONE', #25322, .T. ) ;
#37602 = EDGE_LOOP ( 'NONE', ( #26153, #16343, #13382, #66821 ) ) ;
#37603 = CARTESIAN_POINT ( 'NONE',  ( -6.344366288193437953, -5.793274621760813758, 26.00000000000000711 ) ) ;
#37604 = CIRCLE ( 'NONE', #35285, 3.999999999999993339 ) ;
#37606 = EDGE_LOOP ( 'NONE', ( #29227, #33005, #21140, #43997 ) ) ;
#37605 = DIRECTION ( 'NONE',  ( 0.7071067811865560104, 0.000000000000000000, -0.7071067811865391350 ) ) ;
#37607 = ORIENTED_EDGE ( 'NONE', *, *, #19778, .F. ) ;
#37608 = DIRECTION ( 'NONE',  ( 0.000000000000000000, 1.000000000000000000, 0.000000000000000000 ) ) ;
#37609 = DIRECTION ( 'NONE',  ( 0.000000000000000000, -0.7071067811865474617, 0.7071067811865474617 ) ) ;
#37610 = DIRECTION ( 'NONE',  ( 0.000000000000000000, -0.000000000000000000, -1.000000000000000000 ) ) ;
#37611 = CARTESIAN_POINT ( 'NONE',  ( -29.50000000000000355, -15.97213595500069871, -14.50000000000000000 ) ) ;
#37612 = EDGE_CURVE ( 'NONE', #45178, #62286, #31366, .T. ) ;
#37613 = FACE_OUTER_BOUND ( 'NONE', #46864, .T. ) ;
#37614 = VERTEX_POINT ( 'NONE', #19247 ) ;
#37615 = DIRECTION ( 'NONE',  ( 0.000000000000000000, -1.000000000000000000, 0.000000000000000000 ) ) ;
#37616 = ADVANCED_FACE ( 'NONE', ( #3688 ), #2288, .F. ) ;
#37617 = ORIENTED_EDGE ( 'NONE', *, *, #19700, .T. ) ;
#37618 = LINE ( 'NONE', #65193, #58102 ) ;
#37619 = CIRCLE ( 'NONE', #13921, 0.2000000000000005107 ) ;
#37620 = PLANE ( 'NONE',  #5245 ) ;
#37622 = EDGE_CURVE ( 'NONE', #35004, #57266, #34800, .T. ) ;
#37621 = DIRECTION ( 'NONE',  ( -1.000000000000000000, 0.000000000000000000, 0.000000000000000000 ) ) ;
#37624 = CARTESIAN_POINT ( 'NONE',  ( -7.342976262117259623, 3.834182069070703580, 26.00000000000000711 ) ) ;
#37623 = VECTOR ( 'NONE', #2302, 1000.000000000000000 ) ;
#37625 = CIRCLE ( 'NONE', #8215, 2.215251240775983899 ) ;
#37626 = DIRECTION ( 'NONE',  ( 0.000000000000000000, 0.000000000000000000, -1.000000000000000000 ) ) ;
#37627 = ADVANCED_FACE ( 'NONE', ( #29153 ), #45764, .F. ) ;
#37628 = ORIENTED_EDGE ( 'NONE', *, *, #60101, .T. ) ;
#37629 = DIRECTION ( 'NONE',  ( 1.000000000000000000, 0.000000000000000000, 0.000000000000000000 ) ) ;
#37630 = AXIS2_PLACEMENT_3D ( 'NONE', #37357, #47958, #64921 ) ;
#37631 = EDGE_CURVE ( 'NONE', #30523, #32112, #35861, .T. ) ;
#37632 = VECTOR ( 'NONE', #1735, 1000.000000000000000 ) ;
#37633 = ORIENTED_EDGE ( 'NONE', *, *, #33939, .T. ) ;
#37634 = LINE ( 'NONE', #26670, #9029 ) ;
#37635 = DIRECTION ( 'NONE',  ( 0.000000000000000000, 0.000000000000000000, -1.000000000000000000 ) ) ;
#37636 = ORIENTED_EDGE ( 'NONE', *, *, #68476, .F. ) ;
#37637 = CARTESIAN_POINT ( 'NONE',  ( -8.821682069070746479, -2.544523737882736558, 26.00000000000000711 ) ) ;
#37638 = ORIENTED_EDGE ( 'NONE', *, *, #10326, .T. ) ;
#37639 = DIRECTION ( 'NONE',  ( -0.000000000000000000, 1.000000000000000000, -0.000000000000000000 ) ) ;
#37640 = AXIS2_PLACEMENT_3D ( 'NONE', #43274, #64855, #28390 ) ;
#37641 = PLANE ( 'NONE',  #6352 ) ;
#37642 = ADVANCED_FACE ( 'NONE', ( #30560 ), #24204, .F. ) ;
#37643 = LINE ( 'NONE', #59203, #10604 ) ;
#37644 = LINE ( 'NONE', #16420, #19309 ) ;
#37645 = VECTOR ( 'NONE', #54894, 1000.000000000000000 ) ;
#37646 = VERTEX_POINT ( 'NONE', #57428 ) ;
#37648 = ORIENTED_EDGE ( 'NONE', *, *, #44624, .T. ) ;
#37647 = DIRECTION ( 'NONE',  ( -5.981805089575196197E-17, -1.000000000000000000, 0.000000000000000000 ) ) ;
#37649 = CARTESIAN_POINT ( 'NONE',  ( 15.00000000000000000, 0.000000000000000000, -27.00000000000000000 ) ) ;
#37650 = DIRECTION ( 'NONE',  ( 1.000000000000000000, -5.981805089575196197E-17, 0.000000000000000000 ) ) ;
#37651 = DIRECTION ( 'NONE',  ( 0.000000000000000000, 0.000000000000000000, 1.000000000000000000 ) ) ;
#37652 = EDGE_LOOP ( 'NONE', ( #26021, #54008 ) ) ;
#37653 = VECTOR ( 'NONE', #67121, 1000.000000000000114 ) ;
#37654 = FILL_AREA_STYLE_COLOUR ( '', #16359 ) ;
#37655 = CARTESIAN_POINT ( 'NONE',  ( -11.77351654964670935, 4.393516549646602876, 195.0000000000000284 ) ) ;
#37656 = ORIENTED_EDGE ( 'NONE', *, *, #47137, .F. ) ;
#37657 = ORIENTED_EDGE ( 'NONE', *, *, #21505, .T. ) ;
#37658 = ORIENTED_EDGE ( 'NONE', *, *, #13586, .T. ) ;
#37659 = EDGE_CURVE ( 'NONE', #19811, #17866, #4259, .T. ) ;
#37660 = FACE_OUTER_BOUND ( 'NONE', #21019, .T. ) ;
#37661 = CYLINDRICAL_SURFACE ( 'NONE', #45035, 3.499999999999850342 ) ;
#37663 = EDGE_CURVE ( 'NONE', #27468, #59664, #23851, .T. ) ;
#37662 = DIRECTION ( 'NONE',  ( 0.000000000000000000, 1.000000000000000000, 0.000000000000000000 ) ) ;
#37664 = VECTOR ( 'NONE', #4666, 1000.000000000000000 ) ;
#37665 = VECTOR ( 'NONE', #44070, 1000.000000000000000 ) ;
#37666 = ORIENTED_EDGE ( 'NONE', *, *, #24267, .T. ) ;
#37667 = ORIENTED_EDGE ( 'NONE', *, *, #59381, .T. ) ;
#37668 = VECTOR ( 'NONE', #55533, 1000.000000000000000 ) ;
#37669 = LINE ( 'NONE', #32704, #79 ) ;
#37670 = ORIENTED_EDGE ( 'NONE', *, *, #50536, .F. ) ;
#37671 = ORIENTED_EDGE ( 'NONE', *, *, #36563, .T. ) ;
#37672 = ORIENTED_EDGE ( 'NONE', *, *, #31347, .F. ) ;
#37673 = ORIENTED_EDGE ( 'NONE', *, *, #16110, .T. ) ;
#37674 = CARTESIAN_POINT ( 'NONE',  ( -7.250000000000000888, 8.250000000000001776, -11.50000000000000000 ) ) ;
#37675 = AXIS2_PLACEMENT_3D ( 'NONE', #25782, #47332, #20463 ) ;
#37676 = AXIS2_PLACEMENT_3D ( 'NONE', #6569, #60287, #28126 ) ;
#37678 = VERTEX_POINT ( 'NONE', #18903 ) ;
#37677 = DIRECTION ( 'NONE',  ( -1.000000000000000000, 0.000000000000000000, 0.000000000000000000 ) ) ;
#37679 = DIRECTION ( 'NONE',  ( -0.5000000000000019984, -0.8660254037844375974, -0.000000000000000000 ) ) ;
#37680 = CARTESIAN_POINT ( 'NONE',  ( 41.09999999999999432, 20.60000000000000142, -13.86939075806900057 ) ) ;
#37681 = DIRECTION ( 'NONE',  ( -0.000000000000000000, 0.000000000000000000, -1.000000000000000000 ) ) ;
#37682 = ORIENTED_EDGE ( 'NONE', *, *, #29624, .T. ) ;
#37683 = CARTESIAN_POINT ( 'NONE',  ( -3.142976262117267883, -4.046023737882828542, 54.00000000000000711 ) ) ;
#37684 = CARTESIAN_POINT ( 'NONE',  ( -4.141586236041124636, -4.720772854004768426, 26.00000000000000711 ) ) ;
#37685 = EDGE_LOOP ( 'NONE', ( #25955, #51317, #56344, #9662 ) ) ;
#37686 = CARTESIAN_POINT ( 'NONE',  ( 7.450000000000003730, -7.249999999999997335, -10.50000000000000000 ) ) ;
#37687 = EDGE_CURVE ( 'NONE', #62860, #34995, #9856, .T. ) ;
#37688 = CARTESIAN_POINT ( 'NONE',  ( 11.32648345035333293, 4.193516549646572500, 195.0000000000000284 ) ) ;
#37689 = DIRECTION ( 'NONE',  ( 0.000000000000000000, 0.000000000000000000, -1.000000000000000000 ) ) ;
#37690 = VERTEX_POINT ( 'NONE', #51781 ) ;
#37691 = AXIS2_PLACEMENT_3D ( 'NONE', #28463, #7939, #39423 ) ;
#37693 = ADVANCED_FACE ( 'NONE', ( #19949 ), #45408, .T. ) ;
#37692 = CARTESIAN_POINT ( 'NONE',  ( -6.661338147750939243E-15, 17.79289321881346808, 20.50000000000000000 ) ) ;
#37694 = CARTESIAN_POINT ( 'NONE',  ( -15.50000000000000000, 0.000000000000000000, 22.50000000000000000 ) ) ;
#37695 = DIRECTION ( 'NONE',  ( 0.000000000000000000, 1.000000000000000000, 0.000000000000000000 ) ) ;
#37696 = ADVANCED_FACE ( 'NONE', ( #3339 ), #24904, .F. ) ;
#37697 = ADVANCED_FACE ( 'NONE', ( #61317 ), #29850, .T. ) ;
#37698 = LINE ( 'NONE', #59262, #60216 ) ;
#37699 = EDGE_CURVE ( 'NONE', #60252, #13864, #63793, .T. ) ;
#37700 = CARTESIAN_POINT ( 'NONE',  ( 9.562023737882803687, 7.955476262117190167, 26.00000000000000711 ) ) ;
#37701 = EDGE_CURVE ( 'NONE', #46952, #2701, #57777, .T. ) ;
#37702 = CARTESIAN_POINT ( 'NONE',  ( 30.00000000000000000, -10.85999999999999943, -9.350000000000269651 ) ) ;
#37703 = SURFACE_SIDE_STYLE ('',( #42997 ) ) ;
#37704 = CARTESIAN_POINT ( 'NONE',  ( 15.50000000000000000, -5.000000000000000000, -22.50000000000000000 ) ) ;
#37705 = AXIS2_PLACEMENT_3D ( 'NONE', #14488, #58333, #36043 ) ;
#37706 = CIRCLE ( 'NONE', #27555, 4.000000000000000888 ) ;
#37707 = EDGE_CURVE ( 'NONE', #20854, #33919, #25968, .T. ) ;
#37708 = ORIENTED_EDGE ( 'NONE', *, *, #56678, .F. ) ;
#37709 = CARTESIAN_POINT ( 'NONE',  ( -3.842976262117221875, 10.30047626211716860, 26.00000000000000711 ) ) ;
#37710 = DIRECTION ( 'NONE',  ( 0.000000000000000000, 0.000000000000000000, -1.000000000000000000 ) ) ;
#37711 = DIRECTION ( 'NONE',  ( 0.000000000000000000, -3.673940397442059868E-16, 1.000000000000000000 ) ) ;
#37712 = DIRECTION ( 'NONE',  ( 1.221996412923863792E-14, 1.000000000000000000, 1.836970198721013910E-16 ) ) ;
#37713 = VECTOR ( 'NONE', #29096, 1000.000000000000000 ) ;
#37714 = ORIENTED_EDGE ( 'NONE', *, *, #50942, .F. ) ;
#37715 = CARTESIAN_POINT ( 'NONE',  ( 23.75054448485400016, -17.50000000000000000, 25.53140320652400064 ) ) ;
#37716 = DIRECTION ( 'NONE',  ( 0.000000000000000000, -1.000000000000000000, -8.396061623720747815E-13 ) ) ;
#37717 = CARTESIAN_POINT ( 'NONE',  ( 7.000000000000000000, -25.60000000000000142, 15.10000000000000142 ) ) ;
#37718 = LINE ( 'NONE', #11178, #40031 ) ;
#37719 = VECTOR ( 'NONE', #55089, 1000.000000000000000 ) ;
#37720 = VECTOR ( 'NONE', #44574, 1000.000000000000000 ) ;
#37722 = VECTOR ( 'NONE', #15637, 1000.000000000000000 ) ;
#37721 = DIRECTION ( 'NONE',  ( -1.000000000000000000, 0.000000000000000000, 0.000000000000000000 ) ) ;
#37723 = DIRECTION ( 'NONE',  ( -0.7071067811865474617, -0.7071067811865474617, 0.000000000000000000 ) ) ;
#37724 = ORIENTED_EDGE ( 'NONE', *, *, #34567, .T. ) ;
#37725 = VERTEX_POINT ( 'NONE', #20642 ) ;
#37726 = PLANE ( 'NONE',  #68834 ) ;
#37727 = DIRECTION ( 'NONE',  ( -1.794541526872559352E-16, -1.000000000000000000, 0.000000000000000000 ) ) ;
#37728 = ORIENTED_EDGE ( 'NONE', *, *, #47975, .T. ) ;
#37729 = CARTESIAN_POINT ( 'NONE',  ( -6.606374702650169795, 4.734785091273855606, 455.0000000000000568 ) ) ;
#37730 = AXIS2_PLACEMENT_3D ( 'NONE', #6434, #53841, #91 ) ;
#37731 = LINE ( 'NONE', #52959, #21705 ) ;
#37732 = EDGE_LOOP ( 'NONE', ( #65658, #43641, #43165, #47981 ) ) ;
#37733 = CARTESIAN_POINT ( 'NONE',  ( 23.48000000000000043, -17.50000000000000000, 26.00000000000000355 ) ) ;
#37734 = ORIENTED_EDGE ( 'NONE', *, *, #61062, .T. ) ;
#37735 = ORIENTED_EDGE ( 'NONE', *, *, #65404, .T. ) ;
#37736 = CARTESIAN_POINT ( 'NONE',  ( 30.00000000000000000, -11.50000000000100009, -15.00000000000084910 ) ) ;
#37737 = EDGE_LOOP ( 'NONE', ( #25684, #38362, #13640, #11809 ) ) ;
#37738 = CARTESIAN_POINT ( 'NONE',  ( 39.00000000000000000, 0.000000000000000000, 0.000000000000000000 ) ) ;
#37739 = DIRECTION ( 'NONE',  ( 0.000000000000000000, 0.000000000000000000, -1.000000000000000000 ) ) ;
#37741 = EDGE_CURVE ( 'NONE', #5332, #62566, #51686, .T. ) ;
#37740 = DIRECTION ( 'NONE',  ( -0.000000000000000000, -0.000000000000000000, -1.000000000000000000 ) ) ;
#37742 = VERTEX_POINT ( 'NONE', #31965 ) ;
#37743 = AXIS2_PLACEMENT_3D ( 'NONE', #35879, #41878, #13951 ) ;
#37745 = ADVANCED_FACE ( 'NONE', ( #58129 ), #69439, .F. ) ;
#37744 = ORIENTED_EDGE ( 'NONE', *, *, #63028, .F. ) ;
#37746 = FACE_OUTER_BOUND ( 'NONE', #63298, .T. ) ;
#37747 = EDGE_CURVE ( 'NONE', #41000, #55063, #31284, .T. ) ;
#37749 = LINE ( 'NONE', #48006, #43501 ) ;
#37748 = CARTESIAN_POINT ( 'NONE',  ( 41.09999999999999432, -0.2000000000000000111, 0.000000000000000000 ) ) ;
#37750 = ORIENTED_EDGE ( 'NONE', *, *, #26449, .F. ) ;
#37751 = CIRCLE ( 'NONE', #7229, 0.3999999999999993006 ) ;
#37752 = EDGE_LOOP ( 'NONE', ( #19479, #64379, #19012, #19371 ) ) ;
#37753 = EDGE_CURVE ( 'NONE', #50075, #62767, #53199, .T. ) ;
#37754 = ORIENTED_EDGE ( 'NONE', *, *, #60274, .F. ) ;
#37755 = CARTESIAN_POINT ( 'NONE',  ( 275.5000000000000000, -0.5000000000000000000, -27.00000000000000000 ) ) ;
#37757 = ORIENTED_EDGE ( 'NONE', *, *, #682, .F. ) ;
#37756 = DIRECTION ( 'NONE',  ( 0.000000000000000000, -1.000000000000000000, 0.000000000000000000 ) ) ;
#37758 = LINE ( 'NONE', #15836, #5164 ) ;
#37759 = AXIS2_PLACEMENT_3D ( 'NONE', #6908, #56049, #1600 ) ;
#37760 = VECTOR ( 'NONE', #54540, 1000.000000000000000 ) ;
#37761 = DIRECTION ( 'NONE',  ( 1.000000000000000000, -0.000000000000000000, 0.000000000000000000 ) ) ;
#37762 = VERTEX_POINT ( 'NONE', #36207 ) ;
#37763 = ORIENTED_EDGE ( 'NONE', *, *, #55273, .F. ) ;
#37764 = AXIS2_PLACEMENT_3D ( 'NONE', #12658, #39540, #21910 ) ;
#37765 = AXIS2_PLACEMENT_3D ( 'NONE', #10674, #32242, #11027 ) ;
#37766 = DIRECTION ( 'NONE',  ( 0.000000000000000000, 0.000000000000000000, 1.000000000000000000 ) ) ;
#37767 = EDGE_LOOP ( 'NONE', ( #40593, #32323, #5134, #17086 ) ) ;
#37768 = PLANE ( 'NONE',  #24734 ) ;
#37769 = DIRECTION ( 'NONE',  ( 0.000000000000000000, 0.000000000000000000, 1.000000000000000000 ) ) ;
#37770 = CIRCLE ( 'NONE', #26465, 0.9999999999999991118 ) ;
#37771 = VERTEX_POINT ( 'NONE', #47522 ) ;
#37772 = EDGE_CURVE ( 'NONE', #41033, #33622, #34755, .T. ) ;
#37773 = DIRECTION ( 'NONE',  ( -1.000000000000000000, 0.000000000000000000, 0.000000000000000000 ) ) ;
#37774 = DIRECTION ( 'NONE',  ( -7.808916176531286882E-15, -1.000000000000000000, -3.673940397442059868E-16 ) ) ;
#37776 = VERTEX_POINT ( 'NONE', #48575 ) ;
#37775 = PRESENTATION_STYLE_ASSIGNMENT (( #53005 ) ) ;
#37777 = ORIENTED_EDGE ( 'NONE', *, *, #34902, .F. ) ;
#37778 = VECTOR ( 'NONE', #32178, 1000.000000000000000 ) ;
#37779 = DIRECTION ( 'NONE',  ( -0.000000000000000000, 3.673940397442059868E-16, -1.000000000000000000 ) ) ;
#37780 = DIRECTION ( 'NONE',  ( -1.000000000000000000, 0.000000000000000000, 0.000000000000000000 ) ) ;
#37781 = CARTESIAN_POINT ( 'NONE',  ( -9.781776262117249487, 10.49297626211718359, 26.00000000000000711 ) ) ;
#37782 = DIRECTION ( 'NONE',  ( 0.000000000000000000, 0.000000000000000000, 1.000000000000000000 ) ) ;
#37783 = DIRECTION ( 'NONE',  ( -1.000000000000000000, 0.000000000000000000, 0.000000000000000000 ) ) ;
#37785 = ORIENTED_EDGE ( 'NONE', *, *, #7332, .F. ) ;
#37784 = ADVANCED_FACE ( 'NONE', ( #26659 ), #69089, .F. ) ;
#37786 = CARTESIAN_POINT ( 'NONE',  ( -9.897976262117250457, -3.857023737882721903, 54.00000000000000711 ) ) ;
#37787 = EDGE_CURVE ( 'NONE', #18785, #39920, #9959, .T. ) ;
#37788 = CARTESIAN_POINT ( 'NONE',  ( 7.900000000000000355, 14.08845687959340331, 21.00000000000000000 ) ) ;
#37789 = CARTESIAN_POINT ( 'NONE',  ( 7.606483450353376696, 11.77351654964662053, 195.0000000000000284 ) ) ;
#37791 = VERTEX_POINT ( 'NONE', #41517 ) ;
#37790 = DIRECTION ( 'NONE',  ( 0.000000000000000000, 0.000000000000000000, -1.000000000000000000 ) ) ;
#37792 = FACE_OUTER_BOUND ( 'NONE', #47979, .T. ) ;
#37793 = EDGE_CURVE ( 'NONE', #33976, #55193, #32312, .T. ) ;
#37794 = CARTESIAN_POINT ( 'NONE',  ( -2.693516549646675529, 10.91351654964657314, 455.0000000000000568 ) ) ;
#37795 = VECTOR ( 'NONE', #26873, 1000.000000000000000 ) ;
#37796 = DIRECTION ( 'NONE',  ( -0.000000000000000000, 3.673940397442059868E-16, -1.000000000000000000 ) ) ;
#37797 = LINE ( 'NONE', #1346, #51043 ) ;
#37798 = ORIENTED_EDGE ( 'NONE', *, *, #62949, .T. ) ;
#37799 = LINE ( 'NONE', #1017, #67055 ) ;
#37800 = CARTESIAN_POINT ( 'NONE',  ( -7.342976262117259623, 4.947141984184421304, 26.00000000000000711 ) ) ;
#37801 = AXIS2_PLACEMENT_3D ( 'NONE', #29954, #3099, #4503 ) ;
#37802 = ORIENTED_EDGE ( 'NONE', *, *, #69483, .T. ) ;
#37803 = DIRECTION ( 'NONE',  ( -1.000000000000000000, 0.000000000000000000, 0.000000000000000000 ) ) ;
#37804 = CARTESIAN_POINT ( 'NONE',  ( 6.344579767990823349, -8.406483450353491094, 455.0000000000000568 ) ) ;
#37805 = CARTESIAN_POINT ( 'NONE',  ( 28.00000000000000000, -15.50000000000000000, -14.50000000000000000 ) ) ;
#37806 = DIRECTION ( 'NONE',  ( 1.000000000000000000, -5.981805089575194965E-17, 0.000000000000000000 ) ) ;
#37807 = DIRECTION ( 'NONE',  ( 0.000000000000000000, 0.000000000000000000, 1.000000000000000000 ) ) ;
#37808 = AXIS2_PLACEMENT_3D ( 'NONE', #22147, #43714, #42664 ) ;
#37809 = VECTOR ( 'NONE', #58376, 1000.000000000000000 ) ;
#37810 = ORIENTED_EDGE ( 'NONE', *, *, #17650, .T. ) ;
#37811 = VERTEX_POINT ( 'NONE', #26305 ) ;
#37812 = PLANE ( 'NONE',  #31812 ) ;
#37813 = EDGE_LOOP ( 'NONE', ( #13647, #10076, #11330, #67573 ) ) ;
#37814 = ORIENTED_EDGE ( 'NONE', *, *, #53986, .T. ) ;
#37815 = DIRECTION ( 'NONE',  ( 0.000000000000000000, 1.000000000000000000, 0.000000000000000000 ) ) ;
#37816 = VECTOR ( 'NONE', #53234, 1000.000000000000000 ) ;
#37817 = CARTESIAN_POINT ( 'NONE',  ( 15.50000000000000000, -5.000000000000000000, 22.50000000000000000 ) ) ;
#37818 = AXIS2_PLACEMENT_3D ( 'NONE', #9832, #47302, #51910 ) ;
#37819 = DIRECTION ( 'NONE',  ( -1.000000000000000000, 0.000000000000000000, 0.000000000000000000 ) ) ;
#37820 = VERTEX_POINT ( 'NONE', #53892 ) ;
#37821 = ORIENTED_EDGE ( 'NONE', *, *, #56977, .T. ) ;
#37822 = CARTESIAN_POINT ( 'NONE',  ( 3.606483450353350051, 4.609516549646638595, 195.0000000000000284 ) ) ;
#37823 = VERTEX_POINT ( 'NONE', #15704 ) ;
#37824 = ORIENTED_EDGE ( 'NONE', *, *, #12061, .T. ) ;
#37825 = DIRECTION ( 'NONE',  ( -3.491481338843133355E-15, -1.000000000000000000, -1.836970198721029934E-16 ) ) ;
#37826 = DIRECTION ( 'NONE',  ( 0.000000000000000000, 0.000000000000000000, -1.000000000000000000 ) ) ;
#37827 = VECTOR ( 'NONE', #9081, 1000.000000000000000 ) ;
#37828 = DIRECTION ( 'NONE',  ( -1.000000000000000000, 0.000000000000000000, 0.000000000000000000 ) ) ;
#37829 = ORIENTED_EDGE ( 'NONE', *, *, #10525, .T. ) ;
#37830 = EDGE_CURVE ( 'NONE', #14935, #18504, #15571, .T. ) ;
#37831 = VECTOR ( 'NONE', #52926, 1000.000000000000000 ) ;
#37832 = EDGE_CURVE ( 'NONE', #31859, #15321, #42568, .T. ) ;
#37833 = CARTESIAN_POINT ( 'NONE',  ( 283.0000000000000568, -23.29603921945599865, -12.50000000000000000 ) ) ;
#37834 = ADVANCED_FACE ( 'NONE', ( #10394 ), #53538, .T. ) ;
#37836 = CARTESIAN_POINT ( 'NONE',  ( -7.250000000000000888, 7.250000000000001776, -26.00000000000001066 ) ) ;
#37835 = CARTESIAN_POINT ( 'NONE',  ( 25.50000000000000355, -5.578999999999999737, 22.50000000000000000 ) ) ;
#37837 = ORIENTED_EDGE ( 'NONE', *, *, #26038, .F. ) ;
#37838 = VERTEX_POINT ( 'NONE', #21354 ) ;
#37840 = ORIENTED_EDGE ( 'NONE', *, *, #24275, .T. ) ;
#37839 = CARTESIAN_POINT ( 'NONE',  ( -8.916576262117349216, -8.930623737882767088, 54.00000000000000711 ) ) ;
#37841 = VERTEX_POINT ( 'NONE', #48231 ) ;
#37842 = EDGE_CURVE ( 'NONE', #26123, #40904, #2007, .T. ) ;
#37843 = LINE ( 'NONE', #53074, #2808 ) ;
#37844 = CARTESIAN_POINT ( 'NONE',  ( -6.835476262117260227, 10.30047626211718104, 54.00000000000000711 ) ) ;
#37845 = ORIENTED_EDGE ( 'NONE', *, *, #64158, .T. ) ;
#37846 = EDGE_LOOP ( 'NONE', ( #36614, #25855, #27979, #41447 ) ) ;
#37847 = FACE_OUTER_BOUND ( 'NONE', #45114, .T. ) ;
#37848 = DIRECTION ( 'NONE',  ( 0.000000000000000000, 3.673940397442059868E-16, -1.000000000000000000 ) ) ;
#37849 = CIRCLE ( 'NONE', #38946, 5.000000000000000000 ) ;
#37850 = ORIENTED_EDGE ( 'NONE', *, *, #53850, .F. ) ;
#37851 = ORIENTED_EDGE ( 'NONE', *, *, #56565, .F. ) ;
#37852 = DIRECTION ( 'NONE',  ( 0.000000000000000000, 0.000000000000000000, 1.000000000000000000 ) ) ;
#37853 = DIRECTION ( 'NONE',  ( -1.000000000000000000, 0.000000000000000000, 0.000000000000000000 ) ) ;
#37854 = EDGE_CURVE ( 'NONE', #56381, #41426, #17809, .T. ) ;
#37855 = CARTESIAN_POINT ( 'NONE',  ( -7.250000000000000888, 8.250000000000001776, -14.00000000000000000 ) ) ;
#37856 = ORIENTED_EDGE ( 'NONE', *, *, #25569, .T. ) ;
#37857 = AXIS2_PLACEMENT_3D ( 'NONE', #52768, #45670, #35061 ) ;
#37858 = CIRCLE ( 'NONE', #20939, 1.929199999999998028 ) ;
#37859 = DIRECTION ( 'NONE',  ( 0.000000000000000000, 1.000000000000000000, 0.000000000000000000 ) ) ;
#37860 = CARTESIAN_POINT ( 'NONE',  ( 152.0064834503532722, -35.83962462487175316, 5.000000000000000000 ) ) ;
#37862 = EDGE_LOOP ( 'NONE', ( #56348, #25105, #31912, #28421 ) ) ;
#37861 = DIRECTION ( 'NONE',  ( 0.000000000000000000, 0.000000000000000000, 1.000000000000000000 ) ) ;
#37864 = ORIENTED_EDGE ( 'NONE', *, *, #34813, .F. ) ;
#37863 = LINE ( 'NONE', #20895, #4136 ) ;
#37865 = CARTESIAN_POINT ( 'NONE',  ( 283.0000000000000568, -38.65000000000095781, -14.49999999999903899 ) ) ;
#37866 = VECTOR ( 'NONE', #30861, 1000.000000000000000 ) ;
#37867 = LINE ( 'NONE', #42815, #29543 ) ;
#37868 = CARTESIAN_POINT ( 'NONE',  ( -10.50000000000000178, -9.690000000000001279, -5.000000000000000000 ) ) ;
#37869 = PLANE ( 'NONE',  #52773 ) ;
#37870 = LINE ( 'NONE', #54138, #36192 ) ;
#37871 = VECTOR ( 'NONE', #61272, 1000.000000000000000 ) ;
#37872 = DIRECTION ( 'NONE',  ( -7.457533623526253657E-15, -1.000000000000000000, -1.836970198721024757E-16 ) ) ;
#37873 = EDGE_LOOP ( 'NONE', ( #16693, #9709, #51994, #10022 ) ) ;
#37874 = DIRECTION ( 'NONE',  ( -1.000000000000000000, 0.000000000000000000, 0.000000000000000000 ) ) ;
#37875 = EDGE_CURVE ( 'NONE', #68313, #15525, #848, .T. ) ;
#37877 = ORIENTED_EDGE ( 'NONE', *, *, #36507, .T. ) ;
#37876 = FACE_OUTER_BOUND ( 'NONE', #25020, .T. ) ;
#37879 = VERTEX_POINT ( 'NONE', #64839 ) ;
#37878 = DIRECTION ( 'NONE',  ( 0.000000000000000000, 0.000000000000000000, -1.000000000000000000 ) ) ;
#37880 = AXIS2_PLACEMENT_3D ( 'NONE', #8283, #20307, #47187 ) ;
#37881 = CARTESIAN_POINT ( 'NONE',  ( -4.383466043307859827, 8.393516549646589553, 455.0000000000000568 ) ) ;
#37882 = EDGE_CURVE ( 'NONE', #44394, #122, #65276, .T. ) ;
#37883 = ADVANCED_FACE ( 'NONE', ( #11424 ), #1178, .T. ) ;
#37884 = AXIS2_PLACEMENT_3D ( 'NONE', #67159, #28289, #1418 ) ;
#37885 = CARTESIAN_POINT ( 'NONE',  ( 111.9257688011041836, 0.000000000000000000, 281.4830310981151911 ) ) ;
#37886 = EDGE_CURVE ( 'NONE', #62248, #51904, #65196, .T. ) ;
#37887 = ORIENTED_EDGE ( 'NONE', *, *, #27632, .F. ) ;
#37888 = CARTESIAN_POINT ( 'NONE',  ( -4.193516549646833624, -11.32648345035344128, 455.0000000000000568 ) ) ;
#37889 = CARTESIAN_POINT ( 'NONE',  ( -7.839518282750262301, 3.417780618358531530, 455.0000000000000568 ) ) ;
#37890 = ORIENTED_EDGE ( 'NONE', *, *, #69803, .F. ) ;
#37891 = EDGE_CURVE ( 'NONE', #58674, #26866, #12114, .T. ) ;
#37892 = FACE_OUTER_BOUND ( 'NONE', #16526, .T. ) ;
#37893 = CARTESIAN_POINT ( 'NONE',  ( -9.293516549646710700, 10.91351654964659801, 455.0000000000000568 ) ) ;
#37894 = EDGE_CURVE ( 'NONE', #2965, #36815, #48924, .T. ) ;
#37895 = CARTESIAN_POINT ( 'NONE',  ( -9.722976262117258628, 3.667976262117184749, 26.00000000000000711 ) ) ;
#37896 = ADVANCED_FACE ( 'NONE', ( #33682 ), #33001, .F. ) ;
#37897 = EDGE_CURVE ( 'NONE', #7638, #18944, #65527, .T. ) ;
#37898 = ORIENTED_EDGE ( 'NONE', *, *, #52934, .T. ) ;
#37899 = LINE ( 'NONE', #59460, #34852 ) ;
#37900 = ORIENTED_EDGE ( 'NONE', *, *, #420, .F. ) ;
#37901 = VERTEX_POINT ( 'NONE', #54578 ) ;
#37902 = LINE ( 'NONE', #23010, #22314 ) ;
#37903 = DIRECTION ( 'NONE',  ( 1.000000000000000000, -0.000000000000000000, -0.000000000000000000 ) ) ;
#37904 = CIRCLE ( 'NONE', #40135, 0.5000000000001357803 ) ;
#37905 = LINE ( 'NONE', #21638, #35511 ) ;
#37906 = CIRCLE ( 'NONE', #54859, 1.000000000000000000 ) ;
#37907 = CARTESIAN_POINT ( 'NONE',  ( -15.50000000000000000, -2.500000000000000000, 21.05662432702600029 ) ) ;
#37908 = ORIENTED_EDGE ( 'NONE', *, *, #60240, .F. ) ;
#37909 = ORIENTED_EDGE ( 'NONE', *, *, #51048, .T. ) ;
#37911 = ORIENTED_EDGE ( 'NONE', *, *, #7468, .T. ) ;
#37910 = CARTESIAN_POINT ( 'NONE',  ( 8.900000000000005684, -21.00000000000000000, -18.00000000000000355 ) ) ;
#37912 = VERTEX_POINT ( 'NONE', #33346 ) ;
#37913 = AXIS2_PLACEMENT_3D ( 'NONE', #10447, #32375, #22105 ) ;
#37914 = AXIS2_PLACEMENT_3D ( 'NONE', #34976, #26483, #5615 ) ;
#37915 = AXIS2_PLACEMENT_3D ( 'NONE', #58384, #8514, #52368 ) ;
#37916 = CARTESIAN_POINT ( 'NONE',  ( -5.242976262117280406, -5.257023737882805747, 54.00000000000000711 ) ) ;
#37917 = CARTESIAN_POINT ( 'NONE',  ( -8.079219948824961861, -8.711985858128649340, 54.00000000000000711 ) ) ;
#37918 = DIRECTION ( 'NONE',  ( 0.000000000000000000, 3.673940397442059868E-16, -1.000000000000000000 ) ) ;
#37919 = FACE_BOUND ( 'NONE', #27977, .T. ) ;
#37920 = VECTOR ( 'NONE', #20455, 1000.000000000000000 ) ;
#37921 = VECTOR ( 'NONE', #47991, 1000.000000000000000 ) ;
#37922 = VECTOR ( 'NONE', #68618, 1000.000000000000000 ) ;
#37924 = CARTESIAN_POINT ( 'NONE',  ( 10.31452373788280497, 6.642976262117183062, 54.00000000000000711 ) ) ;
#37923 = CARTESIAN_POINT ( 'NONE',  ( 7.000000000000000000, -31.30000000000095284, -12.19999999999906315 ) ) ;
#37925 = ORIENTED_EDGE ( 'NONE', *, *, #57890, .F. ) ;
#37927 = EDGE_LOOP ( 'NONE', ( #66469, #16447 ) ) ;
#37926 = DIRECTION ( 'NONE',  ( 0.5001543609659999667, 0.000000000000000000, -0.8659362650950080953 ) ) ;
#37928 = ORIENTED_EDGE ( 'NONE', *, *, #49777, .F. ) ;
#37929 = ORIENTED_EDGE ( 'NONE', *, *, #27902, .F. ) ;
#37930 = AXIS2_PLACEMENT_3D ( 'NONE', #65668, #28517, #44419 ) ;
#37931 = FACE_OUTER_BOUND ( 'NONE', #27153, .T. ) ;
#37932 = LINE ( 'NONE', #16014, #34335 ) ;
#37933 = PLANE ( 'NONE',  #16207 ) ;
#37934 = ORIENTED_EDGE ( 'NONE', *, *, #34557, .F. ) ;
#37935 = ORIENTED_EDGE ( 'NONE', *, *, #33168, .T. ) ;
#37936 = VERTEX_POINT ( 'NONE', #38653 ) ;
#37937 = VECTOR ( 'NONE', #38232, 1000.000000000000000 ) ;
#37938 = DIRECTION ( 'NONE',  ( -1.000000000000000000, 0.000000000000000000, 0.000000000000000000 ) ) ;
#37939 = EDGE_CURVE ( 'NONE', #11801, #36500, #17421, .T. ) ;
#37940 = CARTESIAN_POINT ( 'NONE',  ( 9.955011587777235604, -2.765062094116086833, 195.0000000000000284 ) ) ;
#37941 = PLANE ( 'NONE',  #27758 ) ;
#37942 = ORIENTED_EDGE ( 'NONE', *, *, #10973, .T. ) ;
#37943 = ORIENTED_EDGE ( 'NONE', *, *, #31010, .F. ) ;
#37944 = DIRECTION ( 'NONE',  ( 0.000000000000000000, 1.000000000000000000, 0.000000000000000000 ) ) ;
#37945 = EDGE_CURVE ( 'NONE', #28048, #56362, #44625, .T. ) ;
#37946 = CARTESIAN_POINT ( 'NONE',  ( 24.90000000000000213, 0.000000000000000000, 1.723948796001796511E-15 ) ) ;
#37947 = EDGE_LOOP ( 'NONE', ( #39, #69212, #23988, #33100 ) ) ;
#37948 = DIRECTION ( 'NONE',  ( -0.000000000000000000, 0.000000000000000000, -1.000000000000000000 ) ) ;
#37949 = ADVANCED_FACE ( 'NONE', ( #12446 ), #11762, .T. ) ;
#37950 = AXIS2_PLACEMENT_3D ( 'NONE', #39070, #6884, #49350 ) ;
#37952 = ORIENTED_EDGE ( 'NONE', *, *, #4074, .F. ) ;
#37951 = CARTESIAN_POINT ( 'NONE',  ( 10.05377373788278739, -9.703773737882823269, 54.00000000000000711 ) ) ;
#37953 = ORIENTED_EDGE ( 'NONE', *, *, #38752, .F. ) ;
#37954 = FACE_OUTER_BOUND ( 'NONE', #11466, .T. ) ;
#37955 = DIRECTION ( 'NONE',  ( -0.000000000000000000, -0.000000000000000000, 1.000000000000000000 ) ) ;
#37956 = DIRECTION ( 'NONE',  ( -0.6414496315691494699, 0.7671651518153064231, 2.818519042764025305E-16 ) ) ;
#37957 = EDGE_CURVE ( 'NONE', #59636, #38923, #39336, .T. ) ;
#37958 = FACE_OUTER_BOUND ( 'NONE', #59227, .T. ) ;
#37959 = CARTESIAN_POINT ( 'NONE',  ( 41.09999999999999432, -0.2000000000000000111, 0.000000000000000000 ) ) ;
#37960 = VECTOR ( 'NONE', #10072, 1000.000000000000000 ) ;
#37961 = ORIENTED_EDGE ( 'NONE', *, *, #42758, .T. ) ;
#37962 = DIRECTION ( 'NONE',  ( -8.339399738404099512E-15, -1.000000000000000000, 0.000000000000000000 ) ) ;
#37963 = EDGE_LOOP ( 'NONE', ( #64100, #16212, #64200, #16324 ) ) ;
#37964 = AXIS2_PLACEMENT_3D ( 'NONE', #49920, #17392, #29048 ) ;
#37965 = VECTOR ( 'NONE', #67776, 1000.000000000000000 ) ;
#37967 = LINE ( 'NONE', #5089, #16309 ) ;
#37966 = VECTOR ( 'NONE', #60094, 1000.000000000000000 ) ;
#37968 = DIRECTION ( 'NONE',  ( -1.000000000000000000, 0.000000000000000000, 0.000000000000000000 ) ) ;
#37969 = EDGE_CURVE ( 'NONE', #58919, #36973, #44285, .T. ) ;
#37970 = DIRECTION ( 'NONE',  ( 0.000000000000000000, 0.000000000000000000, 1.000000000000000000 ) ) ;
#37971 = CARTESIAN_POINT ( 'NONE',  ( 7.250000000000005329, 7.250000000000000888, -7.500000000000000000 ) ) ;
#37972 = VECTOR ( 'NONE', #11149, 1000.000000000000000 ) ;
#37973 = VECTOR ( 'NONE', #52438, 1000.000000000000000 ) ;
#37974 = VECTOR ( 'NONE', #69582, 1000.000000000000000 ) ;
#37975 = PLANE ( 'NONE',  #51745 ) ;
#37976 = ORIENTED_EDGE ( 'NONE', *, *, #48011, .T. ) ;
#37977 = AXIS2_PLACEMENT_3D ( 'NONE', #66279, #61290, #1923 ) ;
#37978 = DIRECTION ( 'NONE',  ( 0.000000000000000000, 0.000000000000000000, -1.000000000000000000 ) ) ;
#37979 = ADVANCED_FACE ( 'NONE', ( #65860, #54233 ), #38988, .F. ) ;
#37980 = CARTESIAN_POINT ( 'NONE',  ( -7.250000000000001776, -7.249999999999998224, -20.50000000000000000 ) ) ;
#37981 = EDGE_CURVE ( 'NONE', #32607, #37742, #34020, .T. ) ;
#37982 = VECTOR ( 'NONE', #64142, 1000.000000000000000 ) ;
#37983 = ORIENTED_EDGE ( 'NONE', *, *, #47854, .T. ) ;
#37984 = DIRECTION ( 'NONE',  ( 0.7071067811865398012, -0.7071067811865552333, 0.000000000000000000 ) ) ;
#37985 = CYLINDRICAL_SURFACE ( 'NONE', #63745, 0.1999999999999996503 ) ;
#37986 = VERTEX_POINT ( 'NONE', #55604 ) ;
#37987 = FACE_OUTER_BOUND ( 'NONE', #38811, .T. ) ;
#37988 = LINE ( 'NONE', #31986, #12712 ) ;
#37989 = VERTEX_POINT ( 'NONE', #7144 ) ;
#37990 = DIRECTION ( 'NONE',  ( 1.000000000000000000, -0.000000000000000000, 0.000000000000000000 ) ) ;
#37991 = EDGE_CURVE ( 'NONE', #12647, #64953, #18919, .T. ) ;
#37992 = LINE ( 'NONE', #54252, #2960 ) ;
#37993 =( NAMED_UNIT ( * ) PLANE_ANGLE_UNIT ( ) SI_UNIT ( $, .RADIAN. ) );
#37994 = DIRECTION ( 'NONE',  ( 1.000000000000000000, -0.000000000000000000, -0.000000000000000000 ) ) ;
#37995 = ORIENTED_EDGE ( 'NONE', *, *, #986, .F. ) ;
#37997 = ORIENTED_EDGE ( 'NONE', *, *, #41847, .T. ) ;
#37996 = PLANE ( 'NONE',  #59954 ) ;
#37998 = PLANE ( 'NONE',  #46309 ) ;
#37999 = CARTESIAN_POINT ( 'NONE',  ( 15.50000000000000000, -0.2038245569916604938, -21.05662432702600029 ) ) ;
#38000 = FACE_OUTER_BOUND ( 'NONE', #69595, .T. ) ;
#38001 = VERTEX_POINT ( 'NONE', #2204 ) ;
#38002 = CIRCLE ( 'NONE', #59445, 1.929199999999998028 ) ;
#38003 = CARTESIAN_POINT ( 'NONE',  ( 29.25000000000000000, -5.000000000000000000, -26.25000000000000000 ) ) ;
#38004 = DIRECTION ( 'NONE',  ( 0.000000000000000000, 0.000000000000000000, 1.000000000000000000 ) ) ;
#38005 = AXIS2_PLACEMENT_3D ( 'NONE', #56676, #23100, #56328 ) ;
#38006 = VERTEX_POINT ( 'NONE', #34356 ) ;
#38007 = ORIENTED_EDGE ( 'NONE', *, *, #6254, .F. ) ;
#38008 = EDGE_CURVE ( 'NONE', #10926, #66328, #64128, .T. ) ;
#38009 = CIRCLE ( 'NONE', #17699, 4.000000000000000000 ) ;
#38010 = VECTOR ( 'NONE', #22294, 1000.000000000000000 ) ;
#38011 = ORIENTED_EDGE ( 'NONE', *, *, #31972, .F. ) ;
#38012 = CARTESIAN_POINT ( 'NONE',  ( 275.0000000000000000, -20.40000000000000213, 17.60000000000000142 ) ) ;
#38013 = ADVANCED_FACE ( 'NONE', ( #56297 ), #34721, .F. ) ;
#38014 = CARTESIAN_POINT ( 'NONE',  ( 30.00000000000000000, -17.50000000000000000, 26.64999999999999858 ) ) ;
#38015 = AXIS2_PLACEMENT_3D ( 'NONE', #39596, #45248, #2128 ) ;
#38016 = AXIS2_PLACEMENT_3D ( 'NONE', #7769, #18028, #2469 ) ;
#38017 = AXIS2_PLACEMENT_3D ( 'NONE', #15239, #40698, #47404 ) ;
#38018 = EDGE_LOOP ( 'NONE', ( #5892, #50245, #66945, #20261 ) ) ;
#38019 = VERTEX_POINT ( 'NONE', #23770 ) ;
#38020 = ORIENTED_EDGE ( 'NONE', *, *, #47501, .T. ) ;
#38021 = EDGE_CURVE ( 'NONE', #35023, #8790, #35063, .T. ) ;
#38022 = CARTESIAN_POINT ( 'NONE',  ( 7.250000000000005329, -7.249999999999998224, -12.50000000000000000 ) ) ;
#38023 = VECTOR ( 'NONE', #2192, 1000.000000000000000 ) ;
#38024 = VECTOR ( 'NONE', #5232, 999.9999999999998863 ) ;
#38025 = VERTEX_POINT ( 'NONE', #29079 ) ;
#38026 = ADVANCED_FACE ( 'NONE', ( #45322 ), #40733, .T. ) ;
#38027 = ORIENTED_EDGE ( 'NONE', *, *, #2562, .F. ) ;
#38028 = ORIENTED_EDGE ( 'NONE', *, *, #34321, .F. ) ;
#38029 = ORIENTED_EDGE ( 'NONE', *, *, #27107, .F. ) ;
#38030 = AXIS2_PLACEMENT_3D ( 'NONE', #44873, #39902, #66088 ) ;
#38031 = CARTESIAN_POINT ( 'NONE',  ( -5.655420232009311654, -8.406483450353382736, 195.0000000000000284 ) ) ;
#38032 = UNCERTAINTY_MEASURE_WITH_UNIT (LENGTH_MEASURE( 1.000000000000000082E-05 ), #51157, 'distance_accuracy_value', 'NONE');
#38033 = EDGE_CURVE ( 'NONE', #13102, #60914, #5427, .T. ) ;
#38035 = ORIENTED_EDGE ( 'NONE', *, *, #11221, .T. ) ;
#38034 = DIRECTION ( 'NONE',  ( 1.000000000000000000, -0.000000000000000000, -0.000000000000000000 ) ) ;
#38036 = CARTESIAN_POINT ( 'NONE',  ( -2.355476262117229158, 9.547976262117156665, 26.00000000000000711 ) ) ;
#38037 = PRODUCT ( 'Mounting Feet', 'Mounting Feet', '', ( #58275 ) ) ;
#38038 = CIRCLE ( 'NONE', #62846, 0.5000000000004272138 ) ;
#38039 = DIRECTION ( 'NONE',  ( 0.000000000000000000, 0.000000000000000000, -1.000000000000000000 ) ) ;
#38040 = DIRECTION ( 'NONE',  ( -1.000000000000000000, -0.000000000000000000, -0.000000000000000000 ) ) ;
#38041 = EDGE_CURVE ( 'NONE', #69380, #63685, #50641, .T. ) ;
#38042 = ORIENTED_EDGE ( 'NONE', *, *, #5978, .F. ) ;
#38043 = EDGE_CURVE ( 'NONE', #47818, #41057, #66891, .T. ) ;
#38044 = EDGE_CURVE ( 'NONE', #4484, #65633, #24113, .T. ) ;
#38045 = ADVANCED_FACE ( 'NONE', ( #18447 ), #67258, .F. ) ;
#38046 = DIRECTION ( 'NONE',  ( 9.912705577010361640E-15, 1.000000000000000000, 0.000000000000000000 ) ) ;
#38047 = ORIENTED_EDGE ( 'NONE', *, *, #54796, .F. ) ;
#38048 = DIRECTION ( 'NONE',  ( 1.000000000000000000, -0.000000000000000000, -0.000000000000000000 ) ) ;
#38049 = EDGE_CURVE ( 'NONE', #7966, #16300, #25754, .T. ) ;
#38050 = LINE ( 'NONE', #43690, #51460 ) ;
#38051 = CARTESIAN_POINT ( 'NONE',  ( 39.00000000000000000, -21.00000000000000000, 16.96999999999999886 ) ) ;
#38052 = VECTOR ( 'NONE', #60470, 1000.000000000000000 ) ;
#38053 = ORIENTED_EDGE ( 'NONE', *, *, #33509, .F. ) ;
#38054 = CARTESIAN_POINT ( 'NONE',  ( -11.77351654964670935, 4.173516549646604901, 455.0000000000000568 ) ) ;
#38055 = CARTESIAN_POINT ( 'NONE',  ( -9.690000000000001279, -9.690000000000001279, -5.000000000000000000 ) ) ;
#38056 = VECTOR ( 'NONE', #1325, 1000.000000000000000 ) ;
#38057 = CARTESIAN_POINT ( 'NONE',  ( -11.00000000000000000, -17.50000000000000000, 26.64999999999999858 ) ) ;
#38058 = AXIS2_PLACEMENT_3D ( 'NONE', #66719, #61400, #34533 ) ;
#38059 = AXIS2_PLACEMENT_3D ( 'NONE', #48032, #10898, #64993 ) ;
#38060 = CARTESIAN_POINT ( 'NONE',  ( 0.9555237378827827754, -9.929523737882790968, 54.00000000000000711 ) ) ;
#38061 = DIRECTION ( 'NONE',  ( 0.000000000000000000, -0.000000000000000000, -1.000000000000000000 ) ) ;
#38062 = FACE_OUTER_BOUND ( 'NONE', #56686, .T. ) ;
#38063 = ADVANCED_FACE ( 'NONE', ( #40013 ), #66555, .T. ) ;
#38064 = DIRECTION ( 'NONE',  ( 2.990116172375847553E-15, 1.000000000000000000, 0.000000000000000000 ) ) ;
#38065 = LINE ( 'NONE', #16830, #48105 ) ;
#38066 = EDGE_CURVE ( 'NONE', #24350, #12410, #37014, .T. ) ;
#38067 = AXIS2_PLACEMENT_3D ( 'NONE', #5881, #28465, #33778 ) ;
#38068 = CIRCLE ( 'NONE', #30118, 0.5000000000009441337 ) ;
#38069 = EDGE_LOOP ( 'NONE', ( #65911, #48767 ) ) ;
#38070 = CARTESIAN_POINT ( 'NONE',  ( 30.00000000000000000, -5.000000000000000000, -11.75000000000000000 ) ) ;
#38071 = CARTESIAN_POINT ( 'NONE',  ( 275.0000000000000000, 50.00000000000000000, -26.50000000000000000 ) ) ;
#38072 = AXIS2_PLACEMENT_3D ( 'NONE', #32214, #38560, #22304 ) ;
#38073 = CARTESIAN_POINT ( 'NONE',  ( 283.0000000000000568, -25.93000000000544958, 9.412893218815410634 ) ) ;
#38074 = VECTOR ( 'NONE', #12307, 1000.000000000000000 ) ;
#38075 = FACE_OUTER_BOUND ( 'NONE', #65207, .T. ) ;
#38076 = VERTEX_POINT ( 'NONE', #56983 ) ;
#38077 = LINE ( 'NONE', #11861, #61438 ) ;
#38078 = CARTESIAN_POINT ( 'NONE',  ( 7.250000000000005329, -7.249999999999998224, -26.00000000000001066 ) ) ;
#38079 = DIRECTION ( 'NONE',  ( -1.000000000000000000, 0.000000000000000000, 0.000000000000000000 ) ) ;
#38080 = AXIS2_PLACEMENT_3D ( 'NONE', #55416, #7297, #6955 ) ;
#38081 = CARTESIAN_POINT ( 'NONE',  ( 11.50000000000000000, -11.50000000000000000, 19.00000000000000000 ) ) ;
#38082 = FACE_OUTER_BOUND ( 'NONE', #21553, .T. ) ;
#38083 = DIRECTION ( 'NONE',  ( -0.000000000000000000, -0.000000000000000000, -1.000000000000000000 ) ) ;
#38084 = ORIENTED_EDGE ( 'NONE', *, *, #28225, .F. ) ;
#38085 = VECTOR ( 'NONE', #42379, 1000.000000000000000 ) ;
#38086 = ORIENTED_EDGE ( 'NONE', *, *, #64646, .F. ) ;
#38087 = LINE ( 'NONE', #59639, #13501 ) ;
#38088 = PLANE ( 'NONE',  #63944 ) ;
#38089 = ORIENTED_EDGE ( 'NONE', *, *, #45409, .F. ) ;
#38090 = FACE_BOUND ( 'NONE', #19706, .T. ) ;
#38091 = VERTEX_POINT ( 'NONE', #8543 ) ;
#38092 = DIRECTION ( 'NONE',  ( 1.000000000000000000, -0.000000000000000000, -0.000000000000000000 ) ) ;
#38093 = VERTEX_POINT ( 'NONE', #30123 ) ;
#38094 = ORIENTED_EDGE ( 'NONE', *, *, #52518, .F. ) ;
#38095 = CARTESIAN_POINT ( 'NONE',  ( 8.250000000000005329, -8.249999999999998224, -26.00000000000001066 ) ) ;
#38096 = ORIENTED_EDGE ( 'NONE', *, *, #36412, .T. ) ;
#38097 = PLANE ( 'NONE',  #36538 ) ;
#38098 = EDGE_CURVE ( 'NONE', #50834, #1029, #3252, .T. ) ;
#38099 = DIRECTION ( 'NONE',  ( -1.836970198721029934E-16, -1.836970198721010706E-16, 1.000000000000000000 ) ) ;
#38100 = CYLINDRICAL_SURFACE ( 'NONE', #58471, 0.5999999999999998668 ) ;
#38101 = ORIENTED_EDGE ( 'NONE', *, *, #63883, .F. ) ;
#38102 = ORIENTED_EDGE ( 'NONE', *, *, #26047, .F. ) ;
#38103 = EDGE_CURVE ( 'NONE', #3732, #8019, #55488, .T. ) ;
#38104 = DIRECTION ( 'NONE',  ( 1.000000000000000000, -0.000000000000000000, 0.000000000000000000 ) ) ;
#38106 = CARTESIAN_POINT ( 'NONE',  ( 7.250000000000005329, 8.250000000000001776, -25.50000000000000355 ) ) ;
#38105 = CARTESIAN_POINT ( 'NONE',  ( 7.272650909786644746, 7.798499376343933420, 455.0000000000000568 ) ) ;
#38107 = ORIENTED_EDGE ( 'NONE', *, *, #65871, .T. ) ;
#38108 = EDGE_CURVE ( 'NONE', #27679, #41539, #55144, .T. ) ;
#38109 = ORIENTED_EDGE ( 'NONE', *, *, #44894, .F. ) ;
#38111 = EDGE_LOOP ( 'NONE', ( #28205, #34624, #13522, #24494 ) ) ;
#38110 = ITEM_DEFINED_TRANSFORMATION ( 'NONE', 'NONE', #22265,  #45918 ) ;
#38112 = VECTOR ( 'NONE', #69601, 1000.000000000000000 ) ;
#38113 = VECTOR ( 'NONE', #57165, 1000.000000000000000 ) ;
#38114 = VECTOR ( 'NONE', #45840, 1000.000000000000000 ) ;
#38115 = EDGE_CURVE ( 'NONE', #30238, #65126, #2055, .T. ) ;
#38116 = EDGE_CURVE ( 'NONE', #40247, #39974, #60425, .T. ) ;
#38117 = CARTESIAN_POINT ( 'NONE',  ( 40.90000000000000568, 0.000000000000000000, 5.250000000000000000 ) ) ;
#38119 = EDGE_LOOP ( 'NONE', ( #42210, #43676 ) ) ;
#38118 = CARTESIAN_POINT ( 'NONE',  ( -17.00000000000000000, -15.50000000000000000, -19.33772233983200195 ) ) ;
#38120 = AXIS2_PLACEMENT_3D ( 'NONE', #58854, #157, #10411 ) ;
#38121 = VECTOR ( 'NONE', #38710, 1000.000000000000000 ) ;
#38122 = CARTESIAN_POINT ( 'NONE',  ( 2.632023737882809744, -6.501044194225465311, 26.00000000000000711 ) ) ;
#38123 = FACE_OUTER_BOUND ( 'NONE', #57697, .T. ) ;
#38124 = ORIENTED_EDGE ( 'NONE', *, *, #18363, .F. ) ;
#38125 = ORIENTED_EDGE ( 'NONE', *, *, #23078, .F. ) ;
#38126 = CIRCLE ( 'NONE', #39206, 24.99999999998789946 ) ;
#38127 = VECTOR ( 'NONE', #26090, 1000.000000000000000 ) ;
#38128 = DIRECTION ( 'NONE',  ( 8.359604446858500663E-15, 1.000000000000000000, 3.673940397442059868E-16 ) ) ;
#38129 = ORIENTED_EDGE ( 'NONE', *, *, #31727, .T. ) ;
#38130 = DIRECTION ( 'NONE',  ( 1.000000000000000000, -0.000000000000000000, -0.000000000000000000 ) ) ;
#38131 = DIRECTION ( 'NONE',  ( 0.000000000000000000, 0.000000000000000000, 1.000000000000000000 ) ) ;
#38132 = ORIENTED_EDGE ( 'NONE', *, *, #3619, .T. ) ;
#38133 = AXIS2_PLACEMENT_3D ( 'NONE', #65278, #28124, #37354 ) ;
#38134 = LINE ( 'NONE', #11232, #18855 ) ;
#38136 = ORIENTED_EDGE ( 'NONE', *, *, #15164, .F. ) ;
#38135 = CARTESIAN_POINT ( 'NONE',  ( 7.000000000000000000, -25.93000000000544958, -9.412893218815410634 ) ) ;
#38137 = ORIENTED_EDGE ( 'NONE', *, *, #12904, .T. ) ;
#38138 = CARTESIAN_POINT ( 'NONE',  ( 37.90000000000000568, 13.66939075806899240, -20.79999999999999361 ) ) ;
#38139 = LINE ( 'NONE', #59690, #60087 ) ;
#38140 = PLANE ( 'NONE',  #62898 ) ;
#38141 = CARTESIAN_POINT ( 'NONE',  ( -2.893516549646780511, -10.92648345035340895, 195.0000000000000284 ) ) ;
#38142 = DIRECTION ( 'NONE',  ( 0.000000000000000000, 0.000000000000000000, -1.000000000000000000 ) ) ;
#38143 = ORIENTED_EDGE ( 'NONE', *, *, #52974, .F. ) ;
#38144 = CARTESIAN_POINT ( 'NONE',  ( 30.00000000000000000, -5.000000000000000000, -27.00000000000000000 ) ) ;
#38145 = DIRECTION ( 'NONE',  ( -0.5000000000000067724, -0.8660254037844345998, 0.000000000000000000 ) ) ;
#38146 = CARTESIAN_POINT ( 'NONE',  ( 30.90000000000000213, -0.2000000000089119934, -8.913009219568841313E-12 ) ) ;
#38148 = ORIENTED_EDGE ( 'NONE', *, *, #24968, .F. ) ;
#38147 = CARTESIAN_POINT ( 'NONE',  ( 7.806483450353418618, 11.11351654964657421, 455.0000000000000568 ) ) ;
#38149 = ADVANCED_FACE ( 'NONE', ( #11982 ), #23639, .T. ) ;
#38150 =( NAMED_UNIT ( * ) SI_UNIT ( $, .STERADIAN. ) SOLID_ANGLE_UNIT ( ) );
#38151 = VECTOR ( 'NONE', #29425, 1000.000000000000000 ) ;
#38152 = DIRECTION ( 'NONE',  ( -1.836970198721029934E-16, -1.836970198721010706E-16, 1.000000000000000000 ) ) ;
#38153 = EDGE_CURVE ( 'NONE', #11172, #45635, #17856, .T. ) ;
#38154 = LINE ( 'NONE', #66390, #60109 ) ;
#38155 = CYLINDRICAL_SURFACE ( 'NONE', #54450, 24.99999999998789946 ) ;
#38156 = ORIENTED_EDGE ( 'NONE', *, *, #18194, .F. ) ;
#38157 = CARTESIAN_POINT ( 'NONE',  ( 7.000000000000000000, -38.64999999999999858, 15.00000000000000000 ) ) ;
#38158 = CARTESIAN_POINT ( 'NONE',  ( -15.50000000000000000, -0.2000000000000000111, 25.79999999999947136 ) ) ;
#38159 = ORIENTED_EDGE ( 'NONE', *, *, #26347, .T. ) ;
#38160 = FACE_OUTER_BOUND ( 'NONE', #2604, .T. ) ;
#38161 = DIRECTION ( 'NONE',  ( -0.000000000000000000, -0.000000000000000000, -1.000000000000000000 ) ) ;
#38162 = CARTESIAN_POINT ( 'NONE',  ( 41.09999999999999432, 20.60000000000000142, -13.86939075806900057 ) ) ;
#38163 = CARTESIAN_POINT ( 'NONE',  ( -8.250000000000001776, -7.249999999999998224, -17.00000000000000000 ) ) ;
#38164 = VECTOR ( 'NONE', #64426, 1000.000000000000000 ) ;
#38166 = DIRECTION ( 'NONE',  ( 1.000000000000000000, 0.000000000000000000, 0.000000000000000000 ) ) ;
#38165 = VECTOR ( 'NONE', #34080, 1000.000000000000000 ) ;
#38167 = ORIENTED_EDGE ( 'NONE', *, *, #44793, .T. ) ;
#38168 = ORIENTED_EDGE ( 'NONE', *, *, #9925, .T. ) ;
#38169 = CARTESIAN_POINT ( 'NONE',  ( -1.677516549646676625, 10.73351654964656987, 455.0000000000000568 ) ) ;
#38170 = ORIENTED_EDGE ( 'NONE', *, *, #28881, .F. ) ;
#38171 = CARTESIAN_POINT ( 'NONE',  ( 30.00000000000000000, -8.959999999999999076, -17.04524521594300523 ) ) ;
#38173 = ADVANCED_FACE ( 'NONE', ( #55827 ), #65069, .F. ) ;
#38172 = AXIS2_PLACEMENT_3D ( 'NONE', #26210, #9597, #52751 ) ;
#38174 = ORIENTED_EDGE ( 'NONE', *, *, #47677, .T. ) ;
#38175 = CARTESIAN_POINT ( 'NONE',  ( -11.11351654964671098, 4.193516549646605363, 455.0000000000000568 ) ) ;
#38176 = AXIS2_PLACEMENT_3D ( 'NONE', #50988, #13155, #62290 ) ;
#38177 = FACE_OUTER_BOUND ( 'NONE', #50781, .T. ) ;
#38178 = CARTESIAN_POINT ( 'NONE',  ( 275.0000000000000000, -32.44999999999905071, 14.49999999999906031 ) ) ;
#38179 = ORIENTED_EDGE ( 'NONE', *, *, #52161, .T. ) ;
#38180 = APPLICATION_CONTEXT ( 'automotive_design' ) ;
#38181 = ORIENTED_EDGE ( 'NONE', *, *, #69219, .F. ) ;
#38182 = DIRECTION ( 'NONE',  ( -1.000000000000000000, 0.000000000000000000, 0.000000000000000000 ) ) ;
#38183 = VERTEX_POINT ( 'NONE', #59752 ) ;
#38184 = ORIENTED_EDGE ( 'NONE', *, *, #67048, .F. ) ;
#38185 = CIRCLE ( 'NONE', #16729, 0.5000000000004306555 ) ;
#38186 = EDGE_CURVE ( 'NONE', #28620, #14583, #61114, .T. ) ;
#38187 = LINE ( 'NONE', #33881, #42839 ) ;
#38188 = DIRECTION ( 'NONE',  ( 0.7671651518153106419, -0.6414496315691445849, 0.000000000000000000 ) ) ;
#38189 = DIRECTION ( 'NONE',  ( 1.836970198721029934E-16, 1.836970198721010706E-16, -1.000000000000000000 ) ) ;
#38190 = VERTEX_POINT ( 'NONE', #22952 ) ;
#38191 = LINE ( 'NONE', #43824, #2979 ) ;
#38193 = CARTESIAN_POINT ( 'NONE',  ( 2.706483450353343478, -10.92648345035346225, 455.0000000000000568 ) ) ;
#38192 = FACE_OUTER_BOUND ( 'NONE', #56276, .T. ) ;
#38194 = VERTEX_POINT ( 'NONE', #65411 ) ;
#38195 = ORIENTED_EDGE ( 'NONE', *, *, #55805, .F. ) ;
#38197 = ORIENTED_EDGE ( 'NONE', *, *, #30643, .T. ) ;
#38196 = LINE ( 'NONE', #43829, #22940 ) ;
#38198 = ADVANCED_FACE ( 'NONE', ( #54795 ), #33569, .F. ) ;
#38199 = ORIENTED_EDGE ( 'NONE', *, *, #40277, .F. ) ;
#38200 = EDGE_CURVE ( 'NONE', #13993, #36263, #12191, .T. ) ;
#38201 = EDGE_CURVE ( 'NONE', #59852, #3061, #49830, .T. ) ;
#38202 = EDGE_CURVE ( 'NONE', #66963, #54936, #35933, .T. ) ;
#38203 = DIRECTION ( 'NONE',  ( -1.836970198721029934E-16, 1.836970198721036590E-16, -1.000000000000000000 ) ) ;
#38204 = LINE ( 'NONE', #23301, #6562 ) ;
#38205 = EDGE_CURVE ( 'NONE', #12098, #57808, #38204, .T. ) ;
#38206 = VECTOR ( 'NONE', #20221, 1000.000000000000000 ) ;
#38207 = VERTEX_POINT ( 'NONE', #6359 ) ;
#38208 = ORIENTED_EDGE ( 'NONE', *, *, #16289, .T. ) ;
#38209 = DIRECTION ( 'NONE',  ( -0.7071067811865500152, -0.7071067811865451302, 4.361490581750786694E-31 ) ) ;
#38210 = DIRECTION ( 'NONE',  ( 0.000000000000000000, 0.000000000000000000, 1.000000000000000000 ) ) ;
#38211 = EDGE_LOOP ( 'NONE', ( #58825, #12651, #31376, #18247 ) ) ;
#38212 = CARTESIAN_POINT ( 'NONE',  ( -30.00000000000000000, -5.000000000000000000, -27.00000000000000000 ) ) ;
#38213 = CARTESIAN_POINT ( 'NONE',  ( 11.12648345035338160, 4.193516549646526315, 455.0000000000000568 ) ) ;
#38214 = FACE_OUTER_BOUND ( 'NONE', #35122, .T. ) ;
#38215 = ORIENTED_EDGE ( 'NONE', *, *, #29215, .T. ) ;
#38216 = VECTOR ( 'NONE', #57981, 1000.000000000000000 ) ;
#38217 = DIRECTION ( 'NONE',  ( -1.000000000000000000, 0.000000000000000000, 0.000000000000000000 ) ) ;
#38218 = DIRECTION ( 'NONE',  ( 1.836970198721029934E-16, 1.836970198721010706E-16, -1.000000000000000000 ) ) ;
#38220 = ORIENTED_EDGE ( 'NONE', *, *, #9114, .F. ) ;
#38219 = DIRECTION ( 'NONE',  ( -1.000000000000000000, 0.000000000000000000, 0.000000000000000000 ) ) ;
#38222 = VERTEX_POINT ( 'NONE', #11303 ) ;
#38221 = CARTESIAN_POINT ( 'NONE',  ( 6.358413763958946419, 4.706725378239151603, 54.00000000000000711 ) ) ;
#38223 = DIRECTION ( 'NONE',  ( 0.000000000000000000, 0.000000000000000000, -1.000000000000000000 ) ) ;
#38224 = AXIS2_PLACEMENT_3D ( 'NONE', #39550, #16634, #716 ) ;
#38225 = DIRECTION ( 'NONE',  ( -0.000000000000000000, -0.000000000000000000, 1.000000000000000000 ) ) ;
#38226 = DIRECTION ( 'NONE',  ( 0.8660254037844485886, 0.000000000000000000, -0.4999999999999827360 ) ) ;
#38227 = DIRECTION ( 'NONE',  ( 0.000000000000000000, 0.000000000000000000, 1.000000000000000000 ) ) ;
#38228 = LINE ( 'NONE', #50194, #9085 ) ;
#38229 = DIRECTION ( 'NONE',  ( -0.000000000000000000, -0.000000000000000000, -1.000000000000000000 ) ) ;
#38230 = VERTEX_POINT ( 'NONE', #28259 ) ;
#38231 = DIRECTION ( 'NONE',  ( -0.7071067811865474617, 0.7071067811865474617, -0.000000000000000000 ) ) ;
#38233 = EDGE_LOOP ( 'NONE', ( #38262, #3000 ) ) ;
#38232 = DIRECTION ( 'NONE',  ( 0.000000000000000000, 1.000000000000000000, 0.000000000000000000 ) ) ;
#38234 = CIRCLE ( 'NONE', #979, 3.499999999999054534 ) ;
#38236 = ORIENTED_EDGE ( 'NONE', *, *, #38584, .T. ) ;
#38235 = PLANE ( 'NONE',  #40039 ) ;
#38237 = EDGE_CURVE ( 'NONE', #30268, #17336, #6689, .T. ) ;
#38238 = CARTESIAN_POINT ( 'NONE',  ( -7.798499376344067535, 4.727349090213367688, 455.0000000000000568 ) ) ;
#38239 = EDGE_CURVE ( 'NONE', #29684, #7626, #32879, .T. ) ;
#38240 = ORIENTED_EDGE ( 'NONE', *, *, #45489, .F. ) ;
#38241 = CARTESIAN_POINT ( 'NONE',  ( -7.450000000000001954, -7.249999999999998224, -16.50000000000000000 ) ) ;
#38242 = DIRECTION ( 'NONE',  ( 0.000000000000000000, 0.000000000000000000, -1.000000000000000000 ) ) ;
#38244 = VERTEX_POINT ( 'NONE', #6008 ) ;
#38243 = EDGE_CURVE ( 'NONE', #41058, #59828, #22284, .T. ) ;
#38245 = CARTESIAN_POINT ( 'NONE',  ( 49.00000000000000000, -0.2000000000089119934, -8.913009219568841313E-12 ) ) ;
#38246 = CARTESIAN_POINT ( 'NONE',  ( 15.00000000000000000, -25.60000000000000142, -17.60000000000000142 ) ) ;
#38247 = DIRECTION ( 'NONE',  ( 0.000000000000000000, 0.000000000000000000, -1.000000000000000000 ) ) ;
#38248 = DIRECTION ( 'NONE',  ( -0.4999999999989361843, 0.000000000000000000, -0.8660254037850529940 ) ) ;
#38249 = ORIENTED_EDGE ( 'NONE', *, *, #7935, .T. ) ;
#38250 = CARTESIAN_POINT ( 'NONE',  ( 0.000000000000000000, 8.250000000000001776, -24.50000000000000000 ) ) ;
#38251 = ORIENTED_EDGE ( 'NONE', *, *, #61545, .F. ) ;
#38252 = ORIENTED_EDGE ( 'NONE', *, *, #31428, .F. ) ;
#38253 = PLANE ( 'NONE',  #33600 ) ;
#38254 = CARTESIAN_POINT ( 'NONE',  ( 0.000000000000000000, 0.000000000000000000, 0.000000000000000000 ) ) ;
#38255 = AXIS2_PLACEMENT_3D ( 'NONE', #44071, #37739, #65316 ) ;
#38256 = FACE_OUTER_BOUND ( 'NONE', #22837, .T. ) ;
#38257 = FACE_OUTER_BOUND ( 'NONE', #66925, .T. ) ;
#38258 = ORIENTED_EDGE ( 'NONE', *, *, #52744, .F. ) ;
#38259 = ORIENTED_EDGE ( 'NONE', *, *, #17169, .T. ) ;
#38261 = ORIENTED_EDGE ( 'NONE', *, *, #33394, .T. ) ;
#38260 = FACE_OUTER_BOUND ( 'NONE', #8002, .T. ) ;
#38262 = ORIENTED_EDGE ( 'NONE', *, *, #58516, .T. ) ;
#38263 = VECTOR ( 'NONE', #30154, 1000.000000000000000 ) ;
#38264 = CARTESIAN_POINT ( 'NONE',  ( 11.08848345035334404, -9.804883450353528929, 455.0000000000000568 ) ) ;
#38265 = DIRECTION ( 'NONE',  ( 0.7071067811865550112, 0.7071067811865401342, 2.597868168706466299E-16 ) ) ;
#38266 = CYLINDRICAL_SURFACE ( 'NONE', #43254, 0.2000000000000005107 ) ;
#38267 = VECTOR ( 'NONE', #18533, 1000.000000000000000 ) ;
#38268 = DIRECTION ( 'NONE',  ( -5.981805089575196197E-17, -1.000000000000000000, 0.000000000000000000 ) ) ;
#38270 = LINE ( 'NONE', #44940, #50362 ) ;
#38269 = CARTESIAN_POINT ( 'NONE',  ( 10.50702373788281996, -6.849523737882823760, 54.00000000000000711 ) ) ;
#38271 = ORIENTED_EDGE ( 'NONE', *, *, #55995, .F. ) ;
#38273 = ORIENTED_EDGE ( 'NONE', *, *, #10390, .T. ) ;
#38272 = CARTESIAN_POINT ( 'NONE',  ( -24.00000000000000000, -15.50000000000000000, -14.50000000000000000 ) ) ;
#38274 = ORIENTED_EDGE ( 'NONE', *, *, #36177, .F. ) ;
#38275 = ORIENTED_EDGE ( 'NONE', *, *, #55539, .F. ) ;
#38276 = LINE ( 'NONE', #37582, #26564 ) ;
#38277 = ADVANCED_FACE ( 'NONE', ( #27924 ), #27572, .T. ) ;
#38278 = CARTESIAN_POINT ( 'NONE',  ( 283.0000000000000568, -25.60000000000000142, -15.10000000000000142 ) ) ;
#38279 = EDGE_CURVE ( 'NONE', #11521, #65734, #46260, .T. ) ;
#38280 = AXIS2_PLACEMENT_3D ( 'NONE', #64930, #48666, #44372 ) ;
#38281 = CARTESIAN_POINT ( 'NONE',  ( 11.78648345035337819, -4.406483450353490205, 455.0000000000000568 ) ) ;
#38282 = EDGE_CURVE ( 'NONE', #6090, #190, #21262, .T. ) ;
#38283 = ORIENTED_EDGE ( 'NONE', *, *, #27172, .T. ) ;
#38284 = EDGE_LOOP ( 'NONE', ( #14192, #57001, #53409, #12527 ) ) ;
#38285 = EDGE_CURVE ( 'NONE', #32488, #18662, #67498, .T. ) ;
#38286 = ORIENTED_EDGE ( 'NONE', *, *, #66895, .F. ) ;
#38287 = LINE ( 'NONE', #11058, #64439 ) ;
#38288 = LINE ( 'NONE', #37594, #51227 ) ;
#38289 = EDGE_CURVE ( 'NONE', #31253, #23277, #40257, .T. ) ;
#38290 = CARTESIAN_POINT ( 'NONE',  ( 18.89999999999999858, 13.66939075806899240, 20.79999999999999361 ) ) ;
#38291 = VERTEX_POINT ( 'NONE', #50858 ) ;
#38292 = ORIENTED_EDGE ( 'NONE', *, *, #51138, .F. ) ;
#38293 = PLANE ( 'NONE',  #14738 ) ;
#38294 = EDGE_CURVE ( 'NONE', #49868, #11985, #34598, .T. ) ;
#38295 = DIRECTION ( 'NONE',  ( 3.717264591378875951E-15, 1.000000000000000000, 0.000000000000000000 ) ) ;
#38297 = ORIENTED_EDGE ( 'NONE', *, *, #45715, .F. ) ;
#38296 = EDGE_CURVE ( 'NONE', #46689, #56785, #30710, .T. ) ;
#38298 = DIRECTION ( 'NONE',  ( 1.836970198721029934E-16, 1.836970198721010706E-16, -1.000000000000000000 ) ) ;
#38300 = ORIENTED_EDGE ( 'NONE', *, *, #45853, .T. ) ;
#38299 = CARTESIAN_POINT ( 'NONE',  ( 30.00000000000000000, -12.00000000000000000, 10.20500000000000007 ) ) ;
#38301 = VERTEX_POINT ( 'NONE', #36003 ) ;
#38302 = DIRECTION ( 'NONE',  ( 3.491481338843133355E-15, 1.000000000000000000, 0.000000000000000000 ) ) ;
#38303 = DIRECTION ( 'NONE',  ( -1.000000000000000000, 1.047444401652940007E-14, -1.836970198721010706E-16 ) ) ;
#38304 = LINE ( 'NONE', #69790, #25015 ) ;
#38305 = CARTESIAN_POINT ( 'NONE',  ( 15.50000000000000000, -0.2038245569916604938, 23.94337567297399971 ) ) ;
#38306 = AXIS2_PLACEMENT_3D ( 'NONE', #62408, #41908, #19998 ) ;
#38307 = PLANE ( 'NONE',  #10156 ) ;
#38308 = VERTEX_POINT ( 'NONE', #56181 ) ;
#38309 = CARTESIAN_POINT ( 'NONE',  ( 7.450000000000006395, 7.250000000000000888, -17.50000000000000000 ) ) ;
#38310 = AXIS2_PLACEMENT_3D ( 'NONE', #55209, #55551, #1123 ) ;
#38311 = ORIENTED_EDGE ( 'NONE', *, *, #8105, .T. ) ;
#38312 = CARTESIAN_POINT ( 'NONE',  ( 26.90000000000000213, 13.66939075806899240, 20.79999999999999361 ) ) ;
#38313 = CARTESIAN_POINT ( 'NONE',  ( 283.0000000000000568, -38.09999999999885034, 7.900000000002049383 ) ) ;
#38314 = DIRECTION ( 'NONE',  ( -1.000000000000000000, 0.000000000000000000, 0.000000000000000000 ) ) ;
#38315 = CARTESIAN_POINT ( 'NONE',  ( -8.593516549646711411, 4.383466043307770121, 195.0000000000000284 ) ) ;
#38316 = CIRCLE ( 'NONE', #7793, 1.000000000000000000 ) ;
#38317 = CARTESIAN_POINT ( 'NONE',  ( 7.265214908726123078, -6.619341603356865278, 195.0000000000000284 ) ) ;
#38319 = ORIENTED_EDGE ( 'NONE', *, *, #6413, .F. ) ;
#38318 = EDGE_CURVE ( 'NONE', #20859, #40401, #43855, .T. ) ;
#38320 = VECTOR ( 'NONE', #18256, 1000.000000000000000 ) ;
#38321 = CARTESIAN_POINT ( 'NONE',  ( 7.250000000000005329, 7.250000000000000888, -26.00000000000001066 ) ) ;
#38322 = CARTESIAN_POINT ( 'NONE',  ( 3.003254798005738468, 6.858227778582820733, 26.00000000000000711 ) ) ;
#38324 = CIRCLE ( 'NONE', #7760, 2.000000000000001776 ) ;
#38323 = AXIS2_PLACEMENT_3D ( 'NONE', #46476, #53211, #19601 ) ;
#38325 = ORIENTED_EDGE ( 'NONE', *, *, #19552, .T. ) ;
#38326 = DIRECTION ( 'NONE',  ( 0.000000000000000000, 0.000000000000000000, 1.000000000000000000 ) ) ;
#38327 = DIRECTION ( 'NONE',  ( 1.000000000000000000, -0.000000000000000000, -0.000000000000000000 ) ) ;
#38328 = EDGE_LOOP ( 'NONE', ( #8838, #27282, #6205, #1730, #10309, #10886, #18388, #36171 ) ) ;
#38329 = PLANE ( 'NONE',  #50505 ) ;
#38330 = VECTOR ( 'NONE', #6385, 1000.000000000000000 ) ;
#38331 = CARTESIAN_POINT ( 'NONE',  ( -7.450000000000001954, 0.000000000000000000, -17.50000000000000000 ) ) ;
#38333 = EDGE_LOOP ( 'NONE', ( #28022, #22583, #65729, #66884 ) ) ;
#38332 = ADVANCED_FACE ( 'NONE', ( #57574 ), #29643, .F. ) ;
#38334 = CARTESIAN_POINT ( 'NONE',  ( 275.0000000000000000, -25.60000000000000142, 17.60000000000000142 ) ) ;
#38335 = CARTESIAN_POINT ( 'NONE',  ( 4.961189459950039904, -7.357023737882811609, 26.00000000000000000 ) ) ;
#38336 = LINE ( 'NONE', #59888, #26405 ) ;
#38337 = ADVANCED_FACE ( 'NONE', ( #45204 ), #24347, .F. ) ;
#38338 = CARTESIAN_POINT ( 'NONE',  ( -7.250000000000000888, 8.250000000000001776, -26.00000000000001066 ) ) ;
#38339 = ORIENTED_EDGE ( 'NONE', *, *, #5179, .F. ) ;
#38341 = VERTEX_POINT ( 'NONE', #39889 ) ;
#38340 = DIRECTION ( 'NONE',  ( 0.000000000000000000, -0.000000000000000000, 1.000000000000000000 ) ) ;
#38342 = DIRECTION ( 'NONE',  ( 1.000000000000000000, -0.000000000000000000, -0.000000000000000000 ) ) ;
#38343 = CARTESIAN_POINT ( 'NONE',  ( 41.09999999999999432, -14.06939075806900163, 20.80000000000000426 ) ) ;
#38344 = CARTESIAN_POINT ( 'NONE',  ( -25.50000000000000355, -15.50000000000000000, -22.50000000000000000 ) ) ;
#38345 = EDGE_LOOP ( 'NONE', ( #8089, #66493, #55481, #68097 ) ) ;
#38346 = CARTESIAN_POINT ( 'NONE',  ( 181.4833316329832940, 0.000000000000000000, 316.5239988703752942 ) ) ;
#38347 = CARTESIAN_POINT ( 'NONE',  ( 13.00000000000000178, -17.50000000000000000, -15.70500000000000007 ) ) ;
#38348 = ORIENTED_EDGE ( 'NONE', *, *, #44426, .T. ) ;
#38349 = VERTEX_POINT ( 'NONE', #40606 ) ;
#38350 = EDGE_CURVE ( 'NONE', #24784, #60224, #31463, .T. ) ;
#38351 = ORIENTED_EDGE ( 'NONE', *, *, #26, .T. ) ;
#38352 = LINE ( 'NONE', #6170, #8415 ) ;
#38353 = CYLINDRICAL_SURFACE ( 'NONE', #49012, 24.99999999998789946 ) ;
#38354 = VECTOR ( 'NONE', #22507, 1000.000000000000000 ) ;
#38355 = VECTOR ( 'NONE', #32534, 1000.000000000000000 ) ;
#38356 = PLANE ( 'NONE',  #63124 ) ;
#38357 = ADVANCED_FACE ( 'NONE', ( #62166 ), #13731, .F. ) ;
#38358 = ORIENTED_EDGE ( 'NONE', *, *, #32377, .T. ) ;
#38359 = VERTEX_POINT ( 'NONE', #61461 ) ;
#38360 = ORIENTED_EDGE ( 'NONE', *, *, #32304, .F. ) ;
#38361 = DIRECTION ( 'NONE',  ( 3.491481338843132961E-15, 1.000000000000000000, 1.836970198721029934E-16 ) ) ;
#38362 = ORIENTED_EDGE ( 'NONE', *, *, #36019, .F. ) ;
#38363 = EDGE_CURVE ( 'NONE', #43836, #66768, #23989, .T. ) ;
#38364 = VERTEX_POINT ( 'NONE', #7722 ) ;
#38365 = ORIENTED_EDGE ( 'NONE', *, *, #2545, .T. ) ;
#38366 = AXIS2_PLACEMENT_3D ( 'NONE', #33949, #22334, #12031 ) ;
#38367 = ORIENTED_EDGE ( 'NONE', *, *, #14636, .F. ) ;
#38368 = CARTESIAN_POINT ( 'NONE',  ( -7.250000000000000888, 7.250000000000001776, -22.00000000000000000 ) ) ;
#38369 = EDGE_CURVE ( 'NONE', #6104, #26651, #8788, .T. ) ;
#38371 = ORIENTED_EDGE ( 'NONE', *, *, #27708, .F. ) ;
#38370 = CARTESIAN_POINT ( 'NONE',  ( 10.09643294401448621, 2.893516549646583780, 195.0000000000000284 ) ) ;
#38372 = EDGE_CURVE ( 'NONE', #57112, #18754, #11100, .T. ) ;
#38373 = VECTOR ( 'NONE', #49014, 1000.000000000000000 ) ;
#38374 = CYLINDRICAL_SURFACE ( 'NONE', #45872, 0.4999999999945534124 ) ;
#38375 = CARTESIAN_POINT ( 'NONE',  ( 152.0064834503532722, -29.01119750012554732, 5.000000000000000000 ) ) ;
#38376 = DIRECTION ( 'NONE',  ( 0.000000000000000000, 0.000000000000000000, 1.000000000000000000 ) ) ;
#38377 = EDGE_LOOP ( 'NONE', ( #12167, #36775, #43331, #31400 ) ) ;
#38378 = VECTOR ( 'NONE', #34583, 1000.000000000000000 ) ;
#38379 = CARTESIAN_POINT ( 'NONE',  ( 4.155633711806649977, 4.706725378239165813, 26.00000000000000711 ) ) ;
#38380 = ORIENTED_EDGE ( 'NONE', *, *, #68385, .T. ) ;
#38381 = DIRECTION ( 'NONE',  ( 0.000000000000000000, 1.000000000000000000, 0.000000000000000000 ) ) ;
#38382 = DIRECTION ( 'NONE',  ( 1.000000000000000000, 0.000000000000000000, 0.000000000000000000 ) ) ;
#38383 = DIRECTION ( 'NONE',  ( -1.000000000000000000, 3.491481338843133355E-15, 1.836970198721036344E-16 ) ) ;
#38384 = CARTESIAN_POINT ( 'NONE',  ( 41.09999999999999432, 20.60000000000000142, 13.86939075806900057 ) ) ;
#38385 = CIRCLE ( 'NONE', #39498, 2.250000000000001776 ) ;
#38386 = EDGE_CURVE ( 'NONE', #9129, #58645, #50612, .T. ) ;
#38387 = ORIENTED_EDGE ( 'NONE', *, *, #47417, .F. ) ;
#38388 = LINE ( 'NONE', #33760, #47152 ) ;
#38389 = DIRECTION ( 'NONE',  ( 0.000000000000000000, 0.000000000000000000, 1.000000000000000000 ) ) ;
#38390 = CARTESIAN_POINT ( 'NONE',  ( -30.00000000000000000, -17.50000000000000000, 15.70500000000000007 ) ) ;
#38391 = EDGE_CURVE ( 'NONE', #3700, #21874, #57226, .T. ) ;
#38392 = DIRECTION ( 'NONE',  ( -0.000000000000000000, -0.000000000000000000, 1.000000000000000000 ) ) ;
#38393 = LINE ( 'NONE', #64923, #60695 ) ;
#38394 = DIRECTION ( 'NONE',  ( 1.000000000000000000, -8.359604446858499085E-15, 0.000000000000000000 ) ) ;
#38395 = AXIS2_PLACEMENT_3D ( 'NONE', #28075, #49632, #22761 ) ;
#38396 = PLANE ( 'NONE',  #28766 ) ;
#38397 = VECTOR ( 'NONE', #42340, 1000.000000000000000 ) ;
#38398 = EDGE_CURVE ( 'NONE', #2080, #48487, #67145, .T. ) ;
#38399 = DIRECTION ( 'NONE',  ( 0.000000000000000000, 1.000000000000000000, 3.673940397442059868E-16 ) ) ;
#38400 = AXIS2_PLACEMENT_3D ( 'NONE', #21447, #10488, #20399 ) ;
#38401 = ORIENTED_EDGE ( 'NONE', *, *, #4612, .F. ) ;
#38402 = CARTESIAN_POINT ( 'NONE',  ( 7.450000000000004619, -1.336933437520057563E-15, -19.00000000000000000 ) ) ;
#38403 = LINE ( 'NONE', #27788, #19524 ) ;
#38404 = EDGE_CURVE ( 'NONE', #4079, #16582, #14098, .T. ) ;
#38405 = CARTESIAN_POINT ( 'NONE',  ( 283.0000000000000568, -20.85424868893542438, -17.35424868893542438 ) ) ;
#38406 = DIRECTION ( 'NONE',  ( -1.000000000000000000, 0.000000000000000000, 0.000000000000000000 ) ) ;
#38407 = EDGE_LOOP ( 'NONE', ( #62327, #6604, #55749, #925 ) ) ;
#38408 = CYLINDRICAL_SURFACE ( 'NONE', #2753, 0.4000000000000600298 ) ;
#38409 = CARTESIAN_POINT ( 'NONE',  ( -11.00000000000000000, -12.00000000000000000, 10.20500000000000007 ) ) ;
#38410 = LINE ( 'NONE', #27450, #44682 ) ;
#38411 = VECTOR ( 'NONE', #32506, 1000.000000000000000 ) ;
#38412 = DIRECTION ( 'NONE',  ( -1.000000000000000000, 0.000000000000000000, 0.000000000000000000 ) ) ;
#38413 = EDGE_CURVE ( 'NONE', #35695, #1141, #29305, .T. ) ;
#38414 = LINE ( 'NONE', #16148, #65564 ) ;
#38415 = VECTOR ( 'NONE', #55323, 1000.000000000000000 ) ;
#38416 = ORIENTED_EDGE ( 'NONE', *, *, #38961, .F. ) ;
#38417 = AXIS2_PLACEMENT_3D ( 'NONE', #43269, #59542, #27367 ) ;
#38418 = ORIENTED_EDGE ( 'NONE', *, *, #60101, .F. ) ;
#38419 = CARTESIAN_POINT ( 'NONE',  ( 176.0064834503533575, -29.01119750012555443, 0.000000000000000000 ) ) ;
#38420 = CARTESIAN_POINT ( 'NONE',  ( -5.380658396643234198, 4.734785091273867152, 455.0000000000000568 ) ) ;
#38422 = ORIENTED_EDGE ( 'NONE', *, *, #9214, .T. ) ;
#38421 = ADVANCED_FACE ( 'NONE', ( #51943 ), #8434, .F. ) ;
#38423 = EDGE_CURVE ( 'NONE', #16156, #34744, #40967, .T. ) ;
#38424 = CIRCLE ( 'NONE', #23, 24.99999999998794920 ) ;
#38425 = AXIS2_PLACEMENT_3D ( 'NONE', #48281, #57475, #9038 ) ;
#38426 = FACE_OUTER_BOUND ( 'NONE', #26032, .T. ) ;
#38427 = EDGE_CURVE ( 'NONE', #55973, #21406, #7739, .T. ) ;
#38428 = ORIENTED_EDGE ( 'NONE', *, *, #34155, .T. ) ;
#38429 = EDGE_CURVE ( 'NONE', #47767, #24680, #62531, .T. ) ;
#38430 = EDGE_CURVE ( 'NONE', #13935, #39920, #2444, .T. ) ;
#38431 = LINE ( 'NONE', #11196, #25498 ) ;
#38432 = ORIENTED_EDGE ( 'NONE', *, *, #44613, .T. ) ;
#38433 = ORIENTED_EDGE ( 'NONE', *, *, #34639, .F. ) ;
#38434 = DIRECTION ( 'NONE',  ( 0.7071067811865447972, -0.7071067811865502373, 0.000000000000000000 ) ) ;
#38435 = EDGE_LOOP ( 'NONE', ( #6475, #12036, #60167, #62499 ) ) ;
#38436 = DIRECTION ( 'NONE',  ( 1.000000000000000000, -8.612436249475772606E-15, -1.836970198721045958E-16 ) ) ;
#38437 = EDGE_CURVE ( 'NONE', #26706, #53994, #1869, .T. ) ;
#38438 = CARTESIAN_POINT ( 'NONE',  ( 11.78648345035337996, 4.173516549646518747, 455.0000000000000568 ) ) ;
#38439 = LINE ( 'NONE', #605, #14441 ) ;
#38440 = CIRCLE ( 'NONE', #26030, 2.285366197183106074 ) ;
#38441 = EDGE_CURVE ( 'NONE', #10108, #38244, #45568, .T. ) ;
#38442 = ORIENTED_EDGE ( 'NONE', *, *, #26767, .F. ) ;
#38443 = ORIENTED_EDGE ( 'NONE', *, *, #51742, .T. ) ;
#38444 = FACE_OUTER_BOUND ( 'NONE', #61903, .T. ) ;
#38445 = EDGE_CURVE ( 'NONE', #51774, #64699, #68199, .T. ) ;
#38446 = DIRECTION ( 'NONE',  ( -1.836970198721029934E-16, 1.836970198721036590E-16, -1.000000000000000000 ) ) ;
#38447 = ORIENTED_EDGE ( 'NONE', *, *, #34637, .T. ) ;
#38448 = ORIENTED_EDGE ( 'NONE', *, *, #46201, .F. ) ;
#38450 = VERTEX_POINT ( 'NONE', #40275 ) ;
#38449 = CONTEXT_DEPENDENT_SHAPE_REPRESENTATION ( #3360, #5278 ) ;
#38451 = CARTESIAN_POINT ( 'NONE',  ( 39.90000000000000568, -16.96999999999999886, -21.00000000000000000 ) ) ;
#38452 = EDGE_CURVE ( 'NONE', #3816, #30867, #46070, .T. ) ;
#38453 = AXIS2_PLACEMENT_3D ( 'NONE', #22292, #13032, #56190 ) ;
#38455 = EDGE_LOOP ( 'NONE', ( #28593, #60883, #32636, #15722 ) ) ;
#38454 = CARTESIAN_POINT ( 'NONE',  ( -8.250000000000001776, -8.249999999999998224, -26.00000000000001066 ) ) ;
#38456 = ADVANCED_FACE ( 'NONE', ( #29656 ), #3156, .F. ) ;
#38457 = DIRECTION ( 'NONE',  ( -1.000000000000000000, 0.000000000000000000, 0.000000000000000000 ) ) ;
#38458 = AXIS2_PLACEMENT_3D ( 'NONE', #34461, #24583, #46484 ) ;
#38459 = DIRECTION ( 'NONE',  ( -3.304235192336773145E-15, -1.000000000000000000, 0.000000000000000000 ) ) ;
#38460 = ORIENTED_EDGE ( 'NONE', *, *, #23954, .F. ) ;
#38461 = ORIENTED_EDGE ( 'NONE', *, *, #21127, .T. ) ;
#38462 = EDGE_CURVE ( 'NONE', #56867, #6649, #45933, .T. ) ;
#38463 = EDGE_LOOP ( 'NONE', ( #47925, #31567, #2541, #14360 ) ) ;
#38464 = VECTOR ( 'NONE', #62754, 1000.000000000000000 ) ;
#38465 = CARTESIAN_POINT ( 'NONE',  ( -4.193516549646785663, -11.32648345035339510, 195.0000000000000284 ) ) ;
#38466 = DIRECTION ( 'NONE',  ( -1.000000000000000000, 0.000000000000000000, 0.000000000000000000 ) ) ;
#38467 = AXIS2_PLACEMENT_3D ( 'NONE', #55577, #16725, #55236 ) ;
#38468 = ORIENTED_EDGE ( 'NONE', *, *, #37544, .T. ) ;
#38469 = DIRECTION ( 'NONE',  ( 0.000000000000000000, -1.000000000000000000, 0.000000000000000000 ) ) ;
#38470 = DIRECTION ( 'NONE',  ( 0.000000000000000000, -5.800915303574361727E-12, -1.000000000000000000 ) ) ;
#38471 = ORIENTED_EDGE ( 'NONE', *, *, #4771, .F. ) ;
#38472 = VERTEX_POINT ( 'NONE', #62183 ) ;
#38473 = FACE_OUTER_BOUND ( 'NONE', #43154, .T. ) ;
#38474 = VECTOR ( 'NONE', #52387, 1000.000000000000000 ) ;
#38475 = AXIS2_PLACEMENT_3D ( 'NONE', #49329, #22447, #16095 ) ;
#38476 = CARTESIAN_POINT ( 'NONE',  ( -4.135079735113167843, 6.822336235477362010, 54.00000000000000711 ) ) ;
#38477 = CARTESIAN_POINT ( 'NONE',  ( 30.00000000000000000, -17.14999999999900027, 26.64999999999900027 ) ) ;
#38478 = CARTESIAN_POINT ( 'NONE',  ( -2.993516549646701108, 7.415254214038204061, 195.0000000000000284 ) ) ;
#38479 = DIRECTION ( 'NONE',  ( 0.000000000000000000, 3.673940397442059868E-16, -1.000000000000000000 ) ) ;
#38480 = VERTEX_POINT ( 'NONE', #12687 ) ;
#38481 = DIRECTION ( 'NONE',  ( 0.000000000000000000, -0.7071067811865495711, -0.7071067811865455743 ) ) ;
#38482 = LINE ( 'NONE', #23241, #4547 ) ;
#38483 = CARTESIAN_POINT ( 'NONE',  ( 21.90000000000000213, -21.00000000000000000, 13.86939075806900057 ) ) ;
#38484 = EDGE_CURVE ( 'NONE', #48107, #60085, #33656, .T. ) ;
#38485 = CARTESIAN_POINT ( 'NONE',  ( -9.547976262117300550, -7.969523737882755476, 26.00000000000000000 ) ) ;
#38486 = AXIS2_PLACEMENT_3D ( 'NONE', #59674, #23215, #44768 ) ;
#38487 = CARTESIAN_POINT ( 'NONE',  ( -4.734785091274035018, -6.619341603356897252, 455.0000000000000568 ) ) ;
#38488 = PLANE ( 'NONE',  #28503 ) ;
#38489 = ADVANCED_FACE ( 'NONE', ( #30371 ), #24716, .F. ) ;
#38490 = CARTESIAN_POINT ( 'NONE',  ( -8.000000000000000000, 7.281754163448145079, 0.000000000000000000 ) ) ;
#38491 = ORIENTED_EDGE ( 'NONE', *, *, #22569, .F. ) ;
#38492 = CARTESIAN_POINT ( 'NONE',  ( -15.29633693294650421, -0.2717122460102743275, 21.17420925361331641 ) ) ;
#38493 = EDGE_CURVE ( 'NONE', #38006, #53395, #55164, .T. ) ;
#38494 = DIRECTION ( 'NONE',  ( 0.000000000000000000, -1.000000000000000000, 0.000000000000000000 ) ) ;
#38495 = ORIENTED_EDGE ( 'NONE', *, *, #11335, .F. ) ;
#38496 = DIRECTION ( 'NONE',  ( -0.5000000000000019984, -0.8660254037844375974, -0.000000000000000000 ) ) ;
#38497 = PLANE ( 'NONE',  #44630 ) ;
#38498 = DIRECTION ( 'NONE',  ( 0.000000000000000000, 0.000000000000000000, -1.000000000000000000 ) ) ;
#38499 = DIRECTION ( 'NONE',  ( 1.836970198721029934E-16, 1.836970198721010706E-16, -1.000000000000000000 ) ) ;
#38500 = ADVANCED_FACE ( 'NONE', ( #7390, #28968 ), #59937, .T. ) ;
#38501 = CARTESIAN_POINT ( 'NONE',  ( 16.89194109070750116, -5.000000000000000000, -26.25000000000000000 ) ) ;
#38502 = CARTESIAN_POINT ( 'NONE',  ( 283.0000000000000568, -32.00000000000000000, -8.400000000000000355 ) ) ;
#38503 = VECTOR ( 'NONE', #56274, 1000.000000000000000 ) ;
#38504 = ORIENTED_EDGE ( 'NONE', *, *, #50653, .T. ) ;
#38505 = CARTESIAN_POINT ( 'NONE',  ( 16.54686605390242349, -0.2715358723599884394, -23.33896727494797929 ) ) ;
#38506 = CARTESIAN_POINT ( 'NONE',  ( -8.250000000000001776, 0.000000000000000000, -7.500000000000000000 ) ) ;
#38507 = EDGE_LOOP ( 'NONE', ( #12987, #15137, #37580, #63400 ) ) ;
#38508 = VECTOR ( 'NONE', #65449, 1000.000000000000000 ) ;
#38509 = CARTESIAN_POINT ( 'NONE',  ( -11.00000000000000000, -8.959999999999999076, 17.04524521594300523 ) ) ;
#38510 = CIRCLE ( 'NONE', #33991, 1.399999999999998579 ) ;
#38511 = EDGE_CURVE ( 'NONE', #1369, #2916, #22474, .T. ) ;
#38512 = AXIS2_PLACEMENT_3D ( 'NONE', #41988, #14056, #57547 ) ;
#38513 = LINE ( 'NONE', #11953, #51372 ) ;
#38514 = LINE ( 'NONE', #49803, #11826 ) ;
#38515 = ORIENTED_EDGE ( 'NONE', *, *, #27131, .F. ) ;
#38516 = ORIENTED_EDGE ( 'NONE', *, *, #46961, .F. ) ;
#38517 = FACE_OUTER_BOUND ( 'NONE', #14455, .T. ) ;
#38518 = ORIENTED_EDGE ( 'NONE', *, *, #29936, .F. ) ;
#38519 = AXIS2_PLACEMENT_3D ( 'NONE', #61970, #23094, #61612 ) ;
#38520 = EDGE_LOOP ( 'NONE', ( #36862, #2589, #29282, #54848 ) ) ;
#38521 = CARTESIAN_POINT ( 'NONE',  ( -8.916576262117345664, -8.580623737882765667, 54.00000000000000711 ) ) ;
#38522 = DIRECTION ( 'NONE',  ( -0.000000000000000000, -0.000000000000000000, -1.000000000000000000 ) ) ;
#38523 = CARTESIAN_POINT ( 'NONE',  ( -30.00000000000000000, -15.97213595500069871, 14.50000000000000000 ) ) ;
#38524 = ORIENTED_EDGE ( 'NONE', *, *, #45682, .T. ) ;
#38525 = DIRECTION ( 'NONE',  ( 1.836970198721029934E-16, 1.836970198721010706E-16, -1.000000000000000000 ) ) ;
#38526 = VECTOR ( 'NONE', #51425, 1000.000000000000000 ) ;
#38528 = CARTESIAN_POINT ( 'NONE',  ( -7.839518282750262301, 3.417780618358531530, 195.0000000000000284 ) ) ;
#38527 = DIRECTION ( 'NONE',  ( 0.000000000000000000, 1.000000000000000000, 0.000000000000000000 ) ) ;
#38529 = ORIENTED_EDGE ( 'NONE', *, *, #30829, .T. ) ;
#38530 = ORIENTED_EDGE ( 'NONE', *, *, #66570, .F. ) ;
#38532 = ORIENTED_EDGE ( 'NONE', *, *, #55502, .T. ) ;
#38531 = DIRECTION ( 'NONE',  ( 0.000000000000000000, -0.1249999999999996531, -0.9921567416492215186 ) ) ;
#38533 = ORIENTED_EDGE ( 'NONE', *, *, #56616, .F. ) ;
#38534 = CARTESIAN_POINT ( 'NONE',  ( 33.89999999999999858, -21.00000000000001421, -13.86939075806900945 ) ) ;
#38535 = EDGE_CURVE ( 'NONE', #15450, #17979, #10053, .T. ) ;
#38536 = EDGE_CURVE ( 'NONE', #52304, #69570, #60799, .T. ) ;
#38537 = CARTESIAN_POINT ( 'NONE',  ( 13.00000000000000178, -16.28999999999710369, -15.00000000000794920 ) ) ;
#38538 = AXIS2_PLACEMENT_3D ( 'NONE', #10110, #59240, #4118 ) ;
#38539 = ORIENTED_EDGE ( 'NONE', *, *, #46969, .T. ) ;
#38541 = ORIENTED_EDGE ( 'NONE', *, *, #3612, .F. ) ;
#38540 = ADVANCED_FACE ( 'NONE', ( #46981 ), #65267, .F. ) ;
#38542 = LINE ( 'NONE', #16272, #22206 ) ;
#38543 = DIRECTION ( 'NONE',  ( 0.000000000000000000, 0.000000000000000000, 1.000000000000000000 ) ) ;
#38544 = EDGE_LOOP ( 'NONE', ( #22878, #14216 ) ) ;
#38545 = CARTESIAN_POINT ( 'NONE',  ( -25.50000000000000355, -15.50000000000000000, -22.50000000000000000 ) ) ;
#38546 = CARTESIAN_POINT ( 'NONE',  ( -9.293516549646710700, 10.08346604330776941, 455.0000000000000568 ) ) ;
#38547 = DIRECTION ( 'NONE',  ( -0.4285714285711681448, 0.000000000000000000, -0.9035079029053748600 ) ) ;
#38548 = CIRCLE ( 'NONE', #61124, 1.224999999999999423 ) ;
#38549 = EDGE_LOOP ( 'NONE', ( #59316, #30010 ) ) ;
#38550 = VECTOR ( 'NONE', #69785, 1000.000000000000000 ) ;
#38551 = CARTESIAN_POINT ( 'NONE',  ( 7.000000000000000000, -26.28355339059299922, -9.766446609406699508 ) ) ;
#38552 = LINE ( 'NONE', #22969, #64458 ) ;
#38554 = VERTEX_POINT ( 'NONE', #21417 ) ;
#38553 = CARTESIAN_POINT ( 'NONE',  ( 10.31889768521804207, -20.65270074880752560, 17.15270074880752560 ) ) ;
#38556 = ORIENTED_EDGE ( 'NONE', *, *, #24133, .T. ) ;
#38555 = DIRECTION ( 'NONE',  ( 0.000000000000000000, 0.000000000000000000, 1.000000000000000000 ) ) ;
#38557 = PLANE ( 'NONE',  #23461 ) ;
#38558 = DIRECTION ( 'NONE',  ( 0.000000000000000000, 0.7278708115913746779, -0.6857142857147672244 ) ) ;
#38559 = FACE_OUTER_BOUND ( 'NONE', #2603, .T. ) ;
#38560 = DIRECTION ( 'NONE',  ( 1.000000000000000000, -0.000000000000000000, 0.000000000000000000 ) ) ;
#38561 = CIRCLE ( 'NONE', #27316, 0.1999999999999987899 ) ;
#38562 = VECTOR ( 'NONE', #50424, 1000.000000000000000 ) ;
#38563 = CARTESIAN_POINT ( 'NONE',  ( 29.50000000000000355, -11.50000000000100009, 15.00000000000084910 ) ) ;
#38564 = LINE ( 'NONE', #60117, #29256 ) ;
#38565 = VERTEX_POINT ( 'NONE', #42983 ) ;
#38566 = CARTESIAN_POINT ( 'NONE',  ( -30.00000000000000000, -5.000000000000000000, -27.00000000000000000 ) ) ;
#38568 = EDGE_LOOP ( 'NONE', ( #33990, #10858, #49231, #2949 ) ) ;
#38567 = CARTESIAN_POINT ( 'NONE',  ( 39.90000000000000568, 21.00000000000000000, 16.96999999999999886 ) ) ;
#38569 = EDGE_CURVE ( 'NONE', #41911, #51508, #43688, .T. ) ;
#38571 = VERTEX_POINT ( 'NONE', #64907 ) ;
#38570 = CARTESIAN_POINT ( 'NONE',  ( 282.6457513110646005, -25.50000000000000355, 17.00000000000000000 ) ) ;
#38572 = DIRECTION ( 'NONE',  ( 3.540251991789403884E-15, 1.000000000000000000, 0.000000000000000000 ) ) ;
#38573 = EDGE_CURVE ( 'NONE', #52657, #52369, #27422, .T. ) ;
#38574 = AXIS2_PLACEMENT_3D ( 'NONE', #25533, #51337, #57346 ) ;
#38575 = EDGE_LOOP ( 'NONE', ( #48469, #30199, #9161, #23910 ) ) ;
#38576 = LINE ( 'NONE', #60127, #2656 ) ;
#38577 = EDGE_CURVE ( 'NONE', #20791, #35525, #20115, .T. ) ;
#38578 = CARTESIAN_POINT ( 'NONE',  ( 30.00000000000000000, -5.000000000000000000, 27.00000000000000000 ) ) ;
#38579 = EDGE_CURVE ( 'NONE', #43775, #20610, #36369, .T. ) ;
#38580 = ORIENTED_EDGE ( 'NONE', *, *, #27289, .F. ) ;
#38581 = DIRECTION ( 'NONE',  ( -1.000000000000000000, 3.491481338843133355E-15, 1.836970198721036344E-16 ) ) ;
#38582 = CARTESIAN_POINT ( 'NONE',  ( -11.31351654964671027, 7.593516549646603941, 195.0000000000000284 ) ) ;
#38583 = CARTESIAN_POINT ( 'NONE',  ( 8.250000000000005329, 7.250000000000000888, -26.00000000000001066 ) ) ;
#38584 = EDGE_CURVE ( 'NONE', #11628, #35155, #14813, .T. ) ;
#38585 = EDGE_CURVE ( 'NONE', #22259, #36931, #52655, .T. ) ;
#38586 = LINE ( 'NONE', #49193, #37264 ) ;
#38587 = DIRECTION ( 'NONE',  ( 1.000000000000000000, -0.000000000000000000, 0.000000000000000000 ) ) ;
#38588 = EDGE_CURVE ( 'NONE', #54361, #20807, #48406, .T. ) ;
#38589 = ORIENTED_EDGE ( 'NONE', *, *, #49293, .T. ) ;
#38590 = FACE_OUTER_BOUND ( 'NONE', #64886, .T. ) ;
#38591 = ORIENTED_EDGE ( 'NONE', *, *, #51408, .T. ) ;
#38592 = EDGE_LOOP ( 'NONE', ( #6273, #12830, #56832, #13162 ) ) ;
#38593 = FACE_OUTER_BOUND ( 'NONE', #19042, .T. ) ;
#38594 = DIRECTION ( 'NONE',  ( -0.7671651518153043137, 0.6414496315691521344, 2.587583378555129776E-16 ) ) ;
#38595 = CARTESIAN_POINT ( 'NONE',  ( 40.90000000000000568, 0.000000000000000000, 3.447897592003593022E-15 ) ) ;
#38596 = CARTESIAN_POINT ( 'NONE',  ( 10.20488345035338007, -11.48848345035349361, 455.0000000000000568 ) ) ;
#38597 = VERTEX_POINT ( 'NONE', #26732 ) ;
#38598 = ORIENTED_EDGE ( 'NONE', *, *, #289, .T. ) ;
#38599 = CIRCLE ( 'NONE', #2441, 0.5999999999999998668 ) ;
#38601 = ORIENTED_EDGE ( 'NONE', *, *, #38920, .F. ) ;
#38600 = DIRECTION ( 'NONE',  ( 0.000000000000000000, -1.000000000000000000, 0.000000000000000000 ) ) ;
#38602 = EDGE_LOOP ( 'NONE', ( #30785, #35714, #54271, #21645, #32640, #45560 ) ) ;
#38603 = AXIS2_PLACEMENT_3D ( 'NONE', #10291, #33243, #26910 ) ;
#38604 = CARTESIAN_POINT ( 'NONE',  ( 8.250000000000005329, -7.249999999999998224, -17.00000000000000000 ) ) ;
#38605 = LINE ( 'NONE', #37917, #64831 ) ;
#38606 = PLANE ( 'NONE',  #63604 ) ;
#38607 = CARTESIAN_POINT ( 'NONE',  ( 7.250000000000005329, 7.250000000000000888, -26.00000000000001066 ) ) ;
#38609 = CARTESIAN_POINT ( 'NONE',  ( 146.5599459900709860, 9.000000000000001776, 324.5239988703752942 ) ) ;
#38608 = DIRECTION ( 'NONE',  ( -1.000000000000000000, 2.602085213965213008E-15, 0.000000000000000000 ) ) ;
#38610 = ORIENTED_EDGE ( 'NONE', *, *, #54940, .F. ) ;
#38612 = VERTEX_POINT ( 'NONE', #37686 ) ;
#38611 = CARTESIAN_POINT ( 'NONE',  ( 25.50000000000000355, -15.50000000000000000, -22.50000000000000000 ) ) ;
#38613 = ORIENTED_EDGE ( 'NONE', *, *, #66491, .T. ) ;
#38614 = EDGE_LOOP ( 'NONE', ( #67593, #6399, #41792, #37231 ) ) ;
#38615 = CIRCLE ( 'NONE', #66854, 24.99999999998784972 ) ;
#38616 = CLOSED_SHELL ( 'NONE', ( #9412, #36322, #22863, #25965, #59949, #11522 ) ) ;
#38617 = CARTESIAN_POINT ( 'NONE',  ( 3.664523737882778853, -10.50702373788281285, 54.00000000000000711 ) ) ;
#38618 = DIRECTION ( 'NONE',  ( 0.000000000000000000, 1.000000000000000000, 0.000000000000000000 ) ) ;
#38619 = EDGE_CURVE ( 'NONE', #9955, #55205, #16813, .T. ) ;
#38620 = LINE ( 'NONE', #50255, #56817 ) ;
#38621 = DIRECTION ( 'NONE',  ( 0.000000000000000000, 0.000000000000000000, -1.000000000000000000 ) ) ;
#38622 = ORIENTED_EDGE ( 'NONE', *, *, #58314, .F. ) ;
#38623 = ORIENTED_EDGE ( 'NONE', *, *, #25503, .F. ) ;
#38624 = EDGE_CURVE ( 'NONE', #43288, #64892, #921, .T. ) ;
#38625 = EDGE_CURVE ( 'NONE', #65963, #66645, #32390, .T. ) ;
#38626 = AXIS2_PLACEMENT_3D ( 'NONE', #23677, #34632, #38908 ) ;
#38627 = CARTESIAN_POINT ( 'NONE',  ( 11.00000000000000000, -11.10796162543699950, 9.102987789146602893 ) ) ;
#38628 = FACE_OUTER_BOUND ( 'NONE', #69496, .T. ) ;
#38629 = EDGE_CURVE ( 'NONE', #40700, #25742, #55567, .T. ) ;
#38630 = ORIENTED_EDGE ( 'NONE', *, *, #40306, .F. ) ;
#38631 = ORIENTED_EDGE ( 'NONE', *, *, #11639, .F. ) ;
#38632 = CARTESIAN_POINT ( 'NONE',  ( 4.456444791733522252E-16, 7.450000000000002842, -8.500000000000000000 ) ) ;
#38633 = DIRECTION ( 'NONE',  ( 0.000000000000000000, 0.000000000000000000, -1.000000000000000000 ) ) ;
#38634 = ORIENTED_EDGE ( 'NONE', *, *, #65406, .T. ) ;
#38635 = LINE ( 'NONE', #60186, #55071 ) ;
#38637 = VERTEX_POINT ( 'NONE', #5515 ) ;
#38636 = CARTESIAN_POINT ( 'NONE',  ( 275.0000000000000000, -28.95000000000155183, 14.49999999999845990 ) ) ;
#38638 = ORIENTED_EDGE ( 'NONE', *, *, #64658, .F. ) ;
#38639 = CARTESIAN_POINT ( 'NONE',  ( 7.000000000000000000, -26.50000000000000000, -0.5000000000000000000 ) ) ;
#38640 = CARTESIAN_POINT ( 'NONE',  ( -8.821682069070829968, -8.144523737882765957, 54.00000000000000711 ) ) ;
#38641 = CARTESIAN_POINT ( 'NONE',  ( 9.750000000000001776, -9.690000000000001279, -5.000000000000000000 ) ) ;
#38642 = VECTOR ( 'NONE', #8738, 1000.000000000000000 ) ;
#38643 = CARTESIAN_POINT ( 'NONE',  ( 49.00000000000000000, 13.66939075806899950, 20.80000000000000426 ) ) ;
#38644 = PLANE ( 'NONE',  #14697 ) ;
#38645 = AXIS2_PLACEMENT_3D ( 'NONE', #56201, #2450, #9512 ) ;
#38646 = ORIENTED_EDGE ( 'NONE', *, *, #23597, .T. ) ;
#38647 = DIRECTION ( 'NONE',  ( -1.000000000000000000, 0.000000000000000000, 0.000000000000000000 ) ) ;
#38649 = ORIENTED_EDGE ( 'NONE', *, *, #12538, .F. ) ;
#38648 =( LENGTH_UNIT ( ) NAMED_UNIT ( * ) SI_UNIT ( .MILLI., .METRE. ) );
#38650 = ADVANCED_FACE ( 'NONE', ( #43328, #59603, #16471, #11151, #32721, #17847, #55341, #34431, #45402, #60276 ), #28115, .T. ) ;
#38651 = DIRECTION ( 'NONE',  ( 0.000000000000000000, 0.000000000000000000, -1.000000000000000000 ) ) ;
#38652 = CARTESIAN_POINT ( 'NONE',  ( -10.49297626211725998, 9.781776262117173104, 54.00000000000000711 ) ) ;
#38653 = CARTESIAN_POINT ( 'NONE',  ( 7.450000000000003730, -7.249999999999997335, -21.00000000000000000 ) ) ;
#38654 = CIRCLE ( 'NONE', #8141, 2.250000000000001776 ) ;
#38655 = DIRECTION ( 'NONE',  ( 0.000000000000000000, 0.4606534372016282686, -0.8875800869748744493 ) ) ;
#38656 = DIRECTION ( 'NONE',  ( 0.000000000000000000, 1.000000000000000000, 0.000000000000000000 ) ) ;
#38657 = ORIENTED_EDGE ( 'NONE', *, *, #13898, .T. ) ;
#38658 = AXIS2_PLACEMENT_3D ( 'NONE', #63476, #63121, #68780 ) ;
#38659 = EDGE_LOOP ( 'NONE', ( #44107, #3167, #8503, #56083 ) ) ;
#38660 = DIRECTION ( 'NONE',  ( 0.000000000000000000, 0.000000000000000000, -1.000000000000000000 ) ) ;
#38661 = EDGE_CURVE ( 'NONE', #31121, #19077, #17900, .T. ) ;
#38662 = CARTESIAN_POINT ( 'NONE',  ( 3.664523737882778853, -10.50702373788281285, 54.00000000000000711 ) ) ;
#38663 = CIRCLE ( 'NONE', #63510, 1.000000000000000888 ) ;
#38664 = ADVANCED_FACE ( 'NONE', ( #2625 ), #50016, .F. ) ;
#38665 = ORIENTED_EDGE ( 'NONE', *, *, #6641, .F. ) ;
#38666 = CYLINDRICAL_SURFACE ( 'NONE', #2268, 0.1999999999999987899 ) ;
#38667 = CARTESIAN_POINT ( 'NONE',  ( 7.000000000000000000, -40.30000000000000426, 12.20000000000000107 ) ) ;
#38668 = EDGE_LOOP ( 'NONE', ( #20792, #20428, #49470, #10592 ) ) ;
#38669 = AXIS2_PLACEMENT_3D ( 'NONE', #40551, #7675, #45502 ) ;
#38670 = CARTESIAN_POINT ( 'NONE',  ( -25.50000000000000355, -5.578999999999999737, 22.50000000000000000 ) ) ;
#38671 = LINE ( 'NONE', #65877, #16125 ) ;
#38672 = ORIENTED_EDGE ( 'NONE', *, *, #9695, .T. ) ;
#38673 = LINE ( 'NONE', #7864, #29950 ) ;
#38674 = PLANE ( 'NONE',  #31200 ) ;
#38675 = LINE ( 'NONE', #22073, #55762 ) ;
#38676 = CARTESIAN_POINT ( 'NONE',  ( 10.92648345035337520, -2.906483450353491094, 455.0000000000000568 ) ) ;
#38677 = ORIENTED_EDGE ( 'NONE', *, *, #16153, .T. ) ;
#38679 = VERTEX_POINT ( 'NONE', #7580 ) ;
#38678 = CARTESIAN_POINT ( 'NONE',  ( 283.0000000000000568, -21.00000000000000000, 12.50000000000000000 ) ) ;
#38680 = CARTESIAN_POINT ( 'NONE',  ( 7.250000000000005329, -8.249999999999998224, -21.00000000000000000 ) ) ;
#38681 = CARTESIAN_POINT ( 'NONE',  ( 14.66242688423474050, -0.3152598339554796292, -21.54019739087904384 ) ) ;
#38682 = CARTESIAN_POINT ( 'NONE',  ( 23.75054448485400016, -15.50000000000000000, 25.53140320652400064 ) ) ;
#38683 = VERTEX_POINT ( 'NONE', #6554 ) ;
#38684 = DIRECTION ( 'NONE',  ( -1.000000000000000000, 0.000000000000000000, 0.000000000000000000 ) ) ;
#38685 = DIRECTION ( 'NONE',  ( 0.000000000000000000, 1.000000000000000000, 0.000000000000000000 ) ) ;
#38686 = ORIENTED_EDGE ( 'NONE', *, *, #29215, .F. ) ;
#38687 = ORIENTED_EDGE ( 'NONE', *, *, #43811, .T. ) ;
#38688 = ORIENTED_EDGE ( 'NONE', *, *, #19561, .T. ) ;
#38689 = DIRECTION ( 'NONE',  ( -1.836970198721029934E-16, 1.836970198721036344E-16, -1.000000000000000000 ) ) ;
#38690 = VECTOR ( 'NONE', #54655, 1000.000000000000000 ) ;
#38691 = CARTESIAN_POINT ( 'NONE',  ( -3.834182069070819932, -7.532023737882814096, 26.00000000000000711 ) ) ;
#38692 = CARTESIAN_POINT ( 'NONE',  ( 7.450000000000003730, -7.249999999999997335, -13.50000000000000178 ) ) ;
#38693 = EDGE_LOOP ( 'NONE', ( #50837, #2437, #9571, #62857 ) ) ;
#38694 = ORIENTED_EDGE ( 'NONE', *, *, #1441, .F. ) ;
#38695 = ORIENTED_EDGE ( 'NONE', *, *, #8200, .F. ) ;
#38696 = VECTOR ( 'NONE', #37148, 1000.000000000000000 ) ;
#38697 = ADVANCED_FACE ( 'NONE', ( #55676 ), #49678, .F. ) ;
#38698 = DIRECTION ( 'NONE',  ( -0.000000000000000000, -0.000000000000000000, -1.000000000000000000 ) ) ;
#38699 = ORIENTED_EDGE ( 'NONE', *, *, #66486, .F. ) ;
#38700 = ORIENTED_EDGE ( 'NONE', *, *, #61055, .F. ) ;
#38701 = EDGE_CURVE ( 'NONE', #54414, #22866, #65596, .T. ) ;
#38702 = VERTEX_POINT ( 'NONE', #12867 ) ;
#38703 = VERTEX_POINT ( 'NONE', #61310 ) ;
#38704 = CARTESIAN_POINT ( 'NONE',  ( 10.74648345035329911, 1.077516549646576616, 195.0000000000000284 ) ) ;
#38706 = ORIENTED_EDGE ( 'NONE', *, *, #45193, .T. ) ;
#38705 = DIRECTION ( 'NONE',  ( -1.836970198721029934E-16, 1.836970198721036344E-16, -1.000000000000000000 ) ) ;
#38707 = CARTESIAN_POINT ( 'NONE',  ( -30.00000000000000000, -11.50000000000100009, 15.00000000000084910 ) ) ;
#38709 = CARTESIAN_POINT ( 'NONE',  ( -11.47551654964682122, -10.20488345035336941, 455.0000000000000568 ) ) ;
#38708 = CIRCLE ( 'NONE', #62368, 4.500000000000190958 ) ;
#38710 = DIRECTION ( 'NONE',  ( -1.000000000000000000, 0.000000000000000000, 0.000000000000000000 ) ) ;
#38711 = ORIENTED_EDGE ( 'NONE', *, *, #44824, .T. ) ;
#38712 = DIRECTION ( 'NONE',  ( -1.836970198721029934E-16, 1.836970198721036590E-16, -1.000000000000000000 ) ) ;
#38713 = DIRECTION ( 'NONE',  ( 0.000000000000000000, -0.7096009616570518874, 0.7046037717862339012 ) ) ;
#38714 = CARTESIAN_POINT ( 'NONE',  ( 78.77321854994620765, 47.95351654967443977, 15.00000000000000000 ) ) ;
#38715 = EDGE_CURVE ( 'NONE', #63302, #14096, #39067, .T. ) ;
#38716 = AXIS2_PLACEMENT_3D ( 'NONE', #55852, #61857, #28627 ) ;
#38717 = ORIENTED_EDGE ( 'NONE', *, *, #33935, .T. ) ;
#38718 = DIRECTION ( 'NONE',  ( 0.000000000000000000, 0.000000000000000000, -1.000000000000000000 ) ) ;
#38719 = DIRECTION ( 'NONE',  ( 1.836970198721029934E-16, 1.836970198721010706E-16, -1.000000000000000000 ) ) ;
#38720 = CARTESIAN_POINT ( 'NONE',  ( 30.00000000000000000, -9.200000000000120082, 17.30000000000000071 ) ) ;
#38721 = ORIENTED_EDGE ( 'NONE', *, *, #56919, .F. ) ;
#38722 = DIRECTION ( 'NONE',  ( -0.000000000000000000, -0.000000000000000000, -1.000000000000000000 ) ) ;
#38723 = CYLINDRICAL_SURFACE ( 'NONE', #17223, 24.99999999998789946 ) ;
#38724 = LINE ( 'NONE', #21779, #53977 ) ;
#38725 = VECTOR ( 'NONE', #39007, 1000.000000000000000 ) ;
#38726 = CYLINDRICAL_SURFACE ( 'NONE', #58006, 0.3499999999999614531 ) ;
#38727 = CARTESIAN_POINT ( 'NONE',  ( 7.000000000000000000, -26.50000000000000000, 5.530822723609939651 ) ) ;
#38728 = DIRECTION ( 'NONE',  ( 0.000000000000000000, 0.000000000000000000, -1.000000000000000000 ) ) ;
#38729 = VECTOR ( 'NONE', #29996, 1000.000000000000000 ) ;
#38730 = FACE_OUTER_BOUND ( 'NONE', #67970, .T. ) ;
#38731 = LINE ( 'NONE', #49694, #54868 ) ;
#38732 = ADVANCED_FACE ( 'NONE', ( #55005 ), #65927, .T. ) ;
#38733 = ADVANCED_FACE ( 'NONE', ( #7220 ), #1246, .F. ) ;
#38734 = ORIENTED_EDGE ( 'NONE', *, *, #44613, .F. ) ;
#38735 = CARTESIAN_POINT ( 'NONE',  ( -7.250000000000001776, -7.249999999999998224, -9.000000000000001776 ) ) ;
#38736 = EDGE_CURVE ( 'NONE', #60538, #58562, #61671, .T. ) ;
#38737 = CARTESIAN_POINT ( 'NONE',  ( -11.77351654964670935, 7.593516549646604830, 455.0000000000000568 ) ) ;
#38738 = AXIS2_PLACEMENT_3D ( 'NONE', #57215, #30701, #8411 ) ;
#38739 = CARTESIAN_POINT ( 'NONE',  ( 11.00000000000000000, -11.85423089348099879, -9.852125413066602277 ) ) ;
#38740 = CARTESIAN_POINT ( 'NONE',  ( -13.00000000000000178, -15.50000000000000000, -20.05051025721700242 ) ) ;
#38741 = VERTEX_POINT ( 'NONE', #33753 ) ;
#38742 = DIRECTION ( 'NONE',  ( -0.000000000000000000, -0.000000000000000000, -1.000000000000000000 ) ) ;
#38743 = DIRECTION ( 'NONE',  ( -0.6414496315691494699, -0.7671651518153064231, 0.000000000000000000 ) ) ;
#38744 = ADVANCED_FACE ( 'NONE', ( #44702 ), #40089, .T. ) ;
#38745 = DIRECTION ( 'NONE',  ( 0.000000000000000000, 0.000000000000000000, -1.000000000000000000 ) ) ;
#38746 = PRODUCT_DEFINITION ( 'UNKNOWN', '', #41430, #62146 ) ;
#38747 = ADVANCED_FACE ( 'NONE', ( #33422 ), #22807, .F. ) ;
#38748 = LINE ( 'NONE', #55037, #8312 ) ;
#38749 = ADVANCED_FACE ( 'NONE', ( #7921 ), #12528, .F. ) ;
#38750 = CARTESIAN_POINT ( 'NONE',  ( -4.173516549646790530, -11.78648345035339595, 195.0000000000000284 ) ) ;
#38751 = ORIENTED_EDGE ( 'NONE', *, *, #57305, .T. ) ;
#38752 = EDGE_CURVE ( 'NONE', #46347, #52260, #23501, .T. ) ;
#38753 = AXIS2_PLACEMENT_3D ( 'NONE', #13540, #24508, #36155 ) ;
#38754 = ORIENTED_EDGE ( 'NONE', *, *, #46625, .F. ) ;
#38755 = CARTESIAN_POINT ( 'NONE',  ( 10.00000000000000000, 21.00000000000000000, 18.00000000000000355 ) ) ;
#38756 = CYLINDRICAL_SURFACE ( 'NONE', #19859, 24.99999999998794920 ) ;
#38757 = ORIENTED_EDGE ( 'NONE', *, *, #16939, .F. ) ;
#38758 = CIRCLE ( 'NONE', #61298, 2.458500000000000796 ) ;
#38759 = VECTOR ( 'NONE', #55109, 1000.000000000000000 ) ;
#38760 = DIRECTION ( 'NONE',  ( 0.000000000000000000, 0.000000000000000000, 1.000000000000000000 ) ) ;
#38761 = VECTOR ( 'NONE', #48191, 1000.000000000000114 ) ;
#38762 = ORIENTED_EDGE ( 'NONE', *, *, #57755, .T. ) ;
#38763 = CARTESIAN_POINT ( 'NONE',  ( 24.90000000000000213, -0.2000000000089119934, 8.909539772616881237E-12 ) ) ;
#38765 = EDGE_LOOP ( 'NONE', ( #59917, #43037, #25936, #28614 ) ) ;
#38764 = AXIS2_PLACEMENT_3D ( 'NONE', #3852, #20117, #63251 ) ;
#38766 = CIRCLE ( 'NONE', #17308, 24.99999999998784972 ) ;
#38767 = ORIENTED_EDGE ( 'NONE', *, *, #66697, .T. ) ;
#38768 = FACE_OUTER_BOUND ( 'NONE', #21401, .T. ) ;
#38769 = EDGE_LOOP ( 'NONE', ( #16746, #27600, #7136, #58397 ) ) ;
#38770 = DIRECTION ( 'NONE',  ( 1.000000000000000000, -0.000000000000000000, 0.000000000000000000 ) ) ;
#38771 = PLANE ( 'NONE',  #15784 ) ;
#38772 = DIRECTION ( 'NONE',  ( 0.000000000000000000, 0.000000000000000000, 1.000000000000000000 ) ) ;
#38773 = EDGE_CURVE ( 'NONE', #33676, #38888, #67682, .T. ) ;
#38774 = ORIENTED_EDGE ( 'NONE', *, *, #12781, .F. ) ;
#38775 = ORIENTED_EDGE ( 'NONE', *, *, #49736, .F. ) ;
#38776 = CARTESIAN_POINT ( 'NONE',  ( -7.450000000000001954, -7.249999999999998224, -11.50000000000000000 ) ) ;
#38777 = CARTESIAN_POINT ( 'NONE',  ( -28.00000000000000000, -16.28999999999999915, -14.50000000000000000 ) ) ;
#38778 = ORIENTED_EDGE ( 'NONE', *, *, #22041, .T. ) ;
#38779 = VECTOR ( 'NONE', #49202, 1000.000000000000000 ) ;
#38780 = ORIENTED_EDGE ( 'NONE', *, *, #38816, .F. ) ;
#38781 = ORIENTED_EDGE ( 'NONE', *, *, #30352, .T. ) ;
#38782 = CARTESIAN_POINT ( 'NONE',  ( -11.00000000000000000, -14.04000000000000092, -17.04524521594300523 ) ) ;
#38784 = EDGE_LOOP ( 'NONE', ( #63602, #32546, #5751, #28993 ) ) ;
#38783 = CARTESIAN_POINT ( 'NONE',  ( 7.428221114744993692, 2.993516549646566105, 455.0000000000000568 ) ) ;
#38785 = DIRECTION ( 'NONE',  ( 0.7071067811865474617, 0.7071067811865474617, 2.597868168706479611E-16 ) ) ;
#38786 = CARTESIAN_POINT ( 'NONE',  ( -7.250000000000000888, 7.450000000000003730, -17.50000000000000000 ) ) ;
#38787 = ORIENTED_EDGE ( 'NONE', *, *, #57738, .F. ) ;
#38788 = ORIENTED_EDGE ( 'NONE', *, *, #45019, .T. ) ;
#38789 = AXIS2_PLACEMENT_3D ( 'NONE', #67357, #67697, #55694 ) ;
#38790 = CYLINDRICAL_SURFACE ( 'NONE', #59600, 0.8099999999999999423 ) ;
#38791 = CARTESIAN_POINT ( 'NONE',  ( -7.250000000000001776, -7.249999999999998224, -8.000000000000000000 ) ) ;
#38792 = EDGE_CURVE ( 'NONE', #50861, #35627, #69853, .T. ) ;
#38793 = VECTOR ( 'NONE', #57698, 1000.000000000000000 ) ;
#38794 = AXIS2_PLACEMENT_3D ( 'NONE', #56933, #30426, #19112 ) ;
#38795 = CARTESIAN_POINT ( 'NONE',  ( -3.417780618358626565, 7.839518282750134404, 195.0000000000000284 ) ) ;
#38796 = DIRECTION ( 'NONE',  ( -0.7071067811865500152, -0.7071067811865451302, 4.429638872090642462E-31 ) ) ;
#38797 = EDGE_CURVE ( 'NONE', #32155, #31478, #24674, .T. ) ;
#38799 = ORIENTED_EDGE ( 'NONE', *, *, #61365, .F. ) ;
#38798 = DIRECTION ( 'NONE',  ( 0.6414496315691645689, 0.7671651518152940996, 2.309356642088551915E-17 ) ) ;
#38800 = ORIENTED_EDGE ( 'NONE', *, *, #44269, .T. ) ;
#38801 = LINE ( 'NONE', #54735, #31748 ) ;
#38802 =( GEOMETRIC_REPRESENTATION_CONTEXT ( 3 ) GLOBAL_UNCERTAINTY_ASSIGNED_CONTEXT ( ( #46519 ) ) GLOBAL_UNIT_ASSIGNED_CONTEXT ( ( #57798, #52506, #4431 ) ) REPRESENTATION_CONTEXT ( 'NONE', 'WORKASPACE' ) );
#38804 = CIRCLE ( 'NONE', #7196, 0.1750000000000002387 ) ;
#38803 = CARTESIAN_POINT ( 'NONE',  ( 4.456444791733522252E-16, 7.450000000000002842, -10.50000000000000000 ) ) ;
#38805 = EDGE_CURVE ( 'NONE', #39788, #37177, #14527, .T. ) ;
#38806 = CARTESIAN_POINT ( 'NONE',  ( 289.5000000000000000, -0.5000000000000000000, 27.00000000000000000 ) ) ;
#38807 = EDGE_CURVE ( 'NONE', #24754, #49618, #30908, .T. ) ;
#38808 = DIRECTION ( 'NONE',  ( 0.7671651518153105309, -0.6414496315691445849, -0.000000000000000000 ) ) ;
#38809 = VECTOR ( 'NONE', #65607, 1000.000000000000000 ) ;
#38810 = CARTESIAN_POINT ( 'NONE',  ( 7.250000000000005329, 7.250000000000000888, -18.00000000000000000 ) ) ;
#38811 = EDGE_LOOP ( 'NONE', ( #47240, #35077, #22101, #55396 ) ) ;
#38812 = CARTESIAN_POINT ( 'NONE',  ( 4.456444791733522252E-16, 7.450000000000002842, -21.50000000000000000 ) ) ;
#38813 = DIRECTION ( 'NONE',  ( 1.000000000000000000, 0.000000000000000000, 0.000000000000000000 ) ) ;
#38814 = CARTESIAN_POINT ( 'NONE',  ( 30.00000000000000000, -17.00000000000000000, -15.70499999999969809 ) ) ;
#38815 = CARTESIAN_POINT ( 'NONE',  ( 25.57999999999999829, 0.000000000000000000, 2.458500000000000796 ) ) ;
#38816 = EDGE_CURVE ( 'NONE', #35394, #6695, #18897, .T. ) ;
#38817 = DIRECTION ( 'NONE',  ( 0.000000000000000000, -1.000000000000000000, 0.000000000000000000 ) ) ;
#38818 = CARTESIAN_POINT ( 'NONE',  ( 7.811466277050697293, 4.727349090213374794, 195.0000000000000284 ) ) ;
#38819 = FACE_OUTER_BOUND ( 'NONE', #36459, .T. ) ;
#38820 = ORIENTED_EDGE ( 'NONE', *, *, #10780, .F. ) ;
#38821 = DIRECTION ( 'NONE',  ( 0.000000000000000000, -1.000000000000000000, 0.000000000000000000 ) ) ;
#38822 = CARTESIAN_POINT ( 'NONE',  ( 280.0000000000000000, -53.81370849898476649, 20.00000000000000000 ) ) ;
#38823 = ORIENTED_EDGE ( 'NONE', *, *, #9207, .F. ) ;
#38824 = FACE_OUTER_BOUND ( 'NONE', #31222, .T. ) ;
#38825 = FACE_OUTER_BOUND ( 'NONE', #33648, .T. ) ;
#38826 = CARTESIAN_POINT ( 'NONE',  ( -7.813516549646791098, -12.00648345035336284, 195.0000000000000284 ) ) ;
#38827 = DIRECTION ( 'NONE',  ( 0.000000000000000000, 1.000000000000000000, 0.000000000000000000 ) ) ;
#38828 = EDGE_CURVE ( 'NONE', #6379, #4689, #63436, .T. ) ;
#38829 = DIRECTION ( 'NONE',  ( 1.000000000000000000, -8.802523127157697409E-15, 1.836970198721013910E-16 ) ) ;
#38830 = EDGE_CURVE ( 'NONE', #16718, #68045, #56720, .T. ) ;
#38831 = DIRECTION ( 'NONE',  ( 1.000000000000000000, -0.000000000000000000, 0.000000000000000000 ) ) ;
#38832 = ORIENTED_EDGE ( 'NONE', *, *, #47581, .T. ) ;
#38833 = CARTESIAN_POINT ( 'NONE',  ( 78.77321854994620765, 47.95351654967443977, 29.00000000000000000 ) ) ;
#38834 = ORIENTED_EDGE ( 'NONE', *, *, #15319, .T. ) ;
#38835 = CIRCLE ( 'NONE', #47879, 0.5000000000009406920 ) ;
#38836 = DIRECTION ( 'NONE',  ( -0.000000000000000000, 3.673940397442059868E-16, -1.000000000000000000 ) ) ;
#38837 = AXIS2_PLACEMENT_3D ( 'NONE', #36769, #15558, #19435 ) ;
#38838 = DIRECTION ( 'NONE',  ( 1.000000000000000000, -0.000000000000000000, 0.000000000000000000 ) ) ;
#38839 = LINE ( 'NONE', #60065, #17484 ) ;
#38840 = ORIENTED_EDGE ( 'NONE', *, *, #8092, .T. ) ;
#38841 = ORIENTED_EDGE ( 'NONE', *, *, #62602, .T. ) ;
#38842 = DIRECTION ( 'NONE',  ( 0.000000000000000000, -0.7046037717859445770, 0.7096009616573392131 ) ) ;
#38843 = ORIENTED_EDGE ( 'NONE', *, *, #35773, .T. ) ;
#38844 = ORIENTED_EDGE ( 'NONE', *, *, #37525, .F. ) ;
#38845 = PRODUCT_DEFINITION_CONTEXT ( 'detailed design', #53971, 'design' ) ;
#38846 = CARTESIAN_POINT ( 'NONE',  ( -1.620245201994301665, 8.227189898828640935, 54.00000000000000711 ) ) ;
#38847 = CARTESIAN_POINT ( 'NONE',  ( 14.25000000000000000, -2.500000000000000000, -21.77831216351300014 ) ) ;
#38848 = VECTOR ( 'NONE', #7678, 1000.000000000000000 ) ;
#38849 = AXIS2_PLACEMENT_3D ( 'NONE', #20342, #35539, #26011 ) ;
#38850 = CARTESIAN_POINT ( 'NONE',  ( 290.0000000000000000, -21.00000000000000000, -5.000000000000000000 ) ) ;
#38851 = ORIENTED_EDGE ( 'NONE', *, *, #49956, .F. ) ;
#38852 = DIRECTION ( 'NONE',  ( 0.000000000000000000, 0.000000000000000000, -1.000000000000000000 ) ) ;
#38854 = DIRECTION ( 'NONE',  ( 0.000000000000000000, 0.000000000000000000, -1.000000000000000000 ) ) ;
#38853 = DIRECTION ( 'NONE',  ( 0.000000000000000000, -1.000000000000000000, 0.000000000000000000 ) ) ;
#38855 = AXIS2_PLACEMENT_3D ( 'NONE', #55480, #34225, #65399 ) ;
#38856 = CIRCLE ( 'NONE', #3837, 2.000000000000001776 ) ;
#38858 = ORIENTED_EDGE ( 'NONE', *, *, #24453, .F. ) ;
#38857 = CIRCLE ( 'NONE', #32108, 0.3499999999999308664 ) ;
#38860 = VERTEX_POINT ( 'NONE', #25615 ) ;
#38859 = LINE ( 'NONE', #2074, #32004 ) ;
#38861 = ORIENTED_EDGE ( 'NONE', *, *, #51134, .T. ) ;
#38862 = B_SPLINE_CURVE_WITH_KNOTS ( 'NONE', 3,
 ( #7116, #39640, #6774, #44596, #28344, #28689 ),
 .UNSPECIFIED., .F., .F.,
 ( 4, 2, 4 ),
 ( 0.0002380763768129734448, 0.7291065797294589146, 1.457975083082104995 ),
 .UNSPECIFIED. ) ;
#38863 = EDGE_CURVE ( 'NONE', #11813, #23831, #47176, .T. ) ;
#38864 = DIRECTION ( 'NONE',  ( -0.000000000000000000, 3.673940397442059868E-16, -1.000000000000000000 ) ) ;
#38865 = EDGE_CURVE ( 'NONE', #48716, #5287, #40459, .T. ) ;
#38866 = CARTESIAN_POINT ( 'NONE',  ( 11.00000000000000000, -10.85999999999999943, 9.350000000000269651 ) ) ;
#38867 = AXIS2_PLACEMENT_3D ( 'NONE', #14013, #23930, #62096 ) ;
#38868 = ORIENTED_EDGE ( 'NONE', *, *, #2947, .F. ) ;
#38869 = ORIENTED_EDGE ( 'NONE', *, *, #34474, .F. ) ;
#38870 = EDGE_CURVE ( 'NONE', #36470, #58038, #40510, .T. ) ;
#38871 = AXIS2_PLACEMENT_3D ( 'NONE', #18061, #39964, #29028 ) ;
#38872 = FACE_OUTER_BOUND ( 'NONE', #29473, .T. ) ;
#38873 = EDGE_CURVE ( 'NONE', #56170, #10380, #13408, .T. ) ;
#38874 = DIRECTION ( 'NONE',  ( -0.000000000000000000, -0.000000000000000000, 1.000000000000000000 ) ) ;
#38875 = ORIENTED_EDGE ( 'NONE', *, *, #26487, .T. ) ;
#38876 = CARTESIAN_POINT ( 'NONE',  ( 9.737023737882765317, 2.530476262117151709, 54.00000000000000711 ) ) ;
#38877 = DIRECTION ( 'NONE',  ( 0.000000000000000000, -1.000000000000000000, 0.000000000000000000 ) ) ;
#38878 = EDGE_CURVE ( 'NONE', #34893, #18134, #56312, .T. ) ;
#38879 = CARTESIAN_POINT ( 'NONE',  ( -7.250000000000000888, 7.450000000000003730, -16.50000000000000000 ) ) ;
#38880 = ORIENTED_EDGE ( 'NONE', *, *, #20540, .T. ) ;
#38881 = CARTESIAN_POINT ( 'NONE',  ( -1.110223024625156540E-16, -42.00000000000000000, -26.50000000000000000 ) ) ;
#38882 = DIRECTION ( 'NONE',  ( -1.000000000000000000, 0.000000000000000000, 0.000000000000000000 ) ) ;
#38883 = EDGE_CURVE ( 'NONE', #44762, #63705, #4408, .T. ) ;
#38884 = CIRCLE ( 'NONE', #49088, 2.500000000000000000 ) ;
#38886 = ORIENTED_EDGE ( 'NONE', *, *, #30576, .F. ) ;
#38885 = CYLINDRICAL_SURFACE ( 'NONE', #40855, 1.000000000000000000 ) ;
#38888 = VERTEX_POINT ( 'NONE', #62719 ) ;
#38887 = LINE ( 'NONE', #60451, #36904 ) ;
#38889 = EDGE_CURVE ( 'NONE', #38703, #13736, #24555, .T. ) ;
#38890 = LINE ( 'NONE', #1079, #32516 ) ;
#38891 = CARTESIAN_POINT ( 'NONE',  ( 11.12648345035337627, -2.906483450353395614, 195.0000000000000284 ) ) ;
#38892 = CIRCLE ( 'NONE', #44529, 1.000000000000000000 ) ;
#38893 = LINE ( 'NONE', #32904, #56128 ) ;
#38894 = CARTESIAN_POINT ( 'NONE',  ( 289.5000000000000000, 0.000000000000000000, -26.50000000000000000 ) ) ;
#38895 = EDGE_CURVE ( 'NONE', #17706, #52264, #14300, .T. ) ;
#38896 = EDGE_CURVE ( 'NONE', #64033, #62061, #13936, .T. ) ;
#38897 = DIRECTION ( 'NONE',  ( 1.836970198721029934E-16, 1.836970198721010706E-16, -1.000000000000000000 ) ) ;
#38898 = CARTESIAN_POINT ( 'NONE',  ( -8.250000000000001776, -8.249999999999998224, -26.00000000000001066 ) ) ;
#38899 = ORIENTED_EDGE ( 'NONE', *, *, #55799, .F. ) ;
#38900 = LINE ( 'NONE', #33927, #6692 ) ;
#38901 = EDGE_CURVE ( 'NONE', #66616, #24826, #5553, .T. ) ;
#38902 = CARTESIAN_POINT ( 'NONE',  ( -8.000000000000000000, -8.000000000000000000, -1.000000000000000000 ) ) ;
#38904 = ORIENTED_EDGE ( 'NONE', *, *, #61716, .T. ) ;
#38903 = PLANE ( 'NONE',  #67162 ) ;
#38905 = AXIS2_PLACEMENT_3D ( 'NONE', #50736, #4071, #51446 ) ;
#38906 = VECTOR ( 'NONE', #52815, 1000.000000000000000 ) ;
#38907 = FILL_AREA_STYLE ('',( #31885 ) ) ;
#38908 = DIRECTION ( 'NONE',  ( -3.540251991789403884E-15, -1.000000000000000000, 0.000000000000000000 ) ) ;
#38909 = VECTOR ( 'NONE', #66490, 1000.000000000000000 ) ;
#38910 = CIRCLE ( 'NONE', #66001, 0.3499999999999597877 ) ;
#38911 = VERTEX_POINT ( 'NONE', #3684 ) ;
#38912 = LINE ( 'NONE', #22658, #67011 ) ;
#38913 = PLANE ( 'NONE',  #20429 ) ;
#38914 = ORIENTED_EDGE ( 'NONE', *, *, #63091, .T. ) ;
#38915 = DIRECTION ( 'NONE',  ( 0.000000000000000000, 0.000000000000000000, 1.000000000000000000 ) ) ;
#38916 = FACE_OUTER_BOUND ( 'NONE', #1930, .T. ) ;
#38917 =( NAMED_UNIT ( * ) SI_UNIT ( $, .STERADIAN. ) SOLID_ANGLE_UNIT ( ) );
#38918 = ADVANCED_FACE ( 'NONE', ( #25256 ), #46806, .T. ) ;
#38919 = DIRECTION ( 'NONE',  ( 0.000000000000000000, 0.000000000000000000, -1.000000000000000000 ) ) ;
#38920 = EDGE_CURVE ( 'NONE', #10709, #961, #3268, .T. ) ;
#38921 = LINE ( 'NONE', #66820, #24064 ) ;
#38922 = VECTOR ( 'NONE', #14114, 1000.000000000000114 ) ;
#38923 = VERTEX_POINT ( 'NONE', #10044 ) ;
#38924 = CARTESIAN_POINT ( 'NONE',  ( 20.90000000000000213, 13.66939075806899240, -20.79999999999999361 ) ) ;
#38925 = ORIENTED_EDGE ( 'NONE', *, *, #35834, .T. ) ;
#38926 = VERTEX_POINT ( 'NONE', #21696 ) ;
#38927 = VECTOR ( 'NONE', #35018, 1000.000000000000000 ) ;
#38928 = CARTESIAN_POINT ( 'NONE',  ( 8.406483450353379183, -4.396432944014657451, 455.0000000000000568 ) ) ;
#38929 = LINE ( 'NONE', #1112, #55254 ) ;
#38930 = CARTESIAN_POINT ( 'NONE',  ( 9.404523737882758638, 1.466476262117154983, 54.00000000000000711 ) ) ;
#38931 = CYLINDRICAL_SURFACE ( 'NONE', #25028, 0.5000000000000000000 ) ;
#38932 = ORIENTED_EDGE ( 'NONE', *, *, #62257, .F. ) ;
#38933 = ORIENTED_EDGE ( 'NONE', *, *, #27320, .F. ) ;
#38935 = ORIENTED_EDGE ( 'NONE', *, *, #11998, .T. ) ;
#38934 = DIRECTION ( 'NONE',  ( 0.000000000000000000, 0.000000000000000000, 1.000000000000000000 ) ) ;
#38936 = ORIENTED_EDGE ( 'NONE', *, *, #53804, .F. ) ;
#38937 = DIRECTION ( 'NONE',  ( -0.000000000000000000, 3.673940397442059868E-16, -1.000000000000000000 ) ) ;
#38938 = DIRECTION ( 'NONE',  ( -1.836970198721029934E-16, 1.836970198721036344E-16, -1.000000000000000000 ) ) ;
#38939 = DIRECTION ( 'NONE',  ( -1.000000000000000000, 0.000000000000000000, 0.000000000000000000 ) ) ;
#38940 = AXIS2_PLACEMENT_3D ( 'NONE', #47374, #42069, #52701 ) ;
#38942 = DIRECTION ( 'NONE',  ( -4.956352788505168198E-15, -1.000000000000000000, 0.000000000000000000 ) ) ;
#38941 = DIRECTION ( 'NONE',  ( -3.491481338843133355E-15, -1.000000000000000000, -1.836970198721029934E-16 ) ) ;
#38943 = VERTEX_POINT ( 'NONE', #11083 ) ;
#38945 = ORIENTED_EDGE ( 'NONE', *, *, #28311, .F. ) ;
#38944 = DIRECTION ( 'NONE',  ( -1.000000000000000000, 0.000000000000000000, 0.000000000000000000 ) ) ;
#38946 = AXIS2_PLACEMENT_3D ( 'NONE', #35793, #25904, #67976 ) ;
#38947 = ORIENTED_EDGE ( 'NONE', *, *, #45959, .T. ) ;
#38948 = VERTEX_POINT ( 'NONE', #36930 ) ;
#38949 = DIRECTION ( 'NONE',  ( -0.8660254037844482555, 0.000000000000000000, 0.4999999999999831801 ) ) ;
#38950 = EDGE_CURVE ( 'NONE', #38612, #66827, #20229, .T. ) ;
#38951 = VECTOR ( 'NONE', #65441, 1000.000000000000000 ) ;
#38952 = PLANE ( 'NONE',  #44393 ) ;
#38953 = LINE ( 'NONE', #23389, #22932 ) ;
#38954 = ORIENTED_EDGE ( 'NONE', *, *, #25563, .T. ) ;
#38955 = ORIENTED_EDGE ( 'NONE', *, *, #41301, .T. ) ;
#38956 = EDGE_CURVE ( 'NONE', #20214, #26006, #49606, .T. ) ;
#38957 = AXIS2_PLACEMENT_3D ( 'NONE', #60769, #12312, #28589 ) ;
#38958 = CARTESIAN_POINT ( 'NONE',  ( 8.835729544836288696, 2.355476262117161657, 54.00000000000000711 ) ) ;
#38959 = EDGE_CURVE ( 'NONE', #15483, #5750, #5788, .T. ) ;
#38960 = DIRECTION ( 'NONE',  ( 0.000000000000000000, -1.000000000000000000, 0.000000000000000000 ) ) ;
#38961 = EDGE_CURVE ( 'NONE', #18752, #57384, #21356, .T. ) ;
#38962 = VERTEX_POINT ( 'NONE', #15699 ) ;
#38963 = ORIENTED_EDGE ( 'NONE', *, *, #2472, .T. ) ;
#38964 = DIRECTION ( 'NONE',  ( -0.7671651518153006499, 0.6414496315691565753, -0.000000000000000000 ) ) ;
#38965 = AXIS2_PLACEMENT_3D ( 'NONE', #54889, #60168, #446 ) ;
#38966 = EDGE_CURVE ( 'NONE', #17214, #4035, #48917, .T. ) ;
#38967 = EDGE_CURVE ( 'NONE', #24515, #23915, #479, .T. ) ;
#38968 = CARTESIAN_POINT ( 'NONE',  ( -7.450000000000001954, 7.250000000000000000, -8.000000000000000000 ) ) ;
#38969 = ORIENTED_EDGE ( 'NONE', *, *, #2482, .T. ) ;
#38970 = STYLED_ITEM ( 'NONE', ( #32404 ), #44296 ) ;
#38971 = DIRECTION ( 'NONE',  ( 0.000000000000000000, -0.9921567416492215186, 0.1249999999999996531 ) ) ;
#38973 = ORIENTED_EDGE ( 'NONE', *, *, #7274, .T. ) ;
#38972 = LINE ( 'NONE', #18427, #61079 ) ;
#38974 = AXIS2_PLACEMENT_3D ( 'NONE', #40380, #61225, #40009 ) ;
#38975 = ORIENTED_EDGE ( 'NONE', *, *, #64844, .T. ) ;
#38976 = DIRECTION ( 'NONE',  ( -1.000000000000000000, 0.000000000000000000, 0.000000000000000000 ) ) ;
#38977 = CARTESIAN_POINT ( 'NONE',  ( 2.906483450353349429, -10.09643294401463365, 455.0000000000000568 ) ) ;
#38978 = CARTESIAN_POINT ( 'NONE',  ( -10.08346604330787777, 2.693516549646604918, 195.0000000000000284 ) ) ;
#38979 = CARTESIAN_POINT ( 'NONE',  ( 0.000000000000000000, 8.250000000000001776, -9.500000000000001776 ) ) ;
#38980 = CARTESIAN_POINT ( 'NONE',  ( 11.19368345035336532, -11.19368345035338308, 195.0000000000000284 ) ) ;
#38981 = PLANE ( 'NONE',  #50810 ) ;
#38982 = VERTEX_POINT ( 'NONE', #31618 ) ;
#38983 = DIRECTION ( 'NONE',  ( 0.000000000000000000, 1.000000000000000000, 0.000000000000000000 ) ) ;
#38985 = EDGE_LOOP ( 'NONE', ( #39372, #27470, #38610, #68611 ) ) ;
#38984 = CARTESIAN_POINT ( 'NONE',  ( 7.250000000000005329, -8.249999999999998224, -19.00000000000000000 ) ) ;
#38986 = DIRECTION ( 'NONE',  ( -0.000000000000000000, -0.000000000000000000, -1.000000000000000000 ) ) ;
#38987 = CARTESIAN_POINT ( 'NONE',  ( -30.00000000000000000, -5.200000000000001066, -26.59999999999999787 ) ) ;
#38988 = PLANE ( 'NONE',  #24577 ) ;
#38989 = CYLINDRICAL_SURFACE ( 'NONE', #50973, 24.99999999998784972 ) ;
#38990 = DIRECTION ( 'NONE',  ( 0.000000000000000000, 0.000000000000000000, 1.000000000000000000 ) ) ;
#38991 = VECTOR ( 'NONE', #14762, 1000.000000000000000 ) ;
#38992 = ORIENTED_EDGE ( 'NONE', *, *, #51941, .F. ) ;
#38993 = ORIENTED_EDGE ( 'NONE', *, *, #38429, .F. ) ;
#38994 = VECTOR ( 'NONE', #33527, 1000.000000000000114 ) ;
#38995 = LINE ( 'NONE', #1185, #20065 ) ;
#38996 = LINE ( 'NONE', #38662, #17613 ) ;
#38997 = ADVANCED_FACE ( 'NONE', ( #47863, #48569, #63789, #53193, #69435, #37268, #64154, #20989, #22040, #32306 ), #43602, .F. ) ;
#38998 = AXIS2_PLACEMENT_3D ( 'NONE', #38370, #38705, #64897 ) ;
#38999 = VECTOR ( 'NONE', #5276, 1000.000000000000000 ) ;
#39000 = VECTOR ( 'NONE', #15143, 1000.000000000000000 ) ;
#39001 = VERTEX_POINT ( 'NONE', #65190 ) ;
#39002 = CARTESIAN_POINT ( 'NONE',  ( -11.50000000000000000, -11.50000000000000000, -15.00000000000000000 ) ) ;
#39003 = ORIENTED_EDGE ( 'NONE', *, *, #27971, .F. ) ;
#39004 = EDGE_CURVE ( 'NONE', #39722, #47486, #21348, .T. ) ;
#39005 = ORIENTED_EDGE ( 'NONE', *, *, #69725, .T. ) ;
#39006 = DIRECTION ( 'NONE',  ( 8.673617379884087537E-15, 1.000000000000000000, 0.000000000000000000 ) ) ;
#39007 = DIRECTION ( 'NONE',  ( -0.000000000000000000, -0.000000000000000000, -1.000000000000000000 ) ) ;
#39008 = AXIS2_PLACEMENT_3D ( 'NONE', #40925, #24677, #61088 ) ;
#39009 = VECTOR ( 'NONE', #28079, 1000.000000000000114 ) ;
#39010 = VERTEX_POINT ( 'NONE', #31959 ) ;
#39011 = FACE_OUTER_BOUND ( 'NONE', #10757, .T. ) ;
#39012 = CYLINDRICAL_SURFACE ( 'NONE', #36856, 0.3499999999998886224 ) ;
#39013 = VECTOR ( 'NONE', #14799, 1000.000000000000000 ) ;
#39014 = FACE_OUTER_BOUND ( 'NONE', #37685, .T. ) ;
#39015 = DIRECTION ( 'NONE',  ( 0.000000000000000000, 0.000000000000000000, 1.000000000000000000 ) ) ;
#39016 = ORIENTED_EDGE ( 'NONE', *, *, #64313, .T. ) ;
#39018 = VERTEX_POINT ( 'NONE', #38309 ) ;
#39017 = CARTESIAN_POINT ( 'NONE',  ( 4.456444791733522252E-16, 7.450000000000002842, -20.50000000000000000 ) ) ;
#39019 = AXIS2_PLACEMENT_3D ( 'NONE', #41165, #67694, #7933 ) ;
#39020 = CARTESIAN_POINT ( 'NONE',  ( -7.450000000000001954, 7.250000000000000000, -16.50000000000000000 ) ) ;
#39021 = DIRECTION ( 'NONE',  ( -0.000000000000000000, -0.000000000000000000, -1.000000000000000000 ) ) ;
#39022 = DIRECTION ( 'NONE',  ( 1.000000000000000000, -1.115702204244422993E-14, -1.836970198721050395E-16 ) ) ;
#39023 = CARTESIAN_POINT ( 'NONE',  ( -5.242976262117259978, 5.242976262117182706, 54.00000000000000711 ) ) ;
#39024 = ORIENTED_EDGE ( 'NONE', *, *, #43677, .T. ) ;
#39025 = PRESENTATION_LAYER_ASSIGNMENT (  '', '', ( #44660 ) ) ;
#39026 = CARTESIAN_POINT ( 'NONE',  ( 11.50000000000000000, -11.50000000000100009, -15.00000000000084910 ) ) ;
#39027 = DIRECTION ( 'NONE',  ( -1.836970198721029934E-16, 1.836970198721036590E-16, -1.000000000000000000 ) ) ;
#39028 = ORIENTED_EDGE ( 'NONE', *, *, #63650, .F. ) ;
#39029 = EDGE_LOOP ( 'NONE', ( #50476, #46580, #17469, #16887 ) ) ;
#39030 = ORIENTED_EDGE ( 'NONE', *, *, #424, .T. ) ;
#39031 = FACE_OUTER_BOUND ( 'NONE', #58421, .T. ) ;
#39032 = LINE ( 'NONE', #60604, #64818 ) ;
#39033 = CARTESIAN_POINT ( 'NONE',  ( 7.826483450353380000, -12.00648345035349251, 455.0000000000000568 ) ) ;
#39034 = EDGE_CURVE ( 'NONE', #9638, #42852, #5451, .T. ) ;
#39035 = ORIENTED_EDGE ( 'NONE', *, *, #35453, .F. ) ;
#39036 = EDGE_LOOP ( 'NONE', ( #41277, #13567, #65158, #18651 ) ) ;
#39037 = CIRCLE ( 'NONE', #6281, 0.1999999999999987899 ) ;
#39038 = VERTEX_POINT ( 'NONE', #5086 ) ;
#39039 = CARTESIAN_POINT ( 'NONE',  ( 4.456444791733522252E-16, 7.450000000000002842, -13.00000000000000178 ) ) ;
#39040 = ORIENTED_EDGE ( 'NONE', *, *, #15769, .F. ) ;
#39041 = AXIS2_PLACEMENT_3D ( 'NONE', #2051, #18298, #35250 ) ;
#39042 = ORIENTED_EDGE ( 'NONE', *, *, #26238, .T. ) ;
#39043 = ORIENTED_EDGE ( 'NONE', *, *, #11513, .F. ) ;
#39044 = ORIENTED_EDGE ( 'NONE', *, *, #41853, .T. ) ;
#39045 = VECTOR ( 'NONE', #54677, 1000.000000000000000 ) ;
#39046 = DIRECTION ( 'NONE',  ( -1.000000000000000000, 0.000000000000000000, 0.000000000000000000 ) ) ;
#39047 = EDGE_CURVE ( 'NONE', #39228, #68196, #26652, .T. ) ;
#39048 = ADVANCED_FACE ( 'NONE', ( #16045 ), #59175, .F. ) ;
#39050 = ORIENTED_EDGE ( 'NONE', *, *, #63155, .F. ) ;
#39049 = CARTESIAN_POINT ( 'NONE',  ( -8.393516549646744096, -7.616533956692189022, 195.0000000000000284 ) ) ;
#39051 = CARTESIAN_POINT ( 'NONE',  ( 3.677663764522603795, 6.350872789121277506, 26.00000000000000711 ) ) ;
#39052 = VECTOR ( 'NONE', #26988, 1000.000000000000000 ) ;
#39053 = VECTOR ( 'NONE', #42302, 1000.000000000000000 ) ;
#39054 = VECTOR ( 'NONE', #55232, 1000.000000000000000 ) ;
#39055 = LINE ( 'NONE', #16808, #10376 ) ;
#39056 = ADVANCED_FACE ( 'NONE', ( #59865 ), #11419, .F. ) ;
#39057 = DIRECTION ( 'NONE',  ( 0.000000000000000000, 0.000000000000000000, -1.000000000000000000 ) ) ;
#39058 = ORIENTED_EDGE ( 'NONE', *, *, #62759, .F. ) ;
#39059 = AXIS2_PLACEMENT_3D ( 'NONE', #63517, #4123, #16114 ) ;
#39060 = AXIS2_PLACEMENT_3D ( 'NONE', #19701, #20764, #53652 ) ;
#39061 = VECTOR ( 'NONE', #56593, 1000.000000000000000 ) ;
#39062 = DIRECTION ( 'NONE',  ( 1.000000000000000000, -1.047444401652940007E-14, 0.000000000000000000 ) ) ;
#39063 = CARTESIAN_POINT ( 'NONE',  ( 7.000000000000000000, -25.60000000000000142, -15.10000000000000142 ) ) ;
#39064 = PLANE ( 'NONE',  #18009 ) ;
#39065 = VECTOR ( 'NONE', #34511, 1000.000000000000000 ) ;
#39066 = ORIENTED_EDGE ( 'NONE', *, *, #52118, .T. ) ;
#39067 = LINE ( 'NONE', #60632, #67580 ) ;
#39068 = AXIS2_PLACEMENT_3D ( 'NONE', #2211, #67267, #7851 ) ;
#39069 = PLANE ( 'NONE',  #69309 ) ;
#39070 = CARTESIAN_POINT ( 'NONE',  ( 7.532023737882817649, -6.665817930929295088, 26.00000000000000000 ) ) ;
#39071 = ORIENTED_EDGE ( 'NONE', *, *, #14840, .F. ) ;
#39072 = PLANE ( 'NONE',  #11010 ) ;
#39073 = CYLINDRICAL_SURFACE ( 'NONE', #60135, 0.5000000000009302559 ) ;
#39074 = CARTESIAN_POINT ( 'NONE',  ( 15.00000000000000000, -21.00000000000000000, 0.000000000000000000 ) ) ;
#39075 = EDGE_LOOP ( 'NONE', ( #29391, #47447, #36017, #55819 ) ) ;
#39076 = DIRECTION ( 'NONE',  ( 1.000000000000000000, -0.000000000000000000, -0.000000000000000000 ) ) ;
#39077 = DIRECTION ( 'NONE',  ( 1.000000000000000000, 0.000000000000000000, 0.000000000000000000 ) ) ;
#39078 = DIRECTION ( 'NONE',  ( -0.000000000000000000, -0.000000000000000000, -1.000000000000000000 ) ) ;
#39079 = CARTESIAN_POINT ( 'NONE',  ( 11.32648345035337911, 4.193516549646524538, 455.0000000000000568 ) ) ;
#39080 = FACE_OUTER_BOUND ( 'NONE', #36447, .T. ) ;
#39081 = VERTEX_POINT ( 'NONE', #59529 ) ;
#39082 = DIRECTION ( 'NONE',  ( 0.000000000000000000, -1.000000000000000000, 0.000000000000000000 ) ) ;
#39083 = DIRECTION ( 'NONE',  ( -1.000000000000000000, 0.000000000000000000, 0.000000000000000000 ) ) ;
#39084 = CARTESIAN_POINT ( 'NONE',  ( -5.242976262117259978, 3.142976262117183062, 26.00000000000000711 ) ) ;
#39085 = EDGE_CURVE ( 'NONE', #12819, #14861, #42209, .T. ) ;
#39086 = EDGE_CURVE ( 'NONE', #49722, #12416, #19114, .T. ) ;
#39087 = EDGE_CURVE ( 'NONE', #66435, #31212, #45315, .T. ) ;
#39088 = DIRECTION ( 'NONE',  ( -0.000000000000000000, -0.000000000000000000, 1.000000000000000000 ) ) ;
#39089 = FACE_OUTER_BOUND ( 'NONE', #32308, .T. ) ;
#39090 = ORIENTED_EDGE ( 'NONE', *, *, #63011, .T. ) ;
#39091 = CARTESIAN_POINT ( 'NONE',  ( 8.241237374594243548, 1.620245201994235718, 26.00000000000000711 ) ) ;
#39092 = CARTESIAN_POINT ( 'NONE',  ( -4.188533722949335569, 4.727349090213398775, 455.0000000000000568 ) ) ;
#39093 = AXIS2_PLACEMENT_3D ( 'NONE', #43018, #43727, #60314 ) ;
#39094 = DIRECTION ( 'NONE',  ( -0.000000000000000000, 0.000000000000000000, -1.000000000000000000 ) ) ;
#39095 = EDGE_CURVE ( 'NONE', #341, #11956, #6476, .T. ) ;
#39096 = CIRCLE ( 'NONE', #22152, 0.2000000000005226763 ) ;
#39097 = CARTESIAN_POINT ( 'NONE',  ( 10.90000000000000036, 20.60000000000000142, 13.86939075806900057 ) ) ;
#39098 = B_SPLINE_CURVE_WITH_KNOTS ( 'NONE', 3,
 ( #18561, #1962, #51088, #24226, #23525, #28468 ),
 .UNSPECIFIED., .F., .F.,
 ( 4, 2, 4 ),
 ( 0.0002380763768129734448, 0.7291065797294584705, 1.457975083082104106 ),
 .UNSPECIFIED. ) ;
#39099 = DIRECTION ( 'NONE',  ( -1.000000000000000000, 0.000000000000000000, 0.000000000000000000 ) ) ;
#39100 = ORIENTED_EDGE ( 'NONE', *, *, #18413, .T. ) ;
#39101 = VECTOR ( 'NONE', #65516, 1000.000000000000000 ) ;
#39102 = VECTOR ( 'NONE', #67172, 1000.000000000000114 ) ;
#39103 = AXIS2_PLACEMENT_3D ( 'NONE', #28265, #55832, #45559 ) ;
#39104 = DIRECTION ( 'NONE',  ( 1.000000000000000000, -0.000000000000000000, 0.000000000000000000 ) ) ;
#39105 = DIRECTION ( 'NONE',  ( 0.000000000000000000, 0.000000000000000000, 1.000000000000000000 ) ) ;
#39106 = ORIENTED_EDGE ( 'NONE', *, *, #23696, .F. ) ;
#39107 = AXIS2_PLACEMENT_3D ( 'NONE', #56970, #8183, #67948 ) ;
#39108 = VECTOR ( 'NONE', #59741, 1000.000000000000000 ) ;
#39109 = CARTESIAN_POINT ( 'NONE',  ( 7.250000000000005329, -7.449999999999998401, -17.50000000000000000 ) ) ;
#39110 = ORIENTED_EDGE ( 'NONE', *, *, #50529, .F. ) ;
#39111 = VECTOR ( 'NONE', #36362, 1000.000000000000000 ) ;
#39112 = DIRECTION ( 'NONE',  ( 0.000000000000000000, 1.000000000000000000, 0.000000000000000000 ) ) ;
#39113 = ORIENTED_EDGE ( 'NONE', *, *, #67316, .F. ) ;
#39114 = EDGE_LOOP ( 'NONE', ( #5401, #13630, #8237, #30708, #42259, #24090, #23154, #18852, #27803, #64624, #13463, #35461, #65797, #67279, #55837, #4437, #32641 ) ) ;
#39115 = LINE ( 'NONE', #7627, #38562 ) ;
#39116 = CARTESIAN_POINT ( 'NONE',  ( 9.912023737882803331, 6.817976262117185549, 54.00000000000000711 ) ) ;
#39117 = CARTESIAN_POINT ( 'NONE',  ( 8.930623737882843471, 9.689726262117160260, 26.00000000000000711 ) ) ;
#39118 = DIRECTION ( 'NONE',  ( 1.000000000000000000, -0.000000000000000000, -0.000000000000000000 ) ) ;
#39119 = AXIS2_PLACEMENT_3D ( 'NONE', #8967, #62709, #25242 ) ;
#39120 = ORIENTED_EDGE ( 'NONE', *, *, #23473, .F. ) ;
#39121 = ORIENTED_EDGE ( 'NONE', *, *, #18813, .T. ) ;
#39122 = PLANE ( 'NONE',  #41434 ) ;
#39123 = DIRECTION ( 'NONE',  ( -1.000000000000000000, 0.000000000000000000, 0.000000000000000000 ) ) ;
#39124 = VERTEX_POINT ( 'NONE', #55942 ) ;
#39125 = VERTEX_POINT ( 'NONE', #44619 ) ;
#39126 = EDGE_LOOP ( 'NONE', ( #53336, #11200, #10856, #22170 ) ) ;
#39127 = CARTESIAN_POINT ( 'NONE',  ( 78.77321854994620765, 47.95351654967443977, 40.00000000000000000 ) ) ;
#39128 = PLANE ( 'NONE',  #9646 ) ;
#39130 = EDGE_LOOP ( 'NONE', ( #40406, #26784, #61424, #33908 ) ) ;
#39129 = DIRECTION ( 'NONE',  ( 0.000000000000000000, 0.000000000000000000, -1.000000000000000000 ) ) ;
#39131 = EDGE_CURVE ( 'NONE', #39415, #69380, #7493, .T. ) ;
#39132 = CARTESIAN_POINT ( 'NONE',  ( 30.00000000000000000, -13.79999999999979998, 17.64999999999988844 ) ) ;
#39133 = DIRECTION ( 'NONE',  ( -1.836970198721029934E-16, 1.836970198721036590E-16, -1.000000000000000000 ) ) ;
#39134 = EDGE_CURVE ( 'NONE', #1047, #37232, #1171, .T. ) ;
#39135 = EDGE_CURVE ( 'NONE', #25678, #27522, #69629, .T. ) ;
#39136 = AXIS2_PLACEMENT_3D ( 'NONE', #64412, #27279, #48843 ) ;
#39137 = ORIENTED_EDGE ( 'NONE', *, *, #22950, .T. ) ;
#39138 = ORIENTED_EDGE ( 'NONE', *, *, #63883, .T. ) ;
#39139 = EDGE_CURVE ( 'NONE', #3338, #64676, #22726, .T. ) ;
#39140 = AXIS2_PLACEMENT_3D ( 'NONE', #27727, #884, #43976 ) ;
#39141 = CARTESIAN_POINT ( 'NONE',  ( 8.250000000000005329, -8.249999999999998224, -26.00000000000001066 ) ) ;
#39142 = PLANE ( 'NONE',  #26764 ) ;
#39143 = CIRCLE ( 'NONE', #8662, 4.000000000000001776 ) ;
#39144 = VECTOR ( 'NONE', #9590, 1000.000000000000114 ) ;
#39145 = EDGE_CURVE ( 'NONE', #24260, #902, #65854, .T. ) ;
#39146 = CARTESIAN_POINT ( 'NONE',  ( 8.612468434717241550, -1.480523737882825985, 54.00000000000000711 ) ) ;
#39147 = EDGE_CURVE ( 'NONE', #20587, #68282, #27688, .T. ) ;
#39148 = VECTOR ( 'NONE', #13608, 1000.000000000000000 ) ;
#39149 = VECTOR ( 'NONE', #65416, 1000.000000000000000 ) ;
#39150 = DIRECTION ( 'NONE',  ( 0.000000000000000000, -1.000000000000000000, 0.000000000000000000 ) ) ;
#39151 = DIRECTION ( 'NONE',  ( -1.000000000000000000, 0.000000000000000000, 0.000000000000000000 ) ) ;
#39153 = VERTEX_POINT ( 'NONE', #50284 ) ;
#39152 = FACE_BOUND ( 'NONE', #4365, .T. ) ;
#39154 = ORIENTED_EDGE ( 'NONE', *, *, #29278, .T. ) ;
#39155 = DIRECTION ( 'NONE',  ( -0.000000000000000000, 0.000000000000000000, 1.000000000000000000 ) ) ;
#39156 = AXIS2_PLACEMENT_3D ( 'NONE', #4994, #41416, #63344 ) ;
#39157 = AXIS2_PLACEMENT_3D ( 'NONE', #17548, #39460, #61021 ) ;
#39158 = DIRECTION ( 'NONE',  ( 0.7671651518153083105, -0.6414496315691473605, -2.587583378555127804E-16 ) ) ;
#39159 = DIRECTION ( 'NONE',  ( -1.836970198721029934E-16, -1.836970198721010706E-16, 1.000000000000000000 ) ) ;
#39160 = FACE_OUTER_BOUND ( 'NONE', #17623, .T. ) ;
#39161 = CIRCLE ( 'NONE', #38080, 1.000000000000000000 ) ;
#39162 = CARTESIAN_POINT ( 'NONE',  ( -0.9414762621173295987, -9.929523737882849588, 54.00000000000000711 ) ) ;
#39163 = ORIENTED_EDGE ( 'NONE', *, *, #49996, .T. ) ;
#39164 = PLANE ( 'NONE',  #28997 ) ;
#39165 = DIRECTION ( 'NONE',  ( -1.836970198721029934E-16, 1.836970198721036344E-16, -1.000000000000000000 ) ) ;
#39166 = CARTESIAN_POINT ( 'NONE',  ( 7.000000000000000000, -39.80000000000000426, -8.400000000000000355 ) ) ;
#39167 = CARTESIAN_POINT ( 'NONE',  ( 30.90000000000000213, 13.66939075806899950, 20.80000000000000426 ) ) ;
#39168 = PRODUCT_DEFINITION_SHAPE ( 'NONE', 'NONE',  #69992 ) ;
#39169 = CIRCLE ( 'NONE', #19945, 0.1749999999999998224 ) ;
#39170 = DIRECTION ( 'NONE',  ( 0.000000000000000000, -3.673940397442059868E-16, 1.000000000000000000 ) ) ;
#39171 = PLANE ( 'NONE',  #64615 ) ;
#39172 = CARTESIAN_POINT ( 'NONE',  ( 7.606483450353380249, -11.78648345035349010, 455.0000000000000568 ) ) ;
#39173 = VERTEX_POINT ( 'NONE', #12108 ) ;
#39174 = LINE ( 'NONE', #28899, #51261 ) ;
#39175 = DIRECTION ( 'NONE',  ( -5.013651664672856055E-16, 1.000000000000000000, 0.000000000000000000 ) ) ;
#39176 = ORIENTED_EDGE ( 'NONE', *, *, #30675, .T. ) ;
#39177 = DIRECTION ( 'NONE',  ( 0.000000000000000000, 0.000000000000000000, 1.000000000000000000 ) ) ;
#39178 = DIRECTION ( 'NONE',  ( 0.000000000000000000, 0.000000000000000000, -1.000000000000000000 ) ) ;
#39179 = CARTESIAN_POINT ( 'NONE',  ( -5.993516549646776603, -6.006483450353426790, 455.0000000000000568 ) ) ;
#39180 = PLANE ( 'NONE',  #64660 ) ;
#39181 = CARTESIAN_POINT ( 'NONE',  ( -1.077516549646676092, 10.73351654964656454, 455.0000000000000568 ) ) ;
#39182 = ORIENTED_EDGE ( 'NONE', *, *, #22187, .T. ) ;
#39183 = CARTESIAN_POINT ( 'NONE',  ( 7.250000000000005329, -8.249999999999998224, -16.00000000000000000 ) ) ;
#39184 = ORIENTED_EDGE ( 'NONE', *, *, #51053, .F. ) ;
#39185 = LINE ( 'NONE', #11607, #55950 ) ;
#39186 = VECTOR ( 'NONE', #35681, 1000.000000000000000 ) ;
#39187 = ORIENTED_EDGE ( 'NONE', *, *, #2634, .F. ) ;
#39188 = DIRECTION ( 'NONE',  ( 1.000000000000000000, 0.000000000000000000, 0.000000000000000000 ) ) ;
#39189 = ADVANCED_FACE ( 'NONE', ( #40007 ), #22394, .T. ) ;
#39190 =( NAMED_UNIT ( * ) SI_UNIT ( $, .STERADIAN. ) SOLID_ANGLE_UNIT ( ) );
#39191 = VECTOR ( 'NONE', #55757, 1000.000000000000000 ) ;
#39192 = ADVANCED_FACE ( 'NONE', ( #66206 ), #12439, .F. ) ;
#39193 = CYLINDRICAL_SURFACE ( 'NONE', #59358, 24.99999999998784972 ) ;
#39194 = ORIENTED_EDGE ( 'NONE', *, *, #20143, .T. ) ;
#39195 = ORIENTED_EDGE ( 'NONE', *, *, #38701, .T. ) ;
#39196 = DIRECTION ( 'NONE',  ( 1.836970198721029934E-16, 1.836970198721010706E-16, -1.000000000000000000 ) ) ;
#39197 = ORIENTED_EDGE ( 'NONE', *, *, #4985, .F. ) ;
#39198 = ORIENTED_EDGE ( 'NONE', *, *, #18864, .T. ) ;
#39199 = AXIS2_PLACEMENT_3D ( 'NONE', #48938, #54595, #55281 ) ;
#39200 = VECTOR ( 'NONE', #62007, 1000.000000000000000 ) ;
#39201 = DIRECTION ( 'NONE',  ( -1.000000000000000000, 0.000000000000000000, 0.000000000000000000 ) ) ;
#39202 = LINE ( 'NONE', #22937, #13212 ) ;
#39203 = DIRECTION ( 'NONE',  ( 0.000000000000000000, 1.000000000000000000, 0.000000000000000000 ) ) ;
#39204 = ORIENTED_EDGE ( 'NONE', *, *, #12726, .T. ) ;
#39205 = CARTESIAN_POINT ( 'NONE',  ( 41.09999999999999432, 20.60000000000000142, -13.86939075806900057 ) ) ;
#39206 = AXIS2_PLACEMENT_3D ( 'NONE', #51150, #14730, #36292 ) ;
#39207 = VECTOR ( 'NONE', #66061, 1000.000000000000000 ) ;
#39209 = DIRECTION ( 'NONE',  ( -1.000000000000000000, 0.000000000000000000, 0.000000000000000000 ) ) ;
#39208 = CYLINDRICAL_SURFACE ( 'NONE', #46230, 24.99999999998784972 ) ;
#39210 = ORIENTED_EDGE ( 'NONE', *, *, #11108, .T. ) ;
#39212 = ORIENTED_EDGE ( 'NONE', *, *, #44876, .T. ) ;
#39211 = LINE ( 'NONE', #7018, #7126 ) ;
#39213 = ORIENTED_EDGE ( 'NONE', *, *, #6317, .F. ) ;
#39214 = ADVANCED_FACE ( 'NONE', ( #39331 ), #49936, .F. ) ;
#39215 = DIRECTION ( 'NONE',  ( -8.359604446858500663E-15, -1.000000000000000000, 0.000000000000000000 ) ) ;
#39216 = VECTOR ( 'NONE', #3164, 1000.000000000000000 ) ;
#39217 = DIRECTION ( 'NONE',  ( -1.000000000000000000, 0.000000000000000000, 0.000000000000000000 ) ) ;
#39218 = EDGE_CURVE ( 'NONE', #17055, #53282, #61574, .T. ) ;
#39219 = EDGE_LOOP ( 'NONE', ( #45164, #68430, #52670, #18000 ) ) ;
#39220 = ORIENTED_EDGE ( 'NONE', *, *, #15378, .T. ) ;
#39221 = CARTESIAN_POINT ( 'NONE',  ( 7.606483450353380249, -11.78648345035339418, 195.0000000000000284 ) ) ;
#39222 = DIRECTION ( 'NONE',  ( 1.000000000000000000, 0.000000000000000000, 0.000000000000000000 ) ) ;
#39223 = ORIENTED_EDGE ( 'NONE', *, *, #7066, .F. ) ;
#39224 = CARTESIAN_POINT ( 'NONE',  ( -9.689726262117313027, -8.930623737882751101, 26.00000000000000000 ) ) ;
#39225 = DIRECTION ( 'NONE',  ( 0.000000000000000000, 0.000000000000000000, 1.000000000000000000 ) ) ;
#39226 = EDGE_CURVE ( 'NONE', #19062, #20091, #31557, .T. ) ;
#39227 = DIRECTION ( 'NONE',  ( -0.000000000000000000, -1.000000000000000000, 0.000000000000000000 ) ) ;
#39228 = VERTEX_POINT ( 'NONE', #55598 ) ;
#39229 = EDGE_CURVE ( 'NONE', #47719, #11735, #1851, .T. ) ;
#39230 = DIRECTION ( 'NONE',  ( 0.000000000000000000, -0.000000000000000000, 1.000000000000000000 ) ) ;
#39231 = DIRECTION ( 'NONE',  ( -1.000000000000000000, 0.000000000000000000, 0.000000000000000000 ) ) ;
#39232 = CIRCLE ( 'NONE', #44881, 24.99999999998784972 ) ;
#39234 = ORIENTED_EDGE ( 'NONE', *, *, #31714, .F. ) ;
#39233 =( LENGTH_UNIT ( ) NAMED_UNIT ( * ) SI_UNIT ( .MILLI., .METRE. ) );
#39236 = ORIENTED_EDGE ( 'NONE', *, *, #58315, .T. ) ;
#39235 = DIRECTION ( 'NONE',  ( 1.000000000000000000, 0.000000000000000000, 0.000000000000000000 ) ) ;
#39237 = LINE ( 'NONE', #65089, #65273 ) ;
#39238 = LINE ( 'NONE', #39573, #23894 ) ;
#39239 = EDGE_CURVE ( 'NONE', #18603, #37912, #39665, .T. ) ;
#39240 = DIRECTION ( 'NONE',  ( 0.000000000000000000, 0.000000000000000000, -1.000000000000000000 ) ) ;
#39241 = PLANE ( 'NONE',  #48620 ) ;
#39242 = VECTOR ( 'NONE', #13862, 1000.000000000000000 ) ;
#39243 = CARTESIAN_POINT ( 'NONE',  ( -8.250000000000001776, -7.249999999999998224, -16.50000000000000000 ) ) ;
#39244 = EDGE_LOOP ( 'NONE', ( #25505, #34192, #63626, #41253 ) ) ;
#39245 = CARTESIAN_POINT ( 'NONE',  ( 6.501044194225444883, 3.142976262117191943, 26.00000000000000711 ) ) ;
#39246 = DIRECTION ( 'NONE',  ( -1.836970198721029934E-16, 1.836970198721036344E-16, -1.000000000000000000 ) ) ;
#39247 = FILL_AREA_STYLE ('',( #17684 ) ) ;
#39248 = VECTOR ( 'NONE', #47114, 1000.000000000000000 ) ;
#39251 = EDGE_LOOP ( 'NONE', ( #45666, #64113, #48284, #14467 ) ) ;
#39250 = CARTESIAN_POINT ( 'NONE',  ( 282.7711612342632179, -25.38939884375893286, 17.11060115624107425 ) ) ;
#39249 = CIRCLE ( 'NONE', #44901, 0.8100000000000017186 ) ;
#39252 = DIRECTION ( 'NONE',  ( 0.000000000000000000, 0.000000000000000000, 1.000000000000000000 ) ) ;
#39253 = PLANE ( 'NONE',  #4762 ) ;
#39254 = AXIS2_PLACEMENT_3D ( 'NONE', #59180, #6131, #27694 ) ;
#39255 = CIRCLE ( 'NONE', #48307, 1.399999999999999245 ) ;
#39256 = EDGE_LOOP ( 'NONE', ( #38156, #39893, #28691, #40673, #56267, #66494, #28863 ) ) ;
#39257 = PLANE ( 'NONE',  #39890 ) ;
#39258 = DIRECTION ( 'NONE',  ( 1.000000000000000000, 0.000000000000000000, 0.000000000000000000 ) ) ;
#39259 = ORIENTED_EDGE ( 'NONE', *, *, #8700, .T. ) ;
#39260 = EDGE_CURVE ( 'NONE', #17912, #24963, #50636, .T. ) ;
#39261 = LINE ( 'NONE', #22996, #9748 ) ;
#39262 = LINE ( 'NONE', #61158, #15399 ) ;
#39263 = SURFACE_SIDE_STYLE ('',( #34285 ) ) ;
#39264 = CARTESIAN_POINT ( 'NONE',  ( -24.00000000000000000, -17.35230188589299871, -15.35019951917099945 ) ) ;
#39265 = EDGE_CURVE ( 'NONE', #39153, #62566, #34714, .T. ) ;
#39266 = CIRCLE ( 'NONE', #24592, 1.929199999999998916 ) ;
#39267 = CARTESIAN_POINT ( 'NONE',  ( 151.5599459900709860, 0.000000000000000000, 322.4587476295993156 ) ) ;
#39268 = ORIENTED_EDGE ( 'NONE', *, *, #3862, .T. ) ;
#39269 = PLANE ( 'NONE',  #31513 ) ;
#39270 = ORIENTED_EDGE ( 'NONE', *, *, #29782, .T. ) ;
#39271 = EDGE_CURVE ( 'NONE', #19830, #58210, #2152, .T. ) ;
#39272 = EDGE_LOOP ( 'NONE', ( #54834, #61204, #24170, #23239 ) ) ;
#39273 = LINE ( 'NONE', #777, #49416 ) ;
#39274 = CARTESIAN_POINT ( 'NONE',  ( -15.50000000000000000, -1.037157890325000054, -22.50000000000000000 ) ) ;
#39275 = EDGE_CURVE ( 'NONE', #31244, #8538, #40727, .T. ) ;
#39276 = DIRECTION ( 'NONE',  ( 1.000000000000000000, -5.981805089575196197E-17, 0.000000000000000000 ) ) ;
#39277 = ADVANCED_FACE ( 'NONE', ( #52043 ), #46032, .F. ) ;
#39278 = PLANE ( 'NONE',  #41983 ) ;
#39279 = ORIENTED_EDGE ( 'NONE', *, *, #4748, .F. ) ;
#39280 = EDGE_LOOP ( 'NONE', ( #12817, #46096, #28602, #16935 ) ) ;
#39281 = PLANE ( 'NONE',  #211 ) ;
#39282 = VERTEX_POINT ( 'NONE', #57687 ) ;
#39283 = FACE_OUTER_BOUND ( 'NONE', #8150, .T. ) ;
#39284 = CARTESIAN_POINT ( 'NONE',  ( -8.250000000000001776, -7.249999999999998224, -8.000000000000000000 ) ) ;
#39285 = DIRECTION ( 'NONE',  ( 0.000000000000000000, 1.000000000000000000, 0.000000000000000000 ) ) ;
#39286 = EDGE_CURVE ( 'NONE', #10779, #34850, #30114, .T. ) ;
#39287 = ADVANCED_FACE ( 'NONE', ( #57338 ), #35058, .F. ) ;
#39288 = CARTESIAN_POINT ( 'NONE',  ( 275.0000000000000000, -42.00000000000000000, -15.10000000000000142 ) ) ;
#39290 = CARTESIAN_POINT ( 'NONE',  ( 9.900000000000000355, 14.08845687959340331, -21.00000000000000000 ) ) ;
#39289 = CARTESIAN_POINT ( 'NONE',  ( 6.006483450353401921, 5.993516549646582092, 455.0000000000000568 ) ) ;
#39291 = VERTEX_POINT ( 'NONE', #8188 ) ;
#39294 = EDGE_CURVE ( 'NONE', #65043, #20060, #62999, .T. ) ;
#39293 = VERTEX_POINT ( 'NONE', #56291 ) ;
#39292 = CARTESIAN_POINT ( 'NONE',  ( -8.250000000000000000, 7.250000000000001776, -20.00000000000000000 ) ) ;
#39295 = ORIENTED_EDGE ( 'NONE', *, *, #14197, .T. ) ;
#39296 = ORIENTED_EDGE ( 'NONE', *, *, #48414, .T. ) ;
#39297 = EDGE_CURVE ( 'NONE', #48502, #10676, #9258, .T. ) ;
#39298 = EDGE_CURVE ( 'NONE', #24504, #32181, #51829, .T. ) ;
#39299 = CARTESIAN_POINT ( 'NONE',  ( 78.77321854994620765, 47.95351654967443977, 25.00000000000000000 ) ) ;
#39300 = ADVANCED_FACE ( 'NONE', ( #2889 ), #52392, .F. ) ;
#39301 = VECTOR ( 'NONE', #19099, 1000.000000000000000 ) ;
#39302 = DIRECTION ( 'NONE',  ( -1.000000000000000000, 0.000000000000000000, 0.000000000000000000 ) ) ;
#39303 = EDGE_CURVE ( 'NONE', #5931, #12238, #68795, .T. ) ;
#39304 = DIRECTION ( 'NONE',  ( 1.836970198721029934E-16, -1.836970198721036344E-16, 1.000000000000000000 ) ) ;
#39305 = ORIENTED_EDGE ( 'NONE', *, *, #19605, .F. ) ;
#39306 = ORIENTED_EDGE ( 'NONE', *, *, #9939, .F. ) ;
#39307 = EDGE_CURVE ( 'NONE', #57216, #31517, #38316, .T. ) ;
#39308 = VECTOR ( 'NONE', #46604, 1000.000000000000000 ) ;
#39309 = AXIS2_PLACEMENT_3D ( 'NONE', #40854, #28839, #18948 ) ;
#39310 = DIRECTION ( 'NONE',  ( 1.836970198721029934E-16, 1.836970198721010706E-16, -1.000000000000000000 ) ) ;
#39311 = DIRECTION ( 'NONE',  ( 0.000000000000000000, 0.000000000000000000, -1.000000000000000000 ) ) ;
#39312 = ORIENTED_EDGE ( 'NONE', *, *, #2157, .T. ) ;
#39313 = ORIENTED_EDGE ( 'NONE', *, *, #40585, .T. ) ;
#39314 = CARTESIAN_POINT ( 'NONE',  ( 9.912023737882815766, -6.657023737882814984, 26.00000000000000000 ) ) ;
#39315 = EDGE_CURVE ( 'NONE', #46458, #21641, #28150, .T. ) ;
#39316 = CARTESIAN_POINT ( 'NONE',  ( -7.250000000000000888, 7.250000000000001776, -7.500000000000000000 ) ) ;
#39317 = VERTEX_POINT ( 'NONE', #24816 ) ;
#39318 = EDGE_CURVE ( 'NONE', #28244, #57835, #41067, .T. ) ;
#39319 = CIRCLE ( 'NONE', #33665, 0.2000000000000005107 ) ;
#39320 = LINE ( 'NONE', #12769, #60599 ) ;
#39322 = ORIENTED_EDGE ( 'NONE', *, *, #52313, .T. ) ;
#39321 = CARTESIAN_POINT ( 'NONE',  ( 46.39999999999999858, 33.00000000000000000, 1.250000000000000000 ) ) ;
#39323 = ORIENTED_EDGE ( 'NONE', *, *, #7818, .F. ) ;
#39324 = CARTESIAN_POINT ( 'NONE',  ( 3.848229544836330174, 7.517976262117205266, 54.00000000000000711 ) ) ;
#39325 = CARTESIAN_POINT ( 'NONE',  ( -7.250000000000000888, 8.250000000000001776, -25.00000000000000000 ) ) ;
#39326 = FACE_OUTER_BOUND ( 'NONE', #43463, .T. ) ;
#39327 = DIRECTION ( 'NONE',  ( 0.000000000000000000, 0.000000000000000000, -1.000000000000000000 ) ) ;
#39328 = CARTESIAN_POINT ( 'NONE',  ( 3.677663764522608680, 6.350872789121272177, 54.00000000000000711 ) ) ;
#39329 = CARTESIAN_POINT ( 'NONE',  ( -11.50000000000000000, -12.00000000000000000, -11.00000000000000000 ) ) ;
#39330 = ORIENTED_EDGE ( 'NONE', *, *, #67858, .T. ) ;
#39331 = FACE_OUTER_BOUND ( 'NONE', #10894, .T. ) ;
#39333 = ORIENTED_EDGE ( 'NONE', *, *, #2982, .T. ) ;
#39332 = CARTESIAN_POINT ( 'NONE',  ( -5.538810540050064901, -7.357023737882800951, 54.00000000000000711 ) ) ;
#39334 = FACE_OUTER_BOUND ( 'NONE', #26714, .T. ) ;
#39335 = DIRECTION ( 'NONE',  ( -1.000000000000000000, 0.000000000000000000, 0.000000000000000000 ) ) ;
#39336 = LINE ( 'NONE', #49604, #4313 ) ;
#39337 = DIRECTION ( 'NONE',  ( 0.000000000000000000, 0.7096009616570518874, 0.7046037717862339012 ) ) ;
#39338 = LINE ( 'NONE', #2206, #34808 ) ;
#39339 = ORIENTED_EDGE ( 'NONE', *, *, #42180, .T. ) ;
#39340 = ORIENTED_EDGE ( 'NONE', *, *, #5480, .T. ) ;
#39341 = DIRECTION ( 'NONE',  ( 1.000000000000000000, -1.047444401652939849E-14, 1.836970198721010706E-16 ) ) ;
#39342 = DIRECTION ( 'NONE',  ( -0.000000000000000000, -0.000000000000000000, 1.000000000000000000 ) ) ;
#39343 = CIRCLE ( 'NONE', #8865, 0.2000000000000005107 ) ;
#39344 = EDGE_CURVE ( 'NONE', #20182, #39844, #67954, .T. ) ;
#39345 = LINE ( 'NONE', #66903, #54532 ) ;
#39346 = ORIENTED_EDGE ( 'NONE', *, *, #20279, .T. ) ;
#39347 = LINE ( 'NONE', #34734, #19174 ) ;
#39348 = ORIENTED_EDGE ( 'NONE', *, *, #61803, .F. ) ;
#39349 = EDGE_CURVE ( 'NONE', #42050, #11645, #4454, .T. ) ;
#39350 = ORIENTED_EDGE ( 'NONE', *, *, #6641, .T. ) ;
#39351 = VECTOR ( 'NONE', #27770, 1000.000000000000000 ) ;
#39352 = DIRECTION ( 'NONE',  ( 0.000000000000000000, 1.000000000000000000, 0.000000000000000000 ) ) ;
#39353 = LINE ( 'NONE', #8212, #56787 ) ;
#39354 = ORIENTED_EDGE ( 'NONE', *, *, #67090, .T. ) ;
#39355 = DIRECTION ( 'NONE',  ( 1.000000000000000000, -3.491481338843133355E-15, 0.000000000000000000 ) ) ;
#39356 = EDGE_CURVE ( 'NONE', #50683, #62375, #47088, .T. ) ;
#39357 = CARTESIAN_POINT ( 'NONE',  ( -7.750000000000001776, 7.750000000000001776, 5.000000000000000000 ) ) ;
#39358 = EDGE_CURVE ( 'NONE', #35896, #11814, #41767, .T. ) ;
#39359 = CARTESIAN_POINT ( 'NONE',  ( 10.70000000000000107, -53.81370849898476649, 17.60000000000000142 ) ) ;
#39360 = ORIENTED_EDGE ( 'NONE', *, *, #69634, .T. ) ;
#39362 = ORIENTED_EDGE ( 'NONE', *, *, #57617, .F. ) ;
#39361 = CARTESIAN_POINT ( 'NONE',  ( 11.78648345035337819, -4.186483450353492231, 455.0000000000000568 ) ) ;
#39363 = TOROIDAL_SURFACE ( 'NONE', #21317, 3.299999999999470024, 0.2000000000005275058 ) ;
#39364 = CARTESIAN_POINT ( 'NONE',  ( 7.806483450353372433, 11.31351654964661968, 195.0000000000000284 ) ) ;
#39365 = DIRECTION ( 'NONE',  ( -0.5773502691896311712, 0.5773502691896230665, -0.5773502691896230665 ) ) ;
#39366 = FACE_OUTER_BOUND ( 'NONE', #2587, .T. ) ;
#39367 = DIRECTION ( 'NONE',  ( 0.000000000000000000, 0.000000000000000000, 1.000000000000000000 ) ) ;
#39368 = ORIENTED_EDGE ( 'NONE', *, *, #67689, .T. ) ;
#39369 = DIRECTION ( 'NONE',  ( 0.000000000000000000, -1.000000000000000000, 0.000000000000000000 ) ) ;
#39370 = CARTESIAN_POINT ( 'NONE',  ( -29.25000000000000000, -5.200000000000001066, 11.75000000000000000 ) ) ;
#39371 = ORIENTED_EDGE ( 'NONE', *, *, #8882, .T. ) ;
#39372 = ORIENTED_EDGE ( 'NONE', *, *, #50087, .T. ) ;
#39373 = EDGE_CURVE ( 'NONE', #17297, #65633, #30428, .T. ) ;
#39374 = ORIENTED_EDGE ( 'NONE', *, *, #42272, .T. ) ;
#39375 = DIRECTION ( 'NONE',  ( -1.000000000000000000, 0.000000000000000000, 0.000000000000000000 ) ) ;
#39376 = CARTESIAN_POINT ( 'NONE',  ( 30.00000000000000000, -11.50000000000000000, -15.00000000000000000 ) ) ;
#39377 = CARTESIAN_POINT ( 'NONE',  ( 50.00000000000000711, 0.7500000000000000000, 4.943429983321300902 ) ) ;
#39378 = VERTEX_POINT ( 'NONE', #21274 ) ;
#39379 = VERTEX_POINT ( 'NONE', #69345 ) ;
#39380 = VERTEX_POINT ( 'NONE', #43166 ) ;
#39381 = CARTESIAN_POINT ( 'NONE',  ( 49.00000000000000000, -0.1999999999911795112, 8.826273045769999343E-12 ) ) ;
#39382 = ORIENTED_EDGE ( 'NONE', *, *, #24453, .T. ) ;
#39383 = ORIENTED_EDGE ( 'NONE', *, *, #10820, .T. ) ;
#39384 = VERTEX_POINT ( 'NONE', #32579 ) ;
#39385 = AXIS2_PLACEMENT_3D ( 'NONE', #27395, #5833, #5133 ) ;
#39386 = VERTEX_POINT ( 'NONE', #36471 ) ;
#39387 = DIRECTION ( 'NONE',  ( 0.000000000000000000, -0.7096009616570518874, -0.7046037717862339012 ) ) ;
#39388 = EDGE_CURVE ( 'NONE', #4296, #32632, #58036, .T. ) ;
#39390 = EDGE_LOOP ( 'NONE', ( #23548, #43757, #68867, #33030 ) ) ;
#39389 = DIRECTION ( 'NONE',  ( 3.491481338843133355E-15, 1.000000000000000000, 1.836970198721029934E-16 ) ) ;
#39391 = CIRCLE ( 'NONE', #1103, 1.929199999999998916 ) ;
#39392 = CARTESIAN_POINT ( 'NONE',  ( 30.00000000000000000, 0.000000000000000000, 27.00000000000000000 ) ) ;
#39393 = EDGE_CURVE ( 'NONE', #24682, #26444, #59088, .T. ) ;
#39394 = CARTESIAN_POINT ( 'NONE',  ( 2.369523737882817116, 9.547976262117204627, 54.00000000000000711 ) ) ;
#39395 = DIRECTION ( 'NONE',  ( -0.000000000000000000, -0.000000000000000000, 1.000000000000000000 ) ) ;
#39396 = ADVANCED_FACE ( 'NONE', ( #20908 ), #31535, .F. ) ;
#39398 = ORIENTED_EDGE ( 'NONE', *, *, #2539, .F. ) ;
#39397 = CARTESIAN_POINT ( 'NONE',  ( 39.90000000000000568, 0.000000000000000000, 0.000000000000000000 ) ) ;
#39399 = AXIS2_PLACEMENT_3D ( 'NONE', #10729, #53888, #27001 ) ;
#39400 = FACE_OUTER_BOUND ( 'NONE', #57361, .T. ) ;
#39401 = CARTESIAN_POINT ( 'NONE',  ( 7.000000000000000000, -26.42999999999999972, 5.874955318979029784 ) ) ;
#39402 = VECTOR ( 'NONE', #50095, 1000.000000000000000 ) ;
#39403 = CARTESIAN_POINT ( 'NONE',  ( 8.250000000000005329, -8.249999999999998224, -26.00000000000001066 ) ) ;
#39404 = ORIENTED_EDGE ( 'NONE', *, *, #66438, .F. ) ;
#39405 = CARTESIAN_POINT ( 'NONE',  ( 4.961189459950039904, -7.357023737882821379, 54.00000000000000711 ) ) ;
#39407 = AXIS2_PLACEMENT_3D ( 'NONE', #18254, #67050, #39817 ) ;
#39406 = AXIS2_PLACEMENT_3D ( 'NONE', #26401, #47966, #26062 ) ;
#39408 = LINE ( 'NONE', #60967, #18506 ) ;
#39409 = DIRECTION ( 'NONE',  ( -1.836970198721029934E-16, 1.836970198721036590E-16, -1.000000000000000000 ) ) ;
#39410 = ORIENTED_EDGE ( 'NONE', *, *, #32988, .F. ) ;
#39411 = CARTESIAN_POINT ( 'NONE',  ( 8.250000000000005329, 8.250000000000001776, -26.00000000000001066 ) ) ;
#39412 = VECTOR ( 'NONE', #37872, 1000.000000000000000 ) ;
#39413 = CARTESIAN_POINT ( 'NONE',  ( 275.0000000000000000, -39.79999999999905214, 12.19999999999906315 ) ) ;
#39414 = PLANE ( 'NONE',  #8832 ) ;
#39415 = VERTEX_POINT ( 'NONE', #53104 ) ;
#39416 = FACE_OUTER_BOUND ( 'NONE', #28560, .T. ) ;
#39417 = DIRECTION ( 'NONE',  ( 0.000000000000000000, 0.1500000000000006328, -0.9886859966642592701 ) ) ;
#39418 =( NAMED_UNIT ( * ) PLANE_ANGLE_UNIT ( ) SI_UNIT ( $, .RADIAN. ) );
#39419 = DIRECTION ( 'NONE',  ( 0.000000000000000000, 0.000000000000000000, -1.000000000000000000 ) ) ;
#39420 = EDGE_CURVE ( 'NONE', #7006, #62810, #42822, .T. ) ;
#39421 = ORIENTED_EDGE ( 'NONE', *, *, #25668, .F. ) ;
#39422 = DIRECTION ( 'NONE',  ( 3.491481338843133355E-15, 1.000000000000000000, 1.836970198721029934E-16 ) ) ;
#39423 = DIRECTION ( 'NONE',  ( -1.084202172485501594E-14, -1.000000000000000000, 0.000000000000000000 ) ) ;
#39424 = DIRECTION ( 'NONE',  ( -1.000000000000000000, 6.308085367188447236E-15, 0.000000000000000000 ) ) ;
#39425 = EDGE_CURVE ( 'NONE', #19716, #62405, #64742, .T. ) ;
#39426 = CARTESIAN_POINT ( 'NONE',  ( -4.173516549646790530, -11.78648345035339595, 195.0000000000000284 ) ) ;
#39427 = DIRECTION ( 'NONE',  ( -1.000000000000000000, 0.000000000000000000, 0.000000000000000000 ) ) ;
#39428 = ORIENTED_EDGE ( 'NONE', *, *, #34988, .F. ) ;
#39429 = DIRECTION ( 'NONE',  ( 1.000000000000000000, 0.000000000000000000, 0.000000000000000000 ) ) ;
#39430 = CARTESIAN_POINT ( 'NONE',  ( -7.250000000000000888, -8.249999999999998224, -26.00000000000001066 ) ) ;
#39431 = EDGE_CURVE ( 'NONE', #26669, #15112, #42119, .T. ) ;
#39432 = EDGE_CURVE ( 'NONE', #30827, #9139, #27272, .T. ) ;
#39433 = CARTESIAN_POINT ( 'NONE',  ( 5.393625297349950110, 4.734785091273829849, 455.0000000000000568 ) ) ;
#39434 = VECTOR ( 'NONE', #39717, 1000.000000000000000 ) ;
#39435 = CARTESIAN_POINT ( 'NONE',  ( 55.00000000000000000, -16.96999999999999886, -21.00000000000000000 ) ) ;
#39436 = EDGE_CURVE ( 'NONE', #25188, #1043, #63706, .T. ) ;
#39437 = LINE ( 'NONE', #61699, #39593 ) ;
#39438 = EDGE_CURVE ( 'NONE', #28744, #10507, #48837, .T. ) ;
#39439 = ORIENTED_EDGE ( 'NONE', *, *, #34542, .T. ) ;
#39440 = AXIS2_PLACEMENT_3D ( 'NONE', #49030, #55044, #17184 ) ;
#39441 = ORIENTED_EDGE ( 'NONE', *, *, #47675, .F. ) ;
#39442 = VECTOR ( 'NONE', #60073, 1000.000000000000000 ) ;
#39443 = EDGE_CURVE ( 'NONE', #69392, #42454, #52762, .T. ) ;
#39444 = CARTESIAN_POINT ( 'NONE',  ( -7.450000000000001954, -7.249999999999998224, -19.00000000000000000 ) ) ;
#39445 = CYLINDRICAL_SURFACE ( 'NONE', #61642, 0.2000000000000005107 ) ;
#39446 = ORIENTED_EDGE ( 'NONE', *, *, #54541, .T. ) ;
#39447 = LINE ( 'NONE', #55047, #44247 ) ;
#39448 = ORIENTED_EDGE ( 'NONE', *, *, #44326, .T. ) ;
#39449 = VECTOR ( 'NONE', #12432, 1000.000000000000000 ) ;
#39450 = DIRECTION ( 'NONE',  ( -1.836970198721029934E-16, 1.836970198721036344E-16, -1.000000000000000000 ) ) ;
#39451 = ORIENTED_EDGE ( 'NONE', *, *, #21775, .T. ) ;
#39452 = ORIENTED_EDGE ( 'NONE', *, *, #21340, .F. ) ;
#39453 = DIRECTION ( 'NONE',  ( 0.000000000000000000, 1.000000000000000000, 0.000000000000000000 ) ) ;
#39454 = CARTESIAN_POINT ( 'NONE',  ( -17.24945551514599984, -15.50000000000000000, 25.53140320652400064 ) ) ;
#39455 = CIRCLE ( 'NONE', #21407, 1.929199999999998028 ) ;
#39456 = CARTESIAN_POINT ( 'NONE',  ( -1.077516549646676092, 10.73351654964656454, 195.0000000000000284 ) ) ;
#39457 = CARTESIAN_POINT ( 'NONE',  ( -9.390476262117260831, 0.9414762621171833823, 54.00000000000000711 ) ) ;
#39458 = EDGE_LOOP ( 'NONE', ( #47375, #5828, #57427, #8393 ) ) ;
#39459 = ORIENTED_EDGE ( 'NONE', *, *, #9003, .F. ) ;
#39460 = DIRECTION ( 'NONE',  ( 0.000000000000000000, 0.000000000000000000, -1.000000000000000000 ) ) ;
#39462 = CARTESIAN_POINT ( 'NONE',  ( -2.893516549646830249, -11.12648345035345621, 455.0000000000000568 ) ) ;
#39461 = AXIS2_PLACEMENT_3D ( 'NONE', #55311, #21477, #26439 ) ;
#39463 = VERTEX_POINT ( 'NONE', #10640 ) ;
#39464 = ORIENTED_EDGE ( 'NONE', *, *, #42317, .T. ) ;
#39466 = ORIENTED_EDGE ( 'NONE', *, *, #69655, .T. ) ;
#39465 = ITEM_DEFINED_TRANSFORMATION ( 'NONE', 'NONE', #58416,  #45918 ) ;
#39467 = DIRECTION ( 'NONE',  ( 1.000000000000000000, -0.000000000000000000, 0.000000000000000000 ) ) ;
#39469 = ORIENTED_EDGE ( 'NONE', *, *, #14879, .T. ) ;
#39468 = CARTESIAN_POINT ( 'NONE',  ( -6.500000000000002665, -6.500000000000002665, -1.000000000000000000 ) ) ;
#39470 = DIRECTION ( 'NONE',  ( -1.000000000000000000, 0.000000000000000000, 0.000000000000000000 ) ) ;
#39471 = DIRECTION ( 'NONE',  ( 0.000000000000000000, 1.000000000000000000, 0.000000000000000000 ) ) ;
#39472 = ORIENTED_EDGE ( 'NONE', *, *, #19516, .F. ) ;
#39473 = EDGE_CURVE ( 'NONE', #61891, #8330, #26217, .T. ) ;
#39474 = ORIENTED_EDGE ( 'NONE', *, *, #4507, .F. ) ;
#39475 = ADVANCED_FACE ( 'NONE', ( #15623 ), #58748, .T. ) ;
#39476 = ADVANCED_FACE ( 'NONE', ( #58409 ), #4998, .T. ) ;
#39477 = DIRECTION ( 'NONE',  ( 2.135044278125299371E-15, -1.000000000000000000, -3.673940397442060361E-16 ) ) ;
#39478 = FACE_OUTER_BOUND ( 'NONE', #62591, .T. ) ;
#39479 = APPLICATION_CONTEXT ( 'automotive_design' ) ;
#39480 = CIRCLE ( 'NONE', #67755, 2.458500000000000796 ) ;
#39481 = VECTOR ( 'NONE', #20423, 1000.000000000000000 ) ;
#39482 = CIRCLE ( 'NONE', #9012, 0.1999999999999996503 ) ;
#39483 = CARTESIAN_POINT ( 'NONE',  ( -1.677516549646683730, 9.828310488885911411, 455.0000000000000568 ) ) ;
#39484 = DIRECTION ( 'NONE',  ( 0.000000000000000000, 0.000000000000000000, 1.000000000000000000 ) ) ;
#39486 = ORIENTED_EDGE ( 'NONE', *, *, #5785, .T. ) ;
#39485 = FILL_AREA_STYLE_COLOUR ( '', #55722 ) ;
#39487 = EDGE_LOOP ( 'NONE', ( #26883, #67317, #17830, #17831, #51459, #19129, #20482, #43296 ) ) ;
#39488 = DIRECTION ( 'NONE',  ( 1.836970198721029934E-16, 1.836970198721010706E-16, -1.000000000000000000 ) ) ;
#39489 = VECTOR ( 'NONE', #29585, 1000.000000000000000 ) ;
#39490 = CARTESIAN_POINT ( 'NONE',  ( -6.775514141871427753, -7.408280051175141878, 54.00000000000000711 ) ) ;
#39491 = LINE ( 'NONE', #56456, #61835 ) ;
#39492 = FACE_OUTER_BOUND ( 'NONE', #51786, .T. ) ;
#39493 = CIRCLE ( 'NONE', #9023, 3.499999999999855227 ) ;
#39494 = DIRECTION ( 'NONE',  ( -1.000000000000000000, 0.000000000000000000, 0.000000000000000000 ) ) ;
#39495 = VERTEX_POINT ( 'NONE', #21949 ) ;
#39496 = CYLINDRICAL_SURFACE ( 'NONE', #38058, 0.5000000000001357803 ) ;
#39498 = AXIS2_PLACEMENT_3D ( 'NONE', #21754, #10106, #31680 ) ;
#39497 = CARTESIAN_POINT ( 'NONE',  ( -30.00000000000000000, -11.50000000000000000, 15.00000000000000000 ) ) ;
#39499 = DIRECTION ( 'NONE',  ( 1.000000000000000000, -0.000000000000000000, 0.000000000000000000 ) ) ;
#39500 = VECTOR ( 'NONE', #11773, 1000.000000000000000 ) ;
#39501 = LINE ( 'NONE', #1670, #45758 ) ;
#39502 = CARTESIAN_POINT ( 'NONE',  ( 7.250000000000004441, 7.450000000000001954, -18.50000000000000000 ) ) ;
#39503 = DIRECTION ( 'NONE',  ( 0.000000000000000000, 1.000000000000000000, 0.000000000000000000 ) ) ;
#39504 = VECTOR ( 'NONE', #29552, 1000.000000000000000 ) ;
#39505 = LINE ( 'NONE', #40554, #38642 ) ;
#39506 = VERTEX_POINT ( 'NONE', #37529 ) ;
#39507 = CARTESIAN_POINT ( 'NONE',  ( 7.616533956692244089, 8.393516549646575342, 455.0000000000000568 ) ) ;
#39508 = CARTESIAN_POINT ( 'NONE',  ( 7.826483450353380000, -12.00648345035349251, 455.0000000000000568 ) ) ;
#39509 = VERTEX_POINT ( 'NONE', #32219 ) ;
#39510 = DIRECTION ( 'NONE',  ( 1.000000000000000000, 0.000000000000000000, 0.000000000000000000 ) ) ;
#39511 = DIRECTION ( 'NONE',  ( 0.8660254037850523279, 0.000000000000000000, -0.4999999999989371835 ) ) ;
#39512 = DIRECTION ( 'NONE',  ( 0.000000000000000000, 0.000000000000000000, -1.000000000000000000 ) ) ;
#39513 = LINE ( 'NONE', #61074, #7099 ) ;
#39514 = DIRECTION ( 'NONE',  ( -1.836970198721029934E-16, 1.836970198721036590E-16, -1.000000000000000000 ) ) ;
#39515 = ADVANCED_FACE ( 'NONE', ( #53796 ), #26922, .T. ) ;
#39516 = VERTEX_POINT ( 'NONE', #17329 ) ;
#39517 = LINE ( 'NONE', #61078, #260 ) ;
#39518 = EDGE_LOOP ( 'NONE', ( #69275, #45919, #35177, #24943 ) ) ;
#39519 = EDGE_CURVE ( 'NONE', #24440, #58530, #59784, .T. ) ;
#39520 = CIRCLE ( 'NONE', #13539, 0.1749999999999989342 ) ;
#39521 = LINE ( 'NONE', #28917, #36801 ) ;
#39522 = ORIENTED_EDGE ( 'NONE', *, *, #56164, .T. ) ;
#39523 = CARTESIAN_POINT ( 'NONE',  ( -7.250000000000000888, 7.250000000000001776, -30.00000000000001066 ) ) ;
#39524 = PLANE ( 'NONE',  #52500 ) ;
#39525 = FACE_OUTER_BOUND ( 'NONE', #4366, .T. ) ;
#39526 = VERTEX_POINT ( 'NONE', #6387 ) ;
#39527 = EDGE_LOOP ( 'NONE', ( #61709, #66775, #12941, #11096 ) ) ;
#39528 = CARTESIAN_POINT ( 'NONE',  ( 12.00648345035340903, 7.813516549646560172, 455.0000000000000568 ) ) ;
#39529 = VECTOR ( 'NONE', #63687, 1000.000000000000000 ) ;
#39531 = ORIENTED_EDGE ( 'NONE', *, *, #49004, .F. ) ;
#39530 = ADVANCED_FACE ( 'NONE', ( #49176 ), #16997, .T. ) ;
#39532 = ORIENTED_EDGE ( 'NONE', *, *, #25297, .T. ) ;
#39533 = LINE ( 'NONE', #29621, #27047 ) ;
#39534 = PLANE ( 'NONE',  #66318 ) ;
#39536 = DIRECTION ( 'NONE',  ( 0.000000000000000000, 0.000000000000000000, -1.000000000000000000 ) ) ;
#39535 = CIRCLE ( 'NONE', #12423, 0.3999999999993835154 ) ;
#39537 = ORIENTED_EDGE ( 'NONE', *, *, #62192, .T. ) ;
#39538 = CARTESIAN_POINT ( 'NONE',  ( 7.250000000000005329, -7.249999999999998224, -22.50000000000000000 ) ) ;
#39540 = DIRECTION ( 'NONE',  ( 0.000000000000000000, 0.000000000000000000, 1.000000000000000000 ) ) ;
#39539 = DIRECTION ( 'NONE',  ( 0.000000000000000000, 0.000000000000000000, -1.000000000000000000 ) ) ;
#39541 = ORIENTED_EDGE ( 'NONE', *, *, #35026, .T. ) ;
#39543 = VERTEX_POINT ( 'NONE', #747 ) ;
#39542 = CARTESIAN_POINT ( 'NONE',  ( 8.093267424590459669, 8.697938382363064491, 54.00000000000000711 ) ) ;
#39544 = ORIENTED_EDGE ( 'NONE', *, *, #17970, .F. ) ;
#39545 = AXIS2_PLACEMENT_3D ( 'NONE', #31389, #53641, #68505 ) ;
#39546 = CARTESIAN_POINT ( 'NONE',  ( 163.9999999999999432, 4.250072512722171625E-13, 8.326672683888295779E-14 ) ) ;
#39548 = AXIS2_PLACEMENT_3D ( 'NONE', #10027, #69779, #5063 ) ;
#39547 = LINE ( 'NONE', #18325, #10743 ) ;
#39549 = EDGE_LOOP ( 'NONE', ( #15227, #57764, #17129, #63719 ) ) ;
#39550 = CARTESIAN_POINT ( 'NONE',  ( 8.250000000000005329, -8.249999999999998224, -26.00000000000001066 ) ) ;
#39551 = CARTESIAN_POINT ( 'NONE',  ( 7.250000000000005329, 8.250000000000001776, -17.00000000000000000 ) ) ;
#39552 = ORIENTED_EDGE ( 'NONE', *, *, #24203, .T. ) ;
#39553 = VERTEX_POINT ( 'NONE', #22982 ) ;
#39554 = CIRCLE ( 'NONE', #57647, 4.500000000000190958 ) ;
#39555 = AXIS2_PLACEMENT_3D ( 'NONE', #53939, #189, #21748 ) ;
#39556 = LINE ( 'NONE', #7377, #26811 ) ;
#39557 = DIRECTION ( 'NONE',  ( -0.4999999999999755196, 0.8660254037844526964, 2.509347957447861534E-16 ) ) ;
#39558 = ORIENTED_EDGE ( 'NONE', *, *, #37172, .T. ) ;
#39559 = ADVANCED_FACE ( 'NONE', ( #22310 ), #33257, .F. ) ;
#39560 = LINE ( 'NONE', #59760, #10514 ) ;
#39561 = DIRECTION ( 'NONE',  ( -1.000000000000000000, 1.047444401652940007E-14, 0.000000000000000000 ) ) ;
#39562 = LINE ( 'NONE', #49840, #7932 ) ;
#39563 = VERTEX_POINT ( 'NONE', #49858 ) ;
#39564 = DIRECTION ( 'NONE',  ( 1.836970198721029934E-16, 1.836970198721010706E-16, -1.000000000000000000 ) ) ;
#39565 = AXIS2_PLACEMENT_3D ( 'NONE', #50172, #28953, #10366 ) ;
#39566 = CARTESIAN_POINT ( 'NONE',  ( -28.00000000000000000, -15.50000000000000000, -20.05051025721700242 ) ) ;
#39568 = ORIENTED_EDGE ( 'NONE', *, *, #40530, .T. ) ;
#39567 = SURFACE_STYLE_FILL_AREA ( #12688 ) ;
#39570 = ORIENTED_EDGE ( 'NONE', *, *, #8153, .F. ) ;
#39569 = CARTESIAN_POINT ( 'NONE',  ( 7.272650909786598561, -7.811466277050764795, 195.0000000000000284 ) ) ;
#39571 = CARTESIAN_POINT ( 'NONE',  ( 3.677663764522614454, -4.149127210878761574, 26.00000000000000711 ) ) ;
#39572 = EDGE_CURVE ( 'NONE', #24415, #22946, #65096, .T. ) ;
#39573 = CARTESIAN_POINT ( 'NONE',  ( 8.250000000000005329, 0.000000000000000000, -20.50000000000000000 ) ) ;
#39574 = CARTESIAN_POINT ( 'NONE',  ( 41.09999999999999432, -14.06939075806900163, 20.80000000000000426 ) ) ;
#39575 = CARTESIAN_POINT ( 'NONE',  ( -9.689726262117227762, 8.916576262117214213, 26.00000000000000711 ) ) ;
#39576 = EDGE_CURVE ( 'NONE', #20601, #30238, #16662, .T. ) ;
#39577 = DIRECTION ( 'NONE',  ( 0.000000000000000000, 1.000000000000000000, 0.000000000000000000 ) ) ;
#39578 = EDGE_LOOP ( 'NONE', ( #34745, #45059, #39113, #64282 ) ) ;
#39579 = DIRECTION ( 'NONE',  ( -1.000000000000000000, 0.000000000000000000, 0.000000000000000000 ) ) ;
#39580 = DIRECTION ( 'NONE',  ( 0.000000000000000000, -0.000000000000000000, 1.000000000000000000 ) ) ;
#39581 = AXIS2_PLACEMENT_3D ( 'NONE', #29142, #45748, #60961 ) ;
#39582 = PLANE ( 'NONE',  #11905 ) ;
#39584 = VERTEX_POINT ( 'NONE', #54491 ) ;
#39583 = DIRECTION ( 'NONE',  ( -1.000000000000000000, 0.000000000000000000, 0.000000000000000000 ) ) ;
#39585 = AXIS2_PLACEMENT_3D ( 'NONE', #41055, #23750, #19487 ) ;
#39586 = CARTESIAN_POINT ( 'NONE',  ( 10.50000000000000000, -9.690000000000001279, 0.000000000000000000 ) ) ;
#39587 = LINE ( 'NONE', #61150, #40874 ) ;
#39588 = AXIS2_PLACEMENT_3D ( 'NONE', #48494, #5716, #38242 ) ;
#39589 = ORIENTED_EDGE ( 'NONE', *, *, #22219, .T. ) ;
#39590 = DIRECTION ( 'NONE',  ( 1.000000000000000000, 0.000000000000000000, 0.000000000000000000 ) ) ;
#39591 = FACE_OUTER_BOUND ( 'NONE', #54900, .T. ) ;
#39592 = ORIENTED_EDGE ( 'NONE', *, *, #34073, .F. ) ;
#39593 = VECTOR ( 'NONE', #1966, 1000.000000000000000 ) ;
#39594 = CIRCLE ( 'NONE', #43148, 0.5000000000079362072 ) ;
#39595 = CARTESIAN_POINT ( 'NONE',  ( 4.396432944014529554, 8.393516549646633962, 195.0000000000000284 ) ) ;
#39596 = CARTESIAN_POINT ( 'NONE',  ( -7.250000000000000888, 7.250000000000001776, -25.50000000000000355 ) ) ;
#39597 = FACE_BOUND ( 'NONE', #61871, .T. ) ;
#39598 = CARTESIAN_POINT ( 'NONE',  ( 1.480523737882794233, -8.612468434717218457, 54.00000000000000711 ) ) ;
#39599 = AXIS2_PLACEMENT_3D ( 'NONE', #36959, #9727, #4436 ) ;
#39600 = EDGE_CURVE ( 'NONE', #40737, #25493, #43862, .T. ) ;
#39601 = PLANE ( 'NONE',  #63612 ) ;
#39602 = ORIENTED_EDGE ( 'NONE', *, *, #53871, .F. ) ;
#39603 = ADVANCED_FACE ( 'NONE', ( #65772 ), #44897, .T. ) ;
#39604 = LINE ( 'NONE', #34292, #69901 ) ;
#39605 = ORIENTED_EDGE ( 'NONE', *, *, #6199, .T. ) ;
#39606 = ADVANCED_FACE ( 'NONE', ( #65438 ), #28982, .T. ) ;
#39607 = ORIENTED_EDGE ( 'NONE', *, *, #25208, .F. ) ;
#39608 = CARTESIAN_POINT ( 'NONE',  ( 283.0000000000000568, -38.15000000000000568, -13.19999999999999929 ) ) ;
#39609 = VECTOR ( 'NONE', #38808, 1000.000000000000114 ) ;
#39610 = ADVANCED_FACE ( 'NONE', ( #1087 ), #54830, .F. ) ;
#39611 = EDGE_CURVE ( 'NONE', #44584, #23076, #28630, .T. ) ;
#39612 = CARTESIAN_POINT ( 'NONE',  ( -9.234937905884020637, 9.942044687070460185, 455.0000000000000568 ) ) ;
#39613 = DIRECTION ( 'NONE',  ( 0.000000000000000000, -0.000000000000000000, 1.000000000000000000 ) ) ;
#39614 = ORIENTED_EDGE ( 'NONE', *, *, #30964, .F. ) ;
#39615 = EDGE_CURVE ( 'NONE', #41426, #48554, #38900, .T. ) ;
#39616 = ORIENTED_EDGE ( 'NONE', *, *, #41435, .F. ) ;
#39617 = DIRECTION ( 'NONE',  ( 0.000000000000000000, 0.000000000000000000, 1.000000000000000000 ) ) ;
#39619 = ORIENTED_EDGE ( 'NONE', *, *, #36911, .F. ) ;
#39618 = ADVANCED_FACE ( 'NONE', ( #55855 ), #44197, .F. ) ;
#39620 = CYLINDRICAL_SURFACE ( 'NONE', #48450, 0.3499999999999614531 ) ;
#39621 = DIRECTION ( 'NONE',  ( 0.000000000000000000, 1.000000000000000000, 0.000000000000000000 ) ) ;
#39622 = CARTESIAN_POINT ( 'NONE',  ( -16.94999999999999929, -0.2000000000000000111, 22.50000000000000000 ) ) ;
#39623 = CARTESIAN_POINT ( 'NONE',  ( 152.5922698879801942, -30.42541106249863603, 0.000000000000000000 ) ) ;
#39625 = CARTESIAN_POINT ( 'NONE',  ( 8.250000000000005329, 8.250000000000001776, -26.00000000000001066 ) ) ;
#39624 = DIRECTION ( 'NONE',  ( -3.540573132209561620E-15, -1.000000000000000000, 0.000000000000000000 ) ) ;
#39626 = ORIENTED_EDGE ( 'NONE', *, *, #13100, .F. ) ;
#39628 = ORIENTED_EDGE ( 'NONE', *, *, #1156, .T. ) ;
#39627 = PLANE ( 'NONE',  #54460 ) ;
#39629 = VERTEX_POINT ( 'NONE', #28287 ) ;
#39630 = VERTEX_POINT ( 'NONE', #17683 ) ;
#39631 = CARTESIAN_POINT ( 'NONE',  ( -8.566576262117346019, -8.930623737882765312, 26.00000000000000000 ) ) ;
#39632 = FACE_OUTER_BOUND ( 'NONE', #50993, .T. ) ;
#39633 = AXIS2_PLACEMENT_3D ( 'NONE', #828, #60188, #33330 ) ;
#39634 = CARTESIAN_POINT ( 'NONE',  ( -15.50000000000000000, -0.4000000000005236034, -22.50000000000000000 ) ) ;
#39635 = EDGE_CURVE ( 'NONE', #29071, #5578, #12352, .T. ) ;
#39636 = ORIENTED_EDGE ( 'NONE', *, *, #66230, .F. ) ;
#39637 = ORIENTED_EDGE ( 'NONE', *, *, #28478, .F. ) ;
#39638 = VECTOR ( 'NONE', #58232, 1000.000000000000000 ) ;
#39639 = CARTESIAN_POINT ( 'NONE',  ( -8.393516549646712122, 5.655420232009161552, 455.0000000000000568 ) ) ;
#39640 = CARTESIAN_POINT ( 'NONE',  ( 15.70313394608856683, -0.2715358723588608414, -21.17390376548178210 ) ) ;
#39641 = ORIENTED_EDGE ( 'NONE', *, *, #38430, .F. ) ;
#39642 = AXIS2_PLACEMENT_3D ( 'NONE', #22756, #10756, #65218 ) ;
#39643 = CIRCLE ( 'NONE', #58863, 4.500000000000191847 ) ;
#39644 = ADVANCED_FACE ( 'NONE', ( #34269 ), #7406, .F. ) ;
#39645 = ORIENTED_EDGE ( 'NONE', *, *, #18362, .T. ) ;
#39646 = CARTESIAN_POINT ( 'NONE',  ( 7.272650909786644746, 7.798499376343933420, 455.0000000000000568 ) ) ;
#39647 = CARTESIAN_POINT ( 'NONE',  ( -11.99351654964671354, 7.813516549646603693, 195.0000000000000284 ) ) ;
#39648 = EDGE_LOOP ( 'NONE', ( #31076, #7430, #25865, #33366 ) ) ;
#39649 = AXIS2_PLACEMENT_3D ( 'NONE', #32606, #53833, #69743 ) ;
#39650 = VECTOR ( 'NONE', #45938, 1000.000000000000000 ) ;
#39651 = CARTESIAN_POINT ( 'NONE',  ( 289.5000000000001705, -0.5000000000000781597, -27.00000000000004263 ) ) ;
#39653 = ORIENTED_EDGE ( 'NONE', *, *, #31168, .F. ) ;
#39652 = CARTESIAN_POINT ( 'NONE',  ( 9.306483450353415066, 10.08346604330773744, 455.0000000000000568 ) ) ;
#39654 = VERTEX_POINT ( 'NONE', #40288 ) ;
#39656 = LINE ( 'NONE', #65515, #27677 ) ;
#39655 = CIRCLE ( 'NONE', #57745, 0.3500000000002719824 ) ;
#39657 = DIRECTION ( 'NONE',  ( 0.000000000000000000, 0.000000000000000000, 1.000000000000000000 ) ) ;
#39658 = DIRECTION ( 'NONE',  ( 0.000000000000000000, 0.000000000000000000, -1.000000000000000000 ) ) ;
#39659 = CARTESIAN_POINT ( 'NONE',  ( 7.250000000000005329, -7.449999999999998401, -9.500000000000001776 ) ) ;
#39660 = CARTESIAN_POINT ( 'NONE',  ( 0.000000000000000000, 8.250000000000001776, -12.00000000000000000 ) ) ;
#39661 = DIRECTION ( 'NONE',  ( 0.000000000000000000, 0.000000000000000000, 1.000000000000000000 ) ) ;
#39662 = EDGE_CURVE ( 'NONE', #29102, #27000, #27051, .T. ) ;
#39663 = CARTESIAN_POINT ( 'NONE',  ( 6.364920264886885448, -6.836383711243021466, 54.00000000000000711 ) ) ;
#39664 = ORIENTED_EDGE ( 'NONE', *, *, #44412, .T. ) ;
#39665 = LINE ( 'NONE', #61224, #57474 ) ;
#39667 = ORIENTED_EDGE ( 'NONE', *, *, #63656, .F. ) ;
#39666 = FACE_OUTER_BOUND ( 'NONE', #45383, .T. ) ;
#39668 = DIRECTION ( 'NONE',  ( -1.000000000000000000, 0.000000000000000000, 0.000000000000000000 ) ) ;
#39669 = FACE_OUTER_BOUND ( 'NONE', #49564, .T. ) ;
#39670 = AXIS2_PLACEMENT_3D ( 'NONE', #3059, #67413, #24967 ) ;
#39671 = ADVANCED_FACE ( 'NONE', ( #24381 ), #45945, .F. ) ;
#39672 = CARTESIAN_POINT ( 'NONE',  ( 7.000000000000000000, -31.99999999999889866, 7.899999999997660893 ) ) ;
#39673 = EDGE_CURVE ( 'NONE', #52904, #14583, #1110, .T. ) ;
#39674 = FACE_OUTER_BOUND ( 'NONE', #30594, .T. ) ;
#39675 = DIRECTION ( 'NONE',  ( -1.000000000000000000, 0.000000000000000000, 0.000000000000000000 ) ) ;
#39676 = EDGE_CURVE ( 'NONE', #39553, #127, #41728, .T. ) ;
#39677 = ORIENTED_EDGE ( 'NONE', *, *, #34234, .F. ) ;
#39678 = ADVANCED_FACE ( 'NONE', ( #19072 ), #5602, .T. ) ;
#39679 = EDGE_CURVE ( 'NONE', #60441, #49549, #55263, .T. ) ;
#39680 = ORIENTED_EDGE ( 'NONE', *, *, #13982, .T. ) ;
#39681 = DIRECTION ( 'NONE',  ( -0.8660254037844363761, 0.5000000000000038858, 0.000000000000000000 ) ) ;
#39682 = VECTOR ( 'NONE', #8529, 1000.000000000000000 ) ;
#39683 = CARTESIAN_POINT ( 'NONE',  ( 7.450000000000004619, -1.336933437520057563E-15, -23.50000000000000000 ) ) ;
#39684 = EDGE_CURVE ( 'NONE', #38554, #62211, #42845, .T. ) ;
#39685 = COLOUR_RGB ( '', 0.09019608, 0.27058824, 0.51372549) ;
#39686 = CARTESIAN_POINT ( 'NONE',  ( 15.00000000000000000, -20.40000000000000213, -12.40000000000000213 ) ) ;
#39687 = ORIENTED_EDGE ( 'NONE', *, *, #44528, .F. ) ;
#39688 = ADVANCED_FACE ( 'NONE', ( #57603 ), #13057, .T. ) ;
#39689 = DIRECTION ( 'NONE',  ( 0.000000000000000000, -0.000000000000000000, 1.000000000000000000 ) ) ;
#39690 = VERTEX_POINT ( 'NONE', #56210 ) ;
#39691 = VERTEX_POINT ( 'NONE', #18355 ) ;
#39692 = EDGE_CURVE ( 'NONE', #65388, #32021, #29671, .T. ) ;
#39693 = CARTESIAN_POINT ( 'NONE',  ( 7.250000000000005329, -7.449999999999998401, -18.00000000000000000 ) ) ;
#39694 = CARTESIAN_POINT ( 'NONE',  ( 7.250000000000005329, 8.250000000000001776, -8.000000000000000000 ) ) ;
#39695 = ORIENTED_EDGE ( 'NONE', *, *, #30977, .F. ) ;
#39696 = DIRECTION ( 'NONE',  ( 0.000000000000000000, -3.673940397442059868E-16, 1.000000000000000000 ) ) ;
#39697 = CIRCLE ( 'NONE', #53261, 3.499999999999850342 ) ;
#39698 = CYLINDRICAL_SURFACE ( 'NONE', #54672, 1.621000000000000885 ) ;
#39699 = CARTESIAN_POINT ( 'NONE',  ( 7.000000000000000000, -38.09999999999885034, -7.900000000002049383 ) ) ;
#39700 = EDGE_CURVE ( 'NONE', #67984, #6255, #9169, .T. ) ;
#39701 = ORIENTED_EDGE ( 'NONE', *, *, #25345, .T. ) ;
#39703 = ORIENTED_EDGE ( 'NONE', *, *, #25150, .F. ) ;
#39702 = DIRECTION ( 'NONE',  ( 0.000000000000000000, 0.000000000000000000, 1.000000000000000000 ) ) ;
#39704 = EDGE_CURVE ( 'NONE', #21321, #34472, #25086, .T. ) ;
#39705 = CARTESIAN_POINT ( 'NONE',  ( 7.250000000000005329, -8.249999999999998224, -24.00000000000000000 ) ) ;
#39706 = CARTESIAN_POINT ( 'NONE',  ( 7.250000000000004441, 7.450000000000001954, -21.50000000000000000 ) ) ;
#39707 = CARTESIAN_POINT ( 'NONE',  ( 14.50000000000000000, -42.50000000000000000, 15.10000000000000142 ) ) ;
#39708 = DIRECTION ( 'NONE',  ( -1.000000000000000000, 0.000000000000000000, 0.000000000000000000 ) ) ;
#39709 = CIRCLE ( 'NONE', #19428, 0.3499999999999597877 ) ;
#39710 = CYLINDRICAL_SURFACE ( 'NONE', #42398, 4.000000000000000000 ) ;
#39711 = CARTESIAN_POINT ( 'NONE',  ( -9.547976262117304103, -8.144523737882758851, 54.00000000000000711 ) ) ;
#39712 = ORIENTED_EDGE ( 'NONE', *, *, #37314, .F. ) ;
#39713 = ORIENTED_EDGE ( 'NONE', *, *, #32111, .T. ) ;
#39714 = ORIENTED_EDGE ( 'NONE', *, *, #52923, .T. ) ;
#39715 = CARTESIAN_POINT ( 'NONE',  ( 16.75000000000000000, -2.500000000000000000, -23.22168783648699986 ) ) ;
#39716 = DIRECTION ( 'NONE',  ( 0.000000000000000000, 1.550842787525658429E-12, 1.000000000000000000 ) ) ;
#39717 = DIRECTION ( 'NONE',  ( -1.000000000000000000, 0.000000000000000000, 0.000000000000000000 ) ) ;
#39718 = VERTEX_POINT ( 'NONE', #56891 ) ;
#39719 = ORIENTED_EDGE ( 'NONE', *, *, #32689, .T. ) ;
#39720 = VERTEX_POINT ( 'NONE', #67158 ) ;
#39721 = DIRECTION ( 'NONE',  ( 0.000000000000000000, 1.000000000000000000, 0.000000000000000000 ) ) ;
#39722 = VERTEX_POINT ( 'NONE', #3169 ) ;
#39723 = VERTEX_POINT ( 'NONE', #57254 ) ;
#39724 = AXIS2_PLACEMENT_3D ( 'NONE', #60731, #49782, #11254 ) ;
#39725 = ORIENTED_EDGE ( 'NONE', *, *, #11211, .T. ) ;
#39726 = ADVANCED_FACE ( 'NONE', ( #62543 ), #18719, .T. ) ;
#39727 = ORIENTED_EDGE ( 'NONE', *, *, #43594, .F. ) ;
#39728 = LINE ( 'NONE', #34072, #31666 ) ;
#39729 = CIRCLE ( 'NONE', #57816, 0.2000000000000005107 ) ;
#39731 = VERTEX_POINT ( 'NONE', #14113 ) ;
#39730 = CARTESIAN_POINT ( 'NONE',  ( 289.5000000000000000, 0.000000000000000000, -26.50000000000000000 ) ) ;
#39732 = EDGE_CURVE ( 'NONE', #38207, #58876, #67719, .T. ) ;
#39733 = CARTESIAN_POINT ( 'NONE',  ( 8.250000000000005329, 7.250000000000000888, -20.00000000000000000 ) ) ;
#39734 = FACE_OUTER_BOUND ( 'NONE', #68544, .T. ) ;
#39735 = FACE_OUTER_BOUND ( 'NONE', #45763, .T. ) ;
#39736 = EDGE_CURVE ( 'NONE', #56607, #58645, #3516, .T. ) ;
#39738 = ORIENTED_EDGE ( 'NONE', *, *, #41865, .F. ) ;
#39737 = DIRECTION ( 'NONE',  ( -0.7671651518152985405, -0.6414496315691592399, 0.000000000000000000 ) ) ;
#39739 = EDGE_LOOP ( 'NONE', ( #45296, #18874, #60814, #14180 ) ) ;
#39740 = EDGE_CURVE ( 'NONE', #29722, #24086, #19164, .T. ) ;
#39741 = LINE ( 'NONE', #18178, #50891 ) ;
#39742 = AXIS2_PLACEMENT_3D ( 'NONE', #58536, #5127, #42605 ) ;
#39743 = CYLINDRICAL_SURFACE ( 'NONE', #660, 25.39999999999999858 ) ;
#39744 = FACE_BOUND ( 'NONE', #4011, .T. ) ;
#39745 = EDGE_CURVE ( 'NONE', #62405, #527, #62913, .T. ) ;
#39746 = ORIENTED_EDGE ( 'NONE', *, *, #4171, .F. ) ;
#39747 = DIRECTION ( 'NONE',  ( 0.6414496315691420314, -0.7671651518153128624, 0.000000000000000000 ) ) ;
#39748 = DIRECTION ( 'NONE',  ( -0.7671651518153131954, -0.6414496315691415873, 0.000000000000000000 ) ) ;
#39749 = AXIS2_PLACEMENT_3D ( 'NONE', #20493, #11265, #26160 ) ;
#39750 = DIRECTION ( 'NONE',  ( 1.000000000000000000, -0.000000000000000000, -0.000000000000000000 ) ) ;
#39751 = VERTEX_POINT ( 'NONE', #21183 ) ;
#39752 = DIRECTION ( 'NONE',  ( -0.000000000000000000, -0.000000000000000000, -1.000000000000000000 ) ) ;
#39753 = EDGE_CURVE ( 'NONE', #30052, #46347, #6742, .T. ) ;
#39754 = CIRCLE ( 'NONE', #68041, 24.99999999998784972 ) ;
#39755 = FACE_OUTER_BOUND ( 'NONE', #30444, .T. ) ;
#39756 = DIRECTION ( 'NONE',  ( 1.000000000000000000, -0.000000000000000000, -0.000000000000000000 ) ) ;
#39757 = EDGE_CURVE ( 'NONE', #4958, #58882, #54055, .T. ) ;
#39758 = ORIENTED_EDGE ( 'NONE', *, *, #28183, .F. ) ;
#39759 = DIRECTION ( 'NONE',  ( 0.000000000000000000, 1.000000000000000000, 0.000000000000000000 ) ) ;
#39760 = DIRECTION ( 'NONE',  ( 0.000000000000000000, -3.673940397442059868E-16, 1.000000000000000000 ) ) ;
#39761 = DIRECTION ( 'NONE',  ( -0.000000000000000000, 1.000000000000000000, -0.000000000000000000 ) ) ;
#39762 = EDGE_CURVE ( 'NONE', #65808, #2847, #45137, .T. ) ;
#39763 = ORIENTED_EDGE ( 'NONE', *, *, #29983, .F. ) ;
#39764 = CARTESIAN_POINT ( 'NONE',  ( 10.31452373788280497, 6.642976262117183062, 54.00000000000000711 ) ) ;
#39765 = CARTESIAN_POINT ( 'NONE',  ( -7.250000000000000888, 7.250000000000001776, -9.500000000000001776 ) ) ;
#39766 = LINE ( 'NONE', #23518, #10500 ) ;
#39767 = DIRECTION ( 'NONE',  ( -1.000000000000000000, 0.000000000000000000, 0.000000000000000000 ) ) ;
#39768 = CARTESIAN_POINT ( 'NONE',  ( 11.00000000000000000, -12.00000000000000000, 10.20500000000000007 ) ) ;
#39769 = ORIENTED_EDGE ( 'NONE', *, *, #43121, .T. ) ;
#39770 = FACE_OUTER_BOUND ( 'NONE', #66012, .T. ) ;
#39771 = CARTESIAN_POINT ( 'NONE',  ( -8.249999999999996447, 8.250000000000001776, 5.000000000000000000 ) ) ;
#39772 = VECTOR ( 'NONE', #36306, 1000.000000000000000 ) ;
#39773 = CARTESIAN_POINT ( 'NONE',  ( 47.00000000000000000, -0.7500000000000000000, -3.418698582794335028 ) ) ;
#39774 = DIRECTION ( 'NONE',  ( 0.000000000000000000, 0.000000000000000000, -1.000000000000000000 ) ) ;
#39775 = LINE ( 'NONE', #60998, #37356 ) ;
#39776 = VECTOR ( 'NONE', #52297, 1000.000000000000000 ) ;
#39777 = EDGE_CURVE ( 'NONE', #56924, #7012, #47436, .T. ) ;
#39778 = ORIENTED_EDGE ( 'NONE', *, *, #52302, .T. ) ;
#39780 = EDGE_LOOP ( 'NONE', ( #41493, #27833, #22185, #30143 ) ) ;
#39779 = DIRECTION ( 'NONE',  ( 0.000000000000000000, 3.673940397442059868E-16, -1.000000000000000000 ) ) ;
#39781 = ADVANCED_FACE ( 'NONE', ( #46996 ), #32132, .F. ) ;
#39782 = DIRECTION ( 'NONE',  ( -1.836970198721029934E-16, 1.836970198721036590E-16, -1.000000000000000000 ) ) ;
#39783 = DIRECTION ( 'NONE',  ( 1.000000000000000000, 0.000000000000000000, 0.000000000000000000 ) ) ;
#39784 = ORIENTED_EDGE ( 'NONE', *, *, #16397, .T. ) ;
#39785 = PLANE ( 'NONE',  #22801 ) ;
#39786 = ORIENTED_EDGE ( 'NONE', *, *, #25751, .F. ) ;
#39787 = LINE ( 'NONE', #57728, #15405 ) ;
#39788 = VERTEX_POINT ( 'NONE', #68919 ) ;
#39789 = ORIENTED_EDGE ( 'NONE', *, *, #17746, .T. ) ;
#39790 = DIRECTION ( 'NONE',  ( -1.000000000000000000, 0.000000000000000000, 0.000000000000000000 ) ) ;
#39791 = DIRECTION ( 'NONE',  ( 0.000000000000000000, 1.000000000000000000, 0.000000000000000000 ) ) ;
#39792 = LINE ( 'NONE', #7969, #14565 ) ;
#39793 = DIRECTION ( 'NONE',  ( 0.000000000000000000, 0.000000000000000000, 1.000000000000000000 ) ) ;
#39794 = AXIS2_PLACEMENT_3D ( 'NONE', #47559, #20673, #26688 ) ;
#39795 = ORIENTED_EDGE ( 'NONE', *, *, #10390, .F. ) ;
#39796 = ORIENTED_EDGE ( 'NONE', *, *, #19955, .T. ) ;
#39797 = CYLINDRICAL_SURFACE ( 'NONE', #17713, 3.499999999999038547 ) ;
#39798 = AXIS2_PLACEMENT_3D ( 'NONE', #31003, #47967, #21441 ) ;
#39799 = CYLINDRICAL_SURFACE ( 'NONE', #46334, 24.99999999998794920 ) ;
#39800 = ORIENTED_EDGE ( 'NONE', *, *, #43926, .T. ) ;
#39801 = VECTOR ( 'NONE', #24490, 1000.000000000000000 ) ;
#39802 = ORIENTED_EDGE ( 'NONE', *, *, #34081, .T. ) ;
#39803 = ORIENTED_EDGE ( 'NONE', *, *, #20888, .T. ) ;
#39804 = CARTESIAN_POINT ( 'NONE',  ( 8.250000000000005329, -8.249999999999998224, -26.00000000000001066 ) ) ;
#39805 = AXIS2_PLACEMENT_3D ( 'NONE', #31451, #53016, #41333 ) ;
#39807 = ORIENTED_EDGE ( 'NONE', *, *, #58924, .F. ) ;
#39806 = CARTESIAN_POINT ( 'NONE',  ( 6.832023737882818359, -9.912023737882819319, 54.00000000000000711 ) ) ;
#39808 = EDGE_CURVE ( 'NONE', #55579, #67623, #42736, .T. ) ;
#39809 = DIRECTION ( 'NONE',  ( 0.000000000000000000, 0.000000000000000000, -1.000000000000000000 ) ) ;
#39810 = AXIS2_PLACEMENT_3D ( 'NONE', #18419, #19481, #45297 ) ;
#39811 = LINE ( 'NONE', #61377, #30651 ) ;
#39812 = ORIENTED_EDGE ( 'NONE', *, *, #65488, .F. ) ;
#39813 = ADVANCED_FACE ( 'NONE', ( #25431 ), #4230, .T. ) ;
#39814 = ORIENTED_EDGE ( 'NONE', *, *, #9044, .F. ) ;
#39815 = EDGE_CURVE ( 'NONE', #42264, #44065, #36746, .T. ) ;
#39816 = ADVANCED_FACE ( 'NONE', ( #4574 ), #64650, .F. ) ;
#39817 = DIRECTION ( 'NONE',  ( -1.000000000000000000, 0.000000000000000000, 0.000000000000000000 ) ) ;
#39818 = DIRECTION ( 'NONE',  ( -0.000000000000000000, -0.000000000000000000, -1.000000000000000000 ) ) ;
#39819 = EDGE_CURVE ( 'NONE', #38923, #21386, #64316, .T. ) ;
#39820 = EDGE_CURVE ( 'NONE', #4332, #53128, #58321, .T. ) ;
#39821 = CIRCLE ( 'NONE', #40949, 4.000000000000000000 ) ;
#39822 = LINE ( 'NONE', #1649, #57480 ) ;
#39823 = EDGE_CURVE ( 'NONE', #17091, #28438, #10912, .T. ) ;
#39824 = CARTESIAN_POINT ( 'NONE',  ( -9.689726262117227762, 9.689726262117183353, 54.00000000000000711 ) ) ;
#39825 = CARTESIAN_POINT ( 'NONE',  ( 9.900000000000000355, 21.00000000000000000, 18.00000000000000355 ) ) ;
#39826 = ORIENTED_EDGE ( 'NONE', *, *, #32434, .F. ) ;
#39827 = ORIENTED_EDGE ( 'NONE', *, *, #6206, .T. ) ;
#39828 = VECTOR ( 'NONE', #6003, 1000.000000000000000 ) ;
#39829 = FACE_OUTER_BOUND ( 'NONE', #9235, .T. ) ;
#39830 = DIRECTION ( 'NONE',  ( 0.5000000000000038858, 0.8660254037844363761, 3.181725716174712609E-16 ) ) ;
#39831 = DIRECTION ( 'NONE',  ( 0.000000000000000000, 0.000000000000000000, 1.000000000000000000 ) ) ;
#39832 = DIRECTION ( 'NONE',  ( -1.000000000000000000, 0.000000000000000000, 0.000000000000000000 ) ) ;
#39833 = ORIENTED_EDGE ( 'NONE', *, *, #63724, .F. ) ;
#39834 = CARTESIAN_POINT ( 'NONE',  ( 5.257023737882801306, 5.242976262117200470, 54.00000000000000711 ) ) ;
#39835 = LINE ( 'NONE', #2717, #1160 ) ;
#39836 = CARTESIAN_POINT ( 'NONE',  ( 15.00000000000000000, -25.60000000000000142, 15.10000000000000142 ) ) ;
#39837 = DIRECTION ( 'NONE',  ( 0.000000000000000000, 0.000000000000000000, 1.000000000000000000 ) ) ;
#39838 = AXIS2_PLACEMENT_3D ( 'NONE', #16339, #31917, #64105 ) ;
#39839 = CARTESIAN_POINT ( 'NONE',  ( -10.30047626211725742, 3.842976262117182351, 54.00000000000000711 ) ) ;
#39840 = CARTESIAN_POINT ( 'NONE',  ( -11.25000000000000178, -11.18999999999999950, -5.000000000000000000 ) ) ;
#39841 = AXIS2_PLACEMENT_3D ( 'NONE', #3890, #30049, #14133 ) ;
#39842 = DIRECTION ( 'NONE',  ( -0.000000000000000000, 0.000000000000000000, 1.000000000000000000 ) ) ;
#39843 = CIRCLE ( 'NONE', #10501, 0.9999999999999991118 ) ;
#39844 = VERTEX_POINT ( 'NONE', #16214 ) ;
#39845 = CARTESIAN_POINT ( 'NONE',  ( -7.798499376344109280, -4.740315990920159095, 455.0000000000000568 ) ) ;
#39846 = CARTESIAN_POINT ( 'NONE',  ( -9.404046420174124066, 1.853252480934674873, 195.0000000000000284 ) ) ;
#39847 = ORIENTED_EDGE ( 'NONE', *, *, #3518, .T. ) ;
#39848 = FACE_OUTER_BOUND ( 'NONE', #65981, .T. ) ;
#39849 = FACE_OUTER_BOUND ( 'NONE', #23602, .T. ) ;
#39850 = DIRECTION ( 'NONE',  ( -0.7671651518153043137, 0.6414496315691521344, 2.587583378555129776E-16 ) ) ;
#39851 = VECTOR ( 'NONE', #19059, 1000.000000000000000 ) ;
#39853 = VECTOR ( 'NONE', #3424, 1000.000000000000000 ) ;
#39852 = LINE ( 'NONE', #60740, #49959 ) ;
#39854 = CARTESIAN_POINT ( 'NONE',  ( -11.00000000000000000, -5.200000000000001066, 9.400000000000000355 ) ) ;
#39855 = ORIENTED_EDGE ( 'NONE', *, *, #19126, .F. ) ;
#39856 = DIRECTION ( 'NONE',  ( 0.000000000000000000, 0.000000000000000000, -1.000000000000000000 ) ) ;
#39857 = ADVANCED_FACE ( 'NONE', ( #9882 ), #42385, .F. ) ;
#39858 = VECTOR ( 'NONE', #49152, 1000.000000000000000 ) ;
#39859 = ORIENTED_EDGE ( 'NONE', *, *, #62513, .T. ) ;
#39860 = CARTESIAN_POINT ( 'NONE',  ( -10.50612335864049740, 6.822329165593917111, 26.00000000000000711 ) ) ;
#39861 = ORIENTED_EDGE ( 'NONE', *, *, #26288, .T. ) ;
#39862 = EDGE_CURVE ( 'NONE', #38301, #53157, #63976, .T. ) ;
#39863 = CYLINDRICAL_SURFACE ( 'NONE', #16755, 1.500000000000001332 ) ;
#39864 = AXIS2_PLACEMENT_3D ( 'NONE', #27296, #11697, #69738 ) ;
#39865 = EDGE_CURVE ( 'NONE', #29082, #29826, #6787, .T. ) ;
#39866 = FACE_OUTER_BOUND ( 'NONE', #29219, .T. ) ;
#39867 = LINE ( 'NONE', #13362, #61601 ) ;
#39868 = ORIENTED_EDGE ( 'NONE', *, *, #6724, .F. ) ;
#39869 = EDGE_LOOP ( 'NONE', ( #58026, #7019, #64365, #7371 ) ) ;
#39870 = VECTOR ( 'NONE', #25052, 1000.000000000000000 ) ;
#39871 = DIRECTION ( 'NONE',  ( 1.000000000000000000, -0.000000000000000000, -0.000000000000000000 ) ) ;
#39872 = ORIENTED_EDGE ( 'NONE', *, *, #3537, .F. ) ;
#39873 = ORIENTED_EDGE ( 'NONE', *, *, #6126, .F. ) ;
#39874 = CARTESIAN_POINT ( 'NONE',  ( -2.277516549646682709, 9.828310488885916740, 195.0000000000000284 ) ) ;
#39875 = DIRECTION ( 'NONE',  ( 0.000000000000000000, 0.000000000000000000, 1.000000000000000000 ) ) ;
#39876 = LINE ( 'NONE', #55133, #43408 ) ;
#39877 = VERTEX_POINT ( 'NONE', #32490 ) ;
#39878 = VECTOR ( 'NONE', #56175, 1000.000000000000000 ) ;
#39879 = FACE_OUTER_BOUND ( 'NONE', #24877, .T. ) ;
#39881 = CARTESIAN_POINT ( 'NONE',  ( 49.00000000000000000, -0.1999999999911795112, 8.826273045769999343E-12 ) ) ;
#39880 = DIRECTION ( 'NONE',  ( 0.000000000000000000, 0.000000000000000000, 1.000000000000000000 ) ) ;
#39882 = ORIENTED_EDGE ( 'NONE', *, *, #38098, .T. ) ;
#39884 = ORIENTED_EDGE ( 'NONE', *, *, #36428, .F. ) ;
#39883 = LINE ( 'NONE', #61450, #39878 ) ;
#39885 = EDGE_LOOP ( 'NONE', ( #11816, #44922, #52702, #48202, #1578, #12853 ) ) ;
#39886 = DIRECTION ( 'NONE',  ( -0.000000000000000000, 3.673940397442059868E-16, -1.000000000000000000 ) ) ;
#39887 = VERTEX_POINT ( 'NONE', #20128 ) ;
#39888 = ADVANCED_FACE ( 'NONE', ( #41687 ), #58663, .T. ) ;
#39889 = CARTESIAN_POINT ( 'NONE',  ( 3.157023737882792780, 4.031976262117212606, 26.00000000000000711 ) ) ;
#39890 = AXIS2_PLACEMENT_3D ( 'NONE', #16311, #5715, #27283 ) ;
#39891 = VECTOR ( 'NONE', #35721, 1000.000000000000000 ) ;
#39892 = DIRECTION ( 'NONE',  ( 0.000000000000000000, 0.000000000000000000, -1.000000000000000000 ) ) ;
#39893 = ORIENTED_EDGE ( 'NONE', *, *, #43543, .T. ) ;
#39894 = ORIENTED_EDGE ( 'NONE', *, *, #26281, .F. ) ;
#39895 = VECTOR ( 'NONE', #35970, 1000.000000000000000 ) ;
#39897 = DIRECTION ( 'NONE',  ( 0.000000000000000000, -3.673940397442059868E-16, 1.000000000000000000 ) ) ;
#39896 = AXIS2_PLACEMENT_3D ( 'NONE', #8299, #29877, #40835 ) ;
#39898 = AXIS2_PLACEMENT_3D ( 'NONE', #45721, #18862, #24524 ) ;
#39899 = DIRECTION ( 'NONE',  ( 0.000000000000000000, -0.7057491738665943037, 0.7084617869628675457 ) ) ;
#39900 = ORIENTED_EDGE ( 'NONE', *, *, #56094, .F. ) ;
#39901 = DIRECTION ( 'NONE',  ( 0.000000000000000000, 0.000000000000000000, 1.000000000000000000 ) ) ;
#39902 = DIRECTION ( 'NONE',  ( 1.000000000000000000, -0.000000000000000000, -0.000000000000000000 ) ) ;
#39903 = VECTOR ( 'NONE', #54526, 1000.000000000000000 ) ;
#39904 = EDGE_CURVE ( 'NONE', #18999, #4958, #53115, .T. ) ;
#39905 = DIRECTION ( 'NONE',  ( 0.000000000000000000, 0.000000000000000000, -1.000000000000000000 ) ) ;
#39906 = EDGE_CURVE ( 'NONE', #16863, #40309, #31659, .T. ) ;
#39907 = VERTEX_POINT ( 'NONE', #1668 ) ;
#39908 = EDGE_CURVE ( 'NONE', #29534, #36809, #9018, .T. ) ;
#39909 = CARTESIAN_POINT ( 'NONE',  ( 8.144523737882812142, 8.821682069070710952, 54.00000000000000711 ) ) ;
#39910 = CARTESIAN_POINT ( 'NONE',  ( 10.92648345035335922, 2.693516549646528091, 455.0000000000000568 ) ) ;
#39912 = ORIENTED_EDGE ( 'NONE', *, *, #44147, .F. ) ;
#39911 = CARTESIAN_POINT ( 'NONE',  ( 3.003254798005743353, 6.858227778582815404, 54.00000000000000711 ) ) ;
#39914 = EDGE_LOOP ( 'NONE', ( #21181, #47686, #64204, #11891 ) ) ;
#39913 = CARTESIAN_POINT ( 'NONE',  ( -9.234937905884127218, -9.955011587777249815, 455.0000000000000568 ) ) ;
#39915 = LINE ( 'NONE', #62190, #39650 ) ;
#39916 = CARTESIAN_POINT ( 'NONE',  ( -7.450000000000001954, -7.249999999999998224, -8.500000000000000000 ) ) ;
#39917 = DIRECTION ( 'NONE',  ( -1.000000000000000000, 0.000000000000000000, 0.000000000000000000 ) ) ;
#39918 = DIRECTION ( 'NONE',  ( -1.000000000000000000, 0.000000000000000000, 0.000000000000000000 ) ) ;
#39919 = DIRECTION ( 'NONE',  ( 1.836970198721029934E-16, 1.836970198721010706E-16, -1.000000000000000000 ) ) ;
#39920 = VERTEX_POINT ( 'NONE', #65355 ) ;
#39921 = CARTESIAN_POINT ( 'NONE',  ( -3.667976262117325081, -9.912023737882812213, 26.00000000000000000 ) ) ;
#39922 = DIRECTION ( 'NONE',  ( -1.084202172485511060E-14, -1.000000000000000000, 0.000000000000000000 ) ) ;
#39923 = DIRECTION ( 'NONE',  ( 1.000000000000000000, 0.000000000000000000, 0.000000000000000000 ) ) ;
#39925 = ORIENTED_EDGE ( 'NONE', *, *, #52802, .T. ) ;
#39924 = DIRECTION ( 'NONE',  ( -0.7071067811865421326, 0.7071067811865530128, 0.000000000000000000 ) ) ;
#39926 = FACE_OUTER_BOUND ( 'NONE', #29744, .T. ) ;
#39927 = DIRECTION ( 'NONE',  ( 1.000000000000000000, -1.671920889371702854E-15, 0.000000000000000000 ) ) ;
#39928 = ORIENTED_EDGE ( 'NONE', *, *, #35355, .F. ) ;
#39929 = CARTESIAN_POINT ( 'NONE',  ( 29.50000000000000355, -15.46862696659690073, 14.50000000000000000 ) ) ;
#39930 = DIRECTION ( 'NONE',  ( 0.000000000000000000, -1.000000000000000000, 0.000000000000000000 ) ) ;
#39931 = EDGE_LOOP ( 'NONE', ( #19564, #6412, #44036, #59472 ) ) ;
#39932 = DIRECTION ( 'NONE',  ( 0.000000000000000000, -9.159339953149780582E-13, 1.000000000000000000 ) ) ;
#39933 = DIRECTION ( 'NONE',  ( 0.000000000000000000, 1.000000000000000000, 0.000000000000000000 ) ) ;
#39934 = PRESENTATION_STYLE_ASSIGNMENT (( #18374 ) ) ;
#39935 = CARTESIAN_POINT ( 'NONE',  ( 18.85410196625000268, -17.50000000000000000, 21.50000000000000000 ) ) ;
#39936 = CARTESIAN_POINT ( 'NONE',  ( 30.00000000000000000, -16.28999999999710369, -15.00000000000794920 ) ) ;
#39937 = AXIS2_PLACEMENT_3D ( 'NONE', #26849, #11593, #60043 ) ;
#39938 = VECTOR ( 'NONE', #60936, 1000.000000000000000 ) ;
#39939 = ORIENTED_EDGE ( 'NONE', *, *, #14919, .T. ) ;
#39940 = CARTESIAN_POINT ( 'NONE',  ( 15.50000000000000000, -5.000000000000000000, -22.50000000000000000 ) ) ;
#39941 = ORIENTED_EDGE ( 'NONE', *, *, #14715, .F. ) ;
#39942 = ORIENTED_EDGE ( 'NONE', *, *, #24158, .T. ) ;
#39943 = EDGE_CURVE ( 'NONE', #11295, #7880, #38482, .T. ) ;
#39944 = ADVANCED_FACE ( 'NONE', ( #33166 ), #27869, .F. ) ;
#39945 = DIRECTION ( 'NONE',  ( -1.000000000000000000, 0.000000000000000000, 0.000000000000000000 ) ) ;
#39946 = EDGE_CURVE ( 'NONE', #50762, #22220, #36124, .T. ) ;
#39947 = CIRCLE ( 'NONE', #16258, 1.000000000000000888 ) ;
#39948 = VECTOR ( 'NONE', #19061, 1000.000000000000000 ) ;
#39949 = ADVANCED_FACE ( 'NONE', ( #49444 ), #66385, .F. ) ;
#39950 = VECTOR ( 'NONE', #3858, 999.9999999999998863 ) ;
#39951 = LINE ( 'NONE', #24409, #7244 ) ;
#39952 = VECTOR ( 'NONE', #7790, 1000.000000000000000 ) ;
#39954 = DIRECTION ( 'NONE',  ( -1.000000000000000000, 0.000000000000000000, 0.000000000000000000 ) ) ;
#39953 = LINE ( 'NONE', #55884, #35149 ) ;
#39955 = VERTEX_POINT ( 'NONE', #5951 ) ;
#39956 = ORIENTED_EDGE ( 'NONE', *, *, #65925, .F. ) ;
#39957 = CARTESIAN_POINT ( 'NONE',  ( 15.00000000000000000, -26.42999999999999972, -5.874955318979029784 ) ) ;
#39958 = ORIENTED_EDGE ( 'NONE', *, *, #53136, .F. ) ;
#39959 = DIRECTION ( 'NONE',  ( -1.836970198721029934E-16, -1.836970198721010706E-16, 1.000000000000000000 ) ) ;
#39960 = PLANE ( 'NONE',  #1561 ) ;
#39961 = DIRECTION ( 'NONE',  ( 0.000000000000000000, 1.000000000000000000, 0.000000000000000000 ) ) ;
#39962 = AXIS2_PLACEMENT_3D ( 'NONE', #41814, #69387, #63747 ) ;
#39963 = CARTESIAN_POINT ( 'NONE',  ( 29.25000000000000000, -5.000000000000000000, 11.75000000000000000 ) ) ;
#39965 = LINE ( 'NONE', #14157, #17498 ) ;
#39964 = DIRECTION ( 'NONE',  ( 1.000000000000000000, -0.000000000000000000, -0.000000000000000000 ) ) ;
#39966 = VERTEX_POINT ( 'NONE', #60726 ) ;
#39968 = EDGE_LOOP ( 'NONE', ( #67459, #38170, #9667, #48207 ) ) ;
#39967 = LINE ( 'NONE', #61533, #22842 ) ;
#39969 = ORIENTED_EDGE ( 'NONE', *, *, #6246, .F. ) ;
#39970 = EDGE_LOOP ( 'NONE', ( #4017, #61808, #69206, #50684 ) ) ;
#39971 = CARTESIAN_POINT ( 'NONE',  ( 7.272650909786602114, 4.188533722949199678, 455.0000000000000568 ) ) ;
#39972 = CARTESIAN_POINT ( 'NONE',  ( -7.250000000000000888, 7.250000000000001776, -20.50000000000000000 ) ) ;
#39973 = ORIENTED_EDGE ( 'NONE', *, *, #32068, .F. ) ;
#39974 = VERTEX_POINT ( 'NONE', #5612 ) ;
#39975 = AXIS2_PLACEMENT_3D ( 'NONE', #57090, #8652, #9356 ) ;
#39976 = DIRECTION ( 'NONE',  ( 0.8660254037844485886, 0.000000000000000000, -0.4999999999999827360 ) ) ;
#39977 = CARTESIAN_POINT ( 'NONE',  ( -10.73351654964671020, 1.677516549646603794, 195.0000000000000284 ) ) ;
#39978 = VECTOR ( 'NONE', #38498, 1000.000000000000000 ) ;
#39979 = ORIENTED_EDGE ( 'NONE', *, *, #34480, .T. ) ;
#39980 = EDGE_LOOP ( 'NONE', ( #45032, #1175, #52182, #26632 ) ) ;
#39981 = FACE_OUTER_BOUND ( 'NONE', #54258, .T. ) ;
#39982 = CARTESIAN_POINT ( 'NONE',  ( 0.9555237378827827754, -9.929523737882782086, 26.00000000000000000 ) ) ;
#39983 = VERTEX_POINT ( 'NONE', #6971 ) ;
#39984 = ADVANCED_FACE ( 'NONE', ( #27519 ), #1007, .F. ) ;
#39985 = CIRCLE ( 'NONE', #68284, 25.39999999999999858 ) ;
#39986 = AXIS2_PLACEMENT_3D ( 'NONE', #67210, #17380, #66171 ) ;
#39987 = EDGE_CURVE ( 'NONE', #1391, #36828, #67763, .T. ) ;
#39988 = DIRECTION ( 'NONE',  ( 0.000000000000000000, 0.000000000000000000, -1.000000000000000000 ) ) ;
#39989 = CARTESIAN_POINT ( 'NONE',  ( -7.450000000000001954, -7.249999999999998224, -17.50000000000000000 ) ) ;
#39990 = ADVANCED_FACE ( 'NONE', ( #22562 ), #17932, .F. ) ;
#39992 = ORIENTED_EDGE ( 'NONE', *, *, #30924, .F. ) ;
#39991 = SURFACE_STYLE_USAGE ( .BOTH. , #34001 ) ;
#39993 = ORIENTED_EDGE ( 'NONE', *, *, #59025, .T. ) ;
#39994 = CARTESIAN_POINT ( 'NONE',  ( 0.000000000000000000, -2.500000000000000000, 45.00000000000000000 ) ) ;
#39995 = CARTESIAN_POINT ( 'NONE',  ( 6.832023737882815695, 9.722976262117192903, 54.00000000000000711 ) ) ;
#39996 = CIRCLE ( 'NONE', #69358, 0.7499999999999997780 ) ;
#39997 = EDGE_CURVE ( 'NONE', #48626, #62359, #44116, .T. ) ;
#39998 = LINE ( 'NONE', #61568, #35139 ) ;
#39999 = CARTESIAN_POINT ( 'NONE',  ( -7.250000000000001776, -7.249999999999998224, -22.50000000000000000 ) ) ;
#40000 = CARTESIAN_POINT ( 'NONE',  ( -7.250000000000000888, 8.250000000000001776, -22.00000000000000000 ) ) ;
#40001 = EDGE_CURVE ( 'NONE', #41898, #2156, #5660, .T. ) ;
#40002 = CARTESIAN_POINT ( 'NONE',  ( 39.00000000000000000, -21.00000000000000000, -16.96999999999999886 ) ) ;
#40003 = EDGE_CURVE ( 'NONE', #60826, #11772, #65514, .T. ) ;
#40004 = EDGE_CURVE ( 'NONE', #66058, #36929, #12615, .T. ) ;
#40005 = DIRECTION ( 'NONE',  ( 1.000000000000000000, -0.000000000000000000, 0.000000000000000000 ) ) ;
#40006 = EDGE_LOOP ( 'NONE', ( #59576, #47827, #69189, #42897 ) ) ;
#40007 = FACE_OUTER_BOUND ( 'NONE', #14989, .T. ) ;
#40008 = ADVANCED_FACE ( 'NONE', ( #65009 ), #17589, .F. ) ;
#40010 = ORIENTED_EDGE ( 'NONE', *, *, #47280, .F. ) ;
#40009 = DIRECTION ( 'NONE',  ( 1.000000000000000000, 0.000000000000000000, 0.000000000000000000 ) ) ;
#40011 = CARTESIAN_POINT ( 'NONE',  ( 0.5000000000000000000, -18.00000000000000355, -21.00000000000000000 ) ) ;
#40012 = CARTESIAN_POINT ( 'NONE',  ( 49.00000000000000000, -0.2000000000089119934, 8.909539772616881237E-12 ) ) ;
#40013 = FACE_OUTER_BOUND ( 'NONE', #12838, .T. ) ;
#40014 = CIRCLE ( 'NONE', #14090, 1.000000000000000000 ) ;
#40015 = CARTESIAN_POINT ( 'NONE',  ( 41.09999999999999432, 20.60000000000000142, 13.86939075806900057 ) ) ;
#40016 = DIRECTION ( 'NONE',  ( 0.000000000000000000, 0.000000000000000000, -1.000000000000000000 ) ) ;
#40017 = VERTEX_POINT ( 'NONE', #49772 ) ;
#40018 = VERTEX_POINT ( 'NONE', #1338 ) ;
#40019 = DIRECTION ( 'NONE',  ( 1.000000000000000000, 0.000000000000000000, 0.000000000000000000 ) ) ;
#40020 = SURFACE_STYLE_FILL_AREA ( #18460 ) ;
#40021 = CARTESIAN_POINT ( 'NONE',  ( 10.31452373788278187, 3.650476262117146042, 54.00000000000000711 ) ) ;
#40022 = VERTEX_POINT ( 'NONE', #22899 ) ;
#40023 = FACE_OUTER_BOUND ( 'NONE', #22573, .T. ) ;
#40024 = ORIENTED_EDGE ( 'NONE', *, *, #46172, .F. ) ;
#40025 = AXIS2_PLACEMENT_3D ( 'NONE', #15574, #9914, #10587 ) ;
#40026 = VERTEX_POINT ( 'NONE', #44452 ) ;
#40027 = CARTESIAN_POINT ( 'NONE',  ( 8.406483450353382736, 4.383466043307721272, 455.0000000000000568 ) ) ;
#40028 = CARTESIAN_POINT ( 'NONE',  ( -7.250000000000000888, 7.250000000000001776, -17.50000000000000000 ) ) ;
#40029 = VERTEX_POINT ( 'NONE', #40546 ) ;
#40030 = DIRECTION ( 'NONE',  ( -1.000000000000000000, 0.000000000000000000, 0.000000000000000000 ) ) ;
#40031 = VECTOR ( 'NONE', #26411, 1000.000000000000000 ) ;
#40032 = CARTESIAN_POINT ( 'NONE',  ( 7.450000000000004619, -1.336933437520057563E-15, -11.50000000000000000 ) ) ;
#40033 = CARTESIAN_POINT ( 'NONE',  ( -4.193516549646675529, 11.11351654964658664, 195.0000000000000284 ) ) ;
#40034 = VERTEX_POINT ( 'NONE', #23937 ) ;
#40035 = ORIENTED_EDGE ( 'NONE', *, *, #52848, .F. ) ;
#40037 = EDGE_LOOP ( 'NONE', ( #32482, #41632, #11707, #61759 ) ) ;
#40036 = CARTESIAN_POINT ( 'NONE',  ( -30.00000000000000000, -12.00000000000000000, -10.20500000000000007 ) ) ;
#40038 = ORIENTED_EDGE ( 'NONE', *, *, #45492, .T. ) ;
#40039 = AXIS2_PLACEMENT_3D ( 'NONE', #54495, #64409, #26570 ) ;
#40040 = AXIS2_PLACEMENT_3D ( 'NONE', #67832, #51922, #4193 ) ;
#40041 = FACE_OUTER_BOUND ( 'NONE', #53259, .T. ) ;
#40042 = DIRECTION ( 'NONE',  ( -1.000000000000000000, 0.000000000000000000, 0.000000000000000000 ) ) ;
#40043 = CYLINDRICAL_SURFACE ( 'NONE', #58350, 0.1749999999999989342 ) ;
#40044 = DIRECTION ( 'NONE',  ( -1.000000000000000000, 0.000000000000000000, 0.000000000000000000 ) ) ;
#40045 = CARTESIAN_POINT ( 'NONE',  ( 106.4257688009193998, 0.000000000000000000, 289.4830310981789125 ) ) ;
#40046 = PRESENTATION_LAYER_ASSIGNMENT (  '', '', ( #64915 ) ) ;
#40047 = EDGE_CURVE ( 'NONE', #40687, #67636, #8012, .T. ) ;
#40048 = LINE ( 'NONE', #61623, #28674 ) ;
#40049 = ORIENTED_EDGE ( 'NONE', *, *, #59543, .T. ) ;
#40050 = VERTEX_POINT ( 'NONE', #14394 ) ;
#40051 = EDGE_LOOP ( 'NONE', ( #17393, #2038, #65670, #602 ) ) ;
#40053 = ORIENTED_EDGE ( 'NONE', *, *, #46259, .F. ) ;
#40052 = AXIS2_PLACEMENT_3D ( 'NONE', #28761, #18152, #2245 ) ;
#40054 = EDGE_CURVE ( 'NONE', #33046, #51738, #56463, .T. ) ;
#40055 = CARTESIAN_POINT ( 'NONE',  ( -9.690000000000001279, -9.750000000000001776, -5.000000000000000000 ) ) ;
#40056 = CARTESIAN_POINT ( 'NONE',  ( -11.77351654964674132, -4.186483450353323477, 455.0000000000000568 ) ) ;
#40057 = CARTESIAN_POINT ( 'NONE',  ( 7.250000000000005329, -7.249999999999998224, -8.000000000000000000 ) ) ;
#40058 =( NAMED_UNIT ( * ) PLANE_ANGLE_UNIT ( ) SI_UNIT ( $, .RADIAN. ) );
#40059 = CARTESIAN_POINT ( 'NONE',  ( 25.50000000000000355, -5.578999999999999737, -20.87900000000000134 ) ) ;
#40060 = ORIENTED_EDGE ( 'NONE', *, *, #24408, .F. ) ;
#40062 = ADVANCED_FACE ( 'NONE', ( #7314 ), #18626, .T. ) ;
#40061 = ORIENTED_EDGE ( 'NONE', *, *, #50132, .T. ) ;
#40063 = ORIENTED_EDGE ( 'NONE', *, *, #6976, .T. ) ;
#40064 = VECTOR ( 'NONE', #24639, 1000.000000000000000 ) ;
#40065 = DIRECTION ( 'NONE',  ( -1.836970198721029934E-16, 1.836970198721036590E-16, -1.000000000000000000 ) ) ;
#40066 = ORIENTED_EDGE ( 'NONE', *, *, #21383, .T. ) ;
#40067 = VERTEX_POINT ( 'NONE', #29229 ) ;
#40068 = ADVANCED_FACE ( 'NONE', ( #29940, #7669 ), #8363, .F. ) ;
#40069 = ORIENTED_EDGE ( 'NONE', *, *, #52223, .F. ) ;
#40070 = ORIENTED_EDGE ( 'NONE', *, *, #12415, .F. ) ;
#40071 = LINE ( 'NONE', #25232, #14688 ) ;
#40073 = ORIENTED_EDGE ( 'NONE', *, *, #1758, .T. ) ;
#40072 = DIRECTION ( 'NONE',  ( -0.4285714285711678118, 0.000000000000000000, -0.9035079029053749711 ) ) ;
#40074 = VERTEX_POINT ( 'NONE', #68125 ) ;
#40075 = DIRECTION ( 'NONE',  ( -8.673617379884013384E-15, -1.000000000000000000, 0.000000000000000000 ) ) ;
#40076 = LINE ( 'NONE', #8617, #36355 ) ;
#40077 = ADVANCED_FACE ( 'NONE', ( #45496 ), #50803, .T. ) ;
#40078 = DIRECTION ( 'NONE',  ( 0.000000000000000000, -0.7046037717806115097, 0.7096009616626348659 ) ) ;
#40080 = ORIENTED_EDGE ( 'NONE', *, *, #43762, .F. ) ;
#40079 = DIRECTION ( 'NONE',  ( 0.000000000000000000, 0.000000000000000000, 1.000000000000000000 ) ) ;
#40081 = ORIENTED_EDGE ( 'NONE', *, *, #7013, .T. ) ;
#40082 = AXIS2_PLACEMENT_3D ( 'NONE', #36950, #16765, #59886 ) ;
#40083 = CARTESIAN_POINT ( 'NONE',  ( 6.006483450353353959, 5.993516549646629166, 195.0000000000000284 ) ) ;
#40084 = DIRECTION ( 'NONE',  ( -1.000000000000000000, 0.000000000000000000, 0.000000000000000000 ) ) ;
#40085 = DIRECTION ( 'NONE',  ( -0.000000000000000000, -0.000000000000000000, -1.000000000000000000 ) ) ;
#40086 = AXIS2_PLACEMENT_3D ( 'NONE', #32838, #59711, #42057 ) ;
#40087 = EDGE_CURVE ( 'NONE', #5599, #50768, #39835, .T. ) ;
#40088 = ORIENTED_EDGE ( 'NONE', *, *, #24205, .T. ) ;
#40089 = CYLINDRICAL_SURFACE ( 'NONE', #33698, 1.000000000000000000 ) ;
#40090 = EDGE_CURVE ( 'NONE', #33817, #14966, #40663, .T. ) ;
#40091 = VECTOR ( 'NONE', #62423, 1000.000000000000114 ) ;
#40092 = VECTOR ( 'NONE', #49085, 1000.000000000000000 ) ;
#40094 = DIRECTION ( 'NONE',  ( -1.000000000000000000, 1.221996412923863950E-14, 1.836970198721052367E-16 ) ) ;
#40093 = AXIS2_PLACEMENT_3D ( 'NONE', #33815, #976, #19220 ) ;
#40095 = DIRECTION ( 'NONE',  ( -0.000000000000000000, 1.000000000000000000, -0.000000000000000000 ) ) ;
#40096 = AXIS2_PLACEMENT_3D ( 'NONE', #41026, #62590, #25127 ) ;
#40097 = ORIENTED_EDGE ( 'NONE', *, *, #67843, .T. ) ;
#40098 = DIRECTION ( 'NONE',  ( 0.000000000000000000, 0.000000000000000000, -1.000000000000000000 ) ) ;
#40099 = VECTOR ( 'NONE', #41292, 1000.000000000000114 ) ;
#40100 = AXIS2_PLACEMENT_3D ( 'NONE', #45014, #11457, #60591 ) ;
#40101 = PLANE ( 'NONE',  #48902 ) ;
#40102 = CARTESIAN_POINT ( 'NONE',  ( -9.689726262117314803, -8.580623737882756785, 54.00000000000000711 ) ) ;
#40103 = EDGE_CURVE ( 'NONE', #47005, #35485, #24994, .T. ) ;
#40104 = EDGE_LOOP ( 'NONE', ( #63979, #53582, #31745, #28574, #68624, #10171, #27392, #26874, #1379, #49119, #27579, #43102, #69126, #64410, #55713, #54434, #8246, #58725, #10337, #52494, #68463, #54837, #32033, #9855, #58952, #48580, #9440, #9173, #9918, #18244 ) ) ;
#40105 = VECTOR ( 'NONE', #25218, 1000.000000000000000 ) ;
#40106 = PRESENTATION_STYLE_ASSIGNMENT (( #7591 ) ) ;
#40107 = PRESENTATION_STYLE_ASSIGNMENT (( #33437 ) ) ;
#40108 = DIRECTION ( 'NONE',  ( 0.000000000000000000, 1.000000000000000000, 0.000000000000000000 ) ) ;
#40109 = AXIS2_PLACEMENT_3D ( 'NONE', #46817, #68401, #10740 ) ;
#40110 = ORIENTED_EDGE ( 'NONE', *, *, #21042, .T. ) ;
#40111 = DIRECTION ( 'NONE',  ( 1.000000000000000000, 0.000000000000000000, 0.000000000000000000 ) ) ;
#40112 = CARTESIAN_POINT ( 'NONE',  ( 0.5000000000000000000, -21.00000000000000000, -18.00000000000000355 ) ) ;
#40113 = DIRECTION ( 'NONE',  ( -0.000000000000000000, -0.000000000000000000, -1.000000000000000000 ) ) ;
#40114 = AXIS2_PLACEMENT_3D ( 'NONE', #51699, #57340, #3602 ) ;
#40115 = CARTESIAN_POINT ( 'NONE',  ( 7.250000000000005329, 7.250000000000000888, -18.50000000000000000 ) ) ;
#40116 = DIRECTION ( 'NONE',  ( 1.836970198721029934E-16, 1.836970198721010706E-16, -1.000000000000000000 ) ) ;
#40117 = ORIENTED_EDGE ( 'NONE', *, *, #64224, .T. ) ;
#40118 = DIRECTION ( 'NONE',  ( 1.000000000000000000, -0.000000000000000000, 0.000000000000000000 ) ) ;
#40119 = CARTESIAN_POINT ( 'NONE',  ( 0.2500000000000000000, -0.2499999999999970302, 26.75000000000000000 ) ) ;
#40120 = CARTESIAN_POINT ( 'NONE',  ( 10.00000000000000000, -18.00000000000000355, 21.00000000000000000 ) ) ;
#40121 = ADVANCED_FACE ( 'NONE', ( #3086 ), #18274, .T. ) ;
#40122 = DIRECTION ( 'NONE',  ( 0.000000000000000000, 0.6666666666652433237, -0.7453559925012029908 ) ) ;
#40123 = DIRECTION ( 'NONE',  ( 0.000000000000000000, 0.7071067811865475727, -0.7071067811865475727 ) ) ;
#40124 = VERTEX_POINT ( 'NONE', #18986 ) ;
#40126 = ORIENTED_EDGE ( 'NONE', *, *, #14393, .F. ) ;
#40125 = LINE ( 'NONE', #30245, #22802 ) ;
#40127 = ADVANCED_FACE ( 'NONE', ( #61401 ), #2375, .F. ) ;
#40128 = DIRECTION ( 'NONE',  ( 0.8660254037844358210, -0.5000000000000049960, 0.000000000000000000 ) ) ;
#40129 = CARTESIAN_POINT ( 'NONE',  ( 283.0000000000000568, -32.00000000000000000, -8.400000000000000355 ) ) ;
#40130 = ORIENTED_EDGE ( 'NONE', *, *, #16132, .F. ) ;
#40131 = AXIS2_PLACEMENT_3D ( 'NONE', #27854, #60712, #34168 ) ;
#40132 = EDGE_CURVE ( 'NONE', #46985, #38472, #15843, .T. ) ;
#40133 = PLANE ( 'NONE',  #34087 ) ;
#40134 = EDGE_CURVE ( 'NONE', #8330, #47821, #34534, .T. ) ;
#40135 = AXIS2_PLACEMENT_3D ( 'NONE', #34563, #17956, #13702 ) ;
#40136 = EDGE_LOOP ( 'NONE', ( #67795, #68916, #42352, #30345 ) ) ;
#40137 = AXIS2_PLACEMENT_3D ( 'NONE', #1603, #49023, #23175 ) ;
#40138 = CARTESIAN_POINT ( 'NONE',  ( 2.765062094116107705, 9.942044687070449527, 455.0000000000000568 ) ) ;
#40139 = ORIENTED_EDGE ( 'NONE', *, *, #28891, .F. ) ;
#40140 = EDGE_CURVE ( 'NONE', #64382, #40458, #64357, .T. ) ;
#40141 = EDGE_LOOP ( 'NONE', ( #40060, #50600, #1726, #40435, #62710 ) ) ;
#40142 = CARTESIAN_POINT ( 'NONE',  ( -7.252248008019455128, 6.606374702650072983, 455.0000000000000568 ) ) ;
#40143 = DIRECTION ( 'NONE',  ( 1.671920889371702657E-15, 1.000000000000000000, -0.000000000000000000 ) ) ;
#40144 = DIRECTION ( 'NONE',  ( -1.000000000000000000, 0.000000000000000000, 0.000000000000000000 ) ) ;
#40145 = FACE_OUTER_BOUND ( 'NONE', #5651, .T. ) ;
#40146 = VECTOR ( 'NONE', #4719, 1000.000000000000000 ) ;
#40147 = VECTOR ( 'NONE', #17744, 1000.000000000000000 ) ;
#40148 = ORIENTED_EDGE ( 'NONE', *, *, #15280, .F. ) ;
#40149 = ADVANCED_FACE ( 'NONE', ( #46198 ), #67772, .F. ) ;
#40150 = EDGE_LOOP ( 'NONE', ( #8494, #64712, #12506, #17961 ) ) ;
#40151 = CARTESIAN_POINT ( 'NONE',  ( -13.00000000000000178, -15.50000000000000000, 14.50000000000000000 ) ) ;
#40152 = ADVANCED_FACE ( 'NONE', ( #35584 ), #57167, .T. ) ;
#40153 = PLANE ( 'NONE',  #48578 ) ;
#40154 = VECTOR ( 'NONE', #46455, 1000.000000000000000 ) ;
#40155 = CIRCLE ( 'NONE', #39060, 24.99999999998794920 ) ;
#40156 = CIRCLE ( 'NONE', #23252, 1.620999999999997332 ) ;
#40157 = ORIENTED_EDGE ( 'NONE', *, *, #67241, .T. ) ;
#40158 = EDGE_LOOP ( 'NONE', ( #7976, #57977, #51888, #40837, #34043, #60964 ) ) ;
#40159 = ADVANCED_FACE ( 'NONE', ( #64236 ), #41606, .F. ) ;
#40160 = EDGE_CURVE ( 'NONE', #60266, #21334, #5, .T. ) ;
#40161 = ORIENTED_EDGE ( 'NONE', *, *, #53027, .F. ) ;
#40162 = AXIS2_PLACEMENT_3D ( 'NONE', #27837, #624, #49418 ) ;
#40163 = LINE ( 'NONE', #28511, #33869 ) ;
#40165 = VERTEX_POINT ( 'NONE', #47266 ) ;
#40164 = FACE_OUTER_BOUND ( 'NONE', #46169, .T. ) ;
#40166 = EDGE_CURVE ( 'NONE', #57686, #39654, #35047, .T. ) ;
#40167 = DIRECTION ( 'NONE',  ( 0.000000000000000000, 1.000000000000000000, 0.000000000000000000 ) ) ;
#40168 = PRODUCT ( 'LEAD SCREW', 'LEAD SCREW', '', ( #61830 ) ) ;
#40169 = CARTESIAN_POINT ( 'NONE',  ( 11.00000000000000000, -14.04000000000000092, -14.80000000000000071 ) ) ;
#40170 = EDGE_LOOP ( 'NONE', ( #64470, #9470, #43297, #19829 ) ) ;
#40171 = AXIS2_PLACEMENT_3D ( 'NONE', #51958, #19422, #46641 ) ;
#40172 = ORIENTED_EDGE ( 'NONE', *, *, #59032, .F. ) ;
#40173 = DIRECTION ( 'NONE',  ( 0.000000000000000000, 0.000000000000000000, -1.000000000000000000 ) ) ;
#40174 = LINE ( 'NONE', #46183, #8681 ) ;
#40175 = EDGE_CURVE ( 'NONE', #35648, #5476, #68833, .T. ) ;
#40176 = DIRECTION ( 'NONE',  ( -0.7671651518153105309, -0.6414496315691445849, 0.000000000000000000 ) ) ;
#40177 = EDGE_CURVE ( 'NONE', #45394, #22980, #57511, .T. ) ;
#40178 = LINE ( 'NONE', #19317, #47078 ) ;
#40179 = DIRECTION ( 'NONE',  ( 0.000000000000000000, 0.000000000000000000, 1.000000000000000000 ) ) ;
#40180 = AXIS2_PLACEMENT_3D ( 'NONE', #56724, #13236, #40813 ) ;
#40182 = ORIENTED_EDGE ( 'NONE', *, *, #37314, .T. ) ;
#40181 = DIRECTION ( 'NONE',  ( -1.794541526872559352E-16, -1.000000000000000000, 0.000000000000000000 ) ) ;
#40183 = ORIENTED_EDGE ( 'NONE', *, *, #3386, .T. ) ;
#40184 = CARTESIAN_POINT ( 'NONE',  ( 10.09643294401453062, 2.693516549646537417, 455.0000000000000568 ) ) ;
#40185 = DIRECTION ( 'NONE',  ( 1.000000000000000000, 0.000000000000000000, 0.000000000000000000 ) ) ;
#40186 = DIRECTION ( 'NONE',  ( 0.000000000000000000, 0.000000000000000000, 1.000000000000000000 ) ) ;
#40187 = VECTOR ( 'NONE', #48681, 1000.000000000000000 ) ;
#40188 = CARTESIAN_POINT ( 'NONE',  ( 7.250000000000005329, 7.250000000000000888, -13.50000000000000178 ) ) ;
#40189 = AXIS2_PLACEMENT_3D ( 'NONE', #67003, #61694, #40834 ) ;
#40190 = LINE ( 'NONE', #44449, #44398 ) ;
#40191 = ORIENTED_EDGE ( 'NONE', *, *, #60026, .T. ) ;
#40192 = CARTESIAN_POINT ( 'NONE',  ( 4.406483450353420928, 11.31351654964658593, 455.0000000000000568 ) ) ;
#40193 = DIRECTION ( 'NONE',  ( 0.000000000000000000, -0.9921567416492215186, 0.1249999999999996531 ) ) ;
#40194 = DIRECTION ( 'NONE',  ( -1.000000000000000000, 0.000000000000000000, 0.000000000000000000 ) ) ;
#40195 = DIRECTION ( 'NONE',  ( 0.000000000000000000, -0.000000000000000000, -1.000000000000000000 ) ) ;
#40196 = VECTOR ( 'NONE', #36305, 1000.000000000000114 ) ;
#40197 = VECTOR ( 'NONE', #32231, 1000.000000000000000 ) ;
#40198 = VECTOR ( 'NONE', #61119, 1000.000000000000000 ) ;
#40199 = EDGE_CURVE ( 'NONE', #41571, #66056, #25348, .T. ) ;
#40200 = CARTESIAN_POINT ( 'NONE',  ( 37.90000000000000568, 0.000000000000000000, 3.232403992503367940E-15 ) ) ;
#40201 = DIRECTION ( 'NONE',  ( -0.6414496315691494699, 0.7671651518153064231, 2.818519042764025305E-16 ) ) ;
#40202 = VECTOR ( 'NONE', #37575, 1000.000000000000000 ) ;
#40203 = AXIS2_PLACEMENT_3D ( 'NONE', #36340, #63214, #69220 ) ;
#40204 = CARTESIAN_POINT ( 'NONE',  ( -8.821682069070780230, 2.355476262117184305, 54.00000000000000711 ) ) ;
#40205 = EDGE_LOOP ( 'NONE', ( #1626, #15678, #41264, #36615 ) ) ;
#40206 = DIRECTION ( 'NONE',  ( 0.000000000000000000, 1.000000000000000000, 0.000000000000000000 ) ) ;
#40207 = LINE ( 'NONE', #56474, #18036 ) ;
#40208 = ORIENTED_EDGE ( 'NONE', *, *, #19864, .T. ) ;
#40209 = CARTESIAN_POINT ( 'NONE',  ( 7.450000000000006395, 7.250000000000000888, -15.50000000000000000 ) ) ;
#40210 = CARTESIAN_POINT ( 'NONE',  ( 276.8775010008008053, -53.81370849898476649, 17.50000000000000000 ) ) ;
#40211 = VECTOR ( 'NONE', #35477, 1000.000000000000000 ) ;
#40212 = FACE_OUTER_BOUND ( 'NONE', #20932, .T. ) ;
#40213 = CARTESIAN_POINT ( 'NONE',  ( 7.357023737882817827, -5.552858015815587578, 54.00000000000000711 ) ) ;
#40214 = CARTESIAN_POINT ( 'NONE',  ( 32.89999999999999858, -21.00000000000000000, 13.86939075806900057 ) ) ;
#40215 = EDGE_LOOP ( 'NONE', ( #39071, #69801, #55549, #2974 ) ) ;
#40216 = EDGE_CURVE ( 'NONE', #31017, #61884, #54265, .T. ) ;
#40217 = CYLINDRICAL_SURFACE ( 'NONE', #14949, 0.5000000000009441337 ) ;
#40218 = CIRCLE ( 'NONE', #4117, 0.1999999999999987899 ) ;
#40219 = VERTEX_POINT ( 'NONE', #9080 ) ;
#40220 = PLANE ( 'NONE',  #6288 ) ;
#40221 = ORIENTED_EDGE ( 'NONE', *, *, #14564, .F. ) ;
#40222 = EDGE_CURVE ( 'NONE', #66435, #54499, #25712, .T. ) ;
#40223 = LINE ( 'NONE', #6998, #59654 ) ;
#40224 = EDGE_CURVE ( 'NONE', #44628, #35366, #30998, .T. ) ;
#40225 = ORIENTED_EDGE ( 'NONE', *, *, #14975, .T. ) ;
#40226 = DIRECTION ( 'NONE',  ( 0.000000000000000000, 3.673940397442059868E-16, -1.000000000000000000 ) ) ;
#40227 = PLANE ( 'NONE',  #13048 ) ;
#40228 = VERTEX_POINT ( 'NONE', #26745 ) ;
#40229 = EDGE_CURVE ( 'NONE', #9548, #41002, #69869, .T. ) ;
#40230 = ORIENTED_EDGE ( 'NONE', *, *, #37064, .F. ) ;
#40231 = DIRECTION ( 'NONE',  ( -1.000000000000000000, -0.000000000000000000, -0.000000000000000000 ) ) ;
#40232 = VERTEX_POINT ( 'NONE', #52577 ) ;
#40233 = ORIENTED_EDGE ( 'NONE', *, *, #6803, .T. ) ;
#40234 = PRODUCT_DEFINITION_CONTEXT ( 'detailed design', #38180, 'design' ) ;
#40235 = CARTESIAN_POINT ( 'NONE',  ( 9.841277389592693936, 1.677516549646539623, 455.0000000000000568 ) ) ;
#40236 = DIRECTION ( 'NONE',  ( 1.000000000000000000, 0.000000000000000000, 0.000000000000000000 ) ) ;
#40237 = CYLINDRICAL_SURFACE ( 'NONE', #42295, 1.929199999999997139 ) ;
#40238 = CONICAL_SURFACE ( 'NONE', #9779, 7.799999999999999822, 1.047197551196693555 ) ;
#40239 = ORIENTED_EDGE ( 'NONE', *, *, #61790, .F. ) ;
#40240 = CARTESIAN_POINT ( 'NONE',  ( 38.90000000000000568, -0.1999999999911795112, 8.826273045769999343E-12 ) ) ;
#40242 = CARTESIAN_POINT ( 'NONE',  ( -7.798499376344067535, 4.727349090213367688, 455.0000000000000568 ) ) ;
#40241 = CARTESIAN_POINT ( 'NONE',  ( 7.000000000000000000, -40.30000000000000426, -8.900000000000000355 ) ) ;
#40243 = ORIENTED_EDGE ( 'NONE', *, *, #37886, .T. ) ;
#40245 = ORIENTED_EDGE ( 'NONE', *, *, #12925, .F. ) ;
#40244 = LINE ( 'NONE', #28591, #30877 ) ;
#40246 = VECTOR ( 'NONE', #69470, 1000.000000000000000 ) ;
#40247 = VERTEX_POINT ( 'NONE', #48314 ) ;
#40248 = ADVANCED_FACE ( 'NONE', ( #63535 ), #64575, .T. ) ;
#40249 = SHAPE_DEFINITION_REPRESENTATION ( #61615, #33595 ) ;
#40250 = AXIS2_PLACEMENT_3D ( 'NONE', #17673, #39235, #12340 ) ;
#40251 = VECTOR ( 'NONE', #61209, 1000.000000000000000 ) ;
#40252 = CARTESIAN_POINT ( 'NONE',  ( 39.00000000000000000, 21.00000000000000000, -16.96999999999999886 ) ) ;
#40253 = VERTEX_POINT ( 'NONE', #36650 ) ;
#40254 = VECTOR ( 'NONE', #21792, 1000.000000000000000 ) ;
#40255 = VECTOR ( 'NONE', #45871, 1000.000000000000000 ) ;
#40256 = AXIS2_PLACEMENT_3D ( 'NONE', #66777, #17656, #44171 ) ;
#40257 = LINE ( 'NONE', #14453, #47249 ) ;
#40258 = CARTESIAN_POINT ( 'NONE',  ( 7.250000000000005329, 7.250000000000000888, -26.00000000000001066 ) ) ;
#40259 = ORIENTED_EDGE ( 'NONE', *, *, #2247, .F. ) ;
#40260 = ORIENTED_EDGE ( 'NONE', *, *, #12936, .T. ) ;
#40261 = CIRCLE ( 'NONE', #62888, 0.5000000000001386669 ) ;
#40262 = CIRCLE ( 'NONE', #10904, 1.000000000000003553 ) ;
#40263 = CARTESIAN_POINT ( 'NONE',  ( -8.598420958951630055, -1.480523737882741164, 26.00000000000000711 ) ) ;
#40264 = LINE ( 'NONE', #28607, #45859 ) ;
#40265 = ORIENTED_EDGE ( 'NONE', *, *, #4432, .T. ) ;
#40266 = PLANE ( 'NONE',  #13244 ) ;
#40268 = AXIS2_PLACEMENT_3D ( 'NONE', #40267, #40617, #62522 ) ;
#40267 = CARTESIAN_POINT ( 'NONE',  ( -9.547976262117227719, -2.544523737882729453, 54.00000000000000711 ) ) ;
#40269 = DIRECTION ( 'NONE',  ( -0.000000000000000000, -0.000000000000000000, -1.000000000000000000 ) ) ;
#40270 = ADVANCED_FACE ( 'NONE', ( #58219 ), #53285, .T. ) ;
#40271 = ORIENTED_EDGE ( 'NONE', *, *, #58286, .F. ) ;
#40272 = EDGE_CURVE ( 'NONE', #32725, #34472, #50844, .T. ) ;
#40273 = VECTOR ( 'NONE', #3596, 1000.000000000000000 ) ;
#40274 = CARTESIAN_POINT ( 'NONE',  ( 36.90000000000000568, 3.010794155703768650E-16, -2.458500000000000796 ) ) ;
#40275 = CARTESIAN_POINT ( 'NONE',  ( 275.5000000000000000, -42.00000000000000000, -27.00000000000000000 ) ) ;
#40278 = ORIENTED_EDGE ( 'NONE', *, *, #41956, .F. ) ;
#40277 = EDGE_CURVE ( 'NONE', #45115, #66583, #15442, .T. ) ;
#40276 = CARTESIAN_POINT ( 'NONE',  ( -7.250000000000001776, -7.249999999999998224, -14.50000000000000000 ) ) ;
#40280 = ORIENTED_EDGE ( 'NONE', *, *, #24048, .F. ) ;
#40279 = FACE_OUTER_BOUND ( 'NONE', #48854, .T. ) ;
#40281 = DIRECTION ( 'NONE',  ( -0.000000000000000000, -0.000000000000000000, 1.000000000000000000 ) ) ;
#40282 = DIRECTION ( 'NONE',  ( 0.7071067811865486830, 0.7071067811865464625, 0.000000000000000000 ) ) ;
#40283 = CARTESIAN_POINT ( 'NONE',  ( 7.450000000000003730, -7.249999999999997335, -10.00000000000000000 ) ) ;
#40284 = LINE ( 'NONE', #61856, #55379 ) ;
#40285 = CARTESIAN_POINT ( 'NONE',  ( -11.99351654964678282, -11.19368345035330314, 195.0000000000000284 ) ) ;
#40286 = ORIENTED_EDGE ( 'NONE', *, *, #64014, .T. ) ;
#40287 = LINE ( 'NONE', #39245, #5306 ) ;
#40288 = CARTESIAN_POINT ( 'NONE',  ( -25.50000000000000355, -15.12100000000000044, 24.12099999999999511 ) ) ;
#40289 = CARTESIAN_POINT ( 'NONE',  ( 7.250000000000005329, 8.250000000000001776, -12.00000000000000000 ) ) ;
#40291 = ORIENTED_EDGE ( 'NONE', *, *, #19215, .T. ) ;
#40290 = LINE ( 'NONE', #8102, #46920 ) ;
#40292 = FACE_OUTER_BOUND ( 'NONE', #21124, .T. ) ;
#40293 = AXIS2_PLACEMENT_3D ( 'NONE', #15268, #42481, #35772 ) ;
#40294 = CARTESIAN_POINT ( 'NONE',  ( 8.930623737882818602, -8.580623737882856261, 54.00000000000000711 ) ) ;
#40295 = ORIENTED_EDGE ( 'NONE', *, *, #20225, .T. ) ;
#40296 = AXIS2_PLACEMENT_3D ( 'NONE', #45839, #50790, #28869 ) ;
#40297 = ORIENTED_EDGE ( 'NONE', *, *, #58060, .F. ) ;
#40298 = LINE ( 'NONE', #61873, #20788 ) ;
#40299 = DIRECTION ( 'NONE',  ( 1.000000000000000000, 0.000000000000000000, 0.000000000000000000 ) ) ;
#40300 = ORIENTED_EDGE ( 'NONE', *, *, #8083, .T. ) ;
#40301 = DIRECTION ( 'NONE',  ( 0.000000000000000000, -5.800915303574361727E-12, 1.000000000000000000 ) ) ;
#40302 = AXIS2_PLACEMENT_3D ( 'NONE', #60029, #48043, #43081 ) ;
#40303 = VECTOR ( 'NONE', #6280, 1000.000000000000000 ) ;
#40304 = CARTESIAN_POINT ( 'NONE',  ( -7.250000000000000000, -7.449999999999998401, -18.00000000000000000 ) ) ;
#40305 = FACE_OUTER_BOUND ( 'NONE', #36335, .T. ) ;
#40306 = EDGE_CURVE ( 'NONE', #48443, #18655, #52210, .T. ) ;
#40308 = CARTESIAN_POINT ( 'NONE',  ( -11.25000000000000000, 11.18999999999999950, -5.000000000000000000 ) ) ;
#40307 = CIRCLE ( 'NONE', #4198, 1.224999999999999423 ) ;
#40309 = VERTEX_POINT ( 'NONE', #47961 ) ;
#40310 = AXIS2_PLACEMENT_3D ( 'NONE', #25221, #14265, #8944 ) ;
#40311 = DIRECTION ( 'NONE',  ( 1.000000000000000000, -0.000000000000000000, -0.000000000000000000 ) ) ;
#40312 = ORIENTED_EDGE ( 'NONE', *, *, #42659, .T. ) ;
#40313 = VERTEX_POINT ( 'NONE', #21089 ) ;
#40314 = CARTESIAN_POINT ( 'NONE',  ( -11.77351654964670935, 7.813516549646603693, 195.0000000000000284 ) ) ;
#40315 = VECTOR ( 'NONE', #52127, 1000.000000000000000 ) ;
#40316 = CIRCLE ( 'NONE', #12102, 4.500000000000191847 ) ;
#40317 = EDGE_CURVE ( 'NONE', #2273, #65266, #15782, .T. ) ;
#40318 = ADVANCED_FACE ( 'NONE', ( #33771 ), #44030, .F. ) ;
#40319 = ADVANCED_FACE ( 'NONE', ( #60289 ), #5874, .F. ) ;
#40320 = AXIS2_PLACEMENT_3D ( 'NONE', #61039, #66705, #33492 ) ;
#40322 = CARTESIAN_POINT ( 'NONE',  ( -11.75000000000000000, -5.000000000000000000, 11.75000000000000000 ) ) ;
#40321 = CARTESIAN_POINT ( 'NONE',  ( 46.39999999999999858, 21.00000000000000000, -2.250000000000000444 ) ) ;
#40323 = VERTEX_POINT ( 'NONE', #22136 ) ;
#40324 = EDGE_CURVE ( 'NONE', #1387, #15802, #50029, .T. ) ;
#40325 = ORIENTED_EDGE ( 'NONE', *, *, #43462, .T. ) ;
#40326 = EDGE_CURVE ( 'NONE', #57897, #5949, #22819, .T. ) ;
#40327 = LINE ( 'NONE', #1448, #13765 ) ;
#40328 = ORIENTED_EDGE ( 'NONE', *, *, #51941, .T. ) ;
#40329 = AXIS2_PLACEMENT_3D ( 'NONE', #54484, #43857, #39240 ) ;
#40330 = CARTESIAN_POINT ( 'NONE',  ( 30.00000000000000000, -12.00000000000000000, -12.20000000000000107 ) ) ;
#40331 = CARTESIAN_POINT ( 'NONE',  ( -10.30047626211725031, -3.857023737882713466, 54.00000000000000711 ) ) ;
#40332 = DIRECTION ( 'NONE',  ( 0.000000000000000000, 0.000000000000000000, 1.000000000000000000 ) ) ;
#40333 = EDGE_CURVE ( 'NONE', #60944, #19926, #53974, .T. ) ;
#40334 = DIRECTION ( 'NONE',  ( -1.000000000000000000, 1.794541526872559352E-16, 0.000000000000000000 ) ) ;
#40335 = ORIENTED_EDGE ( 'NONE', *, *, #10345, .T. ) ;
#40336 = DIRECTION ( 'NONE',  ( -1.000000000000000000, -3.016910393003147986E-15, -0.000000000000000000 ) ) ;
#40338 = CARTESIAN_POINT ( 'NONE',  ( 39.90000000000000568, 16.96999999999999886, 21.00000000000000000 ) ) ;
#40337 = CARTESIAN_POINT ( 'NONE',  ( 2.706483450353419862, 10.91351654964658735, 455.0000000000000568 ) ) ;
#40339 = VERTEX_POINT ( 'NONE', #16828 ) ;
#40341 = VERTEX_POINT ( 'NONE', #934 ) ;
#40340 = DIRECTION ( 'NONE',  ( 0.000000000000000000, 0.000000000000000000, 1.000000000000000000 ) ) ;
#40342 = ORIENTED_EDGE ( 'NONE', *, *, #61163, .T. ) ;
#40343 = ORIENTED_EDGE ( 'NONE', *, *, #12218, .T. ) ;
#40344 = CARTESIAN_POINT ( 'NONE',  ( -11.00000000000000000, -5.200000000000001066, 26.59999999999999787 ) ) ;
#40345 = DIRECTION ( 'NONE',  ( 0.000000000000000000, -1.000000000000000000, 0.000000000000000000 ) ) ;
#40346 = ORIENTED_EDGE ( 'NONE', *, *, #2230, .F. ) ;
#40347 = ORIENTED_EDGE ( 'NONE', *, *, #43585, .T. ) ;
#40348 = DIRECTION ( 'NONE',  ( 0.000000000000000000, 0.000000000000000000, 1.000000000000000000 ) ) ;
#40349 = CARTESIAN_POINT ( 'NONE',  ( -11.99351654964674374, -4.186483450353318148, 455.0000000000000568 ) ) ;
#40350 = ORIENTED_EDGE ( 'NONE', *, *, #32508, .F. ) ;
#40351 = ORIENTED_EDGE ( 'NONE', *, *, #33427, .T. ) ;
#40352 = VECTOR ( 'NONE', #2904, 1000.000000000000000 ) ;
#40354 = CARTESIAN_POINT ( 'NONE',  ( -7.450000000000001954, 7.250000000000000000, -8.500000000000000000 ) ) ;
#40353 = VECTOR ( 'NONE', #58912, 1000.000000000000000 ) ;
#40355 = DIRECTION ( 'NONE',  ( 0.000000000000000000, 1.000000000000000000, 0.000000000000000000 ) ) ;
#40356 = ORIENTED_EDGE ( 'NONE', *, *, #4935, .F. ) ;
#40357 = VECTOR ( 'NONE', #43535, 1000.000000000000000 ) ;
#40358 = ADVANCED_FACE ( 'NONE', ( #1587 ), #6573, .F. ) ;
#40359 = CIRCLE ( 'NONE', #32509, 0.2000000000000005107 ) ;
#40360 = CARTESIAN_POINT ( 'NONE',  ( 289.7500000000000000, -42.25000000000000000, -26.75000000000000000 ) ) ;
#40361 = DIRECTION ( 'NONE',  ( -1.000000000000000000, 0.000000000000000000, 0.000000000000000000 ) ) ;
#40362 = DIRECTION ( 'NONE',  ( -0.5000000000000049960, -0.8660254037844358210, -6.723777587268367771E-17 ) ) ;
#40365 = ORIENTED_EDGE ( 'NONE', *, *, #20933, .T. ) ;
#40364 = EDGE_CURVE ( 'NONE', #32104, #18160, #9072, .T. ) ;
#40363 = CARTESIAN_POINT ( 'NONE',  ( 7.450000000000003730, -7.249999999999997335, -24.00000000000000000 ) ) ;
#40366 = ORIENTED_EDGE ( 'NONE', *, *, #17366, .F. ) ;
#40367 = EDGE_CURVE ( 'NONE', #60151, #19555, #5527, .T. ) ;
#40368 = FACE_OUTER_BOUND ( 'NONE', #22811, .T. ) ;
#40369 = AXIS2_PLACEMENT_3D ( 'NONE', #64160, #52485, #20996 ) ;
#40370 = LINE ( 'NONE', #17402, #1854 ) ;
#40371 = VECTOR ( 'NONE', #51557, 1000.000000000000114 ) ;
#40372 = LINE ( 'NONE', #67598, #31850 ) ;
#40373 = CARTESIAN_POINT ( 'NONE',  ( -6.817976262117261044, 9.897976262117179402, 54.00000000000000711 ) ) ;
#40374 = DIRECTION ( 'NONE',  ( 0.6414496315691539108, -0.7671651518153028704, -2.587583378555131256E-16 ) ) ;
#40375 = EDGE_CURVE ( 'NONE', #5297, #30586, #44715, .T. ) ;
#40376 = CARTESIAN_POINT ( 'NONE',  ( -7.281754163448141526, 8.000000000000000000, 0.000000000000000000 ) ) ;
#40377 = DIRECTION ( 'NONE',  ( 0.000000000000000000, 0.000000000000000000, -1.000000000000000000 ) ) ;
#40378 = ORIENTED_EDGE ( 'NONE', *, *, #66694, .F. ) ;
#40379 = CARTESIAN_POINT ( 'NONE',  ( -6.651770455163781293, -7.357023737882790293, 54.00000000000000711 ) ) ;
#40381 = ORIENTED_EDGE ( 'NONE', *, *, #46488, .T. ) ;
#40380 = CARTESIAN_POINT ( 'NONE',  ( -7.250000000000001776, -7.249999999999998224, -12.50000000000000000 ) ) ;
#40382 = VECTOR ( 'NONE', #5945, 1000.000000000000000 ) ;
#40383 = DIRECTION ( 'NONE',  ( -3.491481338843132961E-15, -1.000000000000000000, 0.000000000000000000 ) ) ;
#40384 = DIRECTION ( 'NONE',  ( 1.000000000000000000, 0.000000000000000000, 0.000000000000000000 ) ) ;
#40385 = CARTESIAN_POINT ( 'NONE',  ( 8.835729544836290472, 2.530476262117160591, 54.00000000000000711 ) ) ;
#40386 = DIRECTION ( 'NONE',  ( -1.000000000000000000, 0.000000000000000000, 0.000000000000000000 ) ) ;
#40387 = DIRECTION ( 'NONE',  ( 0.000000000000000000, -0.000000000000000000, 1.000000000000000000 ) ) ;
#40388 = EDGE_LOOP ( 'NONE', ( #36038, #17911, #695, #4003 ) ) ;
#40389 = DIRECTION ( 'NONE',  ( 1.000000000000000000, -8.540177112501197482E-15, 0.000000000000000000 ) ) ;
#40390 = VERTEX_POINT ( 'NONE', #43702 ) ;
#40391 = DIRECTION ( 'NONE',  ( 0.5000000000000038858, 0.8660254037844363761, 3.181725716174712116E-16 ) ) ;
#40392 = DIRECTION ( 'NONE',  ( -0.000000000000000000, 1.000000000000000000, -0.000000000000000000 ) ) ;
#40393 = CARTESIAN_POINT ( 'NONE',  ( 0.000000000000000000, 0.000000000000000000, -11.50000000000000000 ) ) ;
#40394 = EDGE_LOOP ( 'NONE', ( #24251, #60496, #30487, #16093 ) ) ;
#40395 = PLANE ( 'NONE',  #27112 ) ;
#40396 = ORIENTED_EDGE ( 'NONE', *, *, #10273, .F. ) ;
#40397 = CIRCLE ( 'NONE', #16700, 1.500000000000000444 ) ;
#40398 = ORIENTED_EDGE ( 'NONE', *, *, #53871, .T. ) ;
#40399 = CARTESIAN_POINT ( 'NONE',  ( -9.689726262117227762, 8.566576262117216345, 54.00000000000000711 ) ) ;
#40400 = CARTESIAN_POINT ( 'NONE',  ( 8.250000000000005329, -7.249999999999998224, -16.00000000000000000 ) ) ;
#40401 = VERTEX_POINT ( 'NONE', #23157 ) ;
#40402 = DIRECTION ( 'NONE',  ( 1.000000000000000000, -1.883404846338789915E-14, 1.836970198720995421E-16 ) ) ;
#40403 = DIRECTION ( 'NONE',  ( 1.000000000000000000, 0.000000000000000000, 0.000000000000000000 ) ) ;
#40404 = DIRECTION ( 'NONE',  ( -1.000000000000000000, 0.000000000000000000, 0.000000000000000000 ) ) ;
#40405 = ORIENTED_EDGE ( 'NONE', *, *, #21582, .F. ) ;
#40406 = ORIENTED_EDGE ( 'NONE', *, *, #24236, .F. ) ;
#40407 = ADVANCED_FACE ( 'NONE', ( #44367 ), #48660, .F. ) ;
#40409 = ORIENTED_EDGE ( 'NONE', *, *, #68714, .T. ) ;
#40408 = LINE ( 'NONE', #55974, #32862 ) ;
#40410 = ADVANCED_FACE ( 'NONE', ( #6216 ), #11846, .T. ) ;
#40411 = EDGE_LOOP ( 'NONE', ( #61363, #60005, #38973, #33061 ) ) ;
#40412 = AXIS2_PLACEMENT_3D ( 'NONE', #51982, #36780, #8841 ) ;
#40413 = CARTESIAN_POINT ( 'NONE',  ( 4.406483450353335662, -11.78648345035347766, 455.0000000000000568 ) ) ;
#40414 = CARTESIAN_POINT ( 'NONE',  ( 30.00000000000000000, -12.00000000000000000, -10.20500000000000007 ) ) ;
#40415 = ADVANCED_FACE ( 'NONE', ( #38062 ), #27781, .F. ) ;
#40416 = DIRECTION ( 'NONE',  ( -1.000000000000000000, 0.000000000000000000, 0.000000000000000000 ) ) ;
#40417 = CARTESIAN_POINT ( 'NONE',  ( 6.500000000000002665, 6.500000000000000888, -1.000000000000000000 ) ) ;
#40418 = EDGE_CURVE ( 'NONE', #13431, #65287, #221, .T. ) ;
#40419 = AXIS2_PLACEMENT_3D ( 'NONE', #7502, #8193, #18106 ) ;
#40421 =( NAMED_UNIT ( * ) SI_UNIT ( $, .STERADIAN. ) SOLID_ANGLE_UNIT ( ) );
#40420 = AXIS2_PLACEMENT_3D ( 'NONE', #36979, #26349, #42256 ) ;
#40422 = PLANE ( 'NONE',  #58065 ) ;
#40423 = ORIENTED_EDGE ( 'NONE', *, *, #2200, .F. ) ;
#40424 = ORIENTED_EDGE ( 'NONE', *, *, #49261, .T. ) ;
#40425 = ORIENTED_EDGE ( 'NONE', *, *, #28877, .T. ) ;
#40426 = ORIENTED_EDGE ( 'NONE', *, *, #385, .T. ) ;
#40427 = DIRECTION ( 'NONE',  ( -5.163402228214836012E-15, -1.000000000000000000, -1.836970198721026976E-16 ) ) ;
#40428 = APPLICATION_CONTEXT ( 'automotive_design' ) ;
#40429 = ADVANCED_FACE ( 'NONE', ( #64925 ), #49366, .T. ) ;
#40430 = CARTESIAN_POINT ( 'NONE',  ( -7.450000000000001954, -7.249999999999998224, -12.00000000000000000 ) ) ;
#40431 = EDGE_CURVE ( 'NONE', #527, #46607, #16483, .T. ) ;
#40432 = VECTOR ( 'NONE', #30562, 1000.000000000000000 ) ;
#40433 = DIRECTION ( 'NONE',  ( -0.000000000000000000, 3.673940397442059868E-16, -1.000000000000000000 ) ) ;
#40434 = VERTEX_POINT ( 'NONE', #3965 ) ;
#40435 = ORIENTED_EDGE ( 'NONE', *, *, #10655, .F. ) ;
#40436 = VERTEX_POINT ( 'NONE', #50380 ) ;
#40437 = CARTESIAN_POINT ( 'NONE',  ( -8.697938382363185283, -8.093267424590415260, 54.00000000000000711 ) ) ;
#40438 = ORIENTED_EDGE ( 'NONE', *, *, #8202, .F. ) ;
#40439 = VERTEX_POINT ( 'NONE', #9267 ) ;
#40440 = DIRECTION ( 'NONE',  ( 0.000000000000000000, 0.7071067811865455743, 0.7071067811865495711 ) ) ;
#40441 = VERTEX_POINT ( 'NONE', #14215 ) ;
#40442 = ORIENTED_EDGE ( 'NONE', *, *, #6846, .T. ) ;
#40443 = PLANE ( 'NONE',  #64421 ) ;
#40445 = ORIENTED_EDGE ( 'NONE', *, *, #26934, .T. ) ;
#40444 = LINE ( 'NONE', #1563, #44633 ) ;
#40446 = VERTEX_POINT ( 'NONE', #34106 ) ;
#40447 = DIRECTION ( 'NONE',  ( 0.000000000000000000, 0.000000000000000000, 1.000000000000000000 ) ) ;
#40448 = LINE ( 'NONE', #12515, #48786 ) ;
#40449 = LINE ( 'NONE', #67671, #39200 ) ;
#40450 = VECTOR ( 'NONE', #16680, 1000.000000000000000 ) ;
#40452 = ORIENTED_EDGE ( 'NONE', *, *, #3950, .T. ) ;
#40451 = DIRECTION ( 'NONE',  ( 0.000000000000000000, 0.000000000000000000, -1.000000000000000000 ) ) ;
#40453 = ORIENTED_EDGE ( 'NONE', *, *, #47921, .T. ) ;
#40454 = DIRECTION ( 'NONE',  ( -1.000000000000000000, 0.000000000000000000, 0.000000000000000000 ) ) ;
#40455 = DIRECTION ( 'NONE',  ( 0.000000000000000000, 1.000000000000000000, 0.000000000000000000 ) ) ;
#40456 = EDGE_CURVE ( 'NONE', #17044, #19926, #41783, .T. ) ;
#40457 = CARTESIAN_POINT ( 'NONE',  ( 47.00000000000000000, 0.7500000000000000000, -5.000000000000000000 ) ) ;
#40458 = VERTEX_POINT ( 'NONE', #19512 ) ;
#40459 = LINE ( 'NONE', #35141, #7747 ) ;
#40460 = DIRECTION ( 'NONE',  ( 0.000000000000000000, 0.000000000000000000, 1.000000000000000000 ) ) ;
#40461 = CARTESIAN_POINT ( 'NONE',  ( 48.50000000000000000, 0.7500000000000000000, -3.418698582794335028 ) ) ;
#40462 = ORIENTED_EDGE ( 'NONE', *, *, #15980, .T. ) ;
#40463 = CARTESIAN_POINT ( 'NONE',  ( -8.916576262117356322, -10.05377373788272877, 26.00000000000000000 ) ) ;
#40464 = VECTOR ( 'NONE', #13040, 1000.000000000000000 ) ;
#40465 = ADVANCED_FACE ( 'NONE', ( #28804 ), #62295, .F. ) ;
#40466 = CARTESIAN_POINT ( 'NONE',  ( -9.897976262117257562, 3.667976262117184749, 26.00000000000000711 ) ) ;
#40467 = DIRECTION ( 'NONE',  ( 0.000000000000000000, 0.000000000000000000, 1.000000000000000000 ) ) ;
#40468 = EDGE_LOOP ( 'NONE', ( #18781, #53175, #683, #58257, #68254, #62232 ) ) ;
#40469 = ADVANCED_FACE ( 'NONE', ( #68673 ), #23511, .F. ) ;
#40470 = CARTESIAN_POINT ( 'NONE',  ( 289.5000000000000000, 0.000000000000000000, 26.50000000000000000 ) ) ;
#40471 = FACE_OUTER_BOUND ( 'NONE', #8272, .T. ) ;
#40472 = ORIENTED_EDGE ( 'NONE', *, *, #4067, .F. ) ;
#40473 = FACE_OUTER_BOUND ( 'NONE', #31979, .T. ) ;
#40474 = LINE ( 'NONE', #60657, #15078 ) ;
#40475 = LINE ( 'NONE', #57091, #60158 ) ;
#40476 = LINE ( 'NONE', #56046, #10949 ) ;
#40477 = FACE_OUTER_BOUND ( 'NONE', #50065, .T. ) ;
#40478 = VERTEX_POINT ( 'NONE', #41080 ) ;
#40479 = LINE ( 'NONE', #45079, #32151 ) ;
#40480 = LINE ( 'NONE', #57097, #26039 ) ;
#40481 = EDGE_CURVE ( 'NONE', #2624, #35475, #55409, .T. ) ;
#40482 = CARTESIAN_POINT ( 'NONE',  ( -28.00000000000000000, -17.00000000000000000, 15.70499999999969809 ) ) ;
#40483 =( NAMED_UNIT ( * ) SI_UNIT ( $, .STERADIAN. ) SOLID_ANGLE_UNIT ( ) );
#40484 = EDGE_LOOP ( 'NONE', ( #32141, #9578, #17962, #9206 ) ) ;
#40486 = EDGE_LOOP ( 'NONE', ( #16753, #58258, #48812, #14541 ) ) ;
#40485 = DIRECTION ( 'NONE',  ( 0.000000000000000000, 0.000000000000000000, 1.000000000000000000 ) ) ;
#40487 = EDGE_CURVE ( 'NONE', #43744, #63779, #7233, .T. ) ;
#40488 = LINE ( 'NONE', #40840, #28237 ) ;
#40489 = ADVANCED_FACE ( 'NONE', ( #63010 ), #20216, .T. ) ;
#40490 = LINE ( 'NONE', #55377, #42483 ) ;
#40491 = VERTEX_POINT ( 'NONE', #19168 ) ;
#40492 = ADVANCED_FACE ( 'NONE', ( #63364 ), #55688, .T. ) ;
#40493 = DIRECTION ( 'NONE',  ( -7.808916176531286882E-15, -1.000000000000000000, 0.000000000000000000 ) ) ;
#40494 = ADVANCED_FACE ( 'NONE', ( #25537 ), #40739, .F. ) ;
#40495 = ORIENTED_EDGE ( 'NONE', *, *, #7554, .T. ) ;
#40496 = AXIS2_PLACEMENT_3D ( 'NONE', #47910, #57119, #19632 ) ;
#40497 = FACE_OUTER_BOUND ( 'NONE', #40158, .T. ) ;
#40498 = ORIENTED_EDGE ( 'NONE', *, *, #7594, .F. ) ;
#40499 = ORIENTED_EDGE ( 'NONE', *, *, #49172, .F. ) ;
#40501 = ADVANCED_FACE ( 'NONE', ( #30131 ), #51709, .T. ) ;
#40500 = DIRECTION ( 'NONE',  ( 1.000000000000000000, -1.671920889371702854E-15, 0.000000000000000000 ) ) ;
#40502 = PLANE ( 'NONE',  #54624 ) ;
#40503 = EDGE_CURVE ( 'NONE', #29633, #33288, #47487, .T. ) ;
#40504 = AXIS2_PLACEMENT_3D ( 'NONE', #35442, #24505, #2231 ) ;
#40505 = DIRECTION ( 'NONE',  ( 1.000000000000000000, 0.000000000000000000, 0.000000000000000000 ) ) ;
#40506 = DIRECTION ( 'NONE',  ( -0.000000000000000000, -0.000000000000000000, 1.000000000000000000 ) ) ;
#40507 = ORIENTED_EDGE ( 'NONE', *, *, #53281, .T. ) ;
#40508 = VERTEX_POINT ( 'NONE', #14925 ) ;
#40509 = DIRECTION ( 'NONE',  ( 0.000000000000000000, 0.000000000000000000, -1.000000000000000000 ) ) ;
#40510 = CIRCLE ( 'NONE', #12235, 4.500000000000191847 ) ;
#40511 = CARTESIAN_POINT ( 'NONE',  ( -11.07551654964681731, -9.804883450353372609, 455.0000000000000568 ) ) ;
#40512 = ORIENTED_EDGE ( 'NONE', *, *, #38427, .F. ) ;
#40513 = ADVANCED_FACE ( 'NONE', ( #30478 ), #19862, .T. ) ;
#40514 = ORIENTED_EDGE ( 'NONE', *, *, #68604, .F. ) ;
#40515 = ORIENTED_EDGE ( 'NONE', *, *, #64056, .F. ) ;
#40516 = AXIS2_PLACEMENT_3D ( 'NONE', #39940, #61513, #56232 ) ;
#40517 = DIRECTION ( 'NONE',  ( 0.000000000000000000, 1.000000000000000000, 0.000000000000000000 ) ) ;
#40519 = EDGE_LOOP ( 'NONE', ( #4474, #45254, #32957, #25128 ) ) ;
#40518 = CARTESIAN_POINT ( 'NONE',  ( 7.250000000000005329, -7.249999999999998224, -8.000000000000000000 ) ) ;
#40520 = CARTESIAN_POINT ( 'NONE',  ( 8.250000000000005329, -7.249999999999998224, -26.00000000000001066 ) ) ;
#40521 = DIRECTION ( 'NONE',  ( -0.000000000000000000, 3.673940397442059868E-16, -1.000000000000000000 ) ) ;
#40522 = EDGE_CURVE ( 'NONE', #59443, #47101, #36127, .T. ) ;
#40523 = ORIENTED_EDGE ( 'NONE', *, *, #41343, .F. ) ;
#40524 = ORIENTED_EDGE ( 'NONE', *, *, #38318, .T. ) ;
#40525 = CIRCLE ( 'NONE', #10067, 4.000000000000000000 ) ;
#40526 = EDGE_CURVE ( 'NONE', #11040, #3811, #24872, .T. ) ;
#40527 = FACE_OUTER_BOUND ( 'NONE', #45506, .T. ) ;
#40528 = CARTESIAN_POINT ( 'NONE',  ( -7.250000000000000888, -8.249999999999998224, -26.00000000000001066 ) ) ;
#40529 = DIRECTION ( 'NONE',  ( 0.000000000000000000, 0.000000000000000000, 1.000000000000000000 ) ) ;
#40530 = EDGE_CURVE ( 'NONE', #59528, #23856, #31197, .T. ) ;
#40531 = CARTESIAN_POINT ( 'NONE',  ( 49.00000000000000000, -14.06939075806900163, -20.80000000000000426 ) ) ;
#40532 = LINE ( 'NONE', #24280, #38114 ) ;
#40534 = ORIENTED_EDGE ( 'NONE', *, *, #41605, .T. ) ;
#40533 = PLANE ( 'NONE',  #45726 ) ;
#40535 = ORIENTED_EDGE ( 'NONE', *, *, #37555, .T. ) ;
#40536 = EDGE_CURVE ( 'NONE', #11215, #24412, #26229, .T. ) ;
#40537 = LINE ( 'NONE', #35218, #63723 ) ;
#40538 = FACE_OUTER_BOUND ( 'NONE', #8502, .T. ) ;
#40539 = DIRECTION ( 'NONE',  ( 1.047444401652940007E-14, 1.000000000000000000, 1.836970198721029934E-16 ) ) ;
#40540 = DIRECTION ( 'NONE',  ( 1.000000000000000000, 0.000000000000000000, 0.000000000000000000 ) ) ;
#40541 = VECTOR ( 'NONE', #12242, 1000.000000000000000 ) ;
#40542 = ADVANCED_FACE ( 'NONE', ( #37198 ), #48149, .F. ) ;
#40543 = DIRECTION ( 'NONE',  ( 0.000000000000000000, -0.9921567416492215186, 0.1249999999999996531 ) ) ;
#40544 = ORIENTED_EDGE ( 'NONE', *, *, #10064, .F. ) ;
#40545 = FACE_OUTER_BOUND ( 'NONE', #4642, .T. ) ;
#40546 = CARTESIAN_POINT ( 'NONE',  ( -8.250000000000000000, 7.250000000000001776, -24.00000000000000000 ) ) ;
#40547 = CARTESIAN_POINT ( 'NONE',  ( 11.25000000000000178, -11.18999999999999950, -4.250000000000000000 ) ) ;
#40548 = CARTESIAN_POINT ( 'NONE',  ( -10.49297626211726175, 3.650476262117184234, 54.00000000000000711 ) ) ;
#40549 = CARTESIAN_POINT ( 'NONE',  ( 10.92648345035335922, 2.693516549646528091, 455.0000000000000568 ) ) ;
#40550 = EDGE_CURVE ( 'NONE', #51881, #40074, #11346, .T. ) ;
#40551 = CARTESIAN_POINT ( 'NONE',  ( -11.07551654964682797, -11.08848345035333693, 455.0000000000000568 ) ) ;
#40552 = ADVANCED_FACE ( 'NONE', ( #47439 ), #69011, .T. ) ;
#40553 = AXIS2_PLACEMENT_3D ( 'NONE', #36201, #9338, #42906 ) ;
#40554 = CARTESIAN_POINT ( 'NONE',  ( 10.00000000000000000, -21.00000000000000000, -18.00000000000000355 ) ) ;
#40555 = ORIENTED_EDGE ( 'NONE', *, *, #61710, .T. ) ;
#40556 = FACE_OUTER_BOUND ( 'NONE', #717, .T. ) ;
#40557 = DIRECTION ( 'NONE',  ( -1.000000000000000000, 0.000000000000000000, 0.000000000000000000 ) ) ;
#40558 = ADVANCED_FACE ( 'NONE', ( #20917 ), #31543, .T. ) ;
#40559 = EDGE_LOOP ( 'NONE', ( #28155, #2653, #27918, #2135 ) ) ;
#40560 = CARTESIAN_POINT ( 'NONE',  ( -6.822336235477489019, -6.364920264886856138, 26.00000000000000711 ) ) ;
#40561 = EDGE_CURVE ( 'NONE', #55382, #61299, #67823, .T. ) ;
#40562 = EDGE_CURVE ( 'NONE', #18663, #23009, #42132, .T. ) ;
#40563 = FACE_OUTER_BOUND ( 'NONE', #63945, .T. ) ;
#40564 = VECTOR ( 'NONE', #23419, 1000.000000000000000 ) ;
#40565 = DIRECTION ( 'NONE',  ( 0.000000000000000000, -3.673940397442059868E-16, 1.000000000000000000 ) ) ;
#40566 = CARTESIAN_POINT ( 'NONE',  ( -7.798499376344067535, 4.727349090213368576, 195.0000000000000284 ) ) ;
#40567 = DIRECTION ( 'NONE',  ( 0.000000000000000000, 0.000000000000000000, 1.000000000000000000 ) ) ;
#40568 = ORIENTED_EDGE ( 'NONE', *, *, #48780, .F. ) ;
#40569 = EDGE_CURVE ( 'NONE', #68865, #56239, #42487, .T. ) ;
#40570 = AXIS2_PLACEMENT_3D ( 'NONE', #1954, #55358, #23516 ) ;
#40571 = DIRECTION ( 'NONE',  ( -0.000000000000000000, 3.673940397442059868E-16, -1.000000000000000000 ) ) ;
#40572 = EDGE_LOOP ( 'NONE', ( #12039, #38899, #26103, #45688 ) ) ;
#40573 = FACE_OUTER_BOUND ( 'NONE', #32766, .T. ) ;
#40574 = EDGE_CURVE ( 'NONE', #33150, #42593, #10316, .T. ) ;
#40575 = CARTESIAN_POINT ( 'NONE',  ( 39.00000000000000000, 16.96999999999999886, 21.00000000000000000 ) ) ;
#40576 = EDGE_LOOP ( 'NONE', ( #12505, #25529, #52341, #40789 ) ) ;
#40577 = DIRECTION ( 'NONE',  ( 1.836970198721029934E-16, 1.836970198721010706E-16, -1.000000000000000000 ) ) ;
#40578 = ADVANCED_FACE ( 'NONE', ( #31889 ), #53459, .F. ) ;
#40579 = VECTOR ( 'NONE', #65924, 1000.000000000000000 ) ;
#40580 = ORIENTED_EDGE ( 'NONE', *, *, #51431, .T. ) ;
#40581 = DIRECTION ( 'NONE',  ( 0.000000000000000000, 0.000000000000000000, 1.000000000000000000 ) ) ;
#40582 = ORIENTED_EDGE ( 'NONE', *, *, #45403, .F. ) ;
#40583 = ORIENTED_EDGE ( 'NONE', *, *, #46973, .T. ) ;
#40585 = EDGE_CURVE ( 'NONE', #61368, #4952, #16676, .T. ) ;
#40584 = CARTESIAN_POINT ( 'NONE',  ( 5.393625297349901260, -4.747751991980754482, 455.0000000000000568 ) ) ;
#40586 = ORIENTED_EDGE ( 'NONE', *, *, #1370, .F. ) ;
#40587 = ORIENTED_EDGE ( 'NONE', *, *, #7463, .F. ) ;
#40588 = EDGE_CURVE ( 'NONE', #30915, #52575, #58423, .T. ) ;
#40589 = LINE ( 'NONE', #2410, #18034 ) ;
#40590 = CARTESIAN_POINT ( 'NONE',  ( -7.250000000000000888, 8.250000000000001776, -26.00000000000001066 ) ) ;
#40591 = FACE_OUTER_BOUND ( 'NONE', #30896, .T. ) ;
#40592 = CIRCLE ( 'NONE', #57554, 4.500000000000190958 ) ;
#40593 = ORIENTED_EDGE ( 'NONE', *, *, #44228, .F. ) ;
#40594 = LINE ( 'NONE', #29985, #28896 ) ;
#40596 = FACE_OUTER_BOUND ( 'NONE', #41652, .T. ) ;
#40595 = CARTESIAN_POINT ( 'NONE',  ( 275.0000000000000000, -23.29603921945599865, 12.50000000000000000 ) ) ;
#40597 = VERTEX_POINT ( 'NONE', #59098 ) ;
#40599 = ORIENTED_EDGE ( 'NONE', *, *, #58008, .T. ) ;
#40598 = CARTESIAN_POINT ( 'NONE',  ( 30.00000000000000000, -9.487228132326899654, -12.50000000000000000 ) ) ;
#40600 = ORIENTED_EDGE ( 'NONE', *, *, #2112, .T. ) ;
#40601 = PRODUCT_CONTEXT ( 'NONE', #23686, 'mechanical' ) ;
#40602 = FACE_OUTER_BOUND ( 'NONE', #48665, .T. ) ;
#40603 = VECTOR ( 'NONE', #35174, 1000.000000000000000 ) ;
#40604 = CIRCLE ( 'NONE', #65457, 4.000000000000000888 ) ;
#40605 = VERTEX_POINT ( 'NONE', #26935 ) ;
#40606 = CARTESIAN_POINT ( 'NONE',  ( 289.5000000000000000, -42.00000000000000000, 27.00000000000000000 ) ) ;
#40607 = DIRECTION ( 'NONE',  ( 0.000000000000000000, 0.000000000000000000, -1.000000000000000000 ) ) ;
#40608 = ORIENTED_EDGE ( 'NONE', *, *, #58669, .F. ) ;
#40609 = VERTEX_POINT ( 'NONE', #5380 ) ;
#40610 = AXIS2_PLACEMENT_3D ( 'NONE', #45231, #56550, #51243 ) ;
#40611 = CARTESIAN_POINT ( 'NONE',  ( 26.90000000000000213, 2.904780276981809389E-16, 2.285366197183106074 ) ) ;
#40612 = CARTESIAN_POINT ( 'NONE',  ( -11.50000000000000000, -11.50000000000100009, 19.50000000000103739 ) ) ;
#40613 = VERTEX_POINT ( 'NONE', #10658 ) ;
#40614 = VECTOR ( 'NONE', #45965, 1000.000000000000000 ) ;
#40615 = EDGE_CURVE ( 'NONE', #10693, #39291, #32229, .T. ) ;
#40616 = DIRECTION ( 'NONE',  ( 1.836970198721029934E-16, 1.836970198721010706E-16, -1.000000000000000000 ) ) ;
#40617 = DIRECTION ( 'NONE',  ( 1.836970198721029934E-16, 1.836970198721010706E-16, -1.000000000000000000 ) ) ;
#40618 = DIRECTION ( 'NONE',  ( -0.000000000000000000, -0.000000000000000000, 1.000000000000000000 ) ) ;
#40619 = ORIENTED_EDGE ( 'NONE', *, *, #45337, .F. ) ;
#40620 = AXIS2_PLACEMENT_3D ( 'NONE', #22743, #43960, #151 ) ;
#40621 = ADVANCED_FACE ( 'NONE', ( #4667 ), #54154, .F. ) ;
#40622 = CARTESIAN_POINT ( 'NONE',  ( -11.00000000000000000, -17.50000000000000000, -26.64999999999900027 ) ) ;
#40623 = CARTESIAN_POINT ( 'NONE',  ( 282.6457513110646005, -20.50000000000000000, 17.00000000000000000 ) ) ;
#40625 = ORIENTED_EDGE ( 'NONE', *, *, #4743, .T. ) ;
#40624 = FILL_AREA_STYLE_COLOUR ( '', #61307 ) ;
#40627 = VERTEX_POINT ( 'NONE', #63 ) ;
#40626 = CARTESIAN_POINT ( 'NONE',  ( -8.250000000000001776, 0.000000000000000000, -12.00000000000000000 ) ) ;
#40628 = EDGE_CURVE ( 'NONE', #22525, #6513, #43175, .T. ) ;
#40629 = DIRECTION ( 'NONE',  ( -1.000000000000000000, 1.130039751537442024E-14, 0.000000000000000000 ) ) ;
#40630 = AXIS2_PLACEMENT_3D ( 'NONE', #3682, #14639, #9335 ) ;
#40631 = LINE ( 'NONE', #57247, #32993 ) ;
#40632 = EDGE_CURVE ( 'NONE', #16696, #6609, #24970, .T. ) ;
#40633 = CARTESIAN_POINT ( 'NONE',  ( -2.893516549646681035, 10.08346604330774632, 455.0000000000000568 ) ) ;
#40634 = LINE ( 'NONE', #19416, #37324 ) ;
#40635 = EDGE_CURVE ( 'NONE', #66346, #34593, #5760, .T. ) ;
#40636 = CARTESIAN_POINT ( 'NONE',  ( -9.690000000000001279, 9.750000000000001776, -4.250000000000000000 ) ) ;
#40637 = ORIENTED_EDGE ( 'NONE', *, *, #20710, .T. ) ;
#40638 = LINE ( 'NONE', #13763, #32399 ) ;
#40639 = CARTESIAN_POINT ( 'NONE',  ( 283.0000000000000568, -32.46196062927499781, -8.091291340630698770 ) ) ;
#40641 = VERTEX_POINT ( 'NONE', #12360 ) ;
#40640 = DIRECTION ( 'NONE',  ( -1.836970198721029934E-16, 1.836970198721036590E-16, -1.000000000000000000 ) ) ;
#40642 = CARTESIAN_POINT ( 'NONE',  ( 2.005523737882793256, -8.612468434717222010, 54.00000000000000711 ) ) ;
#40643 = AXIS2_PLACEMENT_3D ( 'NONE', #3054, #68094, #14705 ) ;
#40644 = LINE ( 'NONE', #8823, #67994 ) ;
#40645 = ORIENTED_EDGE ( 'NONE', *, *, #21881, .F. ) ;
#40646 = ORIENTED_EDGE ( 'NONE', *, *, #15487, .F. ) ;
#40647 = CARTESIAN_POINT ( 'NONE',  ( 1.480523737882811330, 9.390476262117216422, 26.00000000000000711 ) ) ;
#40648 = CARTESIAN_POINT ( 'NONE',  ( 30.00000000000000000, -14.04000000000000092, 14.80000000000000071 ) ) ;
#40649 = ORIENTED_EDGE ( 'NONE', *, *, #65786, .T. ) ;
#40650 = ADVANCED_FACE ( 'NONE', ( #33611 ), #1425, .T. ) ;
#40651 = CARTESIAN_POINT ( 'NONE',  ( -25.50000000000000355, -5.578999999999999737, -20.87900000000000134 ) ) ;
#40652 = CARTESIAN_POINT ( 'NONE',  ( -17.00000000000000000, -17.50000000000000000, 19.33772233983200195 ) ) ;
#40653 = AXIS2_PLACEMENT_3D ( 'NONE', #40715, #24458, #25518 ) ;
#40654 = LINE ( 'NONE', #18377, #10146 ) ;
#40655 = CIRCLE ( 'NONE', #2249, 2.204799999999997429 ) ;
#40656 = VECTOR ( 'NONE', #52257, 1000.000000000000000 ) ;
#40657 = CARTESIAN_POINT ( 'NONE',  ( 0.000000000000000000, -8.249999999999998224, -18.50000000000000000 ) ) ;
#40658 = AXIS2_PLACEMENT_3D ( 'NONE', #61693, #67703, #7948 ) ;
#40659 = ORIENTED_EDGE ( 'NONE', *, *, #13272, .F. ) ;
#40660 = DIRECTION ( 'NONE',  ( 1.000000000000000000, 0.000000000000000000, -0.000000000000000000 ) ) ;
#40661 = ORIENTED_EDGE ( 'NONE', *, *, #35938, .T. ) ;
#40662 = ORIENTED_EDGE ( 'NONE', *, *, #66259, .T. ) ;
#40663 = CIRCLE ( 'NONE', #19214, 4.000000000000000888 ) ;
#40664 = CARTESIAN_POINT ( 'NONE',  ( -8.130476262117259267, 8.821682069070703847, 54.00000000000000711 ) ) ;
#40665 = AXIS2_PLACEMENT_3D ( 'NONE', #42410, #32149, #63996 ) ;
#40666 = SURFACE_STYLE_FILL_AREA ( #67551 ) ;
#40667 = FACE_OUTER_BOUND ( 'NONE', #52095, .T. ) ;
#40668 = ORIENTED_EDGE ( 'NONE', *, *, #56944, .F. ) ;
#40669 = ORIENTED_EDGE ( 'NONE', *, *, #4548, .F. ) ;
#40670 = VECTOR ( 'NONE', #28098, 1000.000000000000000 ) ;
#40672 = ADVANCED_FACE ( 'NONE', ( #50213 ), #38913, .F. ) ;
#40671 = CARTESIAN_POINT ( 'NONE',  ( -8.250000000000001776, 7.250000000000000888, -26.00000000000001066 ) ) ;
#40673 = ORIENTED_EDGE ( 'NONE', *, *, #1537, .F. ) ;
#40674 = CIRCLE ( 'NONE', #24727, 0.1749999999999998224 ) ;
#40675 = ORIENTED_EDGE ( 'NONE', *, *, #7618, .T. ) ;
#40676 = EDGE_CURVE ( 'NONE', #22000, #13327, #45239, .T. ) ;
#40677 = CARTESIAN_POINT ( 'NONE',  ( 7.250000000000005329, -8.249999999999998224, -22.00000000000000000 ) ) ;
#40678 = CARTESIAN_POINT ( 'NONE',  ( 7.250000000000005329, -7.449999999999998401, -22.00000000000000000 ) ) ;
#40679 = DIRECTION ( 'NONE',  ( 7.665540703601094997E-15, 1.000000000000000000, 0.000000000000000000 ) ) ;
#40680 = PLANE ( 'NONE',  #24110 ) ;
#40681 = ORIENTED_EDGE ( 'NONE', *, *, #33163, .F. ) ;
#40682 = DIRECTION ( 'NONE',  ( -0.7671651518153105309, 0.6414496315691445849, 2.356647714346206145E-16 ) ) ;
#40683 = VECTOR ( 'NONE', #56286, 1000.000000000000000 ) ;
#40684 = VECTOR ( 'NONE', #61367, 1000.000000000000000 ) ;
#40686 = DIRECTION ( 'NONE',  ( -0.000000000000000000, -0.000000000000000000, -1.000000000000000000 ) ) ;
#40685 = CARTESIAN_POINT ( 'NONE',  ( 7.450000000000006395, 7.250000000000000888, -21.50000000000000000 ) ) ;
#40687 = VERTEX_POINT ( 'NONE', #18026 ) ;
#40689 = ORIENTED_EDGE ( 'NONE', *, *, #37939, .T. ) ;
#40688 = FACE_OUTER_BOUND ( 'NONE', #64935, .T. ) ;
#40690 = EDGE_LOOP ( 'NONE', ( #54097, #8167, #5142, #60676, #7507, #52337, #45956, #23917, #49390, #48365, #69168, #60320, #26193, #25466, #40524, #41496, #67093 ) ) ;
#40691 = ORIENTED_EDGE ( 'NONE', *, *, #16554, .F. ) ;
#40692 = DIRECTION ( 'NONE',  ( 1.000000000000000000, -0.000000000000000000, -0.000000000000000000 ) ) ;
#40693 = LINE ( 'NONE', #25135, #54148 ) ;
#40694 = AXIS2_PLACEMENT_3D ( 'NONE', #46605, #13021, #29284 ) ;
#40695 = EDGE_LOOP ( 'NONE', ( #24326, #16831, #8825, #57908 ) ) ;
#40696 = VERTEX_POINT ( 'NONE', #17338 ) ;
#40697 = CYLINDRICAL_SURFACE ( 'NONE', #46737, 0.8099999999999999423 ) ;
#40698 = DIRECTION ( 'NONE',  ( 1.000000000000000000, 2.312964634635741083E-15, 0.000000000000000000 ) ) ;
#40699 = VERTEX_POINT ( 'NONE', #1096 ) ;
#40700 = VERTEX_POINT ( 'NONE', #61502 ) ;
#40701 = CARTESIAN_POINT ( 'NONE',  ( 0.000000000000000000, 8.250000000000001776, -15.50000000000000000 ) ) ;
#40702 = VECTOR ( 'NONE', #21261, 1000.000000000000000 ) ;
#40703 = CARTESIAN_POINT ( 'NONE',  ( 35.89999999999999858, -0.2000000000089119934, 8.909539772616881237E-12 ) ) ;
#40704 = VECTOR ( 'NONE', #33911, 1000.000000000000000 ) ;
#40705 = VERTEX_POINT ( 'NONE', #65784 ) ;
#40706 = EDGE_CURVE ( 'NONE', #49824, #3823, #36222, .T. ) ;
#40707 = AXIS2_PLACEMENT_3D ( 'NONE', #63691, #36454, #43152 ) ;
#40708 = FACE_OUTER_BOUND ( 'NONE', #15690, .T. ) ;
#40709 = DIRECTION ( 'NONE',  ( -1.000000000000000000, 0.000000000000000000, 0.000000000000000000 ) ) ;
#40711 = ORIENTED_EDGE ( 'NONE', *, *, #33238, .F. ) ;
#40710 = CARTESIAN_POINT ( 'NONE',  ( -9.781776262117247711, 9.781776262117171328, 54.00000000000000711 ) ) ;
#40712 = VERTEX_POINT ( 'NONE', #17694 ) ;
#40714 = EDGE_CURVE ( 'NONE', #20883, #64619, #13068, .T. ) ;
#40713 = VECTOR ( 'NONE', #27083, 1000.000000000000000 ) ;
#40715 = CARTESIAN_POINT ( 'NONE',  ( 7.000000000000000000, -25.69999999999924967, 14.52500000000000213 ) ) ;
#40716 = CARTESIAN_POINT ( 'NONE',  ( 8.900000000000005684, -21.00000000000000000, 13.86939075806900057 ) ) ;
#40717 = EDGE_CURVE ( 'NONE', #37156, #38565, #56560, .T. ) ;
#40718 = LINE ( 'NONE', #55936, #7514 ) ;
#40719 = EDGE_CURVE ( 'NONE', #25093, #31165, #55182, .T. ) ;
#40720 = CARTESIAN_POINT ( 'NONE',  ( 0.2499999999999831524, -42.25000000000000000, 26.75000000000000711 ) ) ;
#40721 = AXIS2_PLACEMENT_3D ( 'NONE', #69890, #47281, #9452 ) ;
#40722 = PLANE ( 'NONE',  #44059 ) ;
#40723 = EDGE_CURVE ( 'NONE', #36943, #42522, #23805, .T. ) ;
#40724 = ADVANCED_FACE ( 'NONE', ( #55867 ), #60128, .F. ) ;
#40725 = CARTESIAN_POINT ( 'NONE',  ( 7.250000000000005329, 7.250000000000000888, -23.00000000000000000 ) ) ;
#40726 = VERTEX_POINT ( 'NONE', #33942 ) ;
#40727 = LINE ( 'NONE', #35404, #36026 ) ;
#40729 = ORIENTED_EDGE ( 'NONE', *, *, #1829, .T. ) ;
#40728 = CARTESIAN_POINT ( 'NONE',  ( -15.50000000000000000, -17.50000000000000000, -22.50000000000000000 ) ) ;
#40730 = DIRECTION ( 'NONE',  ( 1.836970198721029934E-16, 1.836970198721010706E-16, -1.000000000000000000 ) ) ;
#40731 = CARTESIAN_POINT ( 'NONE',  ( -11.00000000000000000, -5.200000000000001066, 26.59999999999999432 ) ) ;
#40732 = EDGE_CURVE ( 'NONE', #48512, #53541, #23347, .T. ) ;
#40733 = PLANE ( 'NONE',  #38176 ) ;
#40734 = DIRECTION ( 'NONE',  ( -0.000000000000000000, 0.000000000000000000, 1.000000000000000000 ) ) ;
#40735 = CIRCLE ( 'NONE', #18162, 4.000000000000000000 ) ;
#40736 = FACE_OUTER_BOUND ( 'NONE', #21724, .T. ) ;
#40737 = VERTEX_POINT ( 'NONE', #55527 ) ;
#40738 = CARTESIAN_POINT ( 'NONE',  ( 0.000000000000000000, 0.000000000000000000, 0.000000000000000000 ) ) ;
#40739 = PLANE ( 'NONE',  #68945 ) ;
#40740 = VERTEX_POINT ( 'NONE', #7069 ) ;
#40741 = FACE_OUTER_BOUND ( 'NONE', #5299, .T. ) ;
#40742 = CARTESIAN_POINT ( 'NONE',  ( 34.89999999999999858, -0.1999999999911430404, -8.864436962241481021E-12 ) ) ;
#40743 = EDGE_LOOP ( 'NONE', ( #528, #41920 ) ) ;
#40744 = AXIS2_PLACEMENT_3D ( 'NONE', #52992, #15151, #36715 ) ;
#40745 = DIRECTION ( 'NONE',  ( 7.304098846218132892E-15, 1.000000000000000000, 3.673940397442059868E-16 ) ) ;
#40746 = VERTEX_POINT ( 'NONE', #22327 ) ;
#40747 = EDGE_LOOP ( 'NONE', ( #29951, #56795, #58496, #17130 ) ) ;
#40748 = CARTESIAN_POINT ( 'NONE',  ( 1.480523737882816881, 9.390476262117212869, 54.00000000000000711 ) ) ;
#40749 = CARTESIAN_POINT ( 'NONE',  ( -9.828310488886053520, 2.277516549646603661, 455.0000000000000568 ) ) ;
#40750 = PLANE ( 'NONE',  #12973 ) ;
#40751 = LINE ( 'NONE', #51721, #67064 ) ;
#40752 = CARTESIAN_POINT ( 'NONE',  ( -7.250000000000000888, 8.250000000000001776, -26.00000000000001066 ) ) ;
#40753 = ORIENTED_EDGE ( 'NONE', *, *, #11302, .T. ) ;
#40754 = VERTEX_POINT ( 'NONE', #7419 ) ;
#40755 = AXIS2_PLACEMENT_3D ( 'NONE', #32116, #33417, #65922 ) ;
#40757 = ORIENTED_EDGE ( 'NONE', *, *, #21740, .T. ) ;
#40756 = DIRECTION ( 'NONE',  ( -1.000000000000000000, 0.000000000000000000, 0.000000000000000000 ) ) ;
#40758 = ORIENTED_EDGE ( 'NONE', *, *, #2084, .T. ) ;
#40759 = EDGE_CURVE ( 'NONE', #1592, #35824, #66698, .T. ) ;
#40760 = AXIS2_PLACEMENT_3D ( 'NONE', #66015, #39155, #17577 ) ;
#40761 = CIRCLE ( 'NONE', #40812, 24.99999999998794920 ) ;
#40762 = CARTESIAN_POINT ( 'NONE',  ( 8.250000000000005329, 0.000000000000000000, -17.00000000000000000 ) ) ;
#40763 = CARTESIAN_POINT ( 'NONE',  ( 14.10805890929250062, -5.000000000000000000, -26.25000000000000000 ) ) ;
#40764 = CARTESIAN_POINT ( 'NONE',  ( -9.722976262117258628, 6.817976262117182884, 54.00000000000000711 ) ) ;
#40765 = LINE ( 'NONE', #62323, #26350 ) ;
#40766 = ADVANCED_FACE ( 'NONE', ( #39591 ), #43872, .F. ) ;
#40767 = AXIS2_PLACEMENT_3D ( 'NONE', #43522, #5011, #32922 ) ;
#40768 = EDGE_CURVE ( 'NONE', #42852, #45427, #2125, .T. ) ;
#40769 =( LENGTH_UNIT ( ) NAMED_UNIT ( * ) SI_UNIT ( .MILLI., .METRE. ) );
#40770 = LINE ( 'NONE', #28755, #61235 ) ;
#40771 = EDGE_LOOP ( 'NONE', ( #10915, #6012, #23279, #62950 ) ) ;
#40772 = ORIENTED_EDGE ( 'NONE', *, *, #13187, .T. ) ;
#40773 = EDGE_CURVE ( 'NONE', #56509, #42896, #17007, .T. ) ;
#40774 = ORIENTED_EDGE ( 'NONE', *, *, #65634, .F. ) ;
#40775 = AXIS2_PLACEMENT_3D ( 'NONE', #17440, #60230, #11784 ) ;
#40776 = AXIS2_PLACEMENT_3D ( 'NONE', #3039, #41559, #30953 ) ;
#40777 = ORIENTED_EDGE ( 'NONE', *, *, #21730, .T. ) ;
#40778 = CARTESIAN_POINT ( 'NONE',  ( 11.50000000000000000, -11.70000000000000284, 11.00000000000000000 ) ) ;
#40779 = CARTESIAN_POINT ( 'NONE',  ( 8.406483450353379183, -7.616533956692230767, 195.0000000000000284 ) ) ;
#40780 = VECTOR ( 'NONE', #25646, 1000.000000000000000 ) ;
#40781 = CYLINDRICAL_SURFACE ( 'NONE', #35361, 0.5250000000000001332 ) ;
#40782 = AXIS2_PLACEMENT_3D ( 'NONE', #29310, #13754, #56884 ) ;
#40783 = ORIENTED_EDGE ( 'NONE', *, *, #65005, .F. ) ;
#40784 = ORIENTED_EDGE ( 'NONE', *, *, #14919, .F. ) ;
#40785 = ORIENTED_EDGE ( 'NONE', *, *, #11468, .F. ) ;
#40787 = DIRECTION ( 'NONE',  ( -1.000000000000000000, 0.000000000000000000, 0.000000000000000000 ) ) ;
#40786 = CIRCLE ( 'NONE', #62228, 0.3500000000009988455 ) ;
#40788 = VERTEX_POINT ( 'NONE', #8111 ) ;
#40789 = ORIENTED_EDGE ( 'NONE', *, *, #65008, .T. ) ;
#40790 = DIRECTION ( 'NONE',  ( 1.000000000000000000, -7.304098846218132892E-15, 0.000000000000000000 ) ) ;
#40791 = ORIENTED_EDGE ( 'NONE', *, *, #65651, .F. ) ;
#40792 = ORIENTED_EDGE ( 'NONE', *, *, #33163, .T. ) ;
#40793 = FACE_OUTER_BOUND ( 'NONE', #26254, .T. ) ;
#40795 = ORIENTED_EDGE ( 'NONE', *, *, #24990, .F. ) ;
#40794 = DIRECTION ( 'NONE',  ( -1.000000000000000000, 0.000000000000000000, 0.000000000000000000 ) ) ;
#40796 = ORIENTED_EDGE ( 'NONE', *, *, #62648, .T. ) ;
#40797 = FACE_OUTER_BOUND ( 'NONE', #37279, .T. ) ;
#40798 = EDGE_CURVE ( 'NONE', #67879, #43669, #51617, .T. ) ;
#40799 = DIRECTION ( 'NONE',  ( 2.135044278125299371E-15, 1.000000000000000000, 0.000000000000000000 ) ) ;
#40800 = CARTESIAN_POINT ( 'NONE',  ( 75.42576880091937142, 0.000000000000000000, 289.4830310981789125 ) ) ;
#40802 = EDGE_LOOP ( 'NONE', ( #7530, #67120, #63990, #48361 ) ) ;
#40801 = CYLINDRICAL_SURFACE ( 'NONE', #1816, 1.000000000000000000 ) ;
#40803 = ORIENTED_EDGE ( 'NONE', *, *, #14178, .T. ) ;
#40804 = DIRECTION ( 'NONE',  ( -1.000000000000000000, 0.000000000000000000, 0.000000000000000000 ) ) ;
#40805 = CARTESIAN_POINT ( 'NONE',  ( -7.250000000000000888, 7.250000000000001776, -26.00000000000001066 ) ) ;
#40806 = DIRECTION ( 'NONE',  ( -1.000000000000000000, 0.000000000000000000, 0.000000000000000000 ) ) ;
#40807 = EDGE_CURVE ( 'NONE', #59980, #63544, #56564, .T. ) ;
#40808 = VECTOR ( 'NONE', #46454, 1000.000000000000000 ) ;
#40809 = ORIENTED_EDGE ( 'NONE', *, *, #12375, .T. ) ;
#40810 = DIRECTION ( 'NONE',  ( -1.000000000000000000, 0.000000000000000000, 0.000000000000000000 ) ) ;
#40811 = LINE ( 'NONE', #9339, #50160 ) ;
#40812 = AXIS2_PLACEMENT_3D ( 'NONE', #27342, #48907, #467 ) ;
#40813 = DIRECTION ( 'NONE',  ( -1.000000000000000000, 0.000000000000000000, 0.000000000000000000 ) ) ;
#40814 = EDGE_CURVE ( 'NONE', #16097, #64136, #18144, .T. ) ;
#40815 = ORIENTED_EDGE ( 'NONE', *, *, #28356, .T. ) ;
#40816 = CARTESIAN_POINT ( 'NONE',  ( 15.50000000000000000, -0.4000000000000000222, 19.00000000000000355 ) ) ;
#40817 = DIRECTION ( 'NONE',  ( 0.000000000000000000, -1.000000000000000000, -3.673940397442059868E-16 ) ) ;
#40818 = LINE ( 'NONE', #30218, #52880 ) ;
#40819 = VECTOR ( 'NONE', #16691, 1000.000000000000000 ) ;
#40820 = CLOSED_SHELL ( 'NONE', ( #20147, #5082, #2254, #26894, #49280, #24404, #5629, #250, #10513, #53869, #10261, #49319, #61990, #32204, #35622, #50916, #65673, #53575 ) ) ;
#40821 = EDGE_LOOP ( 'NONE', ( #11467, #24283, #36580, #8061, #47113, #4161, #67956 ) ) ;
#40822 = LINE ( 'NONE', #35498, #58448 ) ;
#40823 = LINE ( 'NONE', #51788, #29980 ) ;
#40824 = AXIS2_PLACEMENT_3D ( 'NONE', #17719, #44230, #39617 ) ;
#40825 = VERTEX_POINT ( 'NONE', #24392 ) ;
#40826 = CARTESIAN_POINT ( 'NONE',  ( 8.930623737882843471, 10.03972626211716168, 26.00000000000000711 ) ) ;
#40827 = LINE ( 'NONE', #25631, #63646 ) ;
#40828 = DIRECTION ( 'NONE',  ( -0.5773502691896285066, 0.5773502691896243988, -0.5773502691896243988 ) ) ;
#40829 = DIRECTION ( 'NONE',  ( 1.000000000000000000, 0.000000000000000000, 0.000000000000000000 ) ) ;
#40830 = DIRECTION ( 'NONE',  ( 1.000000000000000000, -0.000000000000000000, 0.000000000000000000 ) ) ;
#40831 = EDGE_LOOP ( 'NONE', ( #20856, #69102, #30434, #10160 ) ) ;
#40832 = DIRECTION ( 'NONE',  ( 0.5000000000000129896, 0.8660254037844311581, 0.000000000000000000 ) ) ;
#40833 = CARTESIAN_POINT ( 'NONE',  ( 7.357023737882802727, 5.538810540049955655, 54.00000000000000711 ) ) ;
#40834 = DIRECTION ( 'NONE',  ( -1.000000000000000000, 0.000000000000000000, 0.000000000000000000 ) ) ;
#40835 = DIRECTION ( 'NONE',  ( 0.000000000000000000, 1.000000000000000000, 0.000000000000000000 ) ) ;
#40836 = CARTESIAN_POINT ( 'NONE',  ( 12.90000000000000213, -14.06939075806902117, -20.80000000000000426 ) ) ;
#40837 = ORIENTED_EDGE ( 'NONE', *, *, #2713, .F. ) ;
#40839 = ORIENTED_EDGE ( 'NONE', *, *, #16029, .T. ) ;
#40838 = FACE_OUTER_BOUND ( 'NONE', #3555, .T. ) ;
#40840 = CARTESIAN_POINT ( 'NONE',  ( 12.00000000000000178, -11.18999999999999950, -5.000000000000000000 ) ) ;
#40841 = DIRECTION ( 'NONE',  ( 1.000000000000000000, -3.491481338843133355E-15, -1.836970198721036344E-16 ) ) ;
#40842 = DIRECTION ( 'NONE',  ( -0.000000000000000000, 3.673940397442059868E-16, -1.000000000000000000 ) ) ;
#40843 = ORIENTED_EDGE ( 'NONE', *, *, #56457, .F. ) ;
#40844 = EDGE_CURVE ( 'NONE', #23324, #65486, #20137, .T. ) ;
#40845 = CARTESIAN_POINT ( 'NONE',  ( -7.450000000000001954, 0.000000000000000000, -21.50000000000000000 ) ) ;
#40846 = ORIENTED_EDGE ( 'NONE', *, *, #229, .F. ) ;
#40847 = EDGE_CURVE ( 'NONE', #3246, #40441, #45958, .T. ) ;
#40848 = ORIENTED_EDGE ( 'NONE', *, *, #2626, .F. ) ;
#40849 = VERTEX_POINT ( 'NONE', #30750 ) ;
#40850 = DIRECTION ( 'NONE',  ( 1.000000000000000000, 0.000000000000000000, 0.000000000000000000 ) ) ;
#40851 = VECTOR ( 'NONE', #33588, 1000.000000000000000 ) ;
#40852 = CARTESIAN_POINT ( 'NONE',  ( 4.201500623655991085, 7.259684009079854228, 195.0000000000000284 ) ) ;
#40853 = CARTESIAN_POINT ( 'NONE',  ( 11.12648345035333186, 4.193516549646575164, 195.0000000000000284 ) ) ;
#40854 = CARTESIAN_POINT ( 'NONE',  ( 49.00000000000000000, -0.1999999999911795112, 8.826273045769999343E-12 ) ) ;
#40855 = AXIS2_PLACEMENT_3D ( 'NONE', #28618, #33583, #45569 ) ;
#40856 = ORIENTED_EDGE ( 'NONE', *, *, #45202, .T. ) ;
#40857 = ORIENTED_EDGE ( 'NONE', *, *, #17849, .F. ) ;
#40858 = CARTESIAN_POINT ( 'NONE',  ( 55.00000000000000000, 21.00000000000000000, -16.96999999999999886 ) ) ;
#40859 = CARTESIAN_POINT ( 'NONE',  ( 41.09999999999999432, 20.60000000000000142, 13.86939075806900057 ) ) ;
#40860 = ORIENTED_EDGE ( 'NONE', *, *, #34233, .T. ) ;
#40861 = ORIENTED_EDGE ( 'NONE', *, *, #12908, .T. ) ;
#40862 = AXIS2_PLACEMENT_3D ( 'NONE', #33462, #22166, #22511 ) ;
#40863 = VECTOR ( 'NONE', #64675, 1000.000000000000114 ) ;
#40864 = ORIENTED_EDGE ( 'NONE', *, *, #568, .T. ) ;
#40865 = EDGE_CURVE ( 'NONE', #41539, #50067, #19086, .T. ) ;
#40866 = DIRECTION ( 'NONE',  ( 1.000000000000000000, 0.000000000000000000, 0.000000000000000000 ) ) ;
#40868 = ORIENTED_EDGE ( 'NONE', *, *, #60765, .T. ) ;
#40867 = DIRECTION ( 'NONE',  ( 0.000000000000000000, 0.7071067811865474617, -0.7071067811865474617 ) ) ;
#40869 = AXIS2_PLACEMENT_3D ( 'NONE', #41368, #8848, #52339 ) ;
#40870 = CARTESIAN_POINT ( 'NONE',  ( 7.450000000000004619, -1.336933437520057563E-15, -12.50000000000000000 ) ) ;
#40871 = CYLINDRICAL_SURFACE ( 'NONE', #7971, 0.5000000000001374456 ) ;
#40872 = ORIENTED_EDGE ( 'NONE', *, *, #48389, .T. ) ;
#40873 = ORIENTED_EDGE ( 'NONE', *, *, #37235, .F. ) ;
#40874 = VECTOR ( 'NONE', #39927, 1000.000000000000000 ) ;
#40875 = CARTESIAN_POINT ( 'NONE',  ( 15.50000000000000000, -5.000000000000000000, -22.50000000000000000 ) ) ;
#40876 = CYLINDRICAL_SURFACE ( 'NONE', #9862, 3.499999999999038547 ) ;
#40877 = CARTESIAN_POINT ( 'NONE',  ( 0.000000000000000000, -7.449999999999998401, -11.50000000000000000 ) ) ;
#40878 = EDGE_CURVE ( 'NONE', #32932, #30081, #62552, .T. ) ;
#40879 = DIRECTION ( 'NONE',  ( 0.000000000000000000, 0.000000000000000000, 1.000000000000000000 ) ) ;
#40880 = LINE ( 'NONE', #68818, #51671 ) ;
#40881 = ADVANCED_FACE ( 'NONE', ( #41700 ), #7767, .F. ) ;
#40882 = ADVANCED_FACE ( 'NONE', ( #61875 ), #34984, .T. ) ;
#40884 = ORIENTED_EDGE ( 'NONE', *, *, #29542, .T. ) ;
#40883 = CYLINDRICAL_SURFACE ( 'NONE', #50274, 2.250000000000001776 ) ;
#40885 = ORIENTED_EDGE ( 'NONE', *, *, #5068, .F. ) ;
#40886 = LINE ( 'NONE', #14728, #46855 ) ;
#40887 = PLANE ( 'NONE',  #25656 ) ;
#40888 = CARTESIAN_POINT ( 'NONE',  ( -3.142976262117292752, -6.501044194225499062, 54.00000000000000711 ) ) ;
#40889 = ADVANCED_FACE ( 'NONE', ( #67170 ), #63274, .F. ) ;
#40890 = DIRECTION ( 'NONE',  ( 0.000000000000000000, 1.000000000000000000, 0.000000000000000000 ) ) ;
#40891 = VECTOR ( 'NONE', #21102, 1000.000000000000000 ) ;
#40892 = EDGE_CURVE ( 'NONE', #13557, #41462, #40992, .T. ) ;
#40893 = CARTESIAN_POINT ( 'NONE',  ( -6.835476262117330393, -10.50702373788278265, 26.00000000000000000 ) ) ;
#40894 = ADVANCED_FACE ( 'NONE', ( #50901 ), #52317, .F. ) ;
#40895 = ORIENTED_EDGE ( 'NONE', *, *, #9153, .F. ) ;
#40896 = DIRECTION ( 'NONE',  ( 9.912705577010386883E-15, 1.000000000000000000, 0.000000000000000000 ) ) ;
#40897 = DIRECTION ( 'NONE',  ( -6.308085367188446447E-15, -1.000000000000000000, 0.000000000000000000 ) ) ;
#40898 = EDGE_CURVE ( 'NONE', #42657, #17601, #44137, .T. ) ;
#40899 = CARTESIAN_POINT ( 'NONE',  ( 11.00000000000000000, -15.97213595500069871, -14.50000000000000000 ) ) ;
#40900 = DIRECTION ( 'NONE',  ( -0.8660254037844482555, 0.000000000000000000, -0.4999999999999831801 ) ) ;
#40901 = DIRECTION ( 'NONE',  ( 1.836970198721029934E-16, 1.836970198721010706E-16, -1.000000000000000000 ) ) ;
#40902 = VECTOR ( 'NONE', #42864, 1000.000000000000000 ) ;
#40903 = DIRECTION ( 'NONE',  ( -0.000000000000000000, -0.000000000000000000, -1.000000000000000000 ) ) ;
#40904 = VERTEX_POINT ( 'NONE', #14126 ) ;
#40905 = CARTESIAN_POINT ( 'NONE',  ( -8.250000000000001776, -7.249999999999998224, -12.00000000000000000 ) ) ;
#40906 = CYLINDRICAL_SURFACE ( 'NONE', #29339, 0.1999999999999987899 ) ;
#40907 = ORIENTED_EDGE ( 'NONE', *, *, #62101, .T. ) ;
#40908 = DIRECTION ( 'NONE',  ( 0.000000000000000000, 0.000000000000000000, 1.000000000000000000 ) ) ;
#40909 = VECTOR ( 'NONE', #65560, 1000.000000000000114 ) ;
#40910 = DIRECTION ( 'NONE',  ( -1.836970198721029934E-16, -1.836970198721010706E-16, 1.000000000000000000 ) ) ;
#40911 = CARTESIAN_POINT ( 'NONE',  ( -10.50000000000000178, -9.690000000000001279, 0.000000000000000000 ) ) ;
#40912 = LINE ( 'NONE', #42669, #56775 ) ;
#40913 = DIRECTION ( 'NONE',  ( 0.000000000000000000, 0.000000000000000000, 1.000000000000000000 ) ) ;
#40914 = ORIENTED_EDGE ( 'NONE', *, *, #67508, .T. ) ;
#40915 = LINE ( 'NONE', #62129, #5911 ) ;
#40916 = VECTOR ( 'NONE', #10080, 1000.000000000000114 ) ;
#40917 = ORIENTED_EDGE ( 'NONE', *, *, #35332, .T. ) ;
#40918 = LINE ( 'NONE', #57193, #54163 ) ;
#40919 = LINE ( 'NONE', #19010, #60489 ) ;
#40920 = ORIENTED_EDGE ( 'NONE', *, *, #27451, .F. ) ;
#40921 = CARTESIAN_POINT ( 'NONE',  ( 7.000000000000000000, -32.00000000000000000, 8.400000000000000355 ) ) ;
#40922 = AXIS2_PLACEMENT_3D ( 'NONE', #49781, #12621, #66725 ) ;
#40923 = VECTOR ( 'NONE', #19517, 1000.000000000000000 ) ;
#40924 = ORIENTED_EDGE ( 'NONE', *, *, #53426, .F. ) ;
#40925 = CARTESIAN_POINT ( 'NONE',  ( 30.00000000000000000, -5.599999999999999645, -9.400000000000000355 ) ) ;
#40926 = VERTEX_POINT ( 'NONE', #19771 ) ;
#40927 = VECTOR ( 'NONE', #34623, 1000.000000000000000 ) ;
#40928 = EDGE_LOOP ( 'NONE', ( #54294, #40864, #40507, #11042 ) ) ;
#40929 = FACE_OUTER_BOUND ( 'NONE', #25815, .T. ) ;
#40930 = ORIENTED_EDGE ( 'NONE', *, *, #62735, .T. ) ;
#40931 = ORIENTED_EDGE ( 'NONE', *, *, #54459, .F. ) ;
#40932 = CARTESIAN_POINT ( 'NONE',  ( -7.450000000000001954, -7.249999999999998224, -8.000000000000000000 ) ) ;
#40933 = LINE ( 'NONE', #56167, #44848 ) ;
#40934 = FACE_OUTER_BOUND ( 'NONE', #17828, .T. ) ;
#40935 = AXIS2_PLACEMENT_3D ( 'NONE', #61919, #24796, #67585 ) ;
#40936 = EDGE_LOOP ( 'NONE', ( #20061, #23786, #22644, #2340 ) ) ;
#40937 = CARTESIAN_POINT ( 'NONE',  ( 73.57321854994619059, 47.95351654967443977, 20.00000000000000000 ) ) ;
#40939 = PLANE ( 'NONE',  #14121 ) ;
#40938 = LINE ( 'NONE', #31412, #4516 ) ;
#40940 = EDGE_CURVE ( 'NONE', #46798, #7898, #62922, .T. ) ;
#40941 = ORIENTED_EDGE ( 'NONE', *, *, #9495, .T. ) ;
#40943 = ORIENTED_EDGE ( 'NONE', *, *, #54644, .F. ) ;
#40942 = CARTESIAN_POINT ( 'NONE',  ( 0.5000000000000000000, -42.50000000000000000, -27.00000000000000000 ) ) ;
#40944 = AXIS2_PLACEMENT_3D ( 'NONE', #59962, #16491, #11509 ) ;
#40945 = EDGE_LOOP ( 'NONE', ( #8836, #3306, #11959, #457 ) ) ;
#40946 = PRODUCT_CONTEXT ( 'NONE', #30935, 'mechanical' ) ;
#40947 = EDGE_CURVE ( 'NONE', #60252, #32685, #24030, .T. ) ;
#40948 = CARTESIAN_POINT ( 'NONE',  ( 8.144523737882815695, 9.547976262117185087, 54.00000000000000711 ) ) ;
#40949 = AXIS2_PLACEMENT_3D ( 'NONE', #35947, #20035, #57505 ) ;
#40951 = ORIENTED_EDGE ( 'NONE', *, *, #8750, .F. ) ;
#40950 = DIRECTION ( 'NONE',  ( -0.000000000000000000, 0.000000000000000000, 1.000000000000000000 ) ) ;
#40952 = DIRECTION ( 'NONE',  ( -1.000000000000000000, 0.000000000000000000, 0.000000000000000000 ) ) ;
#40953 = CARTESIAN_POINT ( 'NONE',  ( -7.250000000000001776, -7.249999999999998224, -22.50000000000000000 ) ) ;
#40954 = ORIENTED_EDGE ( 'NONE', *, *, #25673, .F. ) ;
#40955 = ADVANCED_FACE ( 'NONE', ( #3881 ), #25445, .T. ) ;
#40956 = VERTEX_POINT ( 'NONE', #69277 ) ;
#40957 = FACE_OUTER_BOUND ( 'NONE', #48279, .T. ) ;
#40958 = EDGE_CURVE ( 'NONE', #68720, #25525, #20484, .T. ) ;
#40959 = ORIENTED_EDGE ( 'NONE', *, *, #64785, .T. ) ;
#40960 = CARTESIAN_POINT ( 'NONE',  ( -7.955476262117320729, -9.562023737882766383, 26.00000000000000000 ) ) ;
#40961 = DIRECTION ( 'NONE',  ( 1.836970198721029934E-16, -1.836970198721036344E-16, 1.000000000000000000 ) ) ;
#40962 = FACE_OUTER_BOUND ( 'NONE', #51939, .T. ) ;
#40963 = ORIENTED_EDGE ( 'NONE', *, *, #23273, .T. ) ;
#40964 = CIRCLE ( 'NONE', #50005, 4.000000000000000888 ) ;
#40965 = CARTESIAN_POINT ( 'NONE',  ( 11.12648345035333364, 4.193516549646575164, 195.0000000000000284 ) ) ;
#40966 = ADVANCED_FACE ( 'NONE', ( #15553 ), #26492, .F. ) ;
#40967 = LINE ( 'NONE', #66788, #56263 ) ;
#40969 = VERTEX_POINT ( 'NONE', #59363 ) ;
#40968 = CARTESIAN_POINT ( 'NONE',  ( 3.857023737882817827, 10.30047626211720413, 54.00000000000000711 ) ) ;
#40971 = VERTEX_POINT ( 'NONE', #26152 ) ;
#40970 = DIRECTION ( 'NONE',  ( 0.000000000000000000, -3.673940397442059868E-16, 1.000000000000000000 ) ) ;
#40973 = CARTESIAN_POINT ( 'NONE',  ( 24.00000000000000000, -17.35230188589299871, -15.35019951917099945 ) ) ;
#40972 = VECTOR ( 'NONE', #40113, 1000.000000000000000 ) ;
#40974 = LINE ( 'NONE', #19409, #14930 ) ;
#40975 = LINE ( 'NONE', #8093, #39216 ) ;
#40976 = CARTESIAN_POINT ( 'NONE',  ( 10.31452373788278187, 3.842976262117144159, 54.00000000000000711 ) ) ;
#40977 = DIRECTION ( 'NONE',  ( 1.203165845134433242E-14, 1.000000000000000000, 0.000000000000000000 ) ) ;
#40978 = EDGE_CURVE ( 'NONE', #43112, #6826, #48755, .T. ) ;
#40979 = ORIENTED_EDGE ( 'NONE', *, *, #4007, .F. ) ;
#40980 = DIRECTION ( 'NONE',  ( 4.336808689942006692E-15, 1.000000000000000000, 0.000000000000000000 ) ) ;
#40981 = DIRECTION ( 'NONE',  ( -1.000000000000000000, 0.000000000000000000, 0.000000000000000000 ) ) ;
#40983 = EDGE_CURVE ( 'NONE', #68953, #61998, #9893, .T. ) ;
#40982 = CARTESIAN_POINT ( 'NONE',  ( -9.897976262117250457, -3.857023737882721903, 54.00000000000000711 ) ) ;
#40985 = EDGE_LOOP ( 'NONE', ( #12411, #63494, #58607, #4016, #15380, #6969, #7519, #36744 ) ) ;
#40984 = CARTESIAN_POINT ( 'NONE',  ( 11.75000000000000000, -5.000000000000000000, -11.75000000000000000 ) ) ;
#40986 = DIRECTION ( 'NONE',  ( 0.6785983445458467767, -0.6785983445458462215, 0.2810846377148228381 ) ) ;
#40987 = VECTOR ( 'NONE', #22290, 1000.000000000000000 ) ;
#40988 = DIRECTION ( 'NONE',  ( -0.000000000000000000, -0.000000000000000000, -1.000000000000000000 ) ) ;
#40989 = VERTEX_POINT ( 'NONE', #32143 ) ;
#40990 = VERTEX_POINT ( 'NONE', #20830 ) ;
#40991 = CARTESIAN_POINT ( 'NONE',  ( -3.663616288757055806, 4.135079735113128763, 26.00000000000000711 ) ) ;
#40992 = LINE ( 'NONE', #46301, #35097 ) ;
#40993 = CIRCLE ( 'NONE', #15020, 0.5999999999999998668 ) ;
#40994 = ORIENTED_EDGE ( 'NONE', *, *, #63292, .T. ) ;
#40995 = FACE_OUTER_BOUND ( 'NONE', #49060, .T. ) ;
#40996 = CARTESIAN_POINT ( 'NONE',  ( 7.000000000000000000, -42.00000000000000000, 15.00000000000000000 ) ) ;
#40997 = VECTOR ( 'NONE', #42357, 1000.000000000000000 ) ;
#40998 = DIRECTION ( 'NONE',  ( 0.000000000000000000, 1.000000000000000000, 0.000000000000000000 ) ) ;
#40999 = DIRECTION ( 'NONE',  ( 0.000000000000000000, 0.000000000000000000, -1.000000000000000000 ) ) ;
#41000 = VERTEX_POINT ( 'NONE', #37800 ) ;
#41001 = DIRECTION ( 'NONE',  ( 1.000000000000000000, -0.000000000000000000, -0.000000000000000000 ) ) ;
#41002 = VERTEX_POINT ( 'NONE', #48410 ) ;
#41003 = ORIENTED_EDGE ( 'NONE', *, *, #40569, .T. ) ;
#41004 = VERTEX_POINT ( 'NONE', #53377 ) ;
#41005 = VECTOR ( 'NONE', #16628, 1000.000000000000000 ) ;
#41006 = CARTESIAN_POINT ( 'NONE',  ( -6.835476262117334834, -10.50702373788278798, 54.00000000000000711 ) ) ;
#41007 = EDGE_CURVE ( 'NONE', #10955, #48587, #42403, .T. ) ;
#41008 = CARTESIAN_POINT ( 'NONE',  ( -3.142976262117292308, -6.501044194225499062, 54.00000000000000711 ) ) ;
#41009 = LINE ( 'NONE', #30414, #29849 ) ;
#41010 = ORIENTED_EDGE ( 'NONE', *, *, #69463, .F. ) ;
#41011 = ORIENTED_EDGE ( 'NONE', *, *, #32813, .F. ) ;
#41012 = CARTESIAN_POINT ( 'NONE',  ( 181.4833316329832940, 5.000000000000000000, 284.4801873289890182 ) ) ;
#41013 = VERTEX_POINT ( 'NONE', #316 ) ;
#41014 = EDGE_CURVE ( 'NONE', #46952, #16502, #3524, .T. ) ;
#41015 = ORIENTED_EDGE ( 'NONE', *, *, #22810, .F. ) ;
#41016 = LINE ( 'NONE', #68613, #14623 ) ;
#41017 = DIRECTION ( 'NONE',  ( 1.000000000000000000, 0.000000000000000000, 0.000000000000000000 ) ) ;
#41018 = VECTOR ( 'NONE', #24423, 1000.000000000000000 ) ;
#41019 = CARTESIAN_POINT ( 'NONE',  ( 32.89999999999999858, 13.66939075806899240, 20.79999999999999361 ) ) ;
#41020 = PLANE ( 'NONE',  #38794 ) ;
#41021 = EDGE_LOOP ( 'NONE', ( #60146, #42962, #26386, #40462 ) ) ;
#41022 = ADVANCED_FACE ( 'NONE', ( #48059 ), #69639, .F. ) ;
#41023 = VECTOR ( 'NONE', #26321, 1000.000000000000114 ) ;
#41024 = DIRECTION ( 'NONE',  ( 0.000000000000000000, -0.6874999999999994449, 0.7261843774138911911 ) ) ;
#41026 = CARTESIAN_POINT ( 'NONE',  ( 275.0000000000000000, -38.09999999999885034, -7.900000000002049383 ) ) ;
#41025 = CARTESIAN_POINT ( 'NONE',  ( 283.0000000000000568, -23.29603921945599865, 12.50000000000000000 ) ) ;
#41027 = CIRCLE ( 'NONE', #22957, 0.2000000000000000944 ) ;
#41029 = ORIENTED_EDGE ( 'NONE', *, *, #7372, .F. ) ;
#41028 = AXIS2_PLACEMENT_3D ( 'NONE', #2948, #2252, #8945 ) ;
#41030 = EDGE_CURVE ( 'NONE', #28340, #13228, #36278, .T. ) ;
#41032 = ORIENTED_EDGE ( 'NONE', *, *, #29508, .F. ) ;
#41031 = CARTESIAN_POINT ( 'NONE',  ( -7.250000000000001776, -7.249999999999998224, -25.50000000000000355 ) ) ;
#41033 = VERTEX_POINT ( 'NONE', #64328 ) ;
#41034 = ORIENTED_EDGE ( 'NONE', *, *, #50073, .F. ) ;
#41035 = AXIS2_PLACEMENT_3D ( 'NONE', #38135, #49070, #21849 ) ;
#41036 = CIRCLE ( 'NONE', #30850, 0.5249999999999994671 ) ;
#41037 = EDGE_CURVE ( 'NONE', #49494, #58107, #23850, .T. ) ;
#41038 = FACE_OUTER_BOUND ( 'NONE', #57433, .T. ) ;
#41039 = FACE_OUTER_BOUND ( 'NONE', #57564, .T. ) ;
#41040 = EDGE_LOOP ( 'NONE', ( #6079, #63881, #39195, #4099 ) ) ;
#41041 = ORIENTED_EDGE ( 'NONE', *, *, #10796, .T. ) ;
#41042 = EDGE_CURVE ( 'NONE', #47075, #54499, #59014, .T. ) ;
#41043 = EDGE_CURVE ( 'NONE', #1462, #50319, #31110, .T. ) ;
#41044 = CARTESIAN_POINT ( 'NONE',  ( 283.0000000000000568, -30.45000000000094786, -15.00000000000000000 ) ) ;
#41045 = DIRECTION ( 'NONE',  ( 0.000000000000000000, -1.000000000000000000, 0.000000000000000000 ) ) ;
#41046 = EDGE_LOOP ( 'NONE', ( #37405, #31943, #37271, #69413 ) ) ;
#41047 = ADVANCED_FACE ( 'NONE', ( #26851 ), #69974, .T. ) ;
#41048 = ADVANCED_FACE ( 'NONE', ( #21876 ), #43433, .F. ) ;
#41049 = VERTEX_POINT ( 'NONE', #52683 ) ;
#41050 = FACE_BOUND ( 'NONE', #68784, .T. ) ;
#41051 = DIRECTION ( 'NONE',  ( 0.000000000000000000, 1.000000000000000000, 0.000000000000000000 ) ) ;
#41052 = ORIENTED_EDGE ( 'NONE', *, *, #46963, .F. ) ;
#41053 = ADVANCED_FACE ( 'NONE', ( #4241 ), #25806, .T. ) ;
#41054 = DIRECTION ( 'NONE',  ( 0.000000000000000000, 1.000000000000000000, 0.000000000000000000 ) ) ;
#41055 = CARTESIAN_POINT ( 'NONE',  ( -17.00000000000000000, -15.50000000000000000, -2.000000000000000000 ) ) ;
#41057 = VERTEX_POINT ( 'NONE', #58334 ) ;
#41056 = DIRECTION ( 'NONE',  ( 1.000000000000000000, 2.135044278125301343E-15, 0.000000000000000000 ) ) ;
#41058 = VERTEX_POINT ( 'NONE', #27879 ) ;
#41059 = FACE_OUTER_BOUND ( 'NONE', #41280, .T. ) ;
#41060 = DIRECTION ( 'NONE',  ( 0.000000000000000000, 0.7071067811865074937, 0.7071067811865876518 ) ) ;
#41061 = CARTESIAN_POINT ( 'NONE',  ( -8.916576262117260399, 8.566576262117216345, 54.00000000000000711 ) ) ;
#41062 = CARTESIAN_POINT ( 'NONE',  ( 16.75000000000000000, -0.2038245569916320166, -23.22168783648699986 ) ) ;
#41063 = DIRECTION ( 'NONE',  ( 1.000000000000000000, -0.000000000000000000, -0.000000000000000000 ) ) ;
#41064 = DIRECTION ( 'NONE',  ( 0.000000000000000000, -0.7084617869623469621, -0.7057491738671168857 ) ) ;
#41065 = EDGE_CURVE ( 'NONE', #60260, #4452, #55443, .T. ) ;
#41066 = ORIENTED_EDGE ( 'NONE', *, *, #64158, .F. ) ;
#41067 = LINE ( 'NONE', #46373, #56364 ) ;
#41070 = VERTEX_POINT ( 'NONE', #11594 ) ;
#41069 = EDGE_CURVE ( 'NONE', #7103, #58695, #6311, .T. ) ;
#41068 = LINE ( 'NONE', #69346, #20963 ) ;
#41071 = FACE_OUTER_BOUND ( 'NONE', #38614, .T. ) ;
#41072 = CIRCLE ( 'NONE', #33143, 0.9999999999999991118 ) ;
#41073 = AXIS2_PLACEMENT_3D ( 'NONE', #3382, #47566, #30602 ) ;
#41074 = DIRECTION ( 'NONE',  ( 0.000000000000000000, 0.000000000000000000, 1.000000000000000000 ) ) ;
#41075 = LINE ( 'NONE', #8195, #69054 ) ;
#41076 = VECTOR ( 'NONE', #18132, 1000.000000000000000 ) ;
#41077 = DIRECTION ( 'NONE',  ( 0.000000000000000000, 1.000000000000000000, 3.673940397442059868E-16 ) ) ;
#41078 = VERTEX_POINT ( 'NONE', #39508 ) ;
#41079 = CARTESIAN_POINT ( 'NONE',  ( 29.89999999999999858, 20.60000000000000142, -13.86939075806900057 ) ) ;
#41080 = CARTESIAN_POINT ( 'NONE',  ( 10.74648345035335240, 1.677516549646529409, 455.0000000000000568 ) ) ;
#41081 = ORIENTED_EDGE ( 'NONE', *, *, #5087, .T. ) ;
#41082 = VECTOR ( 'NONE', #1452, 1000.000000000000000 ) ;
#41083 = CYLINDRICAL_SURFACE ( 'NONE', #42627, 24.99999999998794920 ) ;
#41084 = VECTOR ( 'NONE', #69774, 1000.000000000000000 ) ;
#41085 = CYLINDRICAL_SURFACE ( 'NONE', #12694, 0.5999999999999998668 ) ;
#41086 = EDGE_LOOP ( 'NONE', ( #45701, #56393, #10375, #49677, #43879, #23972 ) ) ;
#41087 = LINE ( 'NONE', #57358, #4509 ) ;
#41088 = ORIENTED_EDGE ( 'NONE', *, *, #7653, .T. ) ;
#41089 = ORIENTED_EDGE ( 'NONE', *, *, #33839, .F. ) ;
#41090 = AXIS2_PLACEMENT_3D ( 'NONE', #9654, #31576, #30508 ) ;
#41091 = CARTESIAN_POINT ( 'NONE',  ( 275.0000000000000000, -20.50000000000000000, 13.00000000000000178 ) ) ;
#41092 = DIRECTION ( 'NONE',  ( -0.8660254037850496633, 0.000000000000000000, 0.4999999999989417909 ) ) ;
#41093 = DIRECTION ( 'NONE',  ( 0.000000000000000000, -0.000000000000000000, 1.000000000000000000 ) ) ;
#41094 = CARTESIAN_POINT ( 'NONE',  ( 25.50000000000000355, 0.000000000000000000, 22.50000000000000000 ) ) ;
#41095 = PLANE ( 'NONE',  #57732 ) ;
#41096 = ORIENTED_EDGE ( 'NONE', *, *, #7980, .F. ) ;
#41097 = ORIENTED_EDGE ( 'NONE', *, *, #34868, .F. ) ;
#41099 = EDGE_LOOP ( 'NONE', ( #58356, #27018, #63597, #39313 ) ) ;
#41098 = DIRECTION ( 'NONE',  ( 0.000000000000000000, 0.000000000000000000, -1.000000000000000000 ) ) ;
#41100 = ORIENTED_EDGE ( 'NONE', *, *, #2539, .T. ) ;
#41101 = ADVANCED_FACE ( 'NONE', ( #5965 ), #22575, .T. ) ;
#41102 = DIRECTION ( 'NONE',  ( -1.000000000000000000, 0.000000000000000000, 0.000000000000000000 ) ) ;
#41103 = CARTESIAN_POINT ( 'NONE',  ( 16.75000000000000000, -2.500000000000000000, 21.77831216351300014 ) ) ;
#41104 = DIRECTION ( 'NONE',  ( 0.000000000000000000, -0.1111111111108840643, -0.9938079899999319178 ) ) ;
#41105 = CARTESIAN_POINT ( 'NONE',  ( 11.78648345035337819, -4.186483450353396307, 195.0000000000000284 ) ) ;
#41106 = VECTOR ( 'NONE', #19959, 1000.000000000000000 ) ;
#41107 = EDGE_CURVE ( 'NONE', #15205, #30525, #61069, .T. ) ;
#41108 = DIRECTION ( 'NONE',  ( 0.000000000000000000, 1.000000000000000000, 0.000000000000000000 ) ) ;
#41109 = CARTESIAN_POINT ( 'NONE',  ( 3.157023737882809655, -6.501044194225470640, 26.00000000000000711 ) ) ;
#41110 = ADVANCED_FACE ( 'NONE', ( #17942 ), #16922, .F. ) ;
#41111 = EDGE_LOOP ( 'NONE', ( #16613, #33136, #26689, #15010 ) ) ;
#41112 = VECTOR ( 'NONE', #21536, 1000.000000000000000 ) ;
#41113 = ORIENTED_EDGE ( 'NONE', *, *, #44079, .T. ) ;
#41114 = EDGE_CURVE ( 'NONE', #33288, #19106, #54751, .T. ) ;
#41115 = ORIENTED_EDGE ( 'NONE', *, *, #4428, .F. ) ;
#41116 = ORIENTED_EDGE ( 'NONE', *, *, #37663, .F. ) ;
#41117 = LINE ( 'NONE', #7182, #61507 ) ;
#41118 = ADVANCED_FACE ( 'NONE', ( #1679 ), #55104, .T. ) ;
#41119 = EDGE_CURVE ( 'NONE', #54442, #10200, #51928, .T. ) ;
#41120 = LINE ( 'NONE', #19205, #41123 ) ;
#41121 =( NAMED_UNIT ( * ) PLANE_ANGLE_UNIT ( ) SI_UNIT ( $, .RADIAN. ) );
#41122 = CIRCLE ( 'NONE', #56908, 0.2000000000005261458 ) ;
#41124 = DIRECTION ( 'NONE',  ( 0.000000000000000000, 0.000000000000000000, 1.000000000000000000 ) ) ;
#41123 = VECTOR ( 'NONE', #69048, 1000.000000000000000 ) ;
#41125 = ORIENTED_EDGE ( 'NONE', *, *, #15323, .T. ) ;
#41126 = VERTEX_POINT ( 'NONE', #33176 ) ;
#41127 = ORIENTED_EDGE ( 'NONE', *, *, #1580, .T. ) ;
#41128 = DIRECTION ( 'NONE',  ( 1.000000000000000000, -8.359604446858500663E-15, 0.000000000000000000 ) ) ;
#41129 = ORIENTED_EDGE ( 'NONE', *, *, #21968, .T. ) ;
#41130 = AXIS2_PLACEMENT_3D ( 'NONE', #4680, #26248, #41801 ) ;
#41131 = ORIENTED_EDGE ( 'NONE', *, *, #45672, .T. ) ;
#41132 = CARTESIAN_POINT ( 'NONE',  ( -14.25000000000000000, -2.500000000000000000, -21.77831216351300014 ) ) ;
#41133 = ORIENTED_EDGE ( 'NONE', *, *, #7980, .T. ) ;
#41134 = VERTEX_POINT ( 'NONE', #28217 ) ;
#41135 = DIRECTION ( 'NONE',  ( 1.000000000000000000, 0.000000000000000000, 0.000000000000000000 ) ) ;
#41136 = AXIS2_PLACEMENT_3D ( 'NONE', #66761, #7358, #2068 ) ;
#41138 = VERTEX_POINT ( 'NONE', #38158 ) ;
#41137 = FACE_OUTER_BOUND ( 'NONE', #60118, .T. ) ;
#41139 = ORIENTED_EDGE ( 'NONE', *, *, #29444, .F. ) ;
#41140 = CARTESIAN_POINT ( 'NONE',  ( 11.78648345035337819, -7.606483450353398013, 195.0000000000000284 ) ) ;
#41141 = CARTESIAN_POINT ( 'NONE',  ( -15.50000000000000000, -1.037157890325000054, 22.50000000000000000 ) ) ;
#41142 = LINE ( 'NONE', #36540, #58462 ) ;
#41144 = ORIENTED_EDGE ( 'NONE', *, *, #49073, .F. ) ;
#41143 = LINE ( 'NONE', #4727, #8634 ) ;
#41145 = AXIS2_PLACEMENT_3D ( 'NONE', #33299, #64789, #27309 ) ;
#41146 = ORIENTED_EDGE ( 'NONE', *, *, #26376, .T. ) ;
#41147 = CARTESIAN_POINT ( 'NONE',  ( -9.689726262117318356, -8.930623737882756430, 54.00000000000000711 ) ) ;
#41148 = CARTESIAN_POINT ( 'NONE',  ( 11.50000000000000000, -11.50000000000100009, -15.00000000000084910 ) ) ;
#41149 = PLANE ( 'NONE',  #26709 ) ;
#41150 = LINE ( 'NONE', #8629, #28166 ) ;
#41151 = ORIENTED_EDGE ( 'NONE', *, *, #29619, .T. ) ;
#41152 = CARTESIAN_POINT ( 'NONE',  ( 2.632023737882801306, 6.486996718459885791, 26.00000000000000711 ) ) ;
#41153 = EDGE_CURVE ( 'NONE', #48512, #47820, #22236, .T. ) ;
#41154 = FACE_OUTER_BOUND ( 'NONE', #52985, .T. ) ;
#41155 = LINE ( 'NONE', #63792, #63941 ) ;
#41156 = ORIENTED_EDGE ( 'NONE', *, *, #27735, .F. ) ;
#41157 = CIRCLE ( 'NONE', #45689, 0.2000000000000005107 ) ;
#41158 = EDGE_CURVE ( 'NONE', #32818, #53583, #1018, .T. ) ;
#41159 = PLANE ( 'NONE',  #58419 ) ;
#41160 = LINE ( 'NONE', #8985, #44159 ) ;
#41161 = DIRECTION ( 'NONE',  ( 1.047444401652940007E-14, 1.000000000000000000, 1.836970198721029934E-16 ) ) ;
#41162 = CIRCLE ( 'NONE', #11828, 0.3499999999999285905 ) ;
#41163 = ORIENTED_EDGE ( 'NONE', *, *, #47759, .F. ) ;
#41164 = FACE_OUTER_BOUND ( 'NONE', #44629, .T. ) ;
#41165 = CARTESIAN_POINT ( 'NONE',  ( -13.00000000000000178, -15.50000000000000000, 20.05051025721700242 ) ) ;
#41166 = AXIS2_PLACEMENT_3D ( 'NONE', #41883, #68058, #14664 ) ;
#41167 = VECTOR ( 'NONE', #69761, 1000.000000000000000 ) ;
#41168 = DIRECTION ( 'NONE',  ( 1.000000000000000000, -0.000000000000000000, 0.000000000000000000 ) ) ;
#41169 = VERTEX_POINT ( 'NONE', #54413 ) ;
#41170 = CARTESIAN_POINT ( 'NONE',  ( 4.456444791733522252E-16, 7.450000000000002842, -7.500000000000000000 ) ) ;
#41171 = DIRECTION ( 'NONE',  ( 0.000000000000000000, -0.7096009616570518874, -0.7046037717862339012 ) ) ;
#41172 = CYLINDRICAL_SURFACE ( 'NONE', #62414, 0.5000000000000000000 ) ;
#41173 = DIRECTION ( 'NONE',  ( 0.000000000000000000, 1.000000000000000000, 3.673940397442059868E-16 ) ) ;
#41174 = CARTESIAN_POINT ( 'NONE',  ( 5.552858015815581361, -7.357023737882814274, 26.00000000000000000 ) ) ;
#41175 = VECTOR ( 'NONE', #48079, 1000.000000000000000 ) ;
#41176 = ORIENTED_EDGE ( 'NONE', *, *, #11672, .F. ) ;
#41177 = PLANE ( 'NONE',  #35501 ) ;
#41178 = DIRECTION ( 'NONE',  ( -1.836970198721029934E-16, 1.836970198721036344E-16, -1.000000000000000000 ) ) ;
#41179 = CARTESIAN_POINT ( 'NONE',  ( 275.4999999999998863, 2.842170943040400743E-14, -26.49999999999993250 ) ) ;
#41180 = AXIS2_PLACEMENT_3D ( 'NONE', #14778, #30694, #52619 ) ;
#41181 = DIRECTION ( 'NONE',  ( 0.4999999999999827360, 0.000000000000000000, -0.8660254037844485886 ) ) ;
#41182 = CARTESIAN_POINT ( 'NONE',  ( -9.722976262117258628, 6.817976262117182884, 54.00000000000000711 ) ) ;
#41183 = ORIENTED_EDGE ( 'NONE', *, *, #21588, .F. ) ;
#41185 = VERTEX_POINT ( 'NONE', #7325 ) ;
#41184 = CARTESIAN_POINT ( 'NONE',  ( -7.450000000000001954, 7.250000000000000000, -19.50000000000000000 ) ) ;
#41186 = ADVANCED_FACE ( 'NONE', ( #66033 ), #50478, .F. ) ;
#41187 = CIRCLE ( 'NONE', #67176, 0.1999999999999996503 ) ;
#41188 = LINE ( 'NONE', #62760, #23688 ) ;
#41189 = CARTESIAN_POINT ( 'NONE',  ( -11.11351654964671098, 7.793516549646603231, 195.0000000000000284 ) ) ;
#41190 = CARTESIAN_POINT ( 'NONE',  ( 4.747751991980608821, 6.606374702650090747, 195.0000000000000284 ) ) ;
#41191 = VERTEX_POINT ( 'NONE', #23593 ) ;
#41192 = CARTESIAN_POINT ( 'NONE',  ( 31.89999999999999858, -14.06939075806902117, -20.80000000000000426 ) ) ;
#41193 = EDGE_CURVE ( 'NONE', #39751, #57629, #43794, .T. ) ;
#41194 = VERTEX_POINT ( 'NONE', #59708 ) ;
#41195 = EDGE_CURVE ( 'NONE', #22707, #66744, #65704, .T. ) ;
#41196 = EDGE_LOOP ( 'NONE', ( #47839, #60408, #15495, #49195 ) ) ;
#41197 = VERTEX_POINT ( 'NONE', #17603 ) ;
#41198 = DIRECTION ( 'NONE',  ( 0.000000000000000000, 0.000000000000000000, -1.000000000000000000 ) ) ;
#41199 = EDGE_CURVE ( 'NONE', #56386, #56861, #7888, .T. ) ;
#41200 = EDGE_CURVE ( 'NONE', #46851, #33133, #33859, .T. ) ;
#41201 = CARTESIAN_POINT ( 'NONE',  ( 7.000000000000000000, -29.94999999999999929, -14.50000000000000000 ) ) ;
#41202 = LINE ( 'NONE', #4449, #46154 ) ;
#41203 = DIRECTION ( 'NONE',  ( 0.000000000000000000, 0.000000000000000000, -1.000000000000000000 ) ) ;
#41204 = EDGE_CURVE ( 'NONE', #67199, #7820, #16953, .T. ) ;
#41205 = VERTEX_POINT ( 'NONE', #62119 ) ;
#41206 = ORIENTED_EDGE ( 'NONE', *, *, #8794, .F. ) ;
#41207 = CARTESIAN_POINT ( 'NONE',  ( 9.795823737882805915, -10.50702373788281463, 26.00000000000000000 ) ) ;
#41208 = CARTESIAN_POINT ( 'NONE',  ( 15.50000000000000000, -5.000000000000000000, 22.50000000000000000 ) ) ;
#41209 = EDGE_LOOP ( 'NONE', ( #8352, #22749, #61024, #27568 ) ) ;
#41210 = VECTOR ( 'NONE', #53907, 1000.000000000000000 ) ;
#41211 = ORIENTED_EDGE ( 'NONE', *, *, #69417, .T. ) ;
#41212 = VERTEX_POINT ( 'NONE', #46908 ) ;
#41213 = ORIENTED_EDGE ( 'NONE', *, *, #14715, .T. ) ;
#41214 = LINE ( 'NONE', #9047, #53089 ) ;
#41216 = ORIENTED_EDGE ( 'NONE', *, *, #62333, .T. ) ;
#41215 = DIRECTION ( 'NONE',  ( -0.000000000000000000, 3.673940397442059868E-16, -1.000000000000000000 ) ) ;
#41217 = CARTESIAN_POINT ( 'NONE',  ( 30.00000000000000000, -5.000000000000000000, -27.00000000000000000 ) ) ;
#41218 = AXIS2_PLACEMENT_3D ( 'NONE', #25088, #52308, #68575 ) ;
#41219 = AXIS2_PLACEMENT_3D ( 'NONE', #66434, #17984, #61112 ) ;
#41220 = FACE_OUTER_BOUND ( 'NONE', #10430, .T. ) ;
#41221 = VECTOR ( 'NONE', #40686, 1000.000000000000000 ) ;
#41222 = ORIENTED_EDGE ( 'NONE', *, *, #59598, .T. ) ;
#41223 = EDGE_LOOP ( 'NONE', ( #14359, #2174, #51246, #17878 ) ) ;
#41224 = VECTOR ( 'NONE', #36343, 1000.000000000000000 ) ;
#41225 = MECHANICAL_DESIGN_GEOMETRIC_PRESENTATION_REPRESENTATION (  '', ( #60455 ), #46880 ) ;
#41226 = CARTESIAN_POINT ( 'NONE',  ( -7.450000000000001954, 7.250000000000000000, -18.50000000000000000 ) ) ;
#41227 = AXIS2_PLACEMENT_3D ( 'NONE', #32140, #9890, #9529 ) ;
#41228 = DIRECTION ( 'NONE',  ( 0.000000000000000000, 0.7071067811865475727, -0.7071067811865475727 ) ) ;
#41229 = AXIS2_PLACEMENT_3D ( 'NONE', #39079, #22489, #1588 ) ;
#41230 = CARTESIAN_POINT ( 'NONE',  ( -30.00000000000000000, -11.70000000000000284, 12.50000000000000000 ) ) ;
#41231 = DIRECTION ( 'NONE',  ( -0.000000000000000000, -0.000000000000000000, 1.000000000000000000 ) ) ;
#41232 =( LENGTH_UNIT ( ) NAMED_UNIT ( * ) SI_UNIT ( .MILLI., .METRE. ) );
#41233 = ORIENTED_EDGE ( 'NONE', *, *, #57565, .T. ) ;
#41234 = EDGE_CURVE ( 'NONE', #54166, #42553, #40207, .T. ) ;
#41235 = COLOUR_RGB ( '', 0.08235294, 0.09019608, 0.10196078) ;
#41236 = DIRECTION ( 'NONE',  ( 0.000000000000000000, 0.000000000000000000, -1.000000000000000000 ) ) ;
#41237 = DIRECTION ( 'NONE',  ( 0.000000000000000000, 0.000000000000000000, -1.000000000000000000 ) ) ;
#41238 = EDGE_CURVE ( 'NONE', #39654, #44220, #2727, .T. ) ;
#41239 = ADVANCED_FACE ( 'NONE', ( #18998 ), #14035, .F. ) ;
#41240 = DIRECTION ( 'NONE',  ( 0.000000000000000000, 0.000000000000000000, -1.000000000000000000 ) ) ;
#41241 = CARTESIAN_POINT ( 'NONE',  ( -9.689726262117227762, 8.566576262117216345, 26.00000000000000711 ) ) ;
#41242 = EDGE_CURVE ( 'NONE', #69246, #67025, #39482, .T. ) ;
#41243 = CARTESIAN_POINT ( 'NONE',  ( -30.00000000000000000, -12.00000000000000000, -10.52786404500095863 ) ) ;
#41244 = ORIENTED_EDGE ( 'NONE', *, *, #2509, .T. ) ;
#41245 = CARTESIAN_POINT ( 'NONE',  ( 7.250000000000005329, 7.250000000000000888, -17.00000000000000000 ) ) ;
#41246 = DIRECTION ( 'NONE',  ( -1.000000000000000000, 0.000000000000000000, 0.000000000000000000 ) ) ;
#41247 = CARTESIAN_POINT ( 'NONE',  ( 14.25000000000000000, -2.500000000000000000, 23.22168783648699986 ) ) ;
#41248 = DIRECTION ( 'NONE',  ( 0.000000000000000000, 0.000000000000000000, 1.000000000000000000 ) ) ;
#41249 = FACE_OUTER_BOUND ( 'NONE', #46937, .T. ) ;
#41250 = DIRECTION ( 'NONE',  ( 0.000000000000000000, 0.7071067811865496822, 0.7071067811865454633 ) ) ;
#41251 = DIRECTION ( 'NONE',  ( -0.000000000000000000, -0.000000000000000000, -1.000000000000000000 ) ) ;
#41252 = DIRECTION ( 'NONE',  ( 0.000000000000000000, -0.9921567416492215186, 0.1249999999999996531 ) ) ;
#41253 = ORIENTED_EDGE ( 'NONE', *, *, #55797, .T. ) ;
#41254 = CARTESIAN_POINT ( 'NONE',  ( -11.47551654964682122, -10.20488345035336941, 455.0000000000000568 ) ) ;
#41255 = DIRECTION ( 'NONE',  ( 1.000000000000000000, 0.000000000000000000, 0.000000000000000000 ) ) ;
#41256 = AXIS2_PLACEMENT_3D ( 'NONE', #36141, #35083, #46400 ) ;
#41257 = ORIENTED_EDGE ( 'NONE', *, *, #47675, .T. ) ;
#41258 = DIRECTION ( 'NONE',  ( 0.000000000000000000, 1.000000000000000000, 0.000000000000000000 ) ) ;
#41259 = LINE ( 'NONE', #13692, #55953 ) ;
#41260 = LINE ( 'NONE', #47278, #2795 ) ;
#41261 = CIRCLE ( 'NONE', #34481, 5.200000000000009948 ) ;
#41262 =( LENGTH_UNIT ( ) NAMED_UNIT ( * ) SI_UNIT ( .MILLI., .METRE. ) );
#41263 = PLANE ( 'NONE',  #16966 ) ;
#41264 = ORIENTED_EDGE ( 'NONE', *, *, #2371, .T. ) ;
#41265 = DIRECTION ( 'NONE',  ( 0.000000000000000000, 1.000000000000000000, 0.000000000000000000 ) ) ;
#41266 = VECTOR ( 'NONE', #40867, 1000.000000000000114 ) ;
#41267 = AXIS2_PLACEMENT_3D ( 'NONE', #42388, #37445, #63978 ) ;
#41268 = AXIS2_PLACEMENT_3D ( 'NONE', #42009, #59669, #37070 ) ;
#41269 = ORIENTED_EDGE ( 'NONE', *, *, #23973, .F. ) ;
#41270 = CYLINDRICAL_SURFACE ( 'NONE', #65880, 4.000000000000000000 ) ;
#41271 = FACE_OUTER_BOUND ( 'NONE', #54043, .T. ) ;
#41272 = VERTEX_POINT ( 'NONE', #46557 ) ;
#41273 = CARTESIAN_POINT ( 'NONE',  ( 11.00000000000000000, -16.28999999999710369, 15.00000000000794920 ) ) ;
#41274 = COLOUR_RGB ( '', 0.31764706, 0.68627451, 0.89019608) ;
#41275 = ORIENTED_EDGE ( 'NONE', *, *, #64762, .F. ) ;
#41276 = LINE ( 'NONE', #20417, #48054 ) ;
#41277 = ORIENTED_EDGE ( 'NONE', *, *, #62587, .F. ) ;
#41278 = ORIENTED_EDGE ( 'NONE', *, *, #3274, .F. ) ;
#41279 = CARTESIAN_POINT ( 'NONE',  ( 9.900000000000000355, -18.00000000000000355, 21.00000000000000000 ) ) ;
#41280 = EDGE_LOOP ( 'NONE', ( #38717, #69565, #34871, #35632 ) ) ;
#41281 = EDGE_LOOP ( 'NONE', ( #21788, #4268, #50422, #10974 ) ) ;
#41282 = ADVANCED_FACE ( 'NONE', ( #24300 ), #19681, .T. ) ;
#41283 = CARTESIAN_POINT ( 'NONE',  ( 7.806483450353418618, 11.11351654964657421, 455.0000000000000568 ) ) ;
#41284 = CARTESIAN_POINT ( 'NONE',  ( -11.75000000000000000, -5.200000000000001066, 26.25000000000000000 ) ) ;
#41285 = VECTOR ( 'NONE', #3884, 1000.000000000000000 ) ;
#41286 = CARTESIAN_POINT ( 'NONE',  ( 7.450000000000004619, -1.336933437520057563E-15, -18.50000000000000000 ) ) ;
#41287 = EDGE_CURVE ( 'NONE', #51206, #27481, #8741, .T. ) ;
#41288 = EDGE_CURVE ( 'NONE', #245, #60080, #2384, .T. ) ;
#41289 = ORIENTED_EDGE ( 'NONE', *, *, #48558, .T. ) ;
#41290 = CARTESIAN_POINT ( 'NONE',  ( -25.50000000000000355, -5.200000000000001066, 20.49999999999999645 ) ) ;
#41292 = DIRECTION ( 'NONE',  ( 0.7071067811865550112, 0.7071067811865401342, 2.597868168706466299E-16 ) ) ;
#41291 = DIRECTION ( 'NONE',  ( 0.000000000000000000, 0.7071067811865475727, -0.7071067811865475727 ) ) ;
#41293 = ORIENTED_EDGE ( 'NONE', *, *, #34095, .T. ) ;
#41296 = EDGE_LOOP ( 'NONE', ( #1551, #62682, #7617, #66205 ) ) ;
#41295 = EDGE_CURVE ( 'NONE', #25935, #4952, #61413, .T. ) ;
#41294 = DIRECTION ( 'NONE',  ( 0.7071067811865391350, -0.7071067811865560104, 0.000000000000000000 ) ) ;
#41297 = ORIENTED_EDGE ( 'NONE', *, *, #20456, .F. ) ;
#41298 = APPLICATION_PROTOCOL_DEFINITION ( 'draft international standard', 'automotive_design', 1998, #2010 ) ;
#41299 = EDGE_CURVE ( 'NONE', #9367, #4940, #63229, .T. ) ;
#41300 = CARTESIAN_POINT ( 'NONE',  ( -11.18999999999999950, 11.25000000000000178, -4.250000000000000000 ) ) ;
#41301 = EDGE_CURVE ( 'NONE', #57771, #53541, #29240, .T. ) ;
#41303 = EDGE_LOOP ( 'NONE', ( #14553, #65799, #66021, #8207 ) ) ;
#41302 = CARTESIAN_POINT ( 'NONE',  ( -30.00000000000000000, -9.200000000000120082, 17.30000000000000071 ) ) ;
#41304 = CARTESIAN_POINT ( 'NONE',  ( -7.250000000000001776, -7.249999999999998224, -11.50000000000000000 ) ) ;
#41305 = CARTESIAN_POINT ( 'NONE',  ( 7.606483450353380249, -11.78648345035349010, 455.0000000000000568 ) ) ;
#41306 = ORIENTED_EDGE ( 'NONE', *, *, #9502, .T. ) ;
#41307 = VERTEX_POINT ( 'NONE', #62835 ) ;
#41308 = DIRECTION ( 'NONE',  ( -1.000000000000000000, 0.000000000000000000, -0.000000000000000000 ) ) ;
#41309 = VECTOR ( 'NONE', #36964, 1000.000000000000000 ) ;
#41310 = ORIENTED_EDGE ( 'NONE', *, *, #14794, .F. ) ;
#41311 = LINE ( 'NONE', #15516, #23400 ) ;
#41312 = DIRECTION ( 'NONE',  ( 1.000000000000000000, 0.000000000000000000, 0.000000000000000000 ) ) ;
#41313 = AXIS2_PLACEMENT_3D ( 'NONE', #52148, #67704, #3016 ) ;
#41314 = LINE ( 'NONE', #9500, #63327 ) ;
#41315 = ORIENTED_EDGE ( 'NONE', *, *, #2569, .F. ) ;
#41316 = AXIS2_PLACEMENT_3D ( 'NONE', #5434, #461, #38295 ) ;
#41317 = CIRCLE ( 'NONE', #9698, 0.2000000000000005107 ) ;
#41318 = VECTOR ( 'NONE', #17054, 1000.000000000000000 ) ;
#41319 = DIRECTION ( 'NONE',  ( 1.047444401652939849E-14, 1.000000000000000000, 0.000000000000000000 ) ) ;
#41320 = CARTESIAN_POINT ( 'NONE',  ( 12.00648345035333620, 4.173516549646563156, 195.0000000000000284 ) ) ;
#41321 = ORIENTED_EDGE ( 'NONE', *, *, #23235, .T. ) ;
#41323 = ORIENTED_EDGE ( 'NONE', *, *, #32686, .F. ) ;
#41322 = CARTESIAN_POINT ( 'NONE',  ( -7.250000000000000000, -7.449999999999998401, -18.50000000000000000 ) ) ;
#41324 = CARTESIAN_POINT ( 'NONE',  ( 3.606483450353397568, 4.609516549646590633, 455.0000000000000568 ) ) ;
#41325 = CIRCLE ( 'NONE', #53825, 0.1999999999999987899 ) ;
#41326 = CIRCLE ( 'NONE', #18766, 1.000000000000000000 ) ;
#41327 = VECTOR ( 'NONE', #23978, 1000.000000000000000 ) ;
#41328 = DIRECTION ( 'NONE',  ( 1.000000000000000000, 0.000000000000000000, 0.000000000000000000 ) ) ;
#41329 = LINE ( 'NONE', #46631, #30192 ) ;
#41330 = CARTESIAN_POINT ( 'NONE',  ( -17.00000000000000000, -15.50000000000000000, 19.33772233983200195 ) ) ;
#41331 = EDGE_CURVE ( 'NONE', #54026, #24533, #51880, .T. ) ;
#41332 = AXIS2_PLACEMENT_3D ( 'NONE', #47932, #69498, #15760 ) ;
#41333 = DIRECTION ( 'NONE',  ( 0.000000000000000000, 1.000000000000000000, 0.000000000000000000 ) ) ;
#41334 = VERTEX_POINT ( 'NONE', #29949 ) ;
#41335 = DIRECTION ( 'NONE',  ( 0.000000000000000000, -1.000000000000000000, 0.000000000000000000 ) ) ;
#41336 = DIRECTION ( 'NONE',  ( 0.000000000000000000, 0.000000000000000000, 1.000000000000000000 ) ) ;
#41337 = DIRECTION ( 'NONE',  ( 5.163402228214835223E-15, 1.000000000000000000, 0.000000000000000000 ) ) ;
#41339 = VERTEX_POINT ( 'NONE', #35961 ) ;
#41338 = DIRECTION ( 'NONE',  ( 1.000000000000000000, 0.000000000000000000, 0.000000000000000000 ) ) ;
#41340 = CIRCLE ( 'NONE', #18777, 5.250000000000000000 ) ;
#41341 = CARTESIAN_POINT ( 'NONE',  ( 5.668387132715918320, -8.406483450353487541, 455.0000000000000568 ) ) ;
#41342 = DIRECTION ( 'NONE',  ( 0.000000000000000000, -0.000000000000000000, 1.000000000000000000 ) ) ;
#41343 = EDGE_CURVE ( 'NONE', #51919, #4444, #13340, .T. ) ;
#41344 = VERTEX_POINT ( 'NONE', #14405 ) ;
#41345 = DIRECTION ( 'NONE',  ( 0.000000000000000000, 0.7071067811865495711, -0.7071067811865455743 ) ) ;
#41346 = DIRECTION ( 'NONE',  ( 0.000000000000000000, 0.000000000000000000, -1.000000000000000000 ) ) ;
#41347 = VERTEX_POINT ( 'NONE', #51531 ) ;
#41348 = FACE_OUTER_BOUND ( 'NONE', #56345, .T. ) ;
#41349 = CARTESIAN_POINT ( 'NONE',  ( -9.915476262117259409, 0.9414762621171833823, 54.00000000000000711 ) ) ;
#41350 = EDGE_CURVE ( 'NONE', #20840, #17214, #30625, .T. ) ;
#41351 = CARTESIAN_POINT ( 'NONE',  ( 39.00000000000000000, 21.00000000000000000, 16.96999999999999886 ) ) ;
#41352 = DIRECTION ( 'NONE',  ( 0.000000000000000000, 0.000000000000000000, 1.000000000000000000 ) ) ;
#41353 = ORIENTED_EDGE ( 'NONE', *, *, #68569, .T. ) ;
#41354 = CARTESIAN_POINT ( 'NONE',  ( 39.90000000000000568, -21.00000000000000000, -16.96999999999999886 ) ) ;
#41355 = ORIENTED_EDGE ( 'NONE', *, *, #23829, .F. ) ;
#41356 = ORIENTED_EDGE ( 'NONE', *, *, #4429, .F. ) ;
#41357 = AXIS2_PLACEMENT_3D ( 'NONE', #58500, #14304, #30557 ) ;
#41358 = ORIENTED_EDGE ( 'NONE', *, *, #40431, .F. ) ;
#41359 = CARTESIAN_POINT ( 'NONE',  ( 30.00000000000000000, -17.50000000000000000, -15.70500000000000007 ) ) ;
#41360 = AXIS2_PLACEMENT_3D ( 'NONE', #68069, #30591, #4777 ) ;
#41361 = ADVANCED_FACE ( 'NONE', ( #67785 ), #19339, .F. ) ;
#41362 = DIRECTION ( 'NONE',  ( -1.836970198721029934E-16, 1.836970198721036344E-16, -1.000000000000000000 ) ) ;
#41363 = AXIS2_PLACEMENT_3D ( 'NONE', #29670, #39579, #2457 ) ;
#41364 = CIRCLE ( 'NONE', #56054, 3.999999999999993339 ) ;
#41365 = PLANE ( 'NONE',  #42277 ) ;
#41366 = VERTEX_POINT ( 'NONE', #9091 ) ;
#41367 = ORIENTED_EDGE ( 'NONE', *, *, #38398, .T. ) ;
#41368 = CARTESIAN_POINT ( 'NONE',  ( 30.00000000000000000, -11.70000000000000284, -12.50000000000000000 ) ) ;
#41369 = ORIENTED_EDGE ( 'NONE', *, *, #68210, .F. ) ;
#41370 = ORIENTED_EDGE ( 'NONE', *, *, #45997, .T. ) ;
#41371 = VECTOR ( 'NONE', #44609, 1000.000000000000000 ) ;
#41372 = AXIS2_PLACEMENT_3D ( 'NONE', #2819, #67540, #47011 ) ;
#41373 = VECTOR ( 'NONE', #36720, 1000.000000000000000 ) ;
#41374 = CARTESIAN_POINT ( 'NONE',  ( 7.450000000000004619, -1.336933437520057563E-15, -18.00000000000000000 ) ) ;
#41375 = CARTESIAN_POINT ( 'NONE',  ( 8.930623737882818602, -8.930623737882855906, 54.00000000000000711 ) ) ;
#41376 = CARTESIAN_POINT ( 'NONE',  ( -16.75000000000000000, -0.2038245569916330158, -21.77831216351300014 ) ) ;
#41377 = ADVANCED_FACE ( 'NONE', ( #30660 ), #40906, .F. ) ;
#41378 = PLANE ( 'NONE',  #28599 ) ;
#41379 = ORIENTED_EDGE ( 'NONE', *, *, #1949, .T. ) ;
#41380 = DIRECTION ( 'NONE',  ( 0.000000000000000000, 0.000000000000000000, 1.000000000000000000 ) ) ;
#41381 = VECTOR ( 'NONE', #43597, 1000.000000000000000 ) ;
#41382 = VECTOR ( 'NONE', #51654, 999.9999999999998863 ) ;
#41383 = VECTOR ( 'NONE', #54098, 1000.000000000000000 ) ;
#41385 = FACE_OUTER_BOUND ( 'NONE', #34936, .T. ) ;
#41384 = CARTESIAN_POINT ( 'NONE',  ( -7.447976262117260049, 9.880476262117177555, 26.00000000000000711 ) ) ;
#41386 = ORIENTED_EDGE ( 'NONE', *, *, #67316, .T. ) ;
#41388 = ORIENTED_EDGE ( 'NONE', *, *, #20690, .F. ) ;
#41387 = CARTESIAN_POINT ( 'NONE',  ( 0.000000000000000000, -7.449999999999998401, -13.50000000000000178 ) ) ;
#41389 = ORIENTED_EDGE ( 'NONE', *, *, #5304, .F. ) ;
#41390 = VECTOR ( 'NONE', #28268, 1000.000000000000000 ) ;
#41391 = EDGE_CURVE ( 'NONE', #52982, #10498, #20330, .T. ) ;
#41392 = DIRECTION ( 'NONE',  ( -0.000000000000000000, 1.000000000000000000, -0.000000000000000000 ) ) ;
#41393 = EDGE_CURVE ( 'NONE', #27989, #33676, #4153, .T. ) ;
#41394 = AXIS2_PLACEMENT_3D ( 'NONE', #31180, #3948, #10635 ) ;
#41395 = DIRECTION ( 'NONE',  ( 0.000000000000000000, 1.000000000000000000, -0.000000000000000000 ) ) ;
#41396 = ORIENTED_EDGE ( 'NONE', *, *, #13351, .T. ) ;
#41397 = ORIENTED_EDGE ( 'NONE', *, *, #52161, .F. ) ;
#41398 = DIRECTION ( 'NONE',  ( -0.000000000000000000, -0.000000000000000000, 1.000000000000000000 ) ) ;
#41399 = CARTESIAN_POINT ( 'NONE',  ( 10.90000000000000036, 0.000000000000000000, 2.154935995002245639E-16 ) ) ;
#41400 = ORIENTED_EDGE ( 'NONE', *, *, #14717, .T. ) ;
#41401 = ORIENTED_EDGE ( 'NONE', *, *, #7810, .F. ) ;
#41402 = LINE ( 'NONE', #40701, #55630 ) ;
#41403 = CARTESIAN_POINT ( 'NONE',  ( 30.00000000000000000, -5.599999999999999645, 27.00000000000000000 ) ) ;
#41404 = EDGE_LOOP ( 'NONE', ( #26037, #69467, #27159, #41676, #8778, #29821, #13909, #1975 ) ) ;
#41405 = CARTESIAN_POINT ( 'NONE',  ( -9.547976262117254365, 8.130476262117182884, 54.00000000000000711 ) ) ;
#41406 = EDGE_CURVE ( 'NONE', #66056, #63673, #25998, .T. ) ;
#41407 = CARTESIAN_POINT ( 'NONE',  ( 10.92648345035340895, 9.293516549646565039, 455.0000000000000568 ) ) ;
#41408 = AXIS2_PLACEMENT_3D ( 'NONE', #7763, #39252, #29324 ) ;
#41410 = EDGE_LOOP ( 'NONE', ( #20008, #19935, #20674, #26538 ) ) ;
#41409 = FACE_OUTER_BOUND ( 'NONE', #64486, .T. ) ;
#41411 = ORIENTED_EDGE ( 'NONE', *, *, #61636, .F. ) ;
#41412 = FACE_BOUND ( 'NONE', #35289, .T. ) ;
#41413 = AXIS2_PLACEMENT_3D ( 'NONE', #40531, #40879, #51503 ) ;
#41414 = FACE_OUTER_BOUND ( 'NONE', #21554, .T. ) ;
#41415 = CARTESIAN_POINT ( 'NONE',  ( 10.31452373788278187, 3.650476262117146042, 54.00000000000000711 ) ) ;
#41416 = DIRECTION ( 'NONE',  ( 1.836970198721029934E-16, 1.836970198721010706E-16, -1.000000000000000000 ) ) ;
#41417 = ADVANCED_FACE ( 'NONE', ( #42665 ), #36664, .T. ) ;
#41418 = CARTESIAN_POINT ( 'NONE',  ( 49.00000000000000000, 20.60000000000000142, -13.86939075806900057 ) ) ;
#41419 = VECTOR ( 'NONE', #53018, 1000.000000000000000 ) ;
#41420 = AXIS2_PLACEMENT_3D ( 'NONE', #57240, #57935, #30370 ) ;
#41421 = LINE ( 'NONE', #68996, #23610 ) ;
#41422 = ORIENTED_EDGE ( 'NONE', *, *, #36829, .F. ) ;
#41423 = DIRECTION ( 'NONE',  ( 1.000000000000000000, -0.000000000000000000, 0.000000000000000000 ) ) ;
#41424 = EDGE_CURVE ( 'NONE', #17228, #21641, #53295, .T. ) ;
#41426 = VERTEX_POINT ( 'NONE', #20051 ) ;
#41425 = CARTESIAN_POINT ( 'NONE',  ( 26.90000000000000213, -21.00000000000001421, -13.86939075806900945 ) ) ;
#41427 = AXIS2_PLACEMENT_3D ( 'NONE', #24578, #67359, #8291 ) ;
#41428 = DIRECTION ( 'NONE',  ( -1.000000000000000000, 0.000000000000000000, 0.000000000000000000 ) ) ;
#41429 = FACE_BOUND ( 'NONE', #33395, .T. ) ;
#41430 = PRODUCT_DEFINITION_FORMATION_WITH_SPECIFIED_SOURCE ( 'ANY', '', #40168, .NOT_KNOWN. ) ;
#41431 = EDGE_CURVE ( 'NONE', #26279, #4186, #25722, .T. ) ;
#41432 = DIRECTION ( 'NONE',  ( -1.000000000000000000, 0.000000000000000000, 0.000000000000000000 ) ) ;
#41433 = AXIS2_PLACEMENT_3D ( 'NONE', #57334, #30813, #46716 ) ;
#41434 = AXIS2_PLACEMENT_3D ( 'NONE', #12577, #34145, #40509 ) ;
#41435 = EDGE_CURVE ( 'NONE', #23148, #16609, #44035, .T. ) ;
#41436 = ORIENTED_EDGE ( 'NONE', *, *, #23703, .T. ) ;
#41437 = DIRECTION ( 'NONE',  ( 1.000000000000000000, 0.000000000000000000, 0.000000000000000000 ) ) ;
#41438 = DIRECTION ( 'NONE',  ( -1.836970198721029934E-16, 1.836970198721036590E-16, -1.000000000000000000 ) ) ;
#41439 = ORIENTED_EDGE ( 'NONE', *, *, #8149, .T. ) ;
#41440 = CARTESIAN_POINT ( 'NONE',  ( 39.00000000000000000, 16.96999999999999886, 21.00000000000000000 ) ) ;
#41441 = VECTOR ( 'NONE', #48378, 999.9999999999998863 ) ;
#41442 = EDGE_CURVE ( 'NONE', #69370, #20669, #4500, .T. ) ;
#41443 = VECTOR ( 'NONE', #12696, 1000.000000000000000 ) ;
#41444 = CARTESIAN_POINT ( 'NONE',  ( 283.0000000000000568, -25.93000000000544958, -9.412893218815410634 ) ) ;
#41445 = ORIENTED_EDGE ( 'NONE', *, *, #20682, .T. ) ;
#41446 = CARTESIAN_POINT ( 'NONE',  ( 8.144523737882817471, -8.835729544836345539, 54.00000000000000711 ) ) ;
#41447 = ORIENTED_EDGE ( 'NONE', *, *, #24857, .T. ) ;
#41448 = EDGE_CURVE ( 'NONE', #62359, #51203, #27260, .T. ) ;
#41449 = ORIENTED_EDGE ( 'NONE', *, *, #35797, .F. ) ;
#41450 = EDGE_CURVE ( 'NONE', #68247, #29691, #27100, .T. ) ;
#41451 = PLANE ( 'NONE',  #61862 ) ;
#41452 = CARTESIAN_POINT ( 'NONE',  ( -17.24945551514599984, -15.50000000000000000, -25.53140320652400064 ) ) ;
#41453 = CARTESIAN_POINT ( 'NONE',  ( 10.92648345035337343, -9.306483450353493225, 455.0000000000000568 ) ) ;
#41454 = EDGE_CURVE ( 'NONE', #54119, #28003, #6782, .T. ) ;
#41455 = EDGE_CURVE ( 'NONE', #55467, #17361, #10144, .T. ) ;
#41456 = EDGE_CURVE ( 'NONE', #55374, #24148, #48326, .T. ) ;
#41457 = CARTESIAN_POINT ( 'NONE',  ( -7.250000000000000888, 7.250000000000001776, -23.50000000000000000 ) ) ;
#41458 = DIRECTION ( 'NONE',  ( 9.912705577010336396E-15, 1.000000000000000000, 0.000000000000000000 ) ) ;
#41459 = ORIENTED_EDGE ( 'NONE', *, *, #22230, .T. ) ;
#41460 = ORIENTED_EDGE ( 'NONE', *, *, #18070, .F. ) ;
#41462 = VERTEX_POINT ( 'NONE', #31384 ) ;
#41461 = CARTESIAN_POINT ( 'NONE',  ( 75.42576880091934299, 10.00000000000000000, 330.9830310981789694 ) ) ;
#41463 = EDGE_CURVE ( 'NONE', #1953, #268, #69882, .T. ) ;
#41464 = ORIENTED_EDGE ( 'NONE', *, *, #66662, .T. ) ;
#41465 = CYLINDRICAL_SURFACE ( 'NONE', #67618, 1.929199999999998916 ) ;
#41466 = LINE ( 'NONE', #64104, #11701 ) ;
#41467 = DIRECTION ( 'NONE',  ( 1.000000000000000000, 0.000000000000000000, 0.000000000000000000 ) ) ;
#41468 = EDGE_CURVE ( 'NONE', #33465, #24609, #64585, .T. ) ;
#41469 = FACE_OUTER_BOUND ( 'NONE', #68607, .T. ) ;
#41470 = CIRCLE ( 'NONE', #67462, 1.500000000000000444 ) ;
#41471 = EDGE_CURVE ( 'NONE', #10448, #10609, #51974, .T. ) ;
#41472 = CARTESIAN_POINT ( 'NONE',  ( 7.357023737882797398, 4.947141984184415087, 54.00000000000000711 ) ) ;
#41473 = DIRECTION ( 'NONE',  ( 0.000000000000000000, 0.000000000000000000, 1.000000000000000000 ) ) ;
#41474 = EDGE_LOOP ( 'NONE', ( #49041, #36721, #22516, #37215 ) ) ;
#41475 = VERTEX_POINT ( 'NONE', #59276 ) ;
#41476 = ORIENTED_EDGE ( 'NONE', *, *, #5862, .F. ) ;
#41477 = VECTOR ( 'NONE', #3413, 1000.000000000000000 ) ;
#41478 = VERTEX_POINT ( 'NONE', #5538 ) ;
#41479 = LINE ( 'NONE', #25578, #32216 ) ;
#41480 = EDGE_CURVE ( 'NONE', #69235, #2477, #68499, .T. ) ;
#41481 = CARTESIAN_POINT ( 'NONE',  ( 152.0064834503532722, 2.160375375128253950, 5.000000000000000000 ) ) ;
#41483 = EDGE_CURVE ( 'NONE', #39722, #27985, #21490, .T. ) ;
#41482 = DIRECTION ( 'NONE',  ( 1.000000000000000000, 0.000000000000000000, 0.000000000000000000 ) ) ;
#41484 = AXIS2_PLACEMENT_3D ( 'NONE', #7212, #39395, #50358 ) ;
#41485 = CARTESIAN_POINT ( 'NONE',  ( 49.00000000000000000, 13.66939075806899950, 20.80000000000000426 ) ) ;
#41486 = CARTESIAN_POINT ( 'NONE',  ( -11.99351654964674374, -4.186483450353318148, 455.0000000000000568 ) ) ;
#41487 = ORIENTED_EDGE ( 'NONE', *, *, #28315, .T. ) ;
#41488 = ORIENTED_EDGE ( 'NONE', *, *, #61767, .F. ) ;
#41489 = ORIENTED_EDGE ( 'NONE', *, *, #53528, .T. ) ;
#41490 = DIRECTION ( 'NONE',  ( -1.000000000000000000, 0.000000000000000000, 0.000000000000000000 ) ) ;
#41491 = VECTOR ( 'NONE', #10814, 1000.000000000000000 ) ;
#41492 = AXIS2_PLACEMENT_3D ( 'NONE', #24059, #63304, #30068 ) ;
#41493 = ORIENTED_EDGE ( 'NONE', *, *, #21980, .F. ) ;
#41494 = ORIENTED_EDGE ( 'NONE', *, *, #38201, .T. ) ;
#41495 = CARTESIAN_POINT ( 'NONE',  ( 7.428221114745003462, -3.606483450353489939, 455.0000000000000568 ) ) ;
#41496 = ORIENTED_EDGE ( 'NONE', *, *, #55932, .T. ) ;
#41497 = ORIENTED_EDGE ( 'NONE', *, *, #39344, .T. ) ;
#41498 = DIRECTION ( 'NONE',  ( 1.000000000000000000, 0.000000000000000000, 0.000000000000000000 ) ) ;
#41500 = ORIENTED_EDGE ( 'NONE', *, *, #58554, .T. ) ;
#41499 = DIRECTION ( 'NONE',  ( 0.000000000000000000, 0.000000000000000000, -1.000000000000000000 ) ) ;
#41501 = ORIENTED_EDGE ( 'NONE', *, *, #54711, .T. ) ;
#41502 = LINE ( 'NONE', #52836, #63470 ) ;
#41503 = CARTESIAN_POINT ( 'NONE',  ( 8.465062094116072799, 4.242044687070411157, 455.0000000000000568 ) ) ;
#41505 = ORIENTED_EDGE ( 'NONE', *, *, #18365, .F. ) ;
#41504 = CARTESIAN_POINT ( 'NONE',  ( 4.720772854004770203, 6.344366288193352688, 54.00000000000000711 ) ) ;
#41506 = VERTEX_POINT ( 'NONE', #52588 ) ;
#41507 = DIRECTION ( 'NONE',  ( 0.4999999999999695799, -0.8660254037844563602, -6.723777587269172655E-17 ) ) ;
#41508 = CARTESIAN_POINT ( 'NONE',  ( 46.39999999999999858, 21.00000000000000000, -0.7500000000000000000 ) ) ;
#41509 = LINE ( 'NONE', #37263, #32363 ) ;
#41510 = DIRECTION ( 'NONE',  ( 1.000000000000000000, 0.000000000000000000, 0.000000000000000000 ) ) ;
#41511 = VERTEX_POINT ( 'NONE', #47275 ) ;
#41512 = DIRECTION ( 'NONE',  ( 0.000000000000000000, 1.000000000000000000, 0.000000000000000000 ) ) ;
#41513 = ADVANCED_FACE ( 'NONE', ( #68846 ), #7248, .T. ) ;
#41514 = DIRECTION ( 'NONE',  ( 0.8660254037844363761, -0.5000000000000038858, 0.000000000000000000 ) ) ;
#41515 = CARTESIAN_POINT ( 'NONE',  ( 283.0000000000000568, -20.40000000000000213, 17.60000000000000142 ) ) ;
#41516 = ORIENTED_EDGE ( 'NONE', *, *, #37707, .T. ) ;
#41518 = EDGE_CURVE ( 'NONE', #34655, #15827, #57, .T. ) ;
#41517 = CARTESIAN_POINT ( 'NONE',  ( 4.186483450353423841, 11.99351654964658742, 455.0000000000000568 ) ) ;
#41519 = CYLINDRICAL_SURFACE ( 'NONE', #65617, 3.499999999999999556 ) ;
#41520 = LINE ( 'NONE', #63442, #40432 ) ;
#41521 = EDGE_CURVE ( 'NONE', #7028, #69370, #60984, .T. ) ;
#41522 = ORIENTED_EDGE ( 'NONE', *, *, #9681, .F. ) ;
#41523 = AXIS2_PLACEMENT_3D ( 'NONE', #39141, #17567, #32798 ) ;
#41524 = CARTESIAN_POINT ( 'NONE',  ( 47.00000000000000000, 0.000000000000000000, 3.500000000000000000 ) ) ;
#41525 = ADVANCED_FACE ( 'NONE', ( #22148 ), #1271, .T. ) ;
#41526 = DIRECTION ( 'NONE',  ( 1.000000000000000000, 0.000000000000000000, 0.000000000000000000 ) ) ;
#41527 = VECTOR ( 'NONE', #8211, 1000.000000000000000 ) ;
#41528 = VECTOR ( 'NONE', #18889, 1000.000000000000000 ) ;
#41529 = DIRECTION ( 'NONE',  ( 1.000000000000000000, 0.000000000000000000, 0.000000000000000000 ) ) ;
#41530 = ORIENTED_EDGE ( 'NONE', *, *, #413, .T. ) ;
#41531 = FACE_OUTER_BOUND ( 'NONE', #60246, .T. ) ;
#41533 = CARTESIAN_POINT ( 'NONE',  ( -11.00000000000000000, -12.00000000000000000, 11.03137303340310282 ) ) ;
#41532 = AXIS2_PLACEMENT_3D ( 'NONE', #1410, #50548, #43854 ) ;
#41534 = CARTESIAN_POINT ( 'NONE',  ( -17.00000000000000000, -16.28999999999999915, 14.50000000000000000 ) ) ;
#41535 = VECTOR ( 'NONE', #69798, 1000.000000000000000 ) ;
#41536 = CARTESIAN_POINT ( 'NONE',  ( -30.00000000000000000, -9.454754784057099570, 17.53999999999999915 ) ) ;
#41537 = AXIS2_PLACEMENT_3D ( 'NONE', #47301, #21132, #69577 ) ;
#41538 = CYLINDRICAL_SURFACE ( 'NONE', #59080, 1.000000000000000000 ) ;
#41539 = VERTEX_POINT ( 'NONE', #32748 ) ;
#41540 = FACE_OUTER_BOUND ( 'NONE', #9101, .T. ) ;
#41541 = CARTESIAN_POINT ( 'NONE',  ( -12.00000000000000000, 11.18999999999999950, -5.000000000000000000 ) ) ;
#41542 = LINE ( 'NONE', #37292, #19866 ) ;
#41543 = EDGE_CURVE ( 'NONE', #30263, #54026, #66322, .T. ) ;
#41544 = DIRECTION ( 'NONE',  ( -0.8660254037844528074, -0.4999999999999755196, 6.723777587269129514E-17 ) ) ;
#41545 = LINE ( 'NONE', #63110, #63294 ) ;
#41546 = ORIENTED_EDGE ( 'NONE', *, *, #47934, .T. ) ;
#41548 = ORIENTED_EDGE ( 'NONE', *, *, #26781, .F. ) ;
#41547 = DIRECTION ( 'NONE',  ( -0.000000000000000000, -0.000000000000000000, -1.000000000000000000 ) ) ;
#41549 = VECTOR ( 'NONE', #11573, 1000.000000000000000 ) ;
#41550 = CARTESIAN_POINT ( 'NONE',  ( -10.91351654964670814, 2.893516549646604208, 195.0000000000000284 ) ) ;
#41551 = DIRECTION ( 'NONE',  ( 0.000000000000000000, 0.000000000000000000, -1.000000000000000000 ) ) ;
#41552 = DIRECTION ( 'NONE',  ( -1.000000000000000000, 0.000000000000000000, 0.000000000000000000 ) ) ;
#41553 = ORIENTED_EDGE ( 'NONE', *, *, #69883, .F. ) ;
#41554 = DIRECTION ( 'NONE',  ( -1.836970198721029934E-16, 1.836970198721036590E-16, -1.000000000000000000 ) ) ;
#41555 = LINE ( 'NONE', #58170, #57828 ) ;
#41556 = ORIENTED_EDGE ( 'NONE', *, *, #3376, .T. ) ;
#41557 = ORIENTED_EDGE ( 'NONE', *, *, #185, .T. ) ;
#41558 = VERTEX_POINT ( 'NONE', #49022 ) ;
#41559 = DIRECTION ( 'NONE',  ( -1.000000000000000000, 0.000000000000000000, 0.000000000000000000 ) ) ;
#41560 = EDGE_CURVE ( 'NONE', #64638, #25131, #34119, .T. ) ;
#41561 = PLANE ( 'NONE',  #13967 ) ;
#41562 = DIRECTION ( 'NONE',  ( 0.000000000000000000, 0.000000000000000000, -1.000000000000000000 ) ) ;
#41564 = EDGE_CURVE ( 'NONE', #29410, #4021, #33883, .T. ) ;
#41563 = FACE_OUTER_BOUND ( 'NONE', #66575, .T. ) ;
#41565 = AXIS2_PLACEMENT_3D ( 'NONE', #48852, #53816, #17343 ) ;
#41566 = VERTEX_POINT ( 'NONE', #38409 ) ;
#41568 = ADVANCED_FACE ( 'NONE', ( #945 ), #65622, .T. ) ;
#41567 = VERTEX_POINT ( 'NONE', #16838 ) ;
#41569 = CARTESIAN_POINT ( 'NONE',  ( 15.70366306705349757, -0.2717122460102775472, 21.17420925361331641 ) ) ;
#41570 = CARTESIAN_POINT ( 'NONE',  ( 0.000000000000000000, -7.449999999999998401, -17.50000000000000000 ) ) ;
#41571 = VERTEX_POINT ( 'NONE', #64937 ) ;
#41572 = ORIENTED_EDGE ( 'NONE', *, *, #9041, .T. ) ;
#41573 = VERTEX_POINT ( 'NONE', #43351 ) ;
#41574 = EDGE_LOOP ( 'NONE', ( #59461, #53823, #17709, #53250 ) ) ;
#41575 = DIRECTION ( 'NONE',  ( 9.912705577010386883E-15, 1.000000000000000000, 0.000000000000000000 ) ) ;
#41576 = UNCERTAINTY_MEASURE_WITH_UNIT (LENGTH_MEASURE( 1.000000000000000082E-05 ), #22887, 'distance_accuracy_value', 'NONE');
#41578 = ORIENTED_EDGE ( 'NONE', *, *, #6724, .T. ) ;
#41577 = CARTESIAN_POINT ( 'NONE',  ( 30.00000000000000000, -9.200000000000120082, -17.30000000000000071 ) ) ;
#41579 = VECTOR ( 'NONE', #45882, 1000.000000000000000 ) ;
#41580 = CARTESIAN_POINT ( 'NONE',  ( -7.450000000000001954, 7.250000000000000000, -13.50000000000000178 ) ) ;
#41581 = CYLINDRICAL_SURFACE ( 'NONE', #37430, 24.99999999998784972 ) ;
#41582 = VERTEX_POINT ( 'NONE', #59965 ) ;
#41583 = ORIENTED_EDGE ( 'NONE', *, *, #62602, .F. ) ;
#41584 = VECTOR ( 'NONE', #67129, 1000.000000000000000 ) ;
#41585 = LINE ( 'NONE', #53263, #34543 ) ;
#41586 = CARTESIAN_POINT ( 'NONE',  ( 9.899999999999998579, -0.2000000000000000111, 0.000000000000000000 ) ) ;
#41587 = VERTEX_POINT ( 'NONE', #17175 ) ;
#41588 = VECTOR ( 'NONE', #7928, 1000.000000000000000 ) ;
#41589 = EDGE_CURVE ( 'NONE', #53596, #28131, #39535, .T. ) ;
#41590 = PRESENTATION_STYLE_ASSIGNMENT (( #69514 ) ) ;
#41591 = CARTESIAN_POINT ( 'NONE',  ( -7.250000000000001776, -7.249999999999998224, -13.00000000000000178 ) ) ;
#41592 = SURFACE_STYLE_USAGE ( .BOTH. , #46889 ) ;
#41593 = EDGE_LOOP ( 'NONE', ( #15846, #28235, #56302, #58820 ) ) ;
#41594 = DIRECTION ( 'NONE',  ( -1.836970198721029934E-16, 1.836970198721036344E-16, -1.000000000000000000 ) ) ;
#41596 = EDGE_CURVE ( 'NONE', #63119, #24837, #17874, .T. ) ;
#41595 = CARTESIAN_POINT ( 'NONE',  ( -10.19191654964671301, 10.19191654964664018, 195.0000000000000284 ) ) ;
#41597 = CARTESIAN_POINT ( 'NONE',  ( 7.357023737882800951, 6.651770455163678264, 26.00000000000000711 ) ) ;
#41598 = LINE ( 'NONE', #15436, #37026 ) ;
#41599 = EDGE_CURVE ( 'NONE', #2177, #22188, #49381, .T. ) ;
#41600 = ADVANCED_FACE ( 'NONE', ( #55033 ), #49705, .T. ) ;
#41601 = DIRECTION ( 'NONE',  ( 1.678252938371784572E-14, 1.000000000000000000, 0.000000000000000000 ) ) ;
#41603 = ORIENTED_EDGE ( 'NONE', *, *, #28354, .F. ) ;
#41602 = EDGE_CURVE ( 'NONE', #39378, #55613, #6584, .T. ) ;
#41604 = DIRECTION ( 'NONE',  ( -1.000000000000000000, 0.000000000000000000, 0.000000000000000000 ) ) ;
#41605 = EDGE_CURVE ( 'NONE', #21803, #34676, #65954, .T. ) ;
#41606 = PLANE ( 'NONE',  #3373 ) ;
#41607 = CARTESIAN_POINT ( 'NONE',  ( -8.250000000000001776, -7.249999999999998224, -26.00000000000001066 ) ) ;
#41608 = LINE ( 'NONE', #63174, #34538 ) ;
#41609 = EDGE_CURVE ( 'NONE', #65753, #27294, #12209, .T. ) ;
#41610 = CARTESIAN_POINT ( 'NONE',  ( 14.50000000000000000, 0.000000000000000000, 26.50000000000000000 ) ) ;
#41611 = CARTESIAN_POINT ( 'NONE',  ( 30.00000000000000000, -13.79999999999979998, -17.30000000000000071 ) ) ;
#41612 = DIRECTION ( 'NONE',  ( 0.000000000000000000, 0.000000000000000000, 1.000000000000000000 ) ) ;
#41613 = CARTESIAN_POINT ( 'NONE',  ( 4.740315990920191958, 4.188533722949208560, 455.0000000000000568 ) ) ;
#41614 = ORIENTED_EDGE ( 'NONE', *, *, #4025, .F. ) ;
#41615 = CARTESIAN_POINT ( 'NONE',  ( 30.90000000000000213, 13.66939075806899240, -20.79999999999999361 ) ) ;
#41616 = DIRECTION ( 'NONE',  ( -1.000000000000000000, 0.000000000000000000, 0.000000000000000000 ) ) ;
#41617 = ORIENTED_EDGE ( 'NONE', *, *, #60813, .T. ) ;
#41618 = DIRECTION ( 'NONE',  ( 1.000000000000000000, 0.000000000000000000, 0.000000000000000000 ) ) ;
#41619 = CARTESIAN_POINT ( 'NONE',  ( 3.848229544836329730, 7.342976262117204556, 54.00000000000000711 ) ) ;
#41620 = CARTESIAN_POINT ( 'NONE',  ( 106.4257688009193998, 0.000000000000000000, 282.4830310981789125 ) ) ;
#41621 = LINE ( 'NONE', #25363, #363 ) ;
#41622 = FACE_OUTER_BOUND ( 'NONE', #33879, .T. ) ;
#41623 = EDGE_LOOP ( 'NONE', ( #48484, #66229, #63384, #40445 ) ) ;
#41624 = AXIS2_PLACEMENT_3D ( 'NONE', #1887, #23457, #37383 ) ;
#41625 = ORIENTED_EDGE ( 'NONE', *, *, #57857, .F. ) ;
#41626 = CARTESIAN_POINT ( 'NONE',  ( 49.00000000000000000, -0.1999999999911430404, -8.864436962241481021E-12 ) ) ;
#41627 = CARTESIAN_POINT ( 'NONE',  ( 2.544523737882817382, 9.547976262117206403, 54.00000000000000711 ) ) ;
#41628 = EDGE_LOOP ( 'NONE', ( #13804, #48504, #44743, #67103 ) ) ;
#41629 = DIRECTION ( 'NONE',  ( -1.836970198721029934E-16, 1.836970198721036590E-16, -1.000000000000000000 ) ) ;
#41630 = AXIS2_PLACEMENT_3D ( 'NONE', #68384, #3334, #46459 ) ;
#41631 = CARTESIAN_POINT ( 'NONE',  ( 7.357023737882784964, 3.834182069070697807, 54.00000000000000711 ) ) ;
#41632 = ORIENTED_EDGE ( 'NONE', *, *, #31182, .F. ) ;
#41633 = DIRECTION ( 'NONE',  ( 0.000000000000000000, 0.7084617869628681008, 0.7057491738665939707 ) ) ;
#41634 = ORIENTED_EDGE ( 'NONE', *, *, #25391, .T. ) ;
#41635 = ORIENTED_EDGE ( 'NONE', *, *, #46226, .F. ) ;
#41636 = DIRECTION ( 'NONE',  ( -0.000000000000000000, 3.673940397442059868E-16, -1.000000000000000000 ) ) ;
#41637 = VERTEX_POINT ( 'NONE', #33782 ) ;
#41638 = EDGE_LOOP ( 'NONE', ( #3057, #68648, #20146, #68419 ) ) ;
#41639 = AXIS2_PLACEMENT_3D ( 'NONE', #28211, #1012, #65697 ) ;
#41640 = CARTESIAN_POINT ( 'NONE',  ( 11.00000000000000000, -12.00000000000000000, 10.52786404500095863 ) ) ;
#41642 = EDGE_CURVE ( 'NONE', #17131, #64382, #28469, .T. ) ;
#41641 = DIRECTION ( 'NONE',  ( 0.000000000000000000, -0.000000000000000000, -1.000000000000000000 ) ) ;
#41643 = CARTESIAN_POINT ( 'NONE',  ( 7.000000000000000000, -26.28355339059299922, 9.766446609406699508 ) ) ;
#41644 = ORIENTED_EDGE ( 'NONE', *, *, #8795, .T. ) ;
#41645 = EDGE_CURVE ( 'NONE', #46607, #20190, #57448, .T. ) ;
#41646 = CARTESIAN_POINT ( 'NONE',  ( 8.900000000000005684, -14.48845687959340012, -21.00000000000000000 ) ) ;
#41647 = ADVANCED_FACE ( 'NONE', ( #8295 ), #67002, .F. ) ;
#41649 = CARTESIAN_POINT ( 'NONE',  ( -8.250000000000001776, 7.250000000000000888, -26.00000000000001066 ) ) ;
#41648 = CARTESIAN_POINT ( 'NONE',  ( 275.5000000000000000, 0.000000000000000000, 26.50000000000000000 ) ) ;
#41650 = ORIENTED_EDGE ( 'NONE', *, *, #227, .T. ) ;
#41652 = EDGE_LOOP ( 'NONE', ( #65469, #20763, #30612, #24984 ) ) ;
#41651 = DIRECTION ( 'NONE',  ( 0.000000000000000000, -1.000000000000000000, -3.673940397442059868E-16 ) ) ;
#41653 = ORIENTED_EDGE ( 'NONE', *, *, #17579, .T. ) ;
#41654 = EDGE_CURVE ( 'NONE', #32917, #51761, #28815, .T. ) ;
#41655 = APPLICATION_PROTOCOL_DEFINITION ( 'draft international standard', 'automotive_design', 1998, #39479 ) ;
#41656 = CARTESIAN_POINT ( 'NONE',  ( 9.106483450353417552, 10.91351654964656603, 455.0000000000000568 ) ) ;
#41658 = ORIENTED_EDGE ( 'NONE', *, *, #6317, .T. ) ;
#41657 = LINE ( 'NONE', #63589, #20666 ) ;
#41659 = LINE ( 'NONE', #36353, #54827 ) ;
#41660 = CARTESIAN_POINT ( 'NONE',  ( -10.73351654964664981, -1.690483450353293948, 195.0000000000000284 ) ) ;
#41661 = ORIENTED_EDGE ( 'NONE', *, *, #11560, .F. ) ;
#41662 = ORIENTED_EDGE ( 'NONE', *, *, #3298, .F. ) ;
#41663 = DIRECTION ( 'NONE',  ( 0.6414496315691494699, -0.7671651518153064231, 0.000000000000000000 ) ) ;
#41664 = ORIENTED_EDGE ( 'NONE', *, *, #45773, .T. ) ;
#41665 = CIRCLE ( 'NONE', #47325, 0.1999999999999996503 ) ;
#41666 = DIRECTION ( 'NONE',  ( 0.000000000000000000, 0.000000000000000000, 1.000000000000000000 ) ) ;
#41667 = LINE ( 'NONE', #19739, #27865 ) ;
#41668 = CYLINDRICAL_SURFACE ( 'NONE', #9117, 0.2000000000000005107 ) ;
#41669 = ORIENTED_EDGE ( 'NONE', *, *, #45582, .F. ) ;
#41670 = VECTOR ( 'NONE', #65475, 1000.000000000000000 ) ;
#41671 = CARTESIAN_POINT ( 'NONE',  ( 283.0000000000000568, -38.15000000000000568, -13.19999999999999929 ) ) ;
#41672 = DIRECTION ( 'NONE',  ( -1.000000000000000000, 2.602085213965213008E-15, 0.000000000000000000 ) ) ;
#41674 = ORIENTED_EDGE ( 'NONE', *, *, #41851, .F. ) ;
#41673 = CARTESIAN_POINT ( 'NONE',  ( -8.250000000000000000, 7.250000000000001776, -25.00000000000000000 ) ) ;
#41676 = ORIENTED_EDGE ( 'NONE', *, *, #29379, .T. ) ;
#41675 = DIRECTION ( 'NONE',  ( 0.000000000000000000, 0.7071067811865474617, -0.7071067811865474617 ) ) ;
#41677 = DIRECTION ( 'NONE',  ( -0.7071067811865476838, -0.4999999999999997780, -0.4999999999999997780 ) ) ;
#41678 = AXIS2_PLACEMENT_3D ( 'NONE', #40379, #56638, #7834 ) ;
#41679 = CARTESIAN_POINT ( 'NONE',  ( 6.832023737882815695, 9.722976262117192903, 54.00000000000000711 ) ) ;
#41680 = CARTESIAN_POINT ( 'NONE',  ( 7.450000000000006395, 7.250000000000000888, -24.00000000000000000 ) ) ;
#41681 = DIRECTION ( 'NONE',  ( 1.000000000000000000, 0.000000000000000000, 0.000000000000000000 ) ) ;
#41682 = AXIS2_PLACEMENT_3D ( 'NONE', #46532, #30631, #24634 ) ;
#41683 = DIRECTION ( 'NONE',  ( -1.000000000000000000, 3.491481338843132961E-15, 1.836970198721036344E-16 ) ) ;
#41684 = ORIENTED_EDGE ( 'NONE', *, *, #33560, .T. ) ;
#41685 = LINE ( 'NONE', #9519, #61750 ) ;
#41686 = EDGE_CURVE ( 'NONE', #67430, #54079, #2308, .T. ) ;
#41687 = FACE_OUTER_BOUND ( 'NONE', #26175, .T. ) ;
#41688 = CARTESIAN_POINT ( 'NONE',  ( 8.900000000000005684, 13.66939075806899240, -20.79999999999999361 ) ) ;
#41690 = VECTOR ( 'NONE', #66704, 1000.000000000000000 ) ;
#41689 = VECTOR ( 'NONE', #36655, 1000.000000000000000 ) ;
#41692 = EDGE_LOOP ( 'NONE', ( #44923, #54285, #8121, #22512 ) ) ;
#41691 = CARTESIAN_POINT ( 'NONE',  ( -5.779227145995285753, 6.344366288193338477, 54.00000000000000711 ) ) ;
#41693 = DIRECTION ( 'NONE',  ( 0.000000000000000000, -3.673940397442059868E-16, 1.000000000000000000 ) ) ;
#41694 = EDGE_CURVE ( 'NONE', #61884, #31017, #31654, .T. ) ;
#41695 = LINE ( 'NONE', #50897, #35208 ) ;
#41696 = AXIS2_PLACEMENT_3D ( 'NONE', #43510, #48834, #27270 ) ;
#41697 = DIRECTION ( 'NONE',  ( -0.000000000000000000, 1.000000000000000000, -0.000000000000000000 ) ) ;
#41698 = ORIENTED_EDGE ( 'NONE', *, *, #19413, .T. ) ;
#41699 = DIRECTION ( 'NONE',  ( 0.000000000000000000, 1.000000000000000000, 0.000000000000000000 ) ) ;
#41700 = FACE_OUTER_BOUND ( 'NONE', #35419, .T. ) ;
#41701 = EDGE_LOOP ( 'NONE', ( #49509, #54357, #21714, #24805 ) ) ;
#41702 = CARTESIAN_POINT ( 'NONE',  ( -7.603567055985586798, -8.406483450353363196, 195.0000000000000284 ) ) ;
#41703 = CARTESIAN_POINT ( 'NONE',  ( 14.89999999999999680, 13.66939075806899240, 20.79999999999999361 ) ) ;
#41704 = CARTESIAN_POINT ( 'NONE',  ( 11.00000000000000000, -11.50000000000100009, 15.00000000000084910 ) ) ;
#41705 = CARTESIAN_POINT ( 'NONE',  ( 7.250000000000004441, 7.450000000000001954, -25.50000000000000355 ) ) ;
#41706 = ADVANCED_FACE ( 'NONE', ( #35166 ), #51447, .F. ) ;
#41707 = LINE ( 'NONE', #40657, #21710 ) ;
#41708 = ORIENTED_EDGE ( 'NONE', *, *, #59779, .F. ) ;
#41709 = DIRECTION ( 'NONE',  ( 0.000000000000000000, -0.7071067811865475727, -0.7071067811865475727 ) ) ;
#41710 = ORIENTED_EDGE ( 'NONE', *, *, #41242, .T. ) ;
#41711 = FACE_OUTER_BOUND ( 'NONE', #36128, .T. ) ;
#41712 = VECTOR ( 'NONE', #40345, 1000.000000000000000 ) ;
#41713 = ORIENTED_EDGE ( 'NONE', *, *, #57009, .T. ) ;
#41714 = ORIENTED_EDGE ( 'NONE', *, *, #46205, .F. ) ;
#41715 = FACE_OUTER_BOUND ( 'NONE', #59565, .T. ) ;
#41716 = DIRECTION ( 'NONE',  ( 0.000000000000000000, 0.000000000000000000, 1.000000000000000000 ) ) ;
#41717 = DIRECTION ( 'NONE',  ( 0.000000000000000000, 1.000000000000000000, 0.000000000000000000 ) ) ;
#41718 = VERTEX_POINT ( 'NONE', #30240 ) ;
#41719 = EDGE_LOOP ( 'NONE', ( #27056, #69293, #36326, #9022 ) ) ;
#41720 = DIRECTION ( 'NONE',  ( 0.7671651518152895477, -0.6414496315691698980, 0.000000000000000000 ) ) ;
#41721 = VERTEX_POINT ( 'NONE', #40119 ) ;
#41722 = VECTOR ( 'NONE', #67818, 1000.000000000000000 ) ;
#41723 = ORIENTED_EDGE ( 'NONE', *, *, #33297, .F. ) ;
#41724 = DIRECTION ( 'NONE',  ( 0.000000000000000000, -1.000000000000000000, 0.000000000000000000 ) ) ;
#41725 = CARTESIAN_POINT ( 'NONE',  ( 25.50000000000000355, -5.578999999999999737, -22.50000000000000000 ) ) ;
#41726 = DIRECTION ( 'NONE',  ( 9.799566706031580591E-15, 1.000000000000000000, 1.836970198721018348E-16 ) ) ;
#41727 = ORIENTED_EDGE ( 'NONE', *, *, #40333, .T. ) ;
#41728 = CIRCLE ( 'NONE', #11236, 0.9999999999999991118 ) ;
#41729 = DIRECTION ( 'NONE',  ( 0.000000000000000000, 1.000000000000000000, 0.000000000000000000 ) ) ;
#41731 = CARTESIAN_POINT ( 'NONE',  ( 46.39999999999999858, 21.00000000000000000, 0.2500000000000000000 ) ) ;
#41730 = DIRECTION ( 'NONE',  ( -2.990116172375847553E-15, -1.000000000000000000, -1.836970198721030920E-16 ) ) ;
#41732 = ORIENTED_EDGE ( 'NONE', *, *, #48720, .F. ) ;
#41734 = ORIENTED_EDGE ( 'NONE', *, *, #30584, .T. ) ;
#41733 = CARTESIAN_POINT ( 'NONE',  ( -7.250000000000000888, -8.249999999999998224, -26.00000000000001066 ) ) ;
#41735 = ORIENTED_EDGE ( 'NONE', *, *, #3710, .T. ) ;
#41736 = ADVANCED_FACE ( 'NONE', ( #18925 ), #50395, .F. ) ;
#41737 = AXIS2_PLACEMENT_3D ( 'NONE', #18738, #51258, #45251 ) ;
#41738 = FACE_OUTER_BOUND ( 'NONE', #25736, .T. ) ;
#41739 = AXIS2_PLACEMENT_3D ( 'NONE', #54321, #11852, #21440 ) ;
#41740 = DIRECTION ( 'NONE',  ( 0.000000000000000000, 0.000000000000000000, -1.000000000000000000 ) ) ;
#41741 = ORIENTED_EDGE ( 'NONE', *, *, #62548, .T. ) ;
#41742 = ORIENTED_EDGE ( 'NONE', *, *, #59029, .T. ) ;
#41743 = CONICAL_SURFACE ( 'NONE', #5621, 4.000000000000000000, 0.7853981633974730370 ) ;
#41744 = EDGE_CURVE ( 'NONE', #46007, #25422, #50737, .T. ) ;
#41745 = FACE_OUTER_BOUND ( 'NONE', #51032, .T. ) ;
#41746 = LINE ( 'NONE', #19478, #59407 ) ;
#41747 = ORIENTED_EDGE ( 'NONE', *, *, #25673, .T. ) ;
#41748 = ORIENTED_EDGE ( 'NONE', *, *, #42176, .F. ) ;
#41749 = PLANE ( 'NONE',  #60172 ) ;
#41750 = ADVANCED_FACE ( 'NONE', ( #62388 ), #18083, .F. ) ;
#41751 = PLANE ( 'NONE',  #13599 ) ;
#41752 = EDGE_LOOP ( 'NONE', ( #6263, #62340, #2867, #38686 ) ) ;
#41753 = DIRECTION ( 'NONE',  ( 1.000000000000000000, 0.000000000000000000, 0.000000000000000000 ) ) ;
#41754 = VECTOR ( 'NONE', #36988, 1000.000000000000000 ) ;
#41755 = CARTESIAN_POINT ( 'NONE',  ( -7.250000000000001776, -7.249999999999998224, -24.50000000000000000 ) ) ;
#41757 = EDGE_LOOP ( 'NONE', ( #21197, #46163, #43474, #1564 ) ) ;
#41756 = LINE ( 'NONE', #4308, #66740 ) ;
#41758 = EDGE_LOOP ( 'NONE', ( #68880, #32166, #59244, #6738 ) ) ;
#41759 = DIRECTION ( 'NONE',  ( 1.836970198721029934E-16, 1.836970198721010706E-16, -1.000000000000000000 ) ) ;
#41760 = CARTESIAN_POINT ( 'NONE',  ( 0.000000000000000000, -7.449999999999998401, -7.000000000000000000 ) ) ;
#41761 = LINE ( 'NONE', #41415, #48228 ) ;
#41762 = LINE ( 'NONE', #53441, #53880 ) ;
#41763 = PLANE ( 'NONE',  #68961 ) ;
#41764 = APPLICATION_CONTEXT ( 'automotive_design' ) ;
#41765 = CARTESIAN_POINT ( 'NONE',  ( 30.00000000000000000, -9.200000000000120082, -17.30000000000000071 ) ) ;
#41766 = EDGE_LOOP ( 'NONE', ( #10034, #58490, #46595, #35476 ) ) ;
#41767 = LINE ( 'NONE', #43512, #53010 ) ;
#41768 = AXIS2_PLACEMENT_3D ( 'NONE', #10078, #69825, #53229 ) ;
#41769 = AXIS2_PLACEMENT_3D ( 'NONE', #3812, #25746, #19707 ) ;
#41770 = ADVANCED_FACE ( 'NONE', ( #51799 ), #62748, .T. ) ;
#41772 = VERTEX_POINT ( 'NONE', #34819 ) ;
#41771 = DIRECTION ( 'NONE',  ( 0.000000000000000000, 0.000000000000000000, -1.000000000000000000 ) ) ;
#41773 = DIRECTION ( 'NONE',  ( 0.000000000000000000, 0.7071067811865475727, -0.7071067811865475727 ) ) ;
#41774 = DIRECTION ( 'NONE',  ( -0.000000000000000000, 3.673940397442059868E-16, -1.000000000000000000 ) ) ;
#41775 = EDGE_CURVE ( 'NONE', #66751, #10351, #40480, .T. ) ;
#41776 = LINE ( 'NONE', #31191, #56790 ) ;
#41777 = ADVANCED_FACE ( 'NONE', ( #2648 ), #51089, .F. ) ;
#41778 = FACE_OUTER_BOUND ( 'NONE', #32794, .T. ) ;
#41779 = AXIS2_PLACEMENT_3D ( 'NONE', #43783, #33847, #38145 ) ;
#41780 = EDGE_CURVE ( 'NONE', #11827, #1911, #42940, .T. ) ;
#41781 = VERTEX_POINT ( 'NONE', #45786 ) ;
#41782 = FACE_OUTER_BOUND ( 'NONE', #13907, .T. ) ;
#41783 = LINE ( 'NONE', #25887, #4602 ) ;
#41784 = EDGE_LOOP ( 'NONE', ( #20019, #64664, #69549, #68348, #33120, #18049, #7072, #6194 ) ) ;
#41785 = DIRECTION ( 'NONE',  ( 0.000000000000000000, -1.000000000000000000, 0.000000000000000000 ) ) ;
#41786 = SURFACE_STYLE_FILL_AREA ( #36484 ) ;
#41787 = EDGE_CURVE ( 'NONE', #16822, #54243, #67363, .T. ) ;
#41788 = VECTOR ( 'NONE', #14617, 1000.000000000000000 ) ;
#41789 = ADVANCED_FACE ( 'NONE', ( #14325 ), #35888, .F. ) ;
#41790 = AXIS2_PLACEMENT_3D ( 'NONE', #6494, #28058, #49617 ) ;
#41791 = DIRECTION ( 'NONE',  ( -0.000000000000000000, -0.000000000000000000, -1.000000000000000000 ) ) ;
#41792 = ORIENTED_EDGE ( 'NONE', *, *, #28502, .T. ) ;
#41793 = CARTESIAN_POINT ( 'NONE',  ( 24.00000000000000000, -15.50000000000000000, -14.50000000000000000 ) ) ;
#41794 = ORIENTED_EDGE ( 'NONE', *, *, #29811, .F. ) ;
#41795 = EDGE_LOOP ( 'NONE', ( #13004, #31568, #17193, #62610 ) ) ;
#41796 = PLANE ( 'NONE',  #52859 ) ;
#41797 = VECTOR ( 'NONE', #55250, 1000.000000000000000 ) ;
#41798 = DIRECTION ( 'NONE',  ( -1.000000000000000000, 0.000000000000000000, 0.000000000000000000 ) ) ;
#41799 = CIRCLE ( 'NONE', #11308, 0.3499999999999611200 ) ;
#41800 = CARTESIAN_POINT ( 'NONE',  ( 7.250000000000005329, -7.449999999999998401, -20.50000000000000000 ) ) ;
#41801 = DIRECTION ( 'NONE',  ( 0.000000000000000000, -1.000000000000000000, 0.000000000000000000 ) ) ;
#41802 = CARTESIAN_POINT ( 'NONE',  ( -11.18999999999999950, -11.18999999999999950, -4.250000000000000000 ) ) ;
#41803 = ORIENTED_EDGE ( 'NONE', *, *, #32603, .T. ) ;
#41804 = ORIENTED_EDGE ( 'NONE', *, *, #8341, .F. ) ;
#41806 = ORIENTED_EDGE ( 'NONE', *, *, #30209, .T. ) ;
#41805 = CARTESIAN_POINT ( 'NONE',  ( 8.711985858128638682, 2.406732575409522568, 26.00000000000000711 ) ) ;
#41807 = ORIENTED_EDGE ( 'NONE', *, *, #44053, .T. ) ;
#41808 = DIRECTION ( 'NONE',  ( 0.000000000000000000, -1.000000000000000000, 0.000000000000000000 ) ) ;
#41809 = CARTESIAN_POINT ( 'NONE',  ( 22.14589803375000088, -15.50000000000000000, -21.50000000000000000 ) ) ;
#41810 = CIRCLE ( 'NONE', #19245, 1.000000000000001776 ) ;
#41811 = EDGE_CURVE ( 'NONE', #65753, #59053, #61337, .T. ) ;
#41812 = CARTESIAN_POINT ( 'NONE',  ( 29.50000000000000355, -12.00000000000000000, 10.69999999999999929 ) ) ;
#41813 = LINE ( 'NONE', #4362, #52554 ) ;
#41815 = CARTESIAN_POINT ( 'NONE',  ( -11.77351654964670935, 4.173516549646604901, 455.0000000000000568 ) ) ;
#41814 = CARTESIAN_POINT ( 'NONE',  ( 151.5599459900709860, -10.00000000000000178, 324.6739988703752715 ) ) ;
#41816 = ORIENTED_EDGE ( 'NONE', *, *, #55795, .F. ) ;
#41817 = ORIENTED_EDGE ( 'NONE', *, *, #67747, .T. ) ;
#41818 = ORIENTED_EDGE ( 'NONE', *, *, #17557, .F. ) ;
#41819 = EDGE_CURVE ( 'NONE', #18073, #60008, #64176, .T. ) ;
#41820 = EDGE_LOOP ( 'NONE', ( #15855, #19352, #18590, #53103 ) ) ;
#41821 = DIRECTION ( 'NONE',  ( -1.000000000000000000, 0.000000000000000000, 0.000000000000000000 ) ) ;
#41822 = CARTESIAN_POINT ( 'NONE',  ( -6.822336235477446387, -4.149127210878696737, 54.00000000000000711 ) ) ;
#41823 = AXIS2_PLACEMENT_3D ( 'NONE', #55836, #34610, #16978 ) ;
#41824 =( LENGTH_UNIT ( ) NAMED_UNIT ( * ) SI_UNIT ( .MILLI., .METRE. ) );
#41825 = CARTESIAN_POINT ( 'NONE',  ( 283.0000000000000568, -30.45000000000000639, 15.00000000000000000 ) ) ;
#41826 = AXIS2_PLACEMENT_3D ( 'NONE', #54329, #65294, #48672 ) ;
#41827 = VERTEX_POINT ( 'NONE', #4072 ) ;
#41828 = VERTEX_POINT ( 'NONE', #36951 ) ;
#41829 = ORIENTED_EDGE ( 'NONE', *, *, #29811, .T. ) ;
#41830 = AXIS2_PLACEMENT_3D ( 'NONE', #31373, #4141, #63170 ) ;
#41831 = ORIENTED_EDGE ( 'NONE', *, *, #14494, .F. ) ;
#41832 = VERTEX_POINT ( 'NONE', #58858 ) ;
#41833 = DIRECTION ( 'NONE',  ( -1.000000000000000000, 0.000000000000000000, 0.000000000000000000 ) ) ;
#41834 = ORIENTED_EDGE ( 'NONE', *, *, #12216, .T. ) ;
#41835 = VECTOR ( 'NONE', #7614, 1000.000000000000000 ) ;
#41836 = ORIENTED_EDGE ( 'NONE', *, *, #26779, .T. ) ;
#41837 = CARTESIAN_POINT ( 'NONE',  ( 11.48848345035342078, 11.07551654964652599, 455.0000000000000568 ) ) ;
#41838 = EDGE_CURVE ( 'NONE', #22707, #49327, #69111, .T. ) ;
#41840 = ORIENTED_EDGE ( 'NONE', *, *, #35885, .F. ) ;
#41839 = DIRECTION ( 'NONE',  ( 0.000000000000000000, -1.000000000000000000, 0.000000000000000000 ) ) ;
#41841 = ORIENTED_EDGE ( 'NONE', *, *, #67100, .F. ) ;
#41842 = DIRECTION ( 'NONE',  ( 0.000000000000000000, 0.000000000000000000, -1.000000000000000000 ) ) ;
#41843 = LINE ( 'NONE', #19577, #26697 ) ;
#41844 = ADVANCED_FACE ( 'NONE', ( #4427 ), #9362, .T. ) ;
#41846 = ORIENTED_EDGE ( 'NONE', *, *, #62111, .T. ) ;
#41845 = CARTESIAN_POINT ( 'NONE',  ( 30.00000000000000000, -5.200000000000001066, 9.400000000000000355 ) ) ;
#41847 = EDGE_CURVE ( 'NONE', #48034, #49731, #25639, .T. ) ;
#41848 = EDGE_LOOP ( 'NONE', ( #62104, #1145, #24135, #42619 ) ) ;
#41849 = DIRECTION ( 'NONE',  ( 9.912705577010336396E-15, 1.000000000000000000, 0.000000000000000000 ) ) ;
#41850 = CIRCLE ( 'NONE', #21511, 4.000000000000001776 ) ;
#41851 = EDGE_CURVE ( 'NONE', #50527, #63961, #15019, .T. ) ;
#41852 = CARTESIAN_POINT ( 'NONE',  ( -5.993516549646728642, -6.006483450353378828, 195.0000000000000284 ) ) ;
#41853 = EDGE_CURVE ( 'NONE', #30539, #2766, #30930, .T. ) ;
#41854 = ADVANCED_FACE ( 'NONE', ( #42230, #30579 ), #21015, .F. ) ;
#41855 = CARTESIAN_POINT ( 'NONE',  ( 9.912023737882803331, 6.817976262117185549, 54.00000000000000711 ) ) ;
#41856 = DIRECTION ( 'NONE',  ( 0.000000000000000000, 0.000000000000000000, -1.000000000000000000 ) ) ;
#41857 = VERTEX_POINT ( 'NONE', #57796 ) ;
#41858 = DIRECTION ( 'NONE',  ( 0.000000000000000000, -1.000000000000000000, -0.000000000000000000 ) ) ;
#41859 = ADVANCED_FACE ( 'NONE', ( #15375 ), #25275, .F. ) ;
#41860 = LINE ( 'NONE', #8274, #9551 ) ;
#41861 = DIRECTION ( 'NONE',  ( 0.000000000000000000, 0.000000000000000000, -1.000000000000000000 ) ) ;
#41862 = VECTOR ( 'NONE', #22876, 1000.000000000000000 ) ;
#41863 = EDGE_CURVE ( 'NONE', #3011, #41013, #3472, .T. ) ;
#41864 = CARTESIAN_POINT ( 'NONE',  ( -11.00000000000000000, -16.28999999999999915, 14.50000000000000000 ) ) ;
#41865 = EDGE_CURVE ( 'NONE', #8459, #21517, #47545, .T. ) ;
#41866 = CARTESIAN_POINT ( 'NONE',  ( 7.250000000000005329, -7.249999999999998224, -13.00000000000000178 ) ) ;
#41867 = DIRECTION ( 'NONE',  ( 0.000000000000000000, 0.000000000000000000, -1.000000000000000000 ) ) ;
#41868 = ORIENTED_EDGE ( 'NONE', *, *, #1939, .F. ) ;
#41869 = LINE ( 'NONE', #21360, #69749 ) ;
#41870 = ADVANCED_FACE ( 'NONE', ( #25987 ), #58522, .T. ) ;
#41871 = AXIS2_PLACEMENT_3D ( 'NONE', #40083, #55670, #56023 ) ;
#41872 = CARTESIAN_POINT ( 'NONE',  ( 146.5599459900709860, 5.000000000000000000, 316.5239988703752942 ) ) ;
#41873 = ADVANCED_FACE ( 'NONE', ( #53219 ), #36227, .F. ) ;
#41874 = VECTOR ( 'NONE', #7822, 1000.000000000000000 ) ;
#41875 = DIRECTION ( 'NONE',  ( -0.000000000000000000, -0.000000000000000000, -1.000000000000000000 ) ) ;
#41876 = ORIENTED_EDGE ( 'NONE', *, *, #56411, .T. ) ;
#41877 = LINE ( 'NONE', #63451, #11245 ) ;
#41878 = DIRECTION ( 'NONE',  ( 1.836970198721029934E-16, 1.836970198721010706E-16, -1.000000000000000000 ) ) ;
#41879 = CYLINDRICAL_SURFACE ( 'NONE', #10549, 0.5999999999999989786 ) ;
#41880 = DIRECTION ( 'NONE',  ( -1.000000000000000000, 9.973078850062115052E-15, -1.836970198721011692E-16 ) ) ;
#41881 = CARTESIAN_POINT ( 'NONE',  ( -6.822336235477446387, 6.350872789121265072, 26.00000000000000711 ) ) ;
#41882 = ORIENTED_EDGE ( 'NONE', *, *, #34824, .T. ) ;
#41883 = CARTESIAN_POINT ( 'NONE',  ( -11.19000000000000128, -12.00000000000000000, -5.000000000000000000 ) ) ;
#41884 = DIRECTION ( 'NONE',  ( -1.000000000000000000, 0.000000000000000000, 0.000000000000000000 ) ) ;
#41885 = EDGE_CURVE ( 'NONE', #21334, #17758, #52872, .T. ) ;
#41886 = DIRECTION ( 'NONE',  ( 0.000000000000000000, 1.000000000000000000, 0.000000000000000000 ) ) ;
#41887 = VECTOR ( 'NONE', #5473, 1000.000000000000114 ) ;
#41888 = VECTOR ( 'NONE', #25033, 1000.000000000000000 ) ;
#41889 = FACE_OUTER_BOUND ( 'NONE', #5912, .T. ) ;
#41890 = CARTESIAN_POINT ( 'NONE',  ( 7.250000000000005329, 8.250000000000001776, -9.000000000000001776 ) ) ;
#41891 = ORIENTED_EDGE ( 'NONE', *, *, #8705, .T. ) ;
#41893 = VERTEX_POINT ( 'NONE', #46359 ) ;
#41892 = CARTESIAN_POINT ( 'NONE',  ( 12.90000000000000213, -0.2000000000089119934, 8.909539772616881237E-12 ) ) ;
#41894 = AXIS2_PLACEMENT_3D ( 'NONE', #45352, #40756, #39702 ) ;
#41895 = DIRECTION ( 'NONE',  ( -1.000000000000000000, 0.000000000000000000, 0.000000000000000000 ) ) ;
#41896 = DIRECTION ( 'NONE',  ( 2.135044278125299371E-15, 1.000000000000000000, 0.000000000000000000 ) ) ;
#41897 = DIRECTION ( 'NONE',  ( -1.836970198721029934E-16, 1.836970198721036344E-16, -1.000000000000000000 ) ) ;
#41898 = VERTEX_POINT ( 'NONE', #56625 ) ;
#41899 = AXIS2_PLACEMENT_3D ( 'NONE', #12263, #33840, #6967 ) ;
#41900 = CARTESIAN_POINT ( 'NONE',  ( 8.250000000000005329, -7.249999999999998224, -24.50000000000000000 ) ) ;
#41901 = CYLINDRICAL_SURFACE ( 'NONE', #28487, 1.000000000000000000 ) ;
#41902 = ORIENTED_EDGE ( 'NONE', *, *, #60547, .F. ) ;
#41903 = ORIENTED_EDGE ( 'NONE', *, *, #31379, .F. ) ;
#41904 = EDGE_CURVE ( 'NONE', #64467, #23968, #46709, .T. ) ;
#41905 = EDGE_LOOP ( 'NONE', ( #37377, #23928, #30177, #7492 ) ) ;
#41906 = FACE_OUTER_BOUND ( 'NONE', #61872, .T. ) ;
#41907 = EDGE_CURVE ( 'NONE', #32441, #56741, #67936, .T. ) ;
#41908 = DIRECTION ( 'NONE',  ( 0.000000000000000000, 1.000000000000000000, 0.000000000000000000 ) ) ;
#41909 = DIRECTION ( 'NONE',  ( -0.000000000000000000, 3.673940397442059868E-16, -1.000000000000000000 ) ) ;
#41910 = VECTOR ( 'NONE', #5156, 1000.000000000000000 ) ;
#41911 = VERTEX_POINT ( 'NONE', #2876 ) ;
#41912 = VERTEX_POINT ( 'NONE', #8881 ) ;
#41913 = EDGE_CURVE ( 'NONE', #62767, #25535, #2184, .T. ) ;
#41914 = CARTESIAN_POINT ( 'NONE',  ( 30.00000000000000000, -16.28999999999710369, -15.00000000000794920 ) ) ;
#41915 = CARTESIAN_POINT ( 'NONE',  ( 15.50000000000000000, -0.2000000000000000111, -19.19999999702029925 ) ) ;
#41916 = ORIENTED_EDGE ( 'NONE', *, *, #53761, .T. ) ;
#41917 = EDGE_CURVE ( 'NONE', #60141, #13479, #24801, .T. ) ;
#41918 = EDGE_LOOP ( 'NONE', ( #53445, #47828, #33893, #10990 ) ) ;
#41919 = ORIENTED_EDGE ( 'NONE', *, *, #65946, .F. ) ;
#41920 = ORIENTED_EDGE ( 'NONE', *, *, #25115, .F. ) ;
#41921 = CARTESIAN_POINT ( 'NONE',  ( 38.90000000000000568, -21.00000000000001421, -13.86939075806900945 ) ) ;
#41922 = EDGE_CURVE ( 'NONE', #5458, #33631, #8174, .T. ) ;
#41923 = AXIS2_PLACEMENT_3D ( 'NONE', #28032, #31954, #11415 ) ;
#41925 = EDGE_LOOP ( 'NONE', ( #26531, #62272, #6409, #23468 ) ) ;
#41924 = DIRECTION ( 'NONE',  ( 1.836970198721029934E-16, 1.836970198721010706E-16, -1.000000000000000000 ) ) ;
#41926 = CARTESIAN_POINT ( 'NONE',  ( 275.0000000000000000, -25.69999999999924967, -14.52500000000000213 ) ) ;
#41927 = VECTOR ( 'NONE', #32638, 1000.000000000000000 ) ;
#41928 = DIRECTION ( 'NONE',  ( 0.000000000000000000, 0.000000000000000000, 1.000000000000000000 ) ) ;
#41929 = DIRECTION ( 'NONE',  ( -1.000000000000000000, 0.000000000000000000, 0.000000000000000000 ) ) ;
#41930 = VERTEX_POINT ( 'NONE', #14188 ) ;
#41931 = ADVANCED_FACE ( 'NONE', ( #24092 ), #19839, .F. ) ;
#41932 = VERTEX_POINT ( 'NONE', #14539 ) ;
#41933 = EDGE_CURVE ( 'NONE', #6920, #38565, #9242, .T. ) ;
#41935 = EDGE_CURVE ( 'NONE', #33525, #9808, #35092, .T. ) ;
#41934 = VECTOR ( 'NONE', #3275, 1000.000000000000000 ) ;
#41936 = EDGE_CURVE ( 'NONE', #14411, #30184, #45301, .T. ) ;
#41937 = VECTOR ( 'NONE', #37051, 1000.000000000000000 ) ;
#41938 = DIRECTION ( 'NONE',  ( 0.000000000000000000, 0.000000000000000000, -1.000000000000000000 ) ) ;
#41939 = CARTESIAN_POINT ( 'NONE',  ( 6.836383711242997485, 6.350872789121265960, 26.00000000000000711 ) ) ;
#41940 = ORIENTED_EDGE ( 'NONE', *, *, #48818, .T. ) ;
#41941 = VECTOR ( 'NONE', #45615, 1000.000000000000000 ) ;
#41942 = EDGE_CURVE ( 'NONE', #19212, #35877, #19141, .T. ) ;
#41943 = DIRECTION ( 'NONE',  ( -1.794541526872559352E-16, -1.000000000000000000, 0.000000000000000000 ) ) ;
#41944 = DIRECTION ( 'NONE',  ( 7.665540703601096574E-15, 1.000000000000000000, 0.000000000000000000 ) ) ;
#41945 = SURFACE_STYLE_USAGE ( .BOTH. , #20377 ) ;
#41946 = ORIENTED_EDGE ( 'NONE', *, *, #10739, .T. ) ;
#41947 = PLANE ( 'NONE',  #44425 ) ;
#41948 = CARTESIAN_POINT ( 'NONE',  ( -29.50000000000000355, -12.00000000000000000, 11.03137303340310282 ) ) ;
#41949 = VECTOR ( 'NONE', #16751, 1000.000000000000000 ) ;
#41950 = CARTESIAN_POINT ( 'NONE',  ( -5.655420232009250370, 8.393516549646600211, 455.0000000000000568 ) ) ;
#41951 = CARTESIAN_POINT ( 'NONE',  ( 23.48000000000000043, -15.50000000000000000, -26.00000000000000355 ) ) ;
#41952 = LINE ( 'NONE', #51515, #12751 ) ;
#41953 = EDGE_LOOP ( 'NONE', ( #539, #39958, #9228, #12723 ) ) ;
#41954 = CARTESIAN_POINT ( 'NONE',  ( 3.157023737882809655, -6.501044194225480410, 54.00000000000000711 ) ) ;
#41955 = CARTESIAN_POINT ( 'NONE',  ( 8.250000000000005329, 0.000000000000000000, -12.50000000000000000 ) ) ;
#41956 = EDGE_CURVE ( 'NONE', #20447, #46212, #61561, .T. ) ;
#41957 = CARTESIAN_POINT ( 'NONE',  ( 0.000000000000000000, 17.79289321881345032, 20.50000000000000000 ) ) ;
#41958 = CARTESIAN_POINT ( 'NONE',  ( -8.393516549646744096, -4.396432944014549093, 455.0000000000000568 ) ) ;
#41959 = EDGE_CURVE ( 'NONE', #34744, #61431, #18790, .T. ) ;
#41960 = VECTOR ( 'NONE', #3322, 1000.000000000000000 ) ;
#41961 = CARTESIAN_POINT ( 'NONE',  ( -11.11351654964671098, 4.193516549646605363, 455.0000000000000568 ) ) ;
#41962 = DIRECTION ( 'NONE',  ( 1.000000000000000000, -0.000000000000000000, -0.000000000000000000 ) ) ;
#41963 = DIRECTION ( 'NONE',  ( 0.000000000000000000, 0.000000000000000000, 1.000000000000000000 ) ) ;
#41964 = CARTESIAN_POINT ( 'NONE',  ( 41.09999999999999432, -0.2000000000000000111, 0.000000000000000000 ) ) ;
#41965 = ORIENTED_EDGE ( 'NONE', *, *, #41602, .T. ) ;
#41966 = DIRECTION ( 'NONE',  ( 1.000000000000000000, 0.000000000000000000, 0.000000000000000000 ) ) ;
#41967 = DIRECTION ( 'NONE',  ( 0.000000000000000000, 0.000000000000000000, -1.000000000000000000 ) ) ;
#41968 = CYLINDRICAL_SURFACE ( 'NONE', #44703, 0.2000000000000005107 ) ;
#41969 = PLANE ( 'NONE',  #33405 ) ;
#41970 = LINE ( 'NONE', #62840, #27651 ) ;
#41971 = DIRECTION ( 'NONE',  ( -0.000000000000000000, 3.673940397442059868E-16, -1.000000000000000000 ) ) ;
#41972 = FACE_OUTER_BOUND ( 'NONE', #59417, .T. ) ;
#41973 = AXIS2_PLACEMENT_3D ( 'NONE', #48132, #37182, #58741 ) ;
#41974 = ORIENTED_EDGE ( 'NONE', *, *, #6043, .T. ) ;
#41975 = COLOUR_RGB ( '', 0.66274510, 0.83137255, 0.94901961) ;
#41976 = ORIENTED_EDGE ( 'NONE', *, *, #113, .T. ) ;
#41977 = FACE_OUTER_BOUND ( 'NONE', #2005, .T. ) ;
#41978 = CARTESIAN_POINT ( 'NONE',  ( -14.45366306705349757, -0.2717122460102549542, 23.33927276307431242 ) ) ;
#41979 = ORIENTED_EDGE ( 'NONE', *, *, #26676, .F. ) ;
#41980 = DIRECTION ( 'NONE',  ( 1.000000000000000000, 0.000000000000000000, 0.000000000000000000 ) ) ;
#41981 = LINE ( 'NONE', #63200, #43095 ) ;
#41982 = ORIENTED_EDGE ( 'NONE', *, *, #5594, .F. ) ;
#41983 = AXIS2_PLACEMENT_3D ( 'NONE', #3803, #61173, #50587 ) ;
#41984 = AXIS2_PLACEMENT_3D ( 'NONE', #3195, #8837, #36407 ) ;
#41985 = CARTESIAN_POINT ( 'NONE',  ( 16.75000000000000000, -2.500000000000000000, 21.77831216351300014 ) ) ;
#41986 = ORIENTED_EDGE ( 'NONE', *, *, #28057, .F. ) ;
#41987 = ORIENTED_EDGE ( 'NONE', *, *, #58330, .T. ) ;
#41988 = CARTESIAN_POINT ( 'NONE',  ( 4.149127210878726046, 6.822336235477391320, 54.00000000000000711 ) ) ;
#41989 = EDGE_LOOP ( 'NONE', ( #6000, #40689, #3966, #4242, #51364, #56159 ) ) ;
#41990 = AXIS2_PLACEMENT_3D ( 'NONE', #20508, #62233, #41720 ) ;
#41991 = EDGE_CURVE ( 'NONE', #18752, #288, #29395, .T. ) ;
#41992 = LINE ( 'NONE', #10166, #57571 ) ;
#41993 = DIRECTION ( 'NONE',  ( -1.000000000000000000, 8.728482790395504563E-15, 0.000000000000000000 ) ) ;
#41994 = CARTESIAN_POINT ( 'NONE',  ( -4.383466043307968185, -8.406483450353443132, 455.0000000000000568 ) ) ;
#41995 = VERTEX_POINT ( 'NONE', #56961 ) ;
#41996 = ADVANCED_FACE ( 'NONE', ( #8523 ), #50969, .F. ) ;
#41997 = CARTESIAN_POINT ( 'NONE',  ( 11.25000000000000000, 11.18999999999999950, -4.250000000000000000 ) ) ;
#41998 = CIRCLE ( 'NONE', #20548, 0.9999999999999991118 ) ;
#42000 = CARTESIAN_POINT ( 'NONE',  ( -1.620245201994368500, -8.241237374594323484, 26.00000000000000711 ) ) ;
#41999 = CARTESIAN_POINT ( 'NONE',  ( 35.89999999999999858, -14.06939075806902117, -20.80000000000000426 ) ) ;
#42001 = ORIENTED_EDGE ( 'NONE', *, *, #15016, .T. ) ;
#42002 = ORIENTED_EDGE ( 'NONE', *, *, #51636, .F. ) ;
#42003 = ADVANCED_FACE ( 'NONE', ( #13128 ), #25153, .F. ) ;
#42004 = EDGE_LOOP ( 'NONE', ( #10429, #33993 ) ) ;
#42005 = EDGE_CURVE ( 'NONE', #59475, #35467, #61924, .T. ) ;
#42006 = ORIENTED_EDGE ( 'NONE', *, *, #64279, .F. ) ;
#42007 = EDGE_CURVE ( 'NONE', #2806, #31244, #13483, .T. ) ;
#42008 = ADVANCED_FACE ( 'NONE', ( #9953 ), #37515, .F. ) ;
#42009 = CARTESIAN_POINT ( 'NONE',  ( -29.50000000000000355, -11.50000000000100009, -15.00000000000084910 ) ) ;
#42011 = ORIENTED_EDGE ( 'NONE', *, *, #30659, .F. ) ;
#42010 = CARTESIAN_POINT ( 'NONE',  ( -3.650476262117223314, 10.30047626211716683, 54.00000000000000711 ) ) ;
#42012 = FACE_OUTER_BOUND ( 'NONE', #45177, .T. ) ;
#42013 = CARTESIAN_POINT ( 'NONE',  ( -25.50000000000000355, -5.200000000000001066, 22.50000000000000000 ) ) ;
#42014 = VECTOR ( 'NONE', #19127, 1000.000000000000000 ) ;
#42015 = ORIENTED_EDGE ( 'NONE', *, *, #23743, .T. ) ;
#42016 = ORIENTED_EDGE ( 'NONE', *, *, #21423, .F. ) ;
#42017 = CARTESIAN_POINT ( 'NONE',  ( 6.836383711243005479, -6.364920264886905876, 54.00000000000000711 ) ) ;
#42018 = AXIS2_PLACEMENT_3D ( 'NONE', #66030, #5961, #54748 ) ;
#42019 = VERTEX_POINT ( 'NONE', #68645 ) ;
#42020 = CARTESIAN_POINT ( 'NONE',  ( -3.842976262117221875, 10.30047626211716860, 54.00000000000000711 ) ) ;
#42021 = DIRECTION ( 'NONE',  ( 0.000000000000000000, -1.000000000000000000, 0.000000000000000000 ) ) ;
#42022 = CARTESIAN_POINT ( 'NONE',  ( 3.664523737882778853, -10.50702373788280219, 26.00000000000000000 ) ) ;
#42023 = VECTOR ( 'NONE', #31789, 1000.000000000000000 ) ;
#42024 = EDGE_LOOP ( 'NONE', ( #22087, #14281, #63987, #35713 ) ) ;
#42025 = DIRECTION ( 'NONE',  ( -1.000000000000000000, 2.602085213965213008E-15, 0.000000000000000000 ) ) ;
#42026 = CARTESIAN_POINT ( 'NONE',  ( -30.00000000000000000, -11.50000000000100009, -15.00000000000084910 ) ) ;
#42028 = VERTEX_POINT ( 'NONE', #31521 ) ;
#42027 = DIRECTION ( 'NONE',  ( 0.000000000000000000, 0.000000000000000000, -1.000000000000000000 ) ) ;
#42030 = VERTEX_POINT ( 'NONE', #21599 ) ;
#42029 = CARTESIAN_POINT ( 'NONE',  ( 9.703773737882817940, 10.03972626211715280, 54.00000000000000711 ) ) ;
#42031 = AXIS2_PLACEMENT_3D ( 'NONE', #61904, #56598, #33974 ) ;
#42032 = CARTESIAN_POINT ( 'NONE',  ( -7.250000000000000888, 8.250000000000001776, -14.50000000000000000 ) ) ;
#42033 = CARTESIAN_POINT ( 'NONE',  ( 7.000000000000000000, -39.80000000000000426, -8.400000000000000355 ) ) ;
#42034 = DIRECTION ( 'NONE',  ( -1.000000000000000000, 0.000000000000000000, 0.000000000000000000 ) ) ;
#42035 = AXIS2_PLACEMENT_3D ( 'NONE', #60675, #594, #12565 ) ;
#42036 = CARTESIAN_POINT ( 'NONE',  ( 7.616533956692198792, 8.593516549646622593, 195.0000000000000284 ) ) ;
#42037 = CARTESIAN_POINT ( 'NONE',  ( 4.406483450353335662, -11.78648345035337996, 195.0000000000000284 ) ) ;
#42038 = ORIENTED_EDGE ( 'NONE', *, *, #55981, .T. ) ;
#42039 = CARTESIAN_POINT ( 'NONE',  ( -11.47551654964683010, -11.08848345035333338, 455.0000000000000568 ) ) ;
#42040 = DIRECTION ( 'NONE',  ( 0.000000000000000000, -1.000000000000000000, 0.000000000000000000 ) ) ;
#42042 = VERTEX_POINT ( 'NONE', #14898 ) ;
#42041 = LINE ( 'NONE', #16216, #36750 ) ;
#42043 = EDGE_CURVE ( 'NONE', #16486, #57476, #42808, .T. ) ;
#42044 = CARTESIAN_POINT ( 'NONE',  ( -3.142976262117251451, 6.486996718459839606, 26.00000000000000711 ) ) ;
#42045 = VECTOR ( 'NONE', #34560, 1000.000000000000000 ) ;
#42046 = ADVANCED_FACE ( 'NONE', ( #5349 ), #47072, .T. ) ;
#42047 = CARTESIAN_POINT ( 'NONE',  ( 7.250000000000005329, -7.449999999999998401, -13.50000000000000178 ) ) ;
#42048 = VECTOR ( 'NONE', #61065, 1000.000000000000000 ) ;
#42049 = CARTESIAN_POINT ( 'NONE',  ( 106.4257688009193430, 10.00000000000000000, 330.9830310981789694 ) ) ;
#42050 = VERTEX_POINT ( 'NONE', #47412 ) ;
#42051 = CARTESIAN_POINT ( 'NONE',  ( 25.50000000000000355, -5.200000000000001066, -22.50000000000000000 ) ) ;
#42052 = CARTESIAN_POINT ( 'NONE',  ( 7.000000000000000000, -38.15000000000000568, 13.19999999999999929 ) ) ;
#42054 = ORIENTED_EDGE ( 'NONE', *, *, #67843, .F. ) ;
#42053 = ADVANCED_FACE ( 'NONE', ( #68984 ), #36823, .F. ) ;
#42055 = PRESENTATION_STYLE_ASSIGNMENT (( #36398 ) ) ;
#42056 = EDGE_CURVE ( 'NONE', #29117, #7067, #58022, .T. ) ;
#42057 = DIRECTION ( 'NONE',  ( 3.540251991789408222E-15, 1.000000000000000000, 0.000000000000000000 ) ) ;
#42058 = CARTESIAN_POINT ( 'NONE',  ( 8.250000000000005329, 8.250000000000001776, -26.00000000000001066 ) ) ;
#42059 = DIRECTION ( 'NONE',  ( 0.7671651518153131954, 0.6414496315691415873, 2.587583378555109562E-16 ) ) ;
#42060 = DIRECTION ( 'NONE',  ( 0.000000000000000000, 1.000000000000000000, 0.000000000000000000 ) ) ;
#42061 = EDGE_LOOP ( 'NONE', ( #58868, #21698, #21752, #29442 ) ) ;
#42062 = ORIENTED_EDGE ( 'NONE', *, *, #52223, .T. ) ;
#42063 = DIRECTION ( 'NONE',  ( -7.665540703601094997E-15, -1.000000000000000000, 0.000000000000000000 ) ) ;
#42064 = EDGE_LOOP ( 'NONE', ( #24445, #22179, #20951, #21194 ) ) ;
#42065 = ORIENTED_EDGE ( 'NONE', *, *, #45856, .T. ) ;
#42066 = LINE ( 'NONE', #35700, #30278 ) ;
#42067 = AXIS2_PLACEMENT_3D ( 'NONE', #44376, #21444, #1268 ) ;
#42068 = DIRECTION ( 'NONE',  ( 0.000000000000000000, 1.000000000000000000, -0.000000000000000000 ) ) ;
#42069 = DIRECTION ( 'NONE',  ( 1.000000000000000000, -0.000000000000000000, 0.000000000000000000 ) ) ;
#42070 = VERTEX_POINT ( 'NONE', #48467 ) ;
#42071 = ORIENTED_EDGE ( 'NONE', *, *, #60603, .T. ) ;
#42072 = VECTOR ( 'NONE', #38389, 1000.000000000000000 ) ;
#42073 = DIRECTION ( 'NONE',  ( -0.000000000000000000, -0.000000000000000000, -1.000000000000000000 ) ) ;
#42074 = VERTEX_POINT ( 'NONE', #48123 ) ;
#42075 = ORIENTED_EDGE ( 'NONE', *, *, #6233, .F. ) ;
#42076 = ADVANCED_FACE ( 'NONE', ( #4306 ), #3941, .F. ) ;
#42077 = CARTESIAN_POINT ( 'NONE',  ( 7.357023737882817827, -5.552858015815587578, 54.00000000000000711 ) ) ;
#42078 = CARTESIAN_POINT ( 'NONE',  ( -7.250000000000001776, -7.249999999999998224, -26.00000000000001066 ) ) ;
#42079 = CARTESIAN_POINT ( 'NONE',  ( 4.206483450353343478, -11.12648345035347575, 455.0000000000000568 ) ) ;
#42080 = ORIENTED_EDGE ( 'NONE', *, *, #36737, .T. ) ;
#42081 = AXIS2_PLACEMENT_3D ( 'NONE', #10269, #32544, #38531 ) ;
#42082 = CARTESIAN_POINT ( 'NONE',  ( 17.89999999999999858, -0.2000000000089119934, 8.909539772616881237E-12 ) ) ;
#42084 = FACE_OUTER_BOUND ( 'NONE', #32915, .T. ) ;
#42083 = CARTESIAN_POINT ( 'NONE',  ( 11.18999999999999950, 12.00000000000000178, 0.000000000000000000 ) ) ;
#42085 = VERTEX_POINT ( 'NONE', #10627 ) ;
#42087 = ORIENTED_EDGE ( 'NONE', *, *, #1712, .T. ) ;
#42086 = CARTESIAN_POINT ( 'NONE',  ( 47.00000000000000000, 0.000000000000000000, 0.000000000000000000 ) ) ;
#42088 = ORIENTED_EDGE ( 'NONE', *, *, #35976, .F. ) ;
#42089 = EDGE_CURVE ( 'NONE', #47121, #11595, #56557, .T. ) ;
#42090 = EDGE_CURVE ( 'NONE', #62566, #5332, #1204, .T. ) ;
#42091 = DIRECTION ( 'NONE',  ( 1.836970198721029934E-16, -1.836970198721036344E-16, 1.000000000000000000 ) ) ;
#42092 = DIRECTION ( 'NONE',  ( 1.000000000000000000, -5.981805089575194965E-17, 0.000000000000000000 ) ) ;
#42093 = AXIS2_PLACEMENT_3D ( 'NONE', #66244, #17806, #28077 ) ;
#42094 = ADVANCED_FACE ( 'NONE', ( #37 ), #20193, .F. ) ;
#42095 = ORIENTED_EDGE ( 'NONE', *, *, #1620, .T. ) ;
#42096 = AXIS2_PLACEMENT_3D ( 'NONE', #42305, #14744, #36304 ) ;
#42098 = CARTESIAN_POINT ( 'NONE',  ( 7.606483450353420217, 11.31351654964657349, 455.0000000000000568 ) ) ;
#42097 = VECTOR ( 'NONE', #52017, 1000.000000000000000 ) ;
#42099 = CARTESIAN_POINT ( 'NONE',  ( -11.50000000000000000, -11.70000000000012008, -10.70000000000011831 ) ) ;
#42100 = ORIENTED_EDGE ( 'NONE', *, *, #13767, .F. ) ;
#42101 = ORIENTED_EDGE ( 'NONE', *, *, #49322, .F. ) ;
#42102 = CARTESIAN_POINT ( 'NONE',  ( 6.832023737882818359, -9.737023737882822161, 54.00000000000000711 ) ) ;
#42103 = AXIS2_PLACEMENT_3D ( 'NONE', #36381, #57948, #9517 ) ;
#42104 = DIRECTION ( 'NONE',  ( 0.000000000000000000, 1.000000000000000000, 0.000000000000000000 ) ) ;
#42105 = ORIENTED_EDGE ( 'NONE', *, *, #5492, .F. ) ;
#42106 = VECTOR ( 'NONE', #35037, 1000.000000000000000 ) ;
#42107 = CARTESIAN_POINT ( 'NONE',  ( 151.5599459900709860, 9.000000000000001776, 280.6301873289890523 ) ) ;
#42108 = LINE ( 'NONE', #16282, #19256 ) ;
#42109 = VERTEX_POINT ( 'NONE', #20892 ) ;
#42111 = ORIENTED_EDGE ( 'NONE', *, *, #16872, .F. ) ;
#42110 = FACE_BOUND ( 'NONE', #62980, .T. ) ;
#42112 = LINE ( 'NONE', #14904, #48637 ) ;
#42113 = DIRECTION ( 'NONE',  ( 0.000000000000000000, 0.000000000000000000, 1.000000000000000000 ) ) ;
#42114 = FACE_BOUND ( 'NONE', #58892, .T. ) ;
#42115 = CARTESIAN_POINT ( 'NONE',  ( -7.250000000000000000, -7.449999999999998401, -19.50000000000000000 ) ) ;
#42116 = DIRECTION ( 'NONE',  ( 0.000000000000000000, -3.673940397442059868E-16, 1.000000000000000000 ) ) ;
#42117 = DIRECTION ( 'NONE',  ( 0.000000000000000000, -1.000000000000000000, 0.000000000000000000 ) ) ;
#42118 = ORIENTED_EDGE ( 'NONE', *, *, #27654, .T. ) ;
#42119 = LINE ( 'NONE', #68998, #60894 ) ;
#42121 = EDGE_LOOP ( 'NONE', ( #43670, #26985, #18818, #23740 ) ) ;
#42120 = FILL_AREA_STYLE ('',( #20560 ) ) ;
#42122 = FACE_OUTER_BOUND ( 'NONE', #9732, .T. ) ;
#42123 = CYLINDRICAL_SURFACE ( 'NONE', #10936, 1.224999999999999423 ) ;
#42124 = DIRECTION ( 'NONE',  ( 0.000000000000000000, 0.000000000000000000, -1.000000000000000000 ) ) ;
#42125 = CIRCLE ( 'NONE', #51148, 24.99999999998784972 ) ;
#42126 = EDGE_CURVE ( 'NONE', #22030, #13975, #32203, .T. ) ;
#42127 = LINE ( 'NONE', #38238, #11495 ) ;
#42128 = EDGE_CURVE ( 'NONE', #20150, #48411, #42108, .T. ) ;
#42129 = EDGE_CURVE ( 'NONE', #48034, #4220, #21255, .T. ) ;
#42130 = VERTEX_POINT ( 'NONE', #64050 ) ;
#42131 = FACE_OUTER_BOUND ( 'NONE', #653, .T. ) ;
#42132 = LINE ( 'NONE', #21628, #17052 ) ;
#42134 = VERTEX_POINT ( 'NONE', #52746 ) ;
#42133 = ADVANCED_FACE ( 'NONE', ( #15609 ), #59427, .T. ) ;
#42135 = DIRECTION ( 'NONE',  ( 1.000000000000000000, 0.000000000000000000, 0.000000000000000000 ) ) ;
#42136 = DIRECTION ( 'NONE',  ( -1.000000000000000000, 0.000000000000000000, 0.000000000000000000 ) ) ;
#42137 = FACE_OUTER_BOUND ( 'NONE', #41296, .T. ) ;
#42138 = VECTOR ( 'NONE', #2150, 1000.000000000000000 ) ;
#42139 = ORIENTED_EDGE ( 'NONE', *, *, #24114, .F. ) ;
#42140 = DIRECTION ( 'NONE',  ( 0.000000000000000000, -3.673940397442059868E-16, 1.000000000000000000 ) ) ;
#42141 = VERTEX_POINT ( 'NONE', #53432 ) ;
#42142 = ORIENTED_EDGE ( 'NONE', *, *, #36968, .F. ) ;
#42143 = VECTOR ( 'NONE', #36049, 1000.000000000000000 ) ;
#42144 = DIRECTION ( 'NONE',  ( 0.000000000000000000, 0.000000000000000000, -1.000000000000000000 ) ) ;
#42145 = DIRECTION ( 'NONE',  ( -0.000000000000000000, -0.000000000000000000, -1.000000000000000000 ) ) ;
#42146 = DIRECTION ( 'NONE',  ( 0.000000000000000000, 0.000000000000000000, 1.000000000000000000 ) ) ;
#42147 = AXIS2_PLACEMENT_3D ( 'NONE', #42316, #63896, #53990 ) ;
#42148 = VECTOR ( 'NONE', #32964, 1000.000000000000000 ) ;
#42149 = CARTESIAN_POINT ( 'NONE',  ( -1.466476262117230034, 9.390476262117152473, 26.00000000000000711 ) ) ;
#42150 = VECTOR ( 'NONE', #67060, 1000.000000000000114 ) ;
#42151 = AXIS2_PLACEMENT_3D ( 'NONE', #53621, #5871, #58578 ) ;
#42152 = LINE ( 'NONE', #46402, #23905 ) ;
#42153 = VERTEX_POINT ( 'NONE', #33915 ) ;
#42154 = VERTEX_POINT ( 'NONE', #22632 ) ;
#42156 = ORIENTED_EDGE ( 'NONE', *, *, #18541, .T. ) ;
#42155 = CARTESIAN_POINT ( 'NONE',  ( 283.0000000000000568, -38.15000000000000568, -14.50000000000000000 ) ) ;
#42157 = ORIENTED_EDGE ( 'NONE', *, *, #9285, .T. ) ;
#42158 = CARTESIAN_POINT ( 'NONE',  ( 7.000000000000000000, -42.00000000000000000, -7.000000000000000000 ) ) ;
#42159 = CARTESIAN_POINT ( 'NONE',  ( 9.417013320880768035, 1.853252480934615809, 455.0000000000000568 ) ) ;
#42160 = CARTESIAN_POINT ( 'NONE',  ( -9.791916549646867196, -11.08848345035335115, 455.0000000000000568 ) ) ;
#42161 = LINE ( 'NONE', #31574, #6307 ) ;
#42163 = CARTESIAN_POINT ( 'NONE',  ( -8.250000000000001776, 0.000000000000000000, -25.00000000000000000 ) ) ;
#42162 = LINE ( 'NONE', #31232, #34309 ) ;
#42164 = VERTEX_POINT ( 'NONE', #7043 ) ;
#42165 = EDGE_LOOP ( 'NONE', ( #63064, #69622, #52059, #16695, #31853, #56915, #7584, #14727 ) ) ;
#42166 = EDGE_LOOP ( 'NONE', ( #46428, #52846 ) ) ;
#42167 = CARTESIAN_POINT ( 'NONE',  ( 7.000000000000000000, -17.00000000000000000, 0.000000000000000000 ) ) ;
#42168 = AXIS2_PLACEMENT_3D ( 'NONE', #35590, #51164, #19336 ) ;
#42169 = LINE ( 'NONE', #40779, #17396 ) ;
#42170 = EDGE_CURVE ( 'NONE', #19296, #6331, #54474, .T. ) ;
#42171 = DIRECTION ( 'NONE',  ( 1.004751837285766511E-14, -1.000000000000000000, 0.000000000000000000 ) ) ;
#42172 = DIRECTION ( 'NONE',  ( 0.8660254037844482555, 0.000000000000000000, 0.4999999999999831801 ) ) ;
#42173 = EDGE_CURVE ( 'NONE', #68953, #35394, #54814, .T. ) ;
#42174 = ORIENTED_EDGE ( 'NONE', *, *, #40199, .F. ) ;
#42175 = ORIENTED_EDGE ( 'NONE', *, *, #34401, .F. ) ;
#42176 = EDGE_CURVE ( 'NONE', #6834, #14797, #20425, .T. ) ;
#42177 = VERTEX_POINT ( 'NONE', #18003 ) ;
#42178 = DIRECTION ( 'NONE',  ( 1.836970198721029934E-16, 1.836970198721010706E-16, -1.000000000000000000 ) ) ;
#42179 = EDGE_LOOP ( 'NONE', ( #67207, #53532, #29992, #22237 ) ) ;
#42180 = EDGE_CURVE ( 'NONE', #8072, #51926, #61128, .T. ) ;
#42181 = LINE ( 'NONE', #14274, #14170 ) ;
#42183 = ORIENTED_EDGE ( 'NONE', *, *, #66985, .F. ) ;
#42182 = PRODUCT_RELATED_PRODUCT_CATEGORY ( 'part', '', ( #8578 ) ) ;
#42184 = VERTEX_POINT ( 'NONE', #12001 ) ;
#42185 = FACE_OUTER_BOUND ( 'NONE', #10564, .T. ) ;
#42186 = EDGE_CURVE ( 'NONE', #17826, #62241, #60448, .T. ) ;
#42188 = ORIENTED_EDGE ( 'NONE', *, *, #50946, .F. ) ;
#42187 = DIRECTION ( 'NONE',  ( -0.000000000000000000, -0.000000000000000000, -1.000000000000000000 ) ) ;
#42190 = EDGE_LOOP ( 'NONE', ( #49635, #13338, #40943, #50009 ) ) ;
#42189 = EDGE_CURVE ( 'NONE', #22125, #21000, #733, .T. ) ;
#42191 = VECTOR ( 'NONE', #49530, 1000.000000000000000 ) ;
#42193 = CARTESIAN_POINT ( 'NONE',  ( 27.90000000000000213, -14.06939075806900874, 20.80000000000001137 ) ) ;
#42192 = CIRCLE ( 'NONE', #1500, 4.000000000000000000 ) ;
#42194 = DIRECTION ( 'NONE',  ( -1.062171939662868249E-14, -1.000000000000000000, 0.000000000000000000 ) ) ;
#42196 = ORIENTED_EDGE ( 'NONE', *, *, #66004, .T. ) ;
#42195 = FACE_OUTER_BOUND ( 'NONE', #2746, .T. ) ;
#42198 = ORIENTED_EDGE ( 'NONE', *, *, #42746, .T. ) ;
#42197 = VECTOR ( 'NONE', #15199, 1000.000000000000000 ) ;
#42199 = DIRECTION ( 'NONE',  ( 0.000000000000000000, 0.000000000000000000, 1.000000000000000000 ) ) ;
#42200 = DIRECTION ( 'NONE',  ( -0.000000000000000000, 3.673940397442059868E-16, -1.000000000000000000 ) ) ;
#42201 = AXIS2_PLACEMENT_3D ( 'NONE', #16714, #49240, #28684 ) ;
#42202 = CARTESIAN_POINT ( 'NONE',  ( 41.09999999999999432, 13.66939075806899950, -20.80000000000000426 ) ) ;
#42203 = CARTESIAN_POINT ( 'NONE',  ( -6.892329165594001772, 4.459829165593958145, 26.00000000000000711 ) ) ;
#42204 = CARTESIAN_POINT ( 'NONE',  ( 8.250000000000005329, 7.250000000000000888, -17.50000000000000000 ) ) ;
#42205 = AXIS2_PLACEMENT_3D ( 'NONE', #25786, #37779, #36376 ) ;
#42206 = AXIS2_PLACEMENT_3D ( 'NONE', #27306, #48519, #65812 ) ;
#42207 = VECTOR ( 'NONE', #39310, 1000.000000000000000 ) ;
#42208 = ORIENTED_EDGE ( 'NONE', *, *, #13666, .F. ) ;
#42209 = LINE ( 'NONE', #13147, #63133 ) ;
#42210 = ORIENTED_EDGE ( 'NONE', *, *, #44430, .F. ) ;
#42211 = CARTESIAN_POINT ( 'NONE',  ( -10.91351654964670992, -2.706483450353338593, 455.0000000000000568 ) ) ;
#42212 = PLANE ( 'NONE',  #60535 ) ;
#42213 = CARTESIAN_POINT ( 'NONE',  ( 289.5000000000001705, 6.039613253960851580E-14, 26.49999999999996092 ) ) ;
#42214 = CARTESIAN_POINT ( 'NONE',  ( 277.3542486889354564, -25.50000000000000355, 17.00000000000000000 ) ) ;
#42215 = CARTESIAN_POINT ( 'NONE',  ( 23.90000000000000213, -14.06939075806902117, -20.80000000000000426 ) ) ;
#42216 = ORIENTED_EDGE ( 'NONE', *, *, #60722, .T. ) ;
#42217 =( NAMED_UNIT ( * ) SI_UNIT ( $, .STERADIAN. ) SOLID_ANGLE_UNIT ( ) );
#42218 = LINE ( 'NONE', #41872, #60469 ) ;
#42219 = DIRECTION ( 'NONE',  ( 0.000000000000000000, 0.000000000000000000, -1.000000000000000000 ) ) ;
#42220 = ORIENTED_EDGE ( 'NONE', *, *, #448, .F. ) ;
#42221 = DIRECTION ( 'NONE',  ( 0.000000000000000000, 0.000000000000000000, -1.000000000000000000 ) ) ;
#42222 = PLANE ( 'NONE',  #8289 ) ;
#42223 = PLANE ( 'NONE',  #36491 ) ;
#42224 = CIRCLE ( 'NONE', #11727, 1.929199999999997139 ) ;
#42225 = CARTESIAN_POINT ( 'NONE',  ( 12.00648345035338060, -7.826483450353491023, 455.0000000000000568 ) ) ;
#42226 = DIRECTION ( 'NONE',  ( -1.000000000000000000, 0.000000000000000000, 0.000000000000000000 ) ) ;
#42228 = ORIENTED_EDGE ( 'NONE', *, *, #51825, .T. ) ;
#42227 = ADVANCED_FACE ( 'NONE', ( #17313 ), #27587, .T. ) ;
#42229 = FACE_OUTER_BOUND ( 'NONE', #47406, .T. ) ;
#42230 = FACE_BOUND ( 'NONE', #46103, .T. ) ;
#42231 = AXIS2_PLACEMENT_3D ( 'NONE', #21205, #16589, #65028 ) ;
#42232 = CARTESIAN_POINT ( 'NONE',  ( 41.09999999999999432, 13.66939075806899950, -20.80000000000000426 ) ) ;
#42233 = DIRECTION ( 'NONE',  ( 0.7071067811865401342, -0.7071067811865550112, -1.355854680848614216E-30 ) ) ;
#42234 = EDGE_CURVE ( 'NONE', #23727, #25048, #63330, .T. ) ;
#42235 = CARTESIAN_POINT ( 'NONE',  ( -6.749999999999998224, -7.348062532927999158, 0.000000000000000000 ) ) ;
#42236 = VERTEX_POINT ( 'NONE', #32563 ) ;
#42238 = ORIENTED_EDGE ( 'NONE', *, *, #41393, .T. ) ;
#42237 = DIRECTION ( 'NONE',  ( 0.000000000000000000, 0.000000000000000000, 1.000000000000000000 ) ) ;
#42239 = AXIS2_PLACEMENT_3D ( 'NONE', #32010, #42953, #64537 ) ;
#42240 = CARTESIAN_POINT ( 'NONE',  ( -11.50000000000000000, -15.46862696659690073, -14.50000000000000000 ) ) ;
#42241 = DIRECTION ( 'NONE',  ( -0.000000000000000000, -0.000000000000000000, -1.000000000000000000 ) ) ;
#42242 = CARTESIAN_POINT ( 'NONE',  ( -8.689999999999999503, 9.750000000000001776, -7.000000000000000000 ) ) ;
#42244 = ORIENTED_EDGE ( 'NONE', *, *, #10733, .T. ) ;
#42243 = EDGE_CURVE ( 'NONE', #69426, #37400, #38552, .T. ) ;
#42245 = PRESENTATION_STYLE_ASSIGNMENT (( #52520 ) ) ;
#42246 = VECTOR ( 'NONE', #20584, 1000.000000000000000 ) ;
#42247 = LINE ( 'NONE', #63828, #35239 ) ;
#42248 = VECTOR ( 'NONE', #2447, 1000.000000000000000 ) ;
#42249 = ORIENTED_EDGE ( 'NONE', *, *, #35866, .T. ) ;
#42250 = ORIENTED_EDGE ( 'NONE', *, *, #62662, .T. ) ;
#42251 = EDGE_CURVE ( 'NONE', #3076, #69116, #65425, .T. ) ;
#42253 = ORIENTED_EDGE ( 'NONE', *, *, #66819, .T. ) ;
#42252 = CIRCLE ( 'NONE', #5014, 3.300000002979700753 ) ;
#42254 = DIRECTION ( 'NONE',  ( 0.000000000000000000, 0.000000000000000000, -1.000000000000000000 ) ) ;
#42255 = DIRECTION ( 'NONE',  ( 0.000000000000000000, 1.000000000000000000, 0.000000000000000000 ) ) ;
#42256 = DIRECTION ( 'NONE',  ( 0.000000000000000000, 0.000000000000000000, -1.000000000000000000 ) ) ;
#42257 = AXIS2_PLACEMENT_3D ( 'NONE', #61391, #3077, #51509 ) ;
#42258 = EDGE_CURVE ( 'NONE', #33149, #27652, #11654, .T. ) ;
#42259 = ORIENTED_EDGE ( 'NONE', *, *, #59149, .F. ) ;
#42260 = ORIENTED_EDGE ( 'NONE', *, *, #51890, .T. ) ;
#42261 = VECTOR ( 'NONE', #66504, 1000.000000000000000 ) ;
#42262 = DIRECTION ( 'NONE',  ( -1.000000000000000000, 0.000000000000000000, 0.000000000000000000 ) ) ;
#42263 = ORIENTED_EDGE ( 'NONE', *, *, #46614, .F. ) ;
#42264 = VERTEX_POINT ( 'NONE', #27936 ) ;
#42265 = ORIENTED_EDGE ( 'NONE', *, *, #27163, .T. ) ;
#42266 = ORIENTED_EDGE ( 'NONE', *, *, #10649, .F. ) ;
#42267 = DIRECTION ( 'NONE',  ( -1.000000000000000000, 0.000000000000000000, 0.000000000000000000 ) ) ;
#42268 = UNCERTAINTY_MEASURE_WITH_UNIT (LENGTH_MEASURE( 1.000000000000000082E-05 ), #31322, 'distance_accuracy_value', 'NONE');
#42269 = EDGE_CURVE ( 'NONE', #41366, #4835, #12481, .T. ) ;
#42271 = ORIENTED_EDGE ( 'NONE', *, *, #28973, .F. ) ;
#42270 = LINE ( 'NONE', #36270, #67211 ) ;
#42272 = EDGE_CURVE ( 'NONE', #24688, #26801, #65598, .T. ) ;
#42273 = FACE_OUTER_BOUND ( 'NONE', #68160, .T. ) ;
#42274 = DIRECTION ( 'NONE',  ( 0.000000000000000000, 1.000000000000000000, 0.000000000000000000 ) ) ;
#42275 = DIRECTION ( 'NONE',  ( 1.000000000000000000, 0.000000000000000000, 0.000000000000000000 ) ) ;
#42276 = ORIENTED_EDGE ( 'NONE', *, *, #9444, .T. ) ;
#42277 = AXIS2_PLACEMENT_3D ( 'NONE', #50588, #45976, #8845 ) ;
#42278 = ORIENTED_EDGE ( 'NONE', *, *, #61698, .T. ) ;
#42279 = AXIS2_PLACEMENT_3D ( 'NONE', #42058, #63636, #14130 ) ;
#42280 = CARTESIAN_POINT ( 'NONE',  ( -6.344366288193410419, 4.706725378239148050, 54.00000000000000711 ) ) ;
#42281 = CARTESIAN_POINT ( 'NONE',  ( -8.250000000000001776, 7.250000000000000888, -13.50000000000000178 ) ) ;
#42282 = ORIENTED_EDGE ( 'NONE', *, *, #1989, .T. ) ;
#42283 = VECTOR ( 'NONE', #61692, 1000.000000000000000 ) ;
#42284 = AXIS2_PLACEMENT_3D ( 'NONE', #32962, #26970, #5048 ) ;
#42285 = CARTESIAN_POINT ( 'NONE',  ( 29.25000000000000000, -5.000000000000000000, 26.25000000000000000 ) ) ;
#42286 = DIRECTION ( 'NONE',  ( 0.9583148474998867128, 0.000000000000000000, -0.2857142857143631365 ) ) ;
#42287 = CARTESIAN_POINT ( 'NONE',  ( 36.90000000000000568, 0.000000000000000000, 0.000000000000000000 ) ) ;
#42288 = VERTEX_POINT ( 'NONE', #377 ) ;
#42289 = PLANE ( 'NONE',  #35513 ) ;
#42290 = CARTESIAN_POINT ( 'NONE',  ( -7.450000000000001954, 0.000000000000000000, -10.00000000000000000 ) ) ;
#42292 = VECTOR ( 'NONE', #18442, 1000.000000000000000 ) ;
#42291 = CARTESIAN_POINT ( 'NONE',  ( 290.0000000000000000, -0.5000000000000000000, 27.00000000000000000 ) ) ;
#42293 = CARTESIAN_POINT ( 'NONE',  ( -7.793516549646712477, 11.11351654964660085, 455.0000000000000568 ) ) ;
#42294 = EDGE_CURVE ( 'NONE', #29870, #32597, #14831, .T. ) ;
#42295 = AXIS2_PLACEMENT_3D ( 'NONE', #1378, #12308, #50154 ) ;
#42296 = DIRECTION ( 'NONE',  ( 0.6414496315691494699, 0.7671651518153064231, 2.818519042764025305E-16 ) ) ;
#42297 = VERTEX_POINT ( 'NONE', #1745 ) ;
#42298 = PLANE ( 'NONE',  #30167 ) ;
#42299 = DIRECTION ( 'NONE',  ( 0.000000000000000000, 0.000000000000000000, 1.000000000000000000 ) ) ;
#42300 = PLANE ( 'NONE',  #54780 ) ;
#42301 = ADVANCED_FACE ( 'NONE', ( #55158 ), #23319, .T. ) ;
#42302 = DIRECTION ( 'NONE',  ( 0.000000000000000000, 0.000000000000000000, 1.000000000000000000 ) ) ;
#42303 = ORIENTED_EDGE ( 'NONE', *, *, #148, .F. ) ;
#42304 = LINE ( 'NONE', #47269, #68805 ) ;
#42305 = CARTESIAN_POINT ( 'NONE',  ( 15.50000000000000000, -5.000000000000000000, -22.50000000000000000 ) ) ;
#42306 = ADVANCED_FACE ( 'NONE', ( #44880 ), #44519, .F. ) ;
#42307 = VECTOR ( 'NONE', #60768, 1000.000000000000000 ) ;
#42308 = LINE ( 'NONE', #26756, #13150 ) ;
#42309 = CARTESIAN_POINT ( 'NONE',  ( 78.77321854994620765, 47.95351654967443977, 39.00000000000000000 ) ) ;
#42310 = VERTEX_POINT ( 'NONE', #48822 ) ;
#42311 = DIRECTION ( 'NONE',  ( 9.912705577010336396E-15, 1.000000000000000000, 0.000000000000000000 ) ) ;
#42312 = EDGE_CURVE ( 'NONE', #7744, #62134, #43589, .T. ) ;
#42313 = CARTESIAN_POINT ( 'NONE',  ( 25.57999999999999829, 0.000000000000000000, 2.458500000000000796 ) ) ;
#42314 = FACE_OUTER_BOUND ( 'NONE', #17470, .T. ) ;
#42315 = DIRECTION ( 'NONE',  ( -1.000000000000000000, 0.000000000000000000, 0.000000000000000000 ) ) ;
#42316 = CARTESIAN_POINT ( 'NONE',  ( -23.48000000000000043, -15.50000000000000000, -26.00000000000000355 ) ) ;
#42317 = EDGE_CURVE ( 'NONE', #2837, #20689, #65845, .T. ) ;
#42318 = DIRECTION ( 'NONE',  ( 1.000000000000000000, 0.000000000000000000, 0.000000000000000000 ) ) ;
#42319 = ORIENTED_EDGE ( 'NONE', *, *, #37854, .T. ) ;
#42320 = EDGE_LOOP ( 'NONE', ( #814, #60850, #35611, #53923 ) ) ;
#42321 = CARTESIAN_POINT ( 'NONE',  ( -7.450000000000001954, 0.000000000000000000, -8.000000000000000000 ) ) ;
#42322 = CARTESIAN_POINT ( 'NONE',  ( 11.75000000000000000, -5.200000000000001066, 26.25000000000000000 ) ) ;
#42324 = ORIENTED_EDGE ( 'NONE', *, *, #38445, .F. ) ;
#42323 = EDGE_CURVE ( 'NONE', #48280, #4451, #21684, .T. ) ;
#42325 = VECTOR ( 'NONE', #16941, 1000.000000000000000 ) ;
#42326 = DIRECTION ( 'NONE',  ( 1.000000000000000000, 0.000000000000000000, 0.000000000000000000 ) ) ;
#42327 = ADVANCED_FACE ( 'NONE', ( #54563 ), #16373, .F. ) ;
#42328 = DIRECTION ( 'NONE',  ( 0.000000000000000000, 0.7071067811865480168, 0.7071067811865470176 ) ) ;
#42329 = EDGE_CURVE ( 'NONE', #22525, #9315, #35143, .T. ) ;
#42330 = AXIS2_PLACEMENT_3D ( 'NONE', #36670, #9813, #52230 ) ;
#42331 = ORIENTED_EDGE ( 'NONE', *, *, #46875, .T. ) ;
#42332 = EDGE_CURVE ( 'NONE', #46063, #4220, #65177, .T. ) ;
#42333 = EDGE_CURVE ( 'NONE', #59753, #31486, #11744, .T. ) ;
#42334 = DIRECTION ( 'NONE',  ( 0.000000000000000000, 1.000000000000000000, 0.000000000000000000 ) ) ;
#42335 = ORIENTED_EDGE ( 'NONE', *, *, #50444, .T. ) ;
#42336 = ORIENTED_EDGE ( 'NONE', *, *, #26573, .T. ) ;
#42337 = CARTESIAN_POINT ( 'NONE',  ( 4.255011587777269177, 8.452095193409277840, 455.0000000000000568 ) ) ;
#42338 = ORIENTED_EDGE ( 'NONE', *, *, #49985, .F. ) ;
#42339 = ADVANCED_FACE ( 'NONE', ( #32292 ), #58824, .T. ) ;
#42340 = DIRECTION ( 'NONE',  ( 0.000000000000000000, -1.000000000000000000, 0.000000000000000000 ) ) ;
#42341 = DIRECTION ( 'NONE',  ( 0.000000000000000000, 0.7057491738665943037, -0.7084617869628675457 ) ) ;
#42342 = AXIS2_PLACEMENT_3D ( 'NONE', #50201, #12015, #6718 ) ;
#42343 = AXIS2_PLACEMENT_3D ( 'NONE', #1056, #60086, #6354 ) ;
#42344 = CARTESIAN_POINT ( 'NONE',  ( 102.9230540376122462, -102.9230540376126015, 5.000000000000000000 ) ) ;
#42345 = VERTEX_POINT ( 'NONE', #17064 ) ;
#42346 = ORIENTED_EDGE ( 'NONE', *, *, #64441, .T. ) ;
#42347 = FACE_OUTER_BOUND ( 'NONE', #28476, .T. ) ;
#42349 = LINE ( 'NONE', #22183, #1701 ) ;
#42348 = DIRECTION ( 'NONE',  ( -1.000000000000000000, 0.000000000000000000, 0.000000000000000000 ) ) ;
#42350 = VECTOR ( 'NONE', #36243, 1000.000000000000000 ) ;
#42351 = ORIENTED_EDGE ( 'NONE', *, *, #19085, .F. ) ;
#42352 = ORIENTED_EDGE ( 'NONE', *, *, #63892, .F. ) ;
#42353 = ORIENTED_EDGE ( 'NONE', *, *, #47629, .T. ) ;
#42354 = CIRCLE ( 'NONE', #24274, 4.000000000000000888 ) ;
#42355 = DIRECTION ( 'NONE',  ( 1.000000000000000000, 0.000000000000000000, 0.000000000000000000 ) ) ;
#42356 = EDGE_CURVE ( 'NONE', #55865, #1911, #11409, .T. ) ;
#42358 = ORIENTED_EDGE ( 'NONE', *, *, #25920, .T. ) ;
#42357 = DIRECTION ( 'NONE',  ( 1.000000000000000000, 0.000000000000000000, 0.000000000000000000 ) ) ;
#42359 = EDGE_CURVE ( 'NONE', #32779, #38222, #29499, .T. ) ;
#42360 = DIRECTION ( 'NONE',  ( 0.000000000000000000, -1.000000000000000000, -3.673940397442059868E-16 ) ) ;
#42361 = COLOUR_RGB ( '', 0.08235294, 0.09019608, 0.10196078) ;
#42362 = DIRECTION ( 'NONE',  ( 0.000000000000000000, 1.000000000000000000, 0.000000000000000000 ) ) ;
#42363 = ORIENTED_EDGE ( 'NONE', *, *, #15466, .T. ) ;
#42364 = ORIENTED_EDGE ( 'NONE', *, *, #52383, .F. ) ;
#42365 = AXIS2_PLACEMENT_3D ( 'NONE', #29757, #1852, #51331 ) ;
#42366 = LINE ( 'NONE', #69598, #25601 ) ;
#42367 = ORIENTED_EDGE ( 'NONE', *, *, #49592, .F. ) ;
#42368 = DIRECTION ( 'NONE',  ( 0.000000000000000000, 0.000000000000000000, 1.000000000000000000 ) ) ;
#42369 = DIRECTION ( 'NONE',  ( 0.000000000000000000, -0.9921567416492215186, -0.1249999999999996531 ) ) ;
#42370 = DIRECTION ( 'NONE',  ( -1.047444401652940007E-14, -1.000000000000000000, -1.836970198721029934E-16 ) ) ;
#42371 = VERTEX_POINT ( 'NONE', #10378 ) ;
#42372 = LINE ( 'NONE', #65343, #44831 ) ;
#42374 = ORIENTED_EDGE ( 'NONE', *, *, #26941, .F. ) ;
#42373 = DIRECTION ( 'NONE',  ( 0.000000000000000000, 0.000000000000000000, 1.000000000000000000 ) ) ;
#42376 = VERTEX_POINT ( 'NONE', #5774 ) ;
#42375 = CARTESIAN_POINT ( 'NONE',  ( 7.250000000000004441, 7.450000000000001954, -22.50000000000000000 ) ) ;
#42377 = CARTESIAN_POINT ( 'NONE',  ( 1.866219381641437636, 9.404046420174054788, 195.0000000000000284 ) ) ;
#42378 = DIRECTION ( 'NONE',  ( 0.000000000000000000, 0.000000000000000000, -1.000000000000000000 ) ) ;
#42379 = DIRECTION ( 'NONE',  ( 1.836970198721029934E-16, 1.836970198721010706E-16, -1.000000000000000000 ) ) ;
#42380 = LINE ( 'NONE', #63970, #31774 ) ;
#42381 = CIRCLE ( 'NONE', #40086, 1.224999999999997868 ) ;
#42382 = DIRECTION ( 'NONE',  ( -0.000000000000000000, 1.000000000000000000, -0.000000000000000000 ) ) ;
#42383 = ORIENTED_EDGE ( 'NONE', *, *, #24909, .F. ) ;
#42384 = CARTESIAN_POINT ( 'NONE',  ( 3.848229544836329730, 7.342976262117204556, 54.00000000000000711 ) ) ;
#42385 = PLANE ( 'NONE',  #23698 ) ;
#42386 = CARTESIAN_POINT ( 'NONE',  ( 11.50000000000000000, -12.00000000000000000, 11.00000000000000000 ) ) ;
#42387 = EDGE_CURVE ( 'NONE', #4916, #54625, #6464, .T. ) ;
#42389 = ORIENTED_EDGE ( 'NONE', *, *, #44844, .F. ) ;
#42388 = CARTESIAN_POINT ( 'NONE',  ( 7.250000000000005329, -7.249999999999998224, -24.50000000000000000 ) ) ;
#42390 = VECTOR ( 'NONE', #15415, 1000.000000000000000 ) ;
#42391 = AXIS2_PLACEMENT_3D ( 'NONE', #38485, #28886, #60033 ) ;
#42392 = VECTOR ( 'NONE', #43048, 1000.000000000000000 ) ;
#42393 = SURFACE_SIDE_STYLE ('',( #32136 ) ) ;
#42394 = DIRECTION ( 'NONE',  ( -4.336808689942025625E-15, -1.000000000000000000, 0.000000000000000000 ) ) ;
#42395 = CARTESIAN_POINT ( 'NONE',  ( -2.752095193409374030, 9.942044687070435316, 455.0000000000000568 ) ) ;
#42396 = EDGE_CURVE ( 'NONE', #40165, #19545, #4690, .T. ) ;
#42397 = VECTOR ( 'NONE', #31413, 1000.000000000000000 ) ;
#42398 = AXIS2_PLACEMENT_3D ( 'NONE', #29114, #67644, #57380 ) ;
#42399 = DIRECTION ( 'NONE',  ( -1.000000000000000000, 0.000000000000000000, 0.000000000000000000 ) ) ;
#42400 = ORIENTED_EDGE ( 'NONE', *, *, #57319, .T. ) ;
#42401 = DIRECTION ( 'NONE',  ( 0.000000000000000000, 0.000000000000000000, 1.000000000000000000 ) ) ;
#42402 = EDGE_CURVE ( 'NONE', #4698, #43746, #126, .T. ) ;
#42403 = LINE ( 'NONE', #47356, #37401 ) ;
#42404 = EDGE_LOOP ( 'NONE', ( #20577, #30498 ) ) ;
#42405 = LINE ( 'NONE', #63991, #26668 ) ;
#42406 = CARTESIAN_POINT ( 'NONE',  ( 7.806483450353379538, -11.12648345035348996, 455.0000000000000568 ) ) ;
#42407 = VECTOR ( 'NONE', #23213, 1000.000000000000000 ) ;
#42408 = CARTESIAN_POINT ( 'NONE',  ( -4.727349090213463612, 7.798499376343949407, 455.0000000000000568 ) ) ;
#42409 = EDGE_CURVE ( 'NONE', #14789, #42432, #40761, .T. ) ;
#42410 = CARTESIAN_POINT ( 'NONE',  ( 39.90000000000000568, 0.000000000000000000, 3.447897592003593022E-15 ) ) ;
#42411 = CARTESIAN_POINT ( 'NONE',  ( 8.250000000000005329, -8.249999999999998224, -26.00000000000001066 ) ) ;
#42412 = AXIS2_PLACEMENT_3D ( 'NONE', #2297, #44716, #23859 ) ;
#42413 = ORIENTED_EDGE ( 'NONE', *, *, #3371, .F. ) ;
#42414 = ORIENTED_EDGE ( 'NONE', *, *, #13541, .T. ) ;
#42415 = CARTESIAN_POINT ( 'NONE',  ( 11.00000000000000000, -17.14999999999999858, -27.00000000000000000 ) ) ;
#42416 = EDGE_LOOP ( 'NONE', ( #9375, #12052, #2776, #49834 ) ) ;
#42417 = ORIENTED_EDGE ( 'NONE', *, *, #33255, .T. ) ;
#42418 = VECTOR ( 'NONE', #28983, 1000.000000000000000 ) ;
#42419 = DIRECTION ( 'NONE',  ( 0.6414496315691494699, -0.7671651518153064231, 0.000000000000000000 ) ) ;
#42420 = EDGE_CURVE ( 'NONE', #63841, #46765, #22029, .T. ) ;
#42421 = CYLINDRICAL_SURFACE ( 'NONE', #3946, 4.500000000000189182 ) ;
#42422 = PLANE ( 'NONE',  #7276 ) ;
#42423 = ORIENTED_EDGE ( 'NONE', *, *, #69036, .F. ) ;
#42424 = ORIENTED_EDGE ( 'NONE', *, *, #53991, .T. ) ;
#42425 = CARTESIAN_POINT ( 'NONE',  ( -11.75000000000000000, -5.200000000000001066, -26.25000000000000000 ) ) ;
#42426 = ORIENTED_EDGE ( 'NONE', *, *, #67678, .T. ) ;
#42427 = ORIENTED_EDGE ( 'NONE', *, *, #14626, .F. ) ;
#42428 = DIRECTION ( 'NONE',  ( -0.000000000000000000, -0.000000000000000000, -1.000000000000000000 ) ) ;
#42429 = LINE ( 'NONE', #57990, #22272 ) ;
#42430 = FACE_OUTER_BOUND ( 'NONE', #56731, .T. ) ;
#42431 = CIRCLE ( 'NONE', #13079, 1.000000000000000000 ) ;
#42432 = VERTEX_POINT ( 'NONE', #6111 ) ;
#42433 = CARTESIAN_POINT ( 'NONE',  ( -7.250000000000000888, 7.250000000000001776, -15.50000000000000000 ) ) ;
#42435 = DIRECTION ( 'NONE',  ( 0.000000000000000000, 0.000000000000000000, -1.000000000000000000 ) ) ;
#42434 = LINE ( 'NONE', #52353, #58118 ) ;
#42436 = ORIENTED_EDGE ( 'NONE', *, *, #1028, .T. ) ;
#42438 = EDGE_LOOP ( 'NONE', ( #66594, #51464, #13392, #13008 ) ) ;
#42437 = DIRECTION ( 'NONE',  ( 0.000000000000000000, 0.000000000000000000, -1.000000000000000000 ) ) ;
#42439 = ORIENTED_EDGE ( 'NONE', *, *, #25528, .T. ) ;
#42440 = VECTOR ( 'NONE', #43009, 1000.000000000000000 ) ;
#42441 = CARTESIAN_POINT ( 'NONE',  ( 151.5599459900709860, 0.000000000000000000, 280.6301873289890523 ) ) ;
#42442 = EDGE_CURVE ( 'NONE', #48624, #35877, #26641, .T. ) ;
#42443 = EDGE_CURVE ( 'NONE', #23322, #50347, #48696, .T. ) ;
#42444 = AXIS2_PLACEMENT_3D ( 'NONE', #7567, #29133, #50696 ) ;
#42445 = VECTOR ( 'NONE', #19865, 1000.000000000000000 ) ;
#42447 = CARTESIAN_POINT ( 'NONE',  ( 8.900000000000002132, 18.00000000000000355, -21.00000000000000000 ) ) ;
#42446 = AXIS2_PLACEMENT_3D ( 'NONE', #112, #49577, #48896 ) ;
#42448 = ORIENTED_EDGE ( 'NONE', *, *, #24906, .F. ) ;
#42449 = EDGE_CURVE ( 'NONE', #33218, #67025, #54910, .T. ) ;
#42450 = VECTOR ( 'NONE', #6196, 1000.000000000000000 ) ;
#42451 = AXIS2_PLACEMENT_3D ( 'NONE', #21653, #796, #43209 ) ;
#42452 = CARTESIAN_POINT ( 'NONE',  ( 8.406483450353405829, 7.603567055985406498, 455.0000000000000568 ) ) ;
#42453 = CARTESIAN_POINT ( 'NONE',  ( -7.250000000000000888, 7.450000000000003730, -9.500000000000001776 ) ) ;
#42454 = VERTEX_POINT ( 'NONE', #22716 ) ;
#42455 = EDGE_LOOP ( 'NONE', ( #4791, #49998, #7088, #66142 ) ) ;
#42456 = LINE ( 'NONE', #64044, #31978 ) ;
#42457 = CARTESIAN_POINT ( 'NONE',  ( 30.00000000000000000, -11.70000000000000284, -12.50000000000000000 ) ) ;
#42458 = CARTESIAN_POINT ( 'NONE',  ( -7.450000000000001954, 0.000000000000000000, -24.50000000000000000 ) ) ;
#42459 = VERTEX_POINT ( 'NONE', #44265 ) ;
#42460 = AXIS2_PLACEMENT_3D ( 'NONE', #57966, #26154, #61952 ) ;
#42462 = MANIFOLD_SOLID_BREP ( 'LPattern1[10]', #54417 ) ;
#42461 = FACE_OUTER_BOUND ( 'NONE', #32861, .T. ) ;
#42463 = DIRECTION ( 'NONE',  ( -0.000000000000000000, -0.000000000000000000, -1.000000000000000000 ) ) ;
#42464 = ADVANCED_FACE ( 'NONE', ( #44966 ), #23051, .T. ) ;
#42466 = EDGE_LOOP ( 'NONE', ( #27232, #31429, #63887, #20175 ) ) ;
#42465 = DIRECTION ( 'NONE',  ( 0.000000000000000000, 0.000000000000000000, -1.000000000000000000 ) ) ;
#42468 = ORIENTED_EDGE ( 'NONE', *, *, #50026, .F. ) ;
#42467 = DIRECTION ( 'NONE',  ( 0.000000000000000000, 0.000000000000000000, -1.000000000000000000 ) ) ;
#42469 = DIRECTION ( 'NONE',  ( 0.000000000000000000, 0.000000000000000000, 1.000000000000000000 ) ) ;
#42470 = CARTESIAN_POINT ( 'NONE',  ( -6.822336235477446387, 6.350872789121265072, 54.00000000000000711 ) ) ;
#42471 = DIRECTION ( 'NONE',  ( 1.000000000000000000, -0.000000000000000000, -0.000000000000000000 ) ) ;
#42472 = DIRECTION ( 'NONE',  ( -3.491481338843132961E-15, -1.000000000000000000, -1.836970198721029934E-16 ) ) ;
#42473 = CARTESIAN_POINT ( 'NONE',  ( 8.930623737882818602, -10.05377373788282469, 54.00000000000000711 ) ) ;
#42474 = DIRECTION ( 'NONE',  ( 0.000000000000000000, 0.000000000000000000, 1.000000000000000000 ) ) ;
#42475 = ORIENTED_EDGE ( 'NONE', *, *, #15851, .T. ) ;
#42476 = CARTESIAN_POINT ( 'NONE',  ( 17.00000000000000000, -17.50000000000000000, -19.33772233983200195 ) ) ;
#42478 = ORIENTED_EDGE ( 'NONE', *, *, #65106, .F. ) ;
#42477 = CARTESIAN_POINT ( 'NONE',  ( 6.665817930929289759, 7.517976262117195496, 54.00000000000000711 ) ) ;
#42479 = EDGE_CURVE ( 'NONE', #57287, #10693, #8175, .T. ) ;
#42480 = CARTESIAN_POINT ( 'NONE',  ( 7.000000000000000000, -31.30000000000045191, 8.900000000000430234 ) ) ;
#42481 = DIRECTION ( 'NONE',  ( -1.000000000000000000, 0.000000000000000000, 0.000000000000000000 ) ) ;
#42482 = CARTESIAN_POINT ( 'NONE',  ( -7.250000000000000888, 7.250000000000001776, -30.00000000000001066 ) ) ;
#42483 = VECTOR ( 'NONE', #23185, 1000.000000000000000 ) ;
#42484 = VERTEX_POINT ( 'NONE', #46019 ) ;
#42485 = CARTESIAN_POINT ( 'NONE',  ( -16.74999999999999289, -0.3152037684892574076, 22.74589050208021490 ) ) ;
#42486 = EDGE_CURVE ( 'NONE', #11546, #36357, #34337, .T. ) ;
#42487 = LINE ( 'NONE', #401, #9125 ) ;
#42488 = EDGE_CURVE ( 'NONE', #8621, #61820, #38972, .T. ) ;
#42489 = ORIENTED_EDGE ( 'NONE', *, *, #541, .F. ) ;
#42490 = CARTESIAN_POINT ( 'NONE',  ( 7.250000000000005329, -7.449999999999998401, -23.50000000000000000 ) ) ;
#42491 = CARTESIAN_POINT ( 'NONE',  ( -8.250000000000000000, 7.250000000000001776, -14.00000000000000000 ) ) ;
#42492 = EDGE_CURVE ( 'NONE', #44196, #1707, #28699, .T. ) ;
#42493 = EDGE_CURVE ( 'NONE', #43288, #36372, #7479, .T. ) ;
#42494 = VECTOR ( 'NONE', #20106, 1000.000000000000000 ) ;
#42495 = LINE ( 'NONE', #64088, #24012 ) ;
#42496 = EDGE_CURVE ( 'NONE', #61169, #9593, #27253, .T. ) ;
#42497 = ORIENTED_EDGE ( 'NONE', *, *, #12947, .F. ) ;
#42498 = CARTESIAN_POINT ( 'NONE',  ( 9.562023737882812569, -8.144523737882824577, 54.00000000000000711 ) ) ;
#42499 = ORIENTED_EDGE ( 'NONE', *, *, #1740, .T. ) ;
#42500 = ORIENTED_EDGE ( 'NONE', *, *, #27489, .T. ) ;
#42501 = DIRECTION ( 'NONE',  ( -1.000000000000000000, 0.000000000000000000, 0.000000000000000000 ) ) ;
#42503 = DIRECTION ( 'NONE',  ( 1.000000000000000000, 0.000000000000000000, 0.000000000000000000 ) ) ;
#42502 = AXIS2_PLACEMENT_3D ( 'NONE', #4734, #64149, #26297 ) ;
#42504 = VECTOR ( 'NONE', #29183, 1000.000000000000000 ) ;
#42505 = AXIS2_PLACEMENT_3D ( 'NONE', #69305, #9926, #25835 ) ;
#42506 = AXIS2_PLACEMENT_3D ( 'NONE', #46793, #64384, #19572 ) ;
#42507 = DIRECTION ( 'NONE',  ( -1.000000000000000000, 2.602085213965213008E-15, 0.000000000000000000 ) ) ;
#42508 = CARTESIAN_POINT ( 'NONE',  ( 7.757955312929553315, 8.452095193409265406, 455.0000000000000568 ) ) ;
#42509 = ORIENTED_EDGE ( 'NONE', *, *, #3950, .F. ) ;
#42510 = VERTEX_POINT ( 'NONE', #1832 ) ;
#42512 = ORIENTED_EDGE ( 'NONE', *, *, #60910, .F. ) ;
#42511 = LINE ( 'NONE', #64099, #52091 ) ;
#42513 = ORIENTED_EDGE ( 'NONE', *, *, #33074, .T. ) ;
#42514 = AXIS2_PLACEMENT_3D ( 'NONE', #67331, #66622, #55666 ) ;
#42515 = DIRECTION ( 'NONE',  ( 0.000000000000000000, 0.000000000000000000, 1.000000000000000000 ) ) ;
#42516 = LINE ( 'NONE', #63742, #8317 ) ;
#42517 = LINE ( 'NONE', #10683, #54576 ) ;
#42518 = DIRECTION ( 'NONE',  ( -1.000000000000000000, 0.000000000000000000, 0.000000000000000000 ) ) ;
#42520 = LINE ( 'NONE', #64790, #13105 ) ;
#42519 = DIRECTION ( 'NONE',  ( 0.000000000000000000, 1.000000000000000000, 0.000000000000000000 ) ) ;
#42521 = ORIENTED_EDGE ( 'NONE', *, *, #759, .F. ) ;
#42522 = VERTEX_POINT ( 'NONE', #39321 ) ;
#42523 = ORIENTED_EDGE ( 'NONE', *, *, #11393, .T. ) ;
#42524 = VERTEX_POINT ( 'NONE', #60536 ) ;
#42525 = CARTESIAN_POINT ( 'NONE',  ( 78.77321854994620765, 47.95351654967443977, 26.00000000000000355 ) ) ;
#42526 = CARTESIAN_POINT ( 'NONE',  ( 9.899999999999998579, -21.00000000000000000, 13.86939075806900057 ) ) ;
#42527 = CARTESIAN_POINT ( 'NONE',  ( 8.250000000000005329, -7.249999999999998224, -11.50000000000000000 ) ) ;
#42528 = VERTEX_POINT ( 'NONE', #39652 ) ;
#42529 = VERTEX_POINT ( 'NONE', #13484 ) ;
#42530 = TOROIDAL_SURFACE ( 'NONE', #50441, 3.299999999999470024, 0.2000000000005275058 ) ;
#42531 = ORIENTED_EDGE ( 'NONE', *, *, #60245, .T. ) ;
#42532 = EDGE_CURVE ( 'NONE', #57915, #10108, #12096, .T. ) ;
#42533 = ADVANCED_FACE ( 'NONE', ( #55927 ), #49924, .T. ) ;
#42534 = CARTESIAN_POINT ( 'NONE',  ( 25.50000000000000355, 0.000000000000000000, -24.12099999999999866 ) ) ;
#42535 = VERTEX_POINT ( 'NONE', #2185 ) ;
#42536 = AXIS2_PLACEMENT_3D ( 'NONE', #29800, #24507, #13889 ) ;
#42537 = FACE_OUTER_BOUND ( 'NONE', #28898, .T. ) ;
#42538 = EDGE_CURVE ( 'NONE', #32965, #65821, #13130, .T. ) ;
#42539 = ORIENTED_EDGE ( 'NONE', *, *, #27975, .F. ) ;
#42540 = ORIENTED_EDGE ( 'NONE', *, *, #37349, .T. ) ;
#42541 = CIRCLE ( 'NONE', #27849, 0.1749999999999980738 ) ;
#42543 = DIRECTION ( 'NONE',  ( -1.836970198721029934E-16, 1.836970198721036344E-16, -1.000000000000000000 ) ) ;
#42542 = AXIS2_PLACEMENT_3D ( 'NONE', #68983, #3940, #30099 ) ;
#42545 = ORIENTED_EDGE ( 'NONE', *, *, #59801, .F. ) ;
#42544 = DIRECTION ( 'NONE',  ( 0.000000000000000000, -1.000000000000000000, 0.000000000000000000 ) ) ;
#42546 = ORIENTED_EDGE ( 'NONE', *, *, #25476, .F. ) ;
#42547 = AXIS2_PLACEMENT_3D ( 'NONE', #59272, #11170, #230 ) ;
#42548 = VECTOR ( 'NONE', #67134, 1000.000000000000000 ) ;
#42549 = DIRECTION ( 'NONE',  ( 0.000000000000000000, 0.000000000000000000, -1.000000000000000000 ) ) ;
#42550 = CARTESIAN_POINT ( 'NONE',  ( 49.00000000000000000, -21.00000000000000000, 13.86939075806900057 ) ) ;
#42552 = ORIENTED_EDGE ( 'NONE', *, *, #275, .T. ) ;
#42551 = PLANE ( 'NONE',  #14248 ) ;
#42553 = VERTEX_POINT ( 'NONE', #40363 ) ;
#42554 = PLANE ( 'NONE',  #20244 ) ;
#42555 = AXIS2_PLACEMENT_3D ( 'NONE', #53099, #31876, #14196 ) ;
#42556 = DIRECTION ( 'NONE',  ( -0.000000000000000000, 3.673940397442059868E-16, -1.000000000000000000 ) ) ;
#42557 = AXIS2_PLACEMENT_3D ( 'NONE', #30609, #3734, #20349 ) ;
#42558 = DIRECTION ( 'NONE',  ( -8.802523127157697409E-15, -1.000000000000000000, -1.836970198721026976E-16 ) ) ;
#42559 = DIRECTION ( 'NONE',  ( 0.000000000000000000, 0.000000000000000000, -1.000000000000000000 ) ) ;
#42560 = LINE ( 'NONE', #64150, #13581 ) ;
#42561 = AXIS2_PLACEMENT_3D ( 'NONE', #22545, #49756, #1321 ) ;
#42562 = ORIENTED_EDGE ( 'NONE', *, *, #50200, .T. ) ;
#42563 = CARTESIAN_POINT ( 'NONE',  ( 9.106483450353417552, 10.91351654964656603, 455.0000000000000568 ) ) ;
#42564 = ORIENTED_EDGE ( 'NONE', *, *, #51494, .F. ) ;
#42565 = AXIS2_PLACEMENT_3D ( 'NONE', #11663, #55511, #49170 ) ;
#42566 = PLANE ( 'NONE',  #55818 ) ;
#42567 = DIRECTION ( 'NONE',  ( 0.7071067811865474617, -0.7071067811865474617, -2.597868168706479611E-16 ) ) ;
#42568 = LINE ( 'NONE', #47181, #67485 ) ;
#42569 = CYLINDRICAL_SURFACE ( 'NONE', #47603, 0.1999999999999987899 ) ;
#42570 = DIRECTION ( 'NONE',  ( -8.359604446858500663E-15, -1.000000000000000000, 0.000000000000000000 ) ) ;
#42571 = ORIENTED_EDGE ( 'NONE', *, *, #67182, .T. ) ;
#42572 = EDGE_CURVE ( 'NONE', #26427, #61169, #56275, .T. ) ;
#42573 = DIRECTION ( 'NONE',  ( 0.000000000000000000, 0.000000000000000000, -1.000000000000000000 ) ) ;
#42574 = EDGE_CURVE ( 'NONE', #21827, #68424, #18792, .T. ) ;
#42575 = VERTEX_POINT ( 'NONE', #57326 ) ;
#42576 = CARTESIAN_POINT ( 'NONE',  ( 25.50000000000000355, -5.200000000000001066, -22.50000000000000000 ) ) ;
#42577 = DIRECTION ( 'NONE',  ( 0.000000000000000000, 0.000000000000000000, -1.000000000000000000 ) ) ;
#42578 = EDGE_CURVE ( 'NONE', #41772, #66919, #41756, .T. ) ;
#42579 = AXIS2_PLACEMENT_3D ( 'NONE', #16578, #15876, #27873 ) ;
#42580 = DIRECTION ( 'NONE',  ( -0.6414496315691367023, 0.7671651518153173033, 0.000000000000000000 ) ) ;
#42581 = LINE ( 'NONE', #26322, #65222 ) ;
#42582 = LINE ( 'NONE', #57792, #60178 ) ;
#42583 = ORIENTED_EDGE ( 'NONE', *, *, #39757, .T. ) ;
#42584 = FACE_OUTER_BOUND ( 'NONE', #915, .T. ) ;
#42585 = CARTESIAN_POINT ( 'NONE',  ( 30.00000000000000000, -17.35230188589299871, 15.35019951917099945 ) ) ;
#42586 = CYLINDRICAL_SURFACE ( 'NONE', #53814, 24.99999999998784972 ) ;
#42587 = AXIS2_PLACEMENT_3D ( 'NONE', #26138, #58662, #8816 ) ;
#42588 = AXIS2_PLACEMENT_3D ( 'NONE', #55422, #60713, #44104 ) ;
#42589 = SURFACE_STYLE_FILL_AREA ( #58864 ) ;
#42590 = CARTESIAN_POINT ( 'NONE',  ( 8.250000000000005329, -7.249999999999998224, -26.00000000000001066 ) ) ;
#42591 = VERTEX_POINT ( 'NONE', #67591 ) ;
#42593 = VERTEX_POINT ( 'NONE', #15250 ) ;
#42592 = DIRECTION ( 'NONE',  ( 0.000000000000000000, 0.000000000000000000, 1.000000000000000000 ) ) ;
#42594 = ADVANCED_FACE ( 'NONE', ( #41409 ), #58025, .F. ) ;
#42595 = VECTOR ( 'NONE', #69813, 1000.000000000000000 ) ;
#42596 = AXIS2_PLACEMENT_3D ( 'NONE', #16460, #11482, #50007 ) ;
#42597 = DIRECTION ( 'NONE',  ( 0.8660254037844482555, 0.000000000000000000, 0.4999999999999831801 ) ) ;
#42598 = AXIS2_PLACEMENT_3D ( 'NONE', #66433, #37586, #13017 ) ;
#42599 = CARTESIAN_POINT ( 'NONE',  ( 30.00000000000000000, -11.50000000000000000, 11.00000000000000000 ) ) ;
#42600 = CARTESIAN_POINT ( 'NONE',  ( -25.50000000000000355, -15.12100000000000044, 20.87900000000000134 ) ) ;
#42601 = VERTEX_POINT ( 'NONE', #20194 ) ;
#42602 = VECTOR ( 'NONE', #64228, 1000.000000000000000 ) ;
#42604 = DIRECTION ( 'NONE',  ( 1.000000000000000000, -3.491481338843133355E-15, 0.000000000000000000 ) ) ;
#42603 = AXIS2_PLACEMENT_3D ( 'NONE', #37482, #10595, #26520 ) ;
#42605 = DIRECTION ( 'NONE',  ( 0.000000000000000000, 0.000000000000000000, -1.000000000000000000 ) ) ;
#42606 = EDGE_LOOP ( 'NONE', ( #67192, #62975, #48960, #64717 ) ) ;
#42607 = ORIENTED_EDGE ( 'NONE', *, *, #27582, .F. ) ;
#42608 = ORIENTED_EDGE ( 'NONE', *, *, #52734, .T. ) ;
#42609 = CARTESIAN_POINT ( 'NONE',  ( 1.480523737882788238, -9.404523737882794165, 54.00000000000000711 ) ) ;
#42610 = CARTESIAN_POINT ( 'NONE',  ( 7.000000000000000000, -23.50007830495750127, 12.28007262201345995 ) ) ;
#42611 = CARTESIAN_POINT ( 'NONE',  ( 7.250000000000005329, 7.250000000000000888, -21.50000000000000000 ) ) ;
#42612 = AXIS2_PLACEMENT_3D ( 'NONE', #45, #1412, #22976 ) ;
#42613 = ORIENTED_EDGE ( 'NONE', *, *, #46148, .T. ) ;
#42614 = VERTEX_POINT ( 'NONE', #68985 ) ;
#42615 = DIRECTION ( 'NONE',  ( -1.000000000000000000, 0.000000000000000000, 0.000000000000000000 ) ) ;
#42616 = ORIENTED_EDGE ( 'NONE', *, *, #111, .T. ) ;
#42617 = ORIENTED_EDGE ( 'NONE', *, *, #50860, .T. ) ;
#42618 = ADVANCED_FACE ( 'NONE', ( #14189 ), #19840, .F. ) ;
#42619 = ORIENTED_EDGE ( 'NONE', *, *, #14980, .F. ) ;
#42620 = ORIENTED_EDGE ( 'NONE', *, *, #45199, .F. ) ;
#42621 = CARTESIAN_POINT ( 'NONE',  ( -8.393516549646712122, 4.383466043307770121, 455.0000000000000568 ) ) ;
#42623 = ORIENTED_EDGE ( 'NONE', *, *, #12994, .T. ) ;
#42622 = CARTESIAN_POINT ( 'NONE',  ( -11.00000000000000000, -12.00000000000000000, 12.20000000000000107 ) ) ;
#42624 = FACE_BOUND ( 'NONE', #56581, .T. ) ;
#42625 = DIRECTION ( 'NONE',  ( 0.000000000000000000, -0.8206518066484758123, -0.5714285714283042772 ) ) ;
#42626 = LINE ( 'NONE', #64213, #22261 ) ;
#42627 = AXIS2_PLACEMENT_3D ( 'NONE', #8201, #67266, #61949 ) ;
#42628 = ORIENTED_EDGE ( 'NONE', *, *, #69883, .T. ) ;
#42629 = EDGE_CURVE ( 'NONE', #45034, #48708, #30102, .T. ) ;
#42630 = CARTESIAN_POINT ( 'NONE',  ( 277.0217896459287203, -25.18021646000301317, -17.31978353999699749 ) ) ;
#42631 = CIRCLE ( 'NONE', #69708, 1.399999999999998579 ) ;
#42632 = VECTOR ( 'NONE', #69526, 1000.000000000000000 ) ;
#42633 = AXIS2_PLACEMENT_3D ( 'NONE', #2535, #34712, #56289 ) ;
#42634 = EDGE_CURVE ( 'NONE', #48721, #3757, #30456, .T. ) ;
#42635 = DIRECTION ( 'NONE',  ( -1.000000000000000000, 0.000000000000000000, 0.000000000000000000 ) ) ;
#42636 = ORIENTED_EDGE ( 'NONE', *, *, #18191, .T. ) ;
#42637 = VECTOR ( 'NONE', #34657, 1000.000000000000000 ) ;
#42638 = CIRCLE ( 'NONE', #30228, 0.1999999999999996503 ) ;
#42639 = CARTESIAN_POINT ( 'NONE',  ( 6.872275254348383378, 2.989207322240120313, 54.00000000000000711 ) ) ;
#42641 = LINE ( 'NONE', #32393, #61806 ) ;
#42640 = PRODUCT_DEFINITION_FORMATION_WITH_SPECIFIED_SOURCE ( 'ANY', '', #44806, .NOT_KNOWN. ) ;
#42642 = CARTESIAN_POINT ( 'NONE',  ( -1.677516549646777877, -10.74648345035342167, 195.0000000000000284 ) ) ;
#42643 = EDGE_LOOP ( 'NONE', ( #43229, #37242, #59740, #38053 ) ) ;
#42644 = DIRECTION ( 'NONE',  ( 0.000000000000000000, 0.000000000000000000, -1.000000000000000000 ) ) ;
#42645 = CARTESIAN_POINT ( 'NONE',  ( 29.50000000000000355, -12.00000000000000000, 10.69999999999999929 ) ) ;
#42646 = AXIS2_PLACEMENT_3D ( 'NONE', #56727, #34439, #18540 ) ;
#42647 = CARTESIAN_POINT ( 'NONE',  ( 283.0000000000000568, -26.50000000000000000, -9.080000000000000071 ) ) ;
#42648 = CARTESIAN_POINT ( 'NONE',  ( 275.0000000000000000, -38.15000000000000568, -14.50000000000000000 ) ) ;
#42649 = FACE_OUTER_BOUND ( 'NONE', #57782, .T. ) ;
#42650 = ORIENTED_EDGE ( 'NONE', *, *, #49827, .T. ) ;
#42651 = FACE_OUTER_BOUND ( 'NONE', #68778, .T. ) ;
#42652 = CARTESIAN_POINT ( 'NONE',  ( 29.89999999999999858, -0.1999999999911795112, 8.826273045769999343E-12 ) ) ;
#42653 = CARTESIAN_POINT ( 'NONE',  ( -3.842976262117224984, 9.897976262117168744, 54.00000000000000711 ) ) ;
#42654 = LINE ( 'NONE', #14741, #28888 ) ;
#42655 = EDGE_CURVE ( 'NONE', #31236, #32512, #28338, .T. ) ;
#42656 = ADVANCED_FACE ( 'NONE', ( #25154 ), #31173, .T. ) ;
#42657 = VERTEX_POINT ( 'NONE', #24802 ) ;
#42658 = DIRECTION ( 'NONE',  ( 3.491481338843133355E-15, 1.000000000000000000, 1.836970198721029934E-16 ) ) ;
#42659 = EDGE_CURVE ( 'NONE', #114, #60715, #62271, .T. ) ;
#42660 = DIRECTION ( 'NONE',  ( 0.000000000000000000, -1.000000000000000000, 0.000000000000000000 ) ) ;
#42661 = LINE ( 'NONE', #4496, #57224 ) ;
#42662 = DIRECTION ( 'NONE',  ( -1.836970198721029934E-16, 1.836970198721036344E-16, -1.000000000000000000 ) ) ;
#42663 = VERTEX_POINT ( 'NONE', #36103 ) ;
#42664 = DIRECTION ( 'NONE',  ( 0.7142857142857395036, 0.000000000000000000, 0.6998542122237394469 ) ) ;
#42665 = FACE_OUTER_BOUND ( 'NONE', #19705, .T. ) ;
#42666 = EDGE_CURVE ( 'NONE', #19943, #60403, #31801, .T. ) ;
#42667 = PLANE ( 'NONE',  #65003 ) ;
#42668 = CARTESIAN_POINT ( 'NONE',  ( 28.00000000000000000, -16.28999999999710369, -15.00000000000794920 ) ) ;
#42669 = CARTESIAN_POINT ( 'NONE',  ( 8.580623737882818958, -8.930623737882855906, 54.00000000000000711 ) ) ;
#42670 = EDGE_CURVE ( 'NONE', #62883, #21000, #46360, .T. ) ;
#42671 = FACE_OUTER_BOUND ( 'NONE', #46051, .T. ) ;
#42672 = ORIENTED_EDGE ( 'NONE', *, *, #26809, .F. ) ;
#42673 = EDGE_CURVE ( 'NONE', #62419, #64092, #9954, .T. ) ;
#42674 = ORIENTED_EDGE ( 'NONE', *, *, #32593, .F. ) ;
#42675 = CARTESIAN_POINT ( 'NONE',  ( -10.19191654964671301, 9.791916549646639822, 195.0000000000000284 ) ) ;
#42676 = CARTESIAN_POINT ( 'NONE',  ( -6.835476262117260227, 10.30047626211718104, 26.00000000000000711 ) ) ;
#42677 = AXIS2_PLACEMENT_3D ( 'NONE', #12119, #39341, #60900 ) ;
#42678 = VERTEX_POINT ( 'NONE', #47074 ) ;
#42679 = CARTESIAN_POINT ( 'NONE',  ( 283.0000000000000568, -25.69999999999924967, 14.52500000000000213 ) ) ;
#42680 = CARTESIAN_POINT ( 'NONE',  ( -30.00000000000000000, -10.85999999999999943, 9.000000000000001776 ) ) ;
#42681 = ORIENTED_EDGE ( 'NONE', *, *, #23716, .T. ) ;
#42682 = FACE_OUTER_BOUND ( 'NONE', #63373, .T. ) ;
#42683 = VERTEX_POINT ( 'NONE', #31522 ) ;
#42684 = ORIENTED_EDGE ( 'NONE', *, *, #9616, .F. ) ;
#42685 = DIRECTION ( 'NONE',  ( 1.000000000000000000, -0.000000000000000000, 0.000000000000000000 ) ) ;
#42686 = VERTEX_POINT ( 'NONE', #68647 ) ;
#42687 = CARTESIAN_POINT ( 'NONE',  ( 283.0000000000000568, -30.80000000000000071, -8.900000000000000355 ) ) ;
#42688 = AXIS2_PLACEMENT_3D ( 'NONE', #6661, #27542, #44139 ) ;
#42689 = DIRECTION ( 'NONE',  ( -1.836970198721029934E-16, 1.836970198721036344E-16, -1.000000000000000000 ) ) ;
#42690 = CARTESIAN_POINT ( 'NONE',  ( -5.242976262117280406, -5.257023737882805747, 54.00000000000000711 ) ) ;
#42691 = MANIFOLD_SOLID_BREP ( 'LPattern1[22]', #38616 ) ;
#42692 = ORIENTED_EDGE ( 'NONE', *, *, #52129, .F. ) ;
#42693 = ORIENTED_EDGE ( 'NONE', *, *, #1486, .F. ) ;
#42694 = CARTESIAN_POINT ( 'NONE',  ( 23.75054448485400016, -15.50000000000000000, -25.53140320652400064 ) ) ;
#42695 = VECTOR ( 'NONE', #3503, 1000.000000000000114 ) ;
#42696 = VECTOR ( 'NONE', #21044, 1000.000000000000000 ) ;
#42698 = CARTESIAN_POINT ( 'NONE',  ( 25.50000000000000355, -15.50000000000000000, -22.50000000000000000 ) ) ;
#42697 = FACE_OUTER_BOUND ( 'NONE', #12405, .T. ) ;
#42699 = EDGE_LOOP ( 'NONE', ( #55538, #19747, #2682, #15502 ) ) ;
#42700 = ORIENTED_EDGE ( 'NONE', *, *, #37463, .T. ) ;
#42701 = EDGE_CURVE ( 'NONE', #15923, #56899, #1343, .T. ) ;
#42703 = ORIENTED_EDGE ( 'NONE', *, *, #67052, .F. ) ;
#42702 = APPLICATION_PROTOCOL_DEFINITION ( 'draft international standard', 'automotive_design', 1998, #12833 ) ;
#42704 = CARTESIAN_POINT ( 'NONE',  ( 39.90000000000000568, -21.00000000000000355, -14.57806571531352269 ) ) ;
#42706 = ORIENTED_EDGE ( 'NONE', *, *, #26095, .T. ) ;
#42705 = CARTESIAN_POINT ( 'NONE',  ( 7.899999999999999467, -14.48845687959340012, 21.00000000000000000 ) ) ;
#42707 = EDGE_CURVE ( 'NONE', #52260, #34851, #48124, .T. ) ;
#42708 = VECTOR ( 'NONE', #26664, 1000.000000000000000 ) ;
#42709 = DIRECTION ( 'NONE',  ( 0.000000000000000000, -0.000000000000000000, 1.000000000000000000 ) ) ;
#42710 = CARTESIAN_POINT ( 'NONE',  ( 20.90000000000000213, -0.1999999999911430404, -8.864436962241481021E-12 ) ) ;
#42711 = ORIENTED_EDGE ( 'NONE', *, *, #1847, .F. ) ;
#42712 = ORIENTED_EDGE ( 'NONE', *, *, #65503, .T. ) ;
#42713 = DIRECTION ( 'NONE',  ( 0.000000000000000000, 0.000000000000000000, 1.000000000000000000 ) ) ;
#42714 = VERTEX_POINT ( 'NONE', #48823 ) ;
#42715 = CARTESIAN_POINT ( 'NONE',  ( 10.90000000000000036, -21.00000000000000000, 13.86939075806900057 ) ) ;
#42716 = CARTESIAN_POINT ( 'NONE',  ( -15.50000000000000000, -5.000000000000000000, -26.00000000000000000 ) ) ;
#42717 = EDGE_CURVE ( 'NONE', #58001, #41070, #49842, .T. ) ;
#42718 = LINE ( 'NONE', #49344, #64499 ) ;
#42719 = ORIENTED_EDGE ( 'NONE', *, *, #24149, .T. ) ;
#42720 = CARTESIAN_POINT ( 'NONE',  ( -10.91351654964671525, -2.906483450353338771, 455.0000000000000568 ) ) ;
#42721 = CARTESIAN_POINT ( 'NONE',  ( 4.046023737882819660, -3.157023737882815873, 26.00000000000000711 ) ) ;
#42722 = EDGE_CURVE ( 'NONE', #22368, #8035, #65695, .T. ) ;
#42723 = ORIENTED_EDGE ( 'NONE', *, *, #29993, .T. ) ;
#42724 = ORIENTED_EDGE ( 'NONE', *, *, #36692, .T. ) ;
#42725 = EDGE_CURVE ( 'NONE', #32135, #64214, #21648, .T. ) ;
#42726 = LINE ( 'NONE', #58654, #16264 ) ;
#42727 = DIRECTION ( 'NONE',  ( -1.836970198721029934E-16, 1.836970198721036344E-16, -1.000000000000000000 ) ) ;
#42728 = EDGE_CURVE ( 'NONE', #52264, #64997, #15610, .T. ) ;
#42729 = DIRECTION ( 'NONE',  ( 0.000000000000000000, -1.000000000000000000, 0.000000000000000000 ) ) ;
#42730 = EDGE_CURVE ( 'NONE', #18454, #8699, #60035, .T. ) ;
#42731 = EDGE_CURVE ( 'NONE', #56899, #16486, #9524, .T. ) ;
#42732 = CARTESIAN_POINT ( 'NONE',  ( 27.00000000000000000, 0.000000000000000000, -2.458500000000000796 ) ) ;
#42733 = CARTESIAN_POINT ( 'NONE',  ( 0.000000000000000000, 0.000000000000000000, 10.00000000000000000 ) ) ;
#42734 = ORIENTED_EDGE ( 'NONE', *, *, #47551, .F. ) ;
#42735 = CARTESIAN_POINT ( 'NONE',  ( 7.000000000000000000, -25.60000000000000142, -15.10000000000000142 ) ) ;
#42736 = LINE ( 'NONE', #4918, #16957 ) ;
#42737 = ADVANCED_FACE ( 'NONE', ( #31867 ), #58736, .F. ) ;
#42738 = DIRECTION ( 'NONE',  ( -1.000000000000000000, 0.000000000000000000, 0.000000000000000000 ) ) ;
#42739 = CIRCLE ( 'NONE', #43895, 4.500000000000190958 ) ;
#42741 = ORIENTED_EDGE ( 'NONE', *, *, #53243, .F. ) ;
#42740 = CARTESIAN_POINT ( 'NONE',  ( 41.09999999999999432, -21.00000000000000000, -13.86939075806900057 ) ) ;
#42742 = DIRECTION ( 'NONE',  ( -0.000000000000000000, 0.000000000000000000, 1.000000000000000000 ) ) ;
#42743 = ADVANCED_FACE ( 'NONE', ( #64392 ), #65085, .F. ) ;
#42744 = DIRECTION ( 'NONE',  ( -1.000000000000000000, 1.047444401652940007E-14, -1.836970198721010706E-16 ) ) ;
#42745 = DIRECTION ( 'NONE',  ( 0.000000000000000000, -0.000000000000000000, 1.000000000000000000 ) ) ;
#42746 = EDGE_CURVE ( 'NONE', #6513, #35140, #30671, .T. ) ;
#42747 = AXIS2_PLACEMENT_3D ( 'NONE', #46114, #8633, #36555 ) ;
#42748 = CYLINDRICAL_SURFACE ( 'NONE', #16418, 1.000000000000000888 ) ;
#42749 = ORIENTED_EDGE ( 'NONE', *, *, #67987, .F. ) ;
#42750 = LINE ( 'NONE', #35684, #10646 ) ;
#42751 = DIRECTION ( 'NONE',  ( 0.000000000000000000, 0.000000000000000000, -1.000000000000000000 ) ) ;
#42752 = ORIENTED_EDGE ( 'NONE', *, *, #16191, .T. ) ;
#42753 = CARTESIAN_POINT ( 'NONE',  ( 11.78648345035337996, 4.173516549646518747, 455.0000000000000568 ) ) ;
#42754 = DIRECTION ( 'NONE',  ( -1.000000000000000000, 0.000000000000000000, 0.000000000000000000 ) ) ;
#42755 = FACE_OUTER_BOUND ( 'NONE', #3075, .T. ) ;
#42756 = ADVANCED_FACE ( 'NONE', ( #32205 ), #5351, .F. ) ;
#42757 = CARTESIAN_POINT ( 'NONE',  ( -11.00000000000000000, -8.959999999999999076, -12.95475478405700009 ) ) ;
#42758 = EDGE_CURVE ( 'NONE', #7139, #41138, #22796, .T. ) ;
#42759 = CIRCLE ( 'NONE', #22427, 4.000000000000000000 ) ;
#42760 = DIRECTION ( 'NONE',  ( 1.000000000000000000, -5.981805089575196197E-17, 0.000000000000000000 ) ) ;
#42761 = ORIENTED_EDGE ( 'NONE', *, *, #26782, .T. ) ;
#42762 = ORIENTED_EDGE ( 'NONE', *, *, #31422, .T. ) ;
#42763 = CARTESIAN_POINT ( 'NONE',  ( 9.900000000000000355, -21.00000000000000000, -18.00000000000000355 ) ) ;
#42764 = ORIENTED_EDGE ( 'NONE', *, *, #30157, .T. ) ;
#42765 = VERTEX_POINT ( 'NONE', #5689 ) ;
#42766 = LINE ( 'NONE', #46666, #38216 ) ;
#42767 = EDGE_CURVE ( 'NONE', #22636, #32305, #10987, .T. ) ;
#42768 = DIRECTION ( 'NONE',  ( 0.7671651518153083105, -0.6414496315691473605, -2.587583378555127804E-16 ) ) ;
#42769 = CARTESIAN_POINT ( 'NONE',  ( -9.722976262117303037, -7.969523737882757253, 54.00000000000000711 ) ) ;
#42770 = ORIENTED_EDGE ( 'NONE', *, *, #17394, .T. ) ;
#42771 = ORIENTED_EDGE ( 'NONE', *, *, #11812, .T. ) ;
#42772 = DIRECTION ( 'NONE',  ( 0.000000000000000000, 0.000000000000000000, -1.000000000000000000 ) ) ;
#42773 = ORIENTED_EDGE ( 'NONE', *, *, #3400, .T. ) ;
#42774 = ORIENTED_EDGE ( 'NONE', *, *, #46633, .T. ) ;
#42775 = DIRECTION ( 'NONE',  ( 0.000000000000000000, 0.000000000000000000, -1.000000000000000000 ) ) ;
#42776 = CARTESIAN_POINT ( 'NONE',  ( 50.00000000000000711, 0.7500000000000000000, -4.943429983321300902 ) ) ;
#42777 = PLANE ( 'NONE',  #49025 ) ;
#42778 = ORIENTED_EDGE ( 'NONE', *, *, #10331, .T. ) ;
#42779 = DIRECTION ( 'NONE',  ( -0.000000000000000000, 0.000000000000000000, 1.000000000000000000 ) ) ;
#42781 = DIRECTION ( 'NONE',  ( -4.745709458399858621E-16, -1.000000000000000000, 0.000000000000000000 ) ) ;
#42780 = CARTESIAN_POINT ( 'NONE',  ( 2.420780051175147829, -8.711985858128677762, 54.00000000000000711 ) ) ;
#42782 = ORIENTED_EDGE ( 'NONE', *, *, #38920, .T. ) ;
#42784 = ORIENTED_EDGE ( 'NONE', *, *, #46205, .T. ) ;
#42783 = DIRECTION ( 'NONE',  ( 0.000000000000000000, -1.000000000000000000, 3.819861094142539476E-12 ) ) ;
#42785 = ORIENTED_EDGE ( 'NONE', *, *, #13381, .T. ) ;
#42786 = AXIS2_PLACEMENT_3D ( 'NONE', #27739, #10435, #11125 ) ;
#42787 = EDGE_CURVE ( 'NONE', #15647, #55647, #59769, .T. ) ;
#42788 = CARTESIAN_POINT ( 'NONE',  ( 4.149127210878725158, -3.677663764522638434, 26.00000000000000711 ) ) ;
#42789 = EDGE_CURVE ( 'NONE', #23385, #19716, #11319, .T. ) ;
#42790 = CARTESIAN_POINT ( 'NONE',  ( 283.0000000000000568, -31.30000000000045191, 8.400000000000000355 ) ) ;
#42791 = ORIENTED_EDGE ( 'NONE', *, *, #33247, .T. ) ;
#42792 = EDGE_CURVE ( 'NONE', #14260, #55322, #60104, .T. ) ;
#42793 = VECTOR ( 'NONE', #19153, 1000.000000000000000 ) ;
#42794 = PLANE ( 'NONE',  #12034 ) ;
#42795 = EDGE_CURVE ( 'NONE', #26651, #48173, #66453, .T. ) ;
#42796 = DIRECTION ( 'NONE',  ( 0.000000000000000000, -0.1249999999999996531, 0.9921567416492215186 ) ) ;
#42797 = EDGE_LOOP ( 'NONE', ( #2062, #18359, #62731, #1538 ) ) ;
#42798 = ORIENTED_EDGE ( 'NONE', *, *, #29200, .T. ) ;
#42799 = AXIS2_PLACEMENT_3D ( 'NONE', #66706, #2357, #17915 ) ;
#42800 = CARTESIAN_POINT ( 'NONE',  ( 7.250000000000005329, 7.250000000000000888, -17.50000000000000000 ) ) ;
#42801 = CYLINDRICAL_SURFACE ( 'NONE', #56071, 2.250000000000001776 ) ;
#42802 = EDGE_CURVE ( 'NONE', #30786, #52350, #50186, .T. ) ;
#42803 = CARTESIAN_POINT ( 'NONE',  ( 7.000000000000000000, -32.45000000000000995, -12.69999999999999929 ) ) ;
#42804 = VERTEX_POINT ( 'NONE', #2102 ) ;
#42805 = VECTOR ( 'NONE', #63882, 1000.000000000000000 ) ;
#42807 = MANIFOLD_SOLID_BREP ( 'LPattern1[20]', #65660 ) ;
#42806 = CARTESIAN_POINT ( 'NONE',  ( -4.193516549646675529, 11.11351654964658664, 455.0000000000000568 ) ) ;
#42808 = LINE ( 'NONE', #58735, #33933 ) ;
#42810 = ORIENTED_EDGE ( 'NONE', *, *, #7230, .T. ) ;
#42809 = CARTESIAN_POINT ( 'NONE',  ( 39.00000000000000000, 0.000000000000000000, 0.000000000000000000 ) ) ;
#42812 = ORIENTED_EDGE ( 'NONE', *, *, #22470, .F. ) ;
#42811 = PLANE ( 'NONE',  #30059 ) ;
#42813 = DIRECTION ( 'NONE',  ( -1.836970198721029934E-16, 1.836970198721036344E-16, -1.000000000000000000 ) ) ;
#42814 = AXIS2_PLACEMENT_3D ( 'NONE', #54139, #44195, #22643 ) ;
#42815 = CARTESIAN_POINT ( 'NONE',  ( -6.500000000000002665, 6.500000000000002665, -1.000000000000000000 ) ) ;
#42816 = LINE ( 'NONE', #59081, #45931 ) ;
#42817 = CARTESIAN_POINT ( 'NONE',  ( -7.603567055985545942, 8.393516549646601987, 195.0000000000000284 ) ) ;
#42818 = ADVANCED_FACE ( 'NONE', ( #24006 ), #38885, .T. ) ;
#42819 = CARTESIAN_POINT ( 'NONE',  ( -7.603567055985634759, -8.406483450353409381, 455.0000000000000568 ) ) ;
#42820 = CARTESIAN_POINT ( 'NONE',  ( 7.250000000000005329, -8.249999999999998224, -17.50000000000000000 ) ) ;
#42821 = ORIENTED_EDGE ( 'NONE', *, *, #52172, .T. ) ;
#42822 = LINE ( 'NONE', #42476, #54170 ) ;
#42824 = ORIENTED_EDGE ( 'NONE', *, *, #23725, .T. ) ;
#42823 =( NAMED_UNIT ( * ) PLANE_ANGLE_UNIT ( ) SI_UNIT ( $, .RADIAN. ) );
#42826 = VERTEX_POINT ( 'NONE', #50543 ) ;
#42825 = DIRECTION ( 'NONE',  ( -1.000000000000000000, 8.339399738404101090E-15, -1.836970198721014896E-16 ) ) ;
#42827 = CARTESIAN_POINT ( 'NONE',  ( -2.355476262117234931, 8.821682069070680754, 26.00000000000000711 ) ) ;
#42828 = CARTESIAN_POINT ( 'NONE',  ( 8.900000000000002132, 0.000000000000000000, 0.000000000000000000 ) ) ;
#42829 = ORIENTED_EDGE ( 'NONE', *, *, #20897, .T. ) ;
#42830 = CARTESIAN_POINT ( 'NONE',  ( 8.250000000000005329, 7.250000000000000888, -21.00000000000000000 ) ) ;
#42831 = DIRECTION ( 'NONE',  ( -0.000000000000000000, 3.673940397442059868E-16, -1.000000000000000000 ) ) ;
#42832 = EDGE_LOOP ( 'NONE', ( #32080, #51902, #17349, #4109 ) ) ;
#42833 = CIRCLE ( 'NONE', #21389, 0.8100000000000017186 ) ;
#42834 = CARTESIAN_POINT ( 'NONE',  ( 39.90000000000000568, 0.000000000000000000, 3.447897592003593022E-15 ) ) ;
#42835 = CARTESIAN_POINT ( 'NONE',  ( 30.00000000000000000, -11.50000000000100009, 10.50000000000065903 ) ) ;
#42836 = SURFACE_STYLE_FILL_AREA ( #11352 ) ;
#42837 = EDGE_CURVE ( 'NONE', #43994, #44242, #44521, .T. ) ;
#42838 = VECTOR ( 'NONE', #49884, 1000.000000000000000 ) ;
#42839 = VECTOR ( 'NONE', #37825, 1000.000000000000000 ) ;
#42840 = ADVANCED_FACE ( 'NONE', ( #45220 ), #66789, .F. ) ;
#42841 = ORIENTED_EDGE ( 'NONE', *, *, #32287, .F. ) ;
#42842 = LINE ( 'NONE', #69734, #48458 ) ;
#42843 = ORIENTED_EDGE ( 'NONE', *, *, #9011, .T. ) ;
#42844 = ORIENTED_EDGE ( 'NONE', *, *, #10257, .T. ) ;
#42845 = CIRCLE ( 'NONE', #50750, 5.250000000000000000 ) ;
#42846 = CARTESIAN_POINT ( 'NONE',  ( -13.00000000000000178, -17.00000000000000000, -15.70499999999969809 ) ) ;
#42847 = CARTESIAN_POINT ( 'NONE',  ( 38.90000000000000568, -0.2000000000089119934, -8.913009219568841313E-12 ) ) ;
#42848 = AXIS2_PLACEMENT_3D ( 'NONE', #26730, #48297, #17406 ) ;
#42849 = DIRECTION ( 'NONE',  ( -1.000000000000000000, 0.000000000000000000, 0.000000000000000000 ) ) ;
#42850 = FACE_OUTER_BOUND ( 'NONE', #12016, .T. ) ;
#42851 = ORIENTED_EDGE ( 'NONE', *, *, #34684, .T. ) ;
#42852 = VERTEX_POINT ( 'NONE', #55842 ) ;
#42854 = VERTEX_POINT ( 'NONE', #33916 ) ;
#42853 = CYLINDRICAL_SURFACE ( 'NONE', #29513, 0.4000000000000617506 ) ;
#42855 = ORIENTED_EDGE ( 'NONE', *, *, #12668, .T. ) ;
#42856 = VECTOR ( 'NONE', #65288, 1000.000000000000000 ) ;
#42857 = FACE_OUTER_BOUND ( 'NONE', #4737, .T. ) ;
#42858 = DIRECTION ( 'NONE',  ( 1.000000000000000000, -0.000000000000000000, 0.000000000000000000 ) ) ;
#42859 = CARTESIAN_POINT ( 'NONE',  ( -8.393516549646697911, -4.396432944014502020, 195.0000000000000284 ) ) ;
#42860 = CARTESIAN_POINT ( 'NONE',  ( -10.30047626211725742, 6.835476262117182955, 26.00000000000000711 ) ) ;
#42862 = CARTESIAN_POINT ( 'NONE',  ( 29.25000000000000000, -5.000000000000000000, 60.00000000000000000 ) ) ;
#42861 = CARTESIAN_POINT ( 'NONE',  ( 8.000000000000001776, -6.879816696376140683, -1.000000000000000000 ) ) ;
#42863 = ORIENTED_EDGE ( 'NONE', *, *, #27630, .F. ) ;
#42865 = ORIENTED_EDGE ( 'NONE', *, *, #51404, .F. ) ;
#42864 = DIRECTION ( 'NONE',  ( -0.000000000000000000, -0.000000000000000000, -1.000000000000000000 ) ) ;
#42866 = ORIENTED_EDGE ( 'NONE', *, *, #371, .F. ) ;
#42867 = ORIENTED_EDGE ( 'NONE', *, *, #37939, .F. ) ;
#42868 = CARTESIAN_POINT ( 'NONE',  ( -7.593516549646791347, -11.78648345035336042, 195.0000000000000284 ) ) ;
#42869 = DIRECTION ( 'NONE',  ( -1.836970198721029934E-16, -1.836970198721010706E-16, 1.000000000000000000 ) ) ;
#42870 = EDGE_CURVE ( 'NONE', #19926, #12566, #55505, .T. ) ;
#42871 = CARTESIAN_POINT ( 'NONE',  ( -4.727349090213512461, -7.811466277050747919, 195.0000000000000284 ) ) ;
#42872 = VECTOR ( 'NONE', #1634, 999.9999999999998863 ) ;
#42873 = ORIENTED_EDGE ( 'NONE', *, *, #58215, .F. ) ;
#42874 = ORIENTED_EDGE ( 'NONE', *, *, #27582, .T. ) ;
#42875 = ORIENTED_EDGE ( 'NONE', *, *, #65392, .T. ) ;
#42876 = EDGE_CURVE ( 'NONE', #46850, #24181, #67921, .T. ) ;
#42877 = DIRECTION ( 'NONE',  ( 0.000000000000000000, 0.000000000000000000, 1.000000000000000000 ) ) ;
#42878 = ORIENTED_EDGE ( 'NONE', *, *, #40732, .T. ) ;
#42879 = LINE ( 'NONE', #65498, #54637 ) ;
#42880 = EDGE_CURVE ( 'NONE', #43217, #44762, #28969, .T. ) ;
#42881 = LINE ( 'NONE', #16025, #41318 ) ;
#42882 = EDGE_CURVE ( 'NONE', #66079, #57523, #32946, .T. ) ;
#42883 = VERTEX_POINT ( 'NONE', #44183 ) ;
#42884 = ORIENTED_EDGE ( 'NONE', *, *, #34029, .F. ) ;
#42885 = DIRECTION ( 'NONE',  ( 0.000000000000000000, 0.000000000000000000, 1.000000000000000000 ) ) ;
#42886 = ADVANCED_FACE ( 'NONE', ( #67146 ), #56537, .T. ) ;
#42887 = EDGE_CURVE ( 'NONE', #9824, #49229, #49506, .T. ) ;
#42888 = CARTESIAN_POINT ( 'NONE',  ( -4.188533722949335569, 4.727349090213398775, 195.0000000000000284 ) ) ;
#42889 = VECTOR ( 'NONE', #16079, 1000.000000000000000 ) ;
#42890 = EDGE_LOOP ( 'NONE', ( #30256, #47658, #49387, #50663 ) ) ;
#42891 = CIRCLE ( 'NONE', #2250, 25.39999999999999858 ) ;
#42892 = AXIS2_PLACEMENT_3D ( 'NONE', #63632, #15883, #37456 ) ;
#42893 = EDGE_CURVE ( 'NONE', #34559, #61917, #36730, .T. ) ;
#42894 = LINE ( 'NONE', #60534, #24572 ) ;
#42896 = VERTEX_POINT ( 'NONE', #40968 ) ;
#42895 = DIRECTION ( 'NONE',  ( 0.7671651518153105309, 0.6414496315691445849, 2.356647714346206145E-16 ) ) ;
#42897 = ORIENTED_EDGE ( 'NONE', *, *, #27175, .F. ) ;
#42898 = AXIS2_PLACEMENT_3D ( 'NONE', #303, #39165, #34181 ) ;
#42899 = FACE_OUTER_BOUND ( 'NONE', #36310, .T. ) ;
#42900 = CARTESIAN_POINT ( 'NONE',  ( 7.250000000000005329, 7.250000000000000888, -22.50000000000000000 ) ) ;
#42901 = CARTESIAN_POINT ( 'NONE',  ( -6.500000000000002665, -6.500000000000002665, -1.000000000000000000 ) ) ;
#42902 = DIRECTION ( 'NONE',  ( 0.000000000000000000, 0.000000000000000000, 1.000000000000000000 ) ) ;
#42903 = AXIS2_PLACEMENT_3D ( 'NONE', #3538, #29335, #13781 ) ;
#42904 = CARTESIAN_POINT ( 'NONE',  ( -8.821682069070780230, 8.130476262117182884, 26.00000000000000711 ) ) ;
#42905 = EDGE_LOOP ( 'NONE', ( #30270, #52596, #32008, #14245 ) ) ;
#42906 = DIRECTION ( 'NONE',  ( -4.956352788505168198E-15, -1.000000000000000000, 0.000000000000000000 ) ) ;
#42907 = AXIS2_PLACEMENT_3D ( 'NONE', #18464, #13169, #56309 ) ;
#42908 = EDGE_LOOP ( 'NONE', ( #10784, #31908, #3110, #58781 ) ) ;
#42909 = DIRECTION ( 'NONE',  ( -1.000000000000000000, -0.000000000000000000, -0.000000000000000000 ) ) ;
#42910 = CARTESIAN_POINT ( 'NONE',  ( 7.357023737882779635, 3.834182069070702692, 26.00000000000000711 ) ) ;
#42911 = DIRECTION ( 'NONE',  ( 0.000000000000000000, -0.7071067811865475727, 0.7071067811865475727 ) ) ;
#42912 = FACE_OUTER_BOUND ( 'NONE', #29863, .T. ) ;
#42913 = AXIS2_PLACEMENT_3D ( 'NONE', #46804, #35138, #62716 ) ;
#42914 = AXIS2_PLACEMENT_3D ( 'NONE', #45459, #7635, #62415 ) ;
#42915 = CARTESIAN_POINT ( 'NONE',  ( 25.50000000000000355, -5.578999999999999737, -24.12099999999999511 ) ) ;
#42916 = ORIENTED_EDGE ( 'NONE', *, *, #47941, .F. ) ;
#42917 = CARTESIAN_POINT ( 'NONE',  ( -7.250000000000001776, -7.249999999999998224, -26.00000000000001066 ) ) ;
#42918 = DIRECTION ( 'NONE',  ( 0.000000000000000000, 0.000000000000000000, -1.000000000000000000 ) ) ;
#42919 = EDGE_CURVE ( 'NONE', #53158, #34278, #63439, .T. ) ;
#42920 = EDGE_LOOP ( 'NONE', ( #787, #46724, #22930, #22434 ) ) ;
#42921 = MANIFOLD_SOLID_BREP ( 'LPattern1[12]', #5853 ) ;
#42922 = AXIS2_PLACEMENT_3D ( 'NONE', #57482, #3395, #30967 ) ;
#42923 = CARTESIAN_POINT ( 'NONE',  ( -7.342976262117252517, -3.848229544836288429, 54.00000000000000711 ) ) ;
#42924 = CARTESIAN_POINT ( 'NONE',  ( -9.689726262117227762, 10.03972626211718300, 26.00000000000000711 ) ) ;
#42925 = ADVANCED_FACE ( 'NONE', ( #2789 ), #3158, .T. ) ;
#42926 = ORIENTED_EDGE ( 'NONE', *, *, #14356, .F. ) ;
#42927 = EDGE_CURVE ( 'NONE', #68445, #44549, #60214, .T. ) ;
#42928 = DIRECTION ( 'NONE',  ( -0.000000000000000000, -0.000000000000000000, -1.000000000000000000 ) ) ;
#42929 = LINE ( 'NONE', #60223, #31990 ) ;
#42930 = ORIENTED_EDGE ( 'NONE', *, *, #65053, .F. ) ;
#42931 = CARTESIAN_POINT ( 'NONE',  ( 4.201500623656003519, -7.272650909786698037, 455.0000000000000568 ) ) ;
#42932 = DIRECTION ( 'NONE',  ( 0.000000000000000000, 0.000000000000000000, -1.000000000000000000 ) ) ;
#42933 = ADVANCED_FACE ( 'NONE', ( #3504 ), #57590, .F. ) ;
#42934 = CARTESIAN_POINT ( 'NONE',  ( 73.57321854994619059, 47.95351654967443977, 20.00000000000000000 ) ) ;
#42935 = CIRCLE ( 'NONE', #12418, 0.1999999999999987899 ) ;
#42936 = CARTESIAN_POINT ( 'NONE',  ( 9.690000000000001279, -9.690000000000001279, -5.000000000000000000 ) ) ;
#42937 = ORIENTED_EDGE ( 'NONE', *, *, #18596, .T. ) ;
#42939 = ORIENTED_EDGE ( 'NONE', *, *, #31085, .T. ) ;
#42938 = CARTESIAN_POINT ( 'NONE',  ( -19.00000000000000000, -5.000000000000000000, -22.50000000000000000 ) ) ;
#42940 = CIRCLE ( 'NONE', #27147, 0.1999999999999987899 ) ;
#42941 = LINE ( 'NONE', #11452, #27084 ) ;
#42942 = LINE ( 'NONE', #32682, #755 ) ;
#42943 = DIRECTION ( 'NONE',  ( 0.000000000000000000, -1.000000000000000000, -0.000000000000000000 ) ) ;
#42944 = ORIENTED_EDGE ( 'NONE', *, *, #67182, .F. ) ;
#42945 = VECTOR ( 'NONE', #10819, 1000.000000000000000 ) ;
#42946 = FACE_OUTER_BOUND ( 'NONE', #19429, .T. ) ;
#42947 = LINE ( 'NONE', #57810, #63497 ) ;
#42948 = ORIENTED_EDGE ( 'NONE', *, *, #47864, .F. ) ;
#42949 = ORIENTED_EDGE ( 'NONE', *, *, #16011, .F. ) ;
#42950 = VECTOR ( 'NONE', #11945, 1000.000000000000000 ) ;
#42951 = ORIENTED_EDGE ( 'NONE', *, *, #45741, .F. ) ;
#42952 = VECTOR ( 'NONE', #6457, 1000.000000000000000 ) ;
#42953 = DIRECTION ( 'NONE',  ( -1.836970198721029934E-16, -1.836970198721010706E-16, 1.000000000000000000 ) ) ;
#42954 = CARTESIAN_POINT ( 'NONE',  ( 8.250000000000005329, 7.250000000000000888, -25.50000000000000355 ) ) ;
#42955 = CARTESIAN_POINT ( 'NONE',  ( 78.77321854994620765, 47.95351654967443977, 43.00000000000000000 ) ) ;
#42956 = EDGE_CURVE ( 'NONE', #32328, #36815, #51596, .T. ) ;
#42957 = EDGE_LOOP ( 'NONE', ( #57913, #3355, #27205, #23554 ) ) ;
#42958 = ORIENTED_EDGE ( 'NONE', *, *, #56682, .F. ) ;
#42960 = CARTESIAN_POINT ( 'NONE',  ( 4.186483450353335023, -12.00648345035338238, 195.0000000000000284 ) ) ;
#42959 = VECTOR ( 'NONE', #51325, 1000.000000000000000 ) ;
#42961 = AXIS2_PLACEMENT_3D ( 'NONE', #5498, #11811, #33399 ) ;
#42962 = ORIENTED_EDGE ( 'NONE', *, *, #38363, .F. ) ;
#42963 = VERTEX_POINT ( 'NONE', #30724 ) ;
#42964 = ORIENTED_EDGE ( 'NONE', *, *, #6871, .T. ) ;
#42965 = EDGE_LOOP ( 'NONE', ( #12163, #45414, #48433, #25300 ) ) ;
#42966 = CARTESIAN_POINT ( 'NONE',  ( 283.0000000000000568, -26.28355339059299922, 9.766446609406699508 ) ) ;
#42967 = UNCERTAINTY_MEASURE_WITH_UNIT (LENGTH_MEASURE( 1.000000000000000082E-05 ), #31784, 'distance_accuracy_value', 'NONE');
#42968 = EDGE_CURVE ( 'NONE', #13563, #29083, #25070, .T. ) ;
#42969 = EDGE_CURVE ( 'NONE', #11541, #13296, #35299, .T. ) ;
#42971 = ORIENTED_EDGE ( 'NONE', *, *, #27070, .F. ) ;
#42970 = CARTESIAN_POINT ( 'NONE',  ( 8.250000000000005329, 7.250000000000000888, -26.00000000000001066 ) ) ;
#42972 = CARTESIAN_POINT ( 'NONE',  ( -11.18999999999999950, -11.25000000000000000, -4.250000000000000000 ) ) ;
#42973 = CARTESIAN_POINT ( 'NONE',  ( 7.250000000000005329, -7.249999999999998224, -18.50000000000000000 ) ) ;
#42974 = EDGE_CURVE ( 'NONE', #32181, #57411, #8436, .T. ) ;
#42975 = AXIS2_PLACEMENT_3D ( 'NONE', #7374, #17990, #18329 ) ;
#42976 = FACE_OUTER_BOUND ( 'NONE', #68585, .T. ) ;
#42977 = ORIENTED_EDGE ( 'NONE', *, *, #62939, .T. ) ;
#42978 = DIRECTION ( 'NONE',  ( -0.000000000000000000, 3.673940397442059868E-16, -1.000000000000000000 ) ) ;
#42979 = AXIS2_PLACEMENT_3D ( 'NONE', #58398, #26914, #63340 ) ;
#42980 = DIRECTION ( 'NONE',  ( 0.000000000000000000, -1.000000000000000000, 0.000000000000000000 ) ) ;
#42981 = AXIS2_PLACEMENT_3D ( 'NONE', #43489, #37170, #4636 ) ;
#42982 = ORIENTED_EDGE ( 'NONE', *, *, #18044, .F. ) ;
#42983 = CARTESIAN_POINT ( 'NONE',  ( -7.450000000000001954, -7.249999999999998224, -17.00000000000000000 ) ) ;
#42984 = VECTOR ( 'NONE', #24452, 1000.000000000000000 ) ;
#42985 = DIRECTION ( 'NONE',  ( 0.000000000000000000, 0.000000000000000000, -1.000000000000000000 ) ) ;
#42986 = CARTESIAN_POINT ( 'NONE',  ( -11.18071654964669825, 11.99351654964660341, 195.0000000000000284 ) ) ;
#42987 = ORIENTED_EDGE ( 'NONE', *, *, #55410, .T. ) ;
#42989 = DIRECTION ( 'NONE',  ( -1.000000000000000000, 0.000000000000000000, 0.000000000000000000 ) ) ;
#42988 = AXIS2_PLACEMENT_3D ( 'NONE', #4928, #63989, #64663 ) ;
#42990 = FACE_OUTER_BOUND ( 'NONE', #21289, .T. ) ;
#42991 = FACE_OUTER_BOUND ( 'NONE', #9623, .T. ) ;
#42992 = TOROIDAL_SURFACE ( 'NONE', #13614, 0.06000000000000080963, 0.7500000000000000000 ) ;
#42993 = AXIS2_PLACEMENT_3D ( 'NONE', #43816, #10591, #5988 ) ;
#42994 = LINE ( 'NONE', #22485, #2623 ) ;
#42995 = DIRECTION ( 'NONE',  ( 0.000000000000000000, 0.000000000000000000, 1.000000000000000000 ) ) ;
#42996 = CARTESIAN_POINT ( 'NONE',  ( 290.0000000000000000, 50.00000000000000000, 26.50000000000000000 ) ) ;
#42997 = SURFACE_STYLE_FILL_AREA ( #25713 ) ;
#42998 = CARTESIAN_POINT ( 'NONE',  ( 7.250000000000005329, -7.449999999999998401, -16.00000000000000000 ) ) ;
#42999 = ORIENTED_EDGE ( 'NONE', *, *, #16058, .T. ) ;
#43000 = FACE_BOUND ( 'NONE', #38233, .T. ) ;
#43001 = LINE ( 'NONE', #20393, #24010 ) ;
#43002 = EDGE_CURVE ( 'NONE', #32778, #23370, #67851, .T. ) ;
#43003 = VECTOR ( 'NONE', #39918, 1000.000000000000000 ) ;
#43004 = DIRECTION ( 'NONE',  ( -1.000000000000000000, 0.000000000000000000, 0.000000000000000000 ) ) ;
#43005 = CYLINDRICAL_SURFACE ( 'NONE', #69173, 5.250000000000000000 ) ;
#43006 = EDGE_LOOP ( 'NONE', ( #60450, #8187, #33977, #30808 ) ) ;
#43007 = DIRECTION ( 'NONE',  ( 1.000000000000000000, -0.000000000000000000, 0.000000000000000000 ) ) ;
#43008 = DIRECTION ( 'NONE',  ( 0.000000000000000000, 0.000000000000000000, -1.000000000000000000 ) ) ;
#43009 = DIRECTION ( 'NONE',  ( 0.000000000000000000, 0.000000000000000000, -1.000000000000000000 ) ) ;
#43010 = EDGE_CURVE ( 'NONE', #22374, #36022, #29724, .T. ) ;
#43011 = CARTESIAN_POINT ( 'NONE',  ( 275.0000000000000000, -21.00000000000000000, 5.000000000000000000 ) ) ;
#43012 = CARTESIAN_POINT ( 'NONE',  ( 41.09999999999999432, 20.60000000000000142, -13.86939075806900057 ) ) ;
#43013 = DIRECTION ( 'NONE',  ( 0.000000000000000000, 0.000000000000000000, 1.000000000000000000 ) ) ;
#43014 = ORIENTED_EDGE ( 'NONE', *, *, #42007, .F. ) ;
#43015 = ORIENTED_EDGE ( 'NONE', *, *, #2366, .T. ) ;
#43016 = LINE ( 'NONE', #10152, #34934 ) ;
#43017 = AXIS2_PLACEMENT_3D ( 'NONE', #28859, #50089, #34160 ) ;
#43018 = CARTESIAN_POINT ( 'NONE',  ( 25.49999999999869971, -17.50000000000000000, 22.50000000000000000 ) ) ;
#43019 = VERTEX_POINT ( 'NONE', #41673 ) ;
#43020 = CARTESIAN_POINT ( 'NONE',  ( 15.50000000000000000, -2.500000000000000000, -23.94337567297399971 ) ) ;
#43021 = DIRECTION ( 'NONE',  ( 0.000000000000000000, 0.000000000000000000, 1.000000000000000000 ) ) ;
#43022 = ORIENTED_EDGE ( 'NONE', *, *, #6171, .T. ) ;
#43023 = ADVANCED_FACE ( 'NONE', ( #31075 ), #52656, .T. ) ;
#43024 = CARTESIAN_POINT ( 'NONE',  ( -2.693516549646780334, -10.92648345035340895, 195.0000000000000284 ) ) ;
#43025 = VERTEX_POINT ( 'NONE', #15167 ) ;
#43026 = ORIENTED_EDGE ( 'NONE', *, *, #66660, .F. ) ;
#43027 = DIRECTION ( 'NONE',  ( 0.000000000000000000, 0.000000000000000000, 1.000000000000000000 ) ) ;
#43028 = VECTOR ( 'NONE', #20111, 1000.000000000000000 ) ;
#43029 = ORIENTED_EDGE ( 'NONE', *, *, #41442, .F. ) ;
#43030 = CARTESIAN_POINT ( 'NONE',  ( 2.544523737882815162, 8.821682069070730492, 54.00000000000000711 ) ) ;
#43031 = CARTESIAN_POINT ( 'NONE',  ( 7.250000000000005329, -7.249999999999998224, -30.00000000000001066 ) ) ;
#43032 = DIRECTION ( 'NONE',  ( 0.000000000000000000, -1.000000000000000000, 0.000000000000000000 ) ) ;
#43033 = VECTOR ( 'NONE', #49075, 1000.000000000000000 ) ;
#43034 = AXIS2_PLACEMENT_3D ( 'NONE', #66452, #17670, #27255 ) ;
#43035 = MANIFOLD_SOLID_BREP ( 'LPattern1[4]', #36328 ) ;
#43036 = ORIENTED_EDGE ( 'NONE', *, *, #10471, .T. ) ;
#43037 = ORIENTED_EDGE ( 'NONE', *, *, #36928, .T. ) ;
#43038 = AXIS2_PLACEMENT_3D ( 'NONE', #50814, #56135, #29595 ) ;
#43039 = DIRECTION ( 'NONE',  ( 0.000000000000000000, 0.000000000000000000, -1.000000000000000000 ) ) ;
#43041 = LINE ( 'NONE', #9837, #36757 ) ;
#43040 = FACE_OUTER_BOUND ( 'NONE', #26794, .T. ) ;
#43042 = ORIENTED_EDGE ( 'NONE', *, *, #6972, .T. ) ;
#43043 = VERTEX_POINT ( 'NONE', #32480 ) ;
#43044 = CIRCLE ( 'NONE', #46420, 0.4999999999979551912 ) ;
#43045 = VECTOR ( 'NONE', #5905, 1000.000000000000000 ) ;
#43047 = ORIENTED_EDGE ( 'NONE', *, *, #27708, .T. ) ;
#43046 = CONTEXT_DEPENDENT_SHAPE_REPRESENTATION ( #69780, #1342 ) ;
#43048 = DIRECTION ( 'NONE',  ( -0.000000000000000000, 3.673940397442059868E-16, -1.000000000000000000 ) ) ;
#43050 = VERTEX_POINT ( 'NONE', #32805 ) ;
#43049 = DIRECTION ( 'NONE',  ( 0.000000000000000000, 0.000000000000000000, -1.000000000000000000 ) ) ;
#43051 = AXIS2_PLACEMENT_3D ( 'NONE', #20934, #25199, #68695 ) ;
#43052 = EDGE_CURVE ( 'NONE', #60243, #16269, #639, .T. ) ;
#43053 = CARTESIAN_POINT ( 'NONE',  ( -11.00000000000000000, -10.85999999999999943, 9.000000000000001776 ) ) ;
#43054 = VECTOR ( 'NONE', #19750, 1000.000000000000000 ) ;
#43055 = LINE ( 'NONE', #32465, #58838 ) ;
#43056 = ADVANCED_FACE ( 'NONE', ( #292 ), #58990, .F. ) ;
#43057 = ORIENTED_EDGE ( 'NONE', *, *, #34829, .T. ) ;
#43058 = ADVANCED_FACE ( 'NONE', ( #65344 ), #5597, .F. ) ;
#43059 = EDGE_LOOP ( 'NONE', ( #25758, #39305, #26129, #26417, #12606, #56402, #21884, #12935 ) ) ;
#43060 = CARTESIAN_POINT ( 'NONE',  ( 14.05000000000000249, -0.2000000000000000111, -22.50000000000000000 ) ) ;
#43061 = EDGE_CURVE ( 'NONE', #29674, #40641, #10546, .T. ) ;
#43062 = EDGE_LOOP ( 'NONE', ( #12309, #6997, #5309, #24761, #69059, #23695, #29042, #65912 ) ) ;
#43063 = ADVANCED_FACE ( 'NONE', ( #32121 ), #5938, .F. ) ;
#43064 = DIRECTION ( 'NONE',  ( 0.000000000000000000, 0.000000000000000000, -1.000000000000000000 ) ) ;
#43065 = CARTESIAN_POINT ( 'NONE',  ( 7.250000000000005329, -7.449999999999998401, -11.00000000000000000 ) ) ;
#43066 = ADVANCED_FACE ( 'NONE', ( #31443 ), #9870, .T. ) ;
#43067 = EDGE_CURVE ( 'NONE', #9337, #34243, #16899, .T. ) ;
#43068 = ORIENTED_EDGE ( 'NONE', *, *, #46161, .F. ) ;
#43069 = EDGE_CURVE ( 'NONE', #27985, #31340, #4562, .T. ) ;
#43070 = DIRECTION ( 'NONE',  ( 1.000000000000000000, 0.000000000000000000, 0.000000000000000000 ) ) ;
#43071 = DIRECTION ( 'NONE',  ( -1.000000000000000000, 0.000000000000000000, 0.000000000000000000 ) ) ;
#43073 = VERTEX_POINT ( 'NONE', #69943 ) ;
#43072 = DIRECTION ( 'NONE',  ( 0.7071067811865441310, -0.7071067811865510144, -2.597868168706485034E-16 ) ) ;
#43074 = ORIENTED_EDGE ( 'NONE', *, *, #46233, .T. ) ;
#43075 = DIRECTION ( 'NONE',  ( -0.000000000000000000, 3.673940397442059868E-16, -1.000000000000000000 ) ) ;
#43076 = DIRECTION ( 'NONE',  ( 1.836970198721029934E-16, 1.836970198721010706E-16, -1.000000000000000000 ) ) ;
#43077 = DIRECTION ( 'NONE',  ( 0.000000000000000000, 0.000000000000000000, 1.000000000000000000 ) ) ;
#43078 = DIRECTION ( 'NONE',  ( 8.673617379884051249E-15, 1.000000000000000000, 0.000000000000000000 ) ) ;
#43079 = DIRECTION ( 'NONE',  ( -1.000000000000000000, 0.000000000000000000, 0.000000000000000000 ) ) ;
#43080 = ORIENTED_EDGE ( 'NONE', *, *, #3720, .F. ) ;
#43081 = DIRECTION ( 'NONE',  ( 0.000000000000000000, -1.000000000000000000, 0.000000000000000000 ) ) ;
#43082 = CARTESIAN_POINT ( 'NONE',  ( 30.00000000000000000, -10.85999999999999943, -9.350000000000269651 ) ) ;
#43084 = ORIENTED_EDGE ( 'NONE', *, *, #24209, .T. ) ;
#43083 = DIRECTION ( 'NONE',  ( 1.000000000000000000, 0.000000000000000000, 0.000000000000000000 ) ) ;
#43085 = PRODUCT_DEFINITION_SHAPE ( 'NONE', 'NONE',  #30933 ) ;
#43086 = STYLED_ITEM ( 'NONE', ( #36455 ), #42691 ) ;
#43087 = CARTESIAN_POINT ( 'NONE',  ( 7.357023737882817827, -5.552858015815577808, 26.00000000000000711 ) ) ;
#43088 = LINE ( 'NONE', #16219, #63516 ) ;
#43089 = CARTESIAN_POINT ( 'NONE',  ( 40.90000000000000568, 6.123233995736766282E-16, -5.000000000000000000 ) ) ;
#43090 = ORIENTED_EDGE ( 'NONE', *, *, #54793, .F. ) ;
#43091 = DIRECTION ( 'NONE',  ( -1.000000000000000000, 0.000000000000000000, 0.000000000000000000 ) ) ;
#43092 = CARTESIAN_POINT ( 'NONE',  ( -6.817976262117261044, 9.897976262117179402, 54.00000000000000711 ) ) ;
#43093 = VERTEX_POINT ( 'NONE', #21506 ) ;
#43094 = PLANE ( 'NONE',  #53730 ) ;
#43095 = VECTOR ( 'NONE', #68513, 1000.000000000000000 ) ;
#43096 = CLOSED_SHELL ( 'NONE', ( #42933, #23305, #61608, #67790, #23916, #2328, #10777, #52559, #20323, #27843, #42076, #14263, #10091, #64764 ) ) ;
#43097 = CARTESIAN_POINT ( 'NONE',  ( 18.89999999999999858, -0.1999999999911430404, -8.864436962241481021E-12 ) ) ;
#43098 = DIRECTION ( 'NONE',  ( -1.836970198721029934E-16, 1.836970198721036590E-16, -1.000000000000000000 ) ) ;
#43099 = CARTESIAN_POINT ( 'NONE',  ( 4.456444791733522252E-16, 7.450000000000002842, -25.50000000000000355 ) ) ;
#43100 = DIRECTION ( 'NONE',  ( 1.000000000000000000, -5.981805089575194965E-17, 0.000000000000000000 ) ) ;
#43101 = VERTEX_POINT ( 'NONE', #64637 ) ;
#43102 = ORIENTED_EDGE ( 'NONE', *, *, #66179, .T. ) ;
#43103 = CARTESIAN_POINT ( 'NONE',  ( -10.91351654964670814, 2.893516549646604208, 455.0000000000000568 ) ) ;
#43104 = ORIENTED_EDGE ( 'NONE', *, *, #3490, .T. ) ;
#43105 = ORIENTED_EDGE ( 'NONE', *, *, #13399, .F. ) ;
#43106 = CARTESIAN_POINT ( 'NONE',  ( 11.78648345035337996, 4.393516549646516722, 455.0000000000000568 ) ) ;
#43107 = CIRCLE ( 'NONE', #23919, 2.458500000000000796 ) ;
#43108 = ADVANCED_FACE ( 'NONE', ( #59686 ), #43411, .F. ) ;
#43109 = DIRECTION ( 'NONE',  ( 0.6414496315691473605, 0.7671651518153083105, 0.000000000000000000 ) ) ;
#43110 = EDGE_CURVE ( 'NONE', #2257, #44787, #32024, .T. ) ;
#43111 = DIRECTION ( 'NONE',  ( 0.000000000000000000, 0.000000000000000000, 1.000000000000000000 ) ) ;
#43112 = VERTEX_POINT ( 'NONE', #58650 ) ;
#43113 = ORIENTED_EDGE ( 'NONE', *, *, #35649, .F. ) ;
#43114 = CARTESIAN_POINT ( 'NONE',  ( 7.250000000000005329, 7.250000000000000888, -20.50000000000000000 ) ) ;
#43115 = VERTEX_POINT ( 'NONE', #23927 ) ;
#43116 = ORIENTED_EDGE ( 'NONE', *, *, #40503, .T. ) ;
#43117 = CARTESIAN_POINT ( 'NONE',  ( -29.50000000000000355, -11.50000000000000000, 11.00000000000000000 ) ) ;
#43118 = FACE_OUTER_BOUND ( 'NONE', #59838, .T. ) ;
#43119 = DIRECTION ( 'NONE',  ( -1.000000000000000000, 0.000000000000000000, 0.000000000000000000 ) ) ;
#43120 = VECTOR ( 'NONE', #25602, 1000.000000000000000 ) ;
#43121 = EDGE_CURVE ( 'NONE', #10117, #27398, #50100, .T. ) ;
#43122 = ORIENTED_EDGE ( 'NONE', *, *, #55420, .F. ) ;
#43123 = DIRECTION ( 'NONE',  ( 1.000000000000000000, -0.000000000000000000, -0.000000000000000000 ) ) ;
#43125 = CARTESIAN_POINT ( 'NONE',  ( 6.364920264886846368, 3.663616288756996298, 26.00000000000000711 ) ) ;
#43124 = CARTESIAN_POINT ( 'NONE',  ( 41.09999999999999432, 13.66939075806899950, 20.80000000000000426 ) ) ;
#43126 = VERTEX_POINT ( 'NONE', #66375 ) ;
#43127 = ORIENTED_EDGE ( 'NONE', *, *, #47251, .T. ) ;
#43129 = VERTEX_POINT ( 'NONE', #12954 ) ;
#43128 = CARTESIAN_POINT ( 'NONE',  ( 3.848229544836325289, 7.517976262117209707, 26.00000000000000711 ) ) ;
#43130 = EDGE_LOOP ( 'NONE', ( #943, #37821, #28156, #53245 ) ) ;
#43131 = EDGE_CURVE ( 'NONE', #46953, #31241, #60356, .T. ) ;
#43132 = DIRECTION ( 'NONE',  ( 0.000000000000000000, -3.673940397442059868E-16, 1.000000000000000000 ) ) ;
#43133 = CIRCLE ( 'NONE', #9225, 0.5249999999999994671 ) ;
#43134 = CARTESIAN_POINT ( 'NONE',  ( 283.0000000000000568, -25.00000000000299849, -9.079999998829670460 ) ) ;
#43135 = EDGE_CURVE ( 'NONE', #49649, #41718, #60714, .T. ) ;
#43136 = ORIENTED_EDGE ( 'NONE', *, *, #68111, .T. ) ;
#43137 = VERTEX_POINT ( 'NONE', #44105 ) ;
#43138 = DIRECTION ( 'NONE',  ( -0.000000000000000000, -0.000000000000000000, -1.000000000000000000 ) ) ;
#43139 = DIRECTION ( 'NONE',  ( 0.000000000000000000, 1.000000000000000000, 0.000000000000000000 ) ) ;
#43140 = ORIENTED_EDGE ( 'NONE', *, *, #35033, .T. ) ;
#43141 = CIRCLE ( 'NONE', #23950, 24.99999999998784972 ) ;
#43142 = VERTEX_POINT ( 'NONE', #6625 ) ;
#43143 = DIRECTION ( 'NONE',  ( 0.000000000000000000, 0.000000000000000000, 1.000000000000000000 ) ) ;
#43144 = DIRECTION ( 'NONE',  ( 0.000000000000000000, 0.000000000000000000, -1.000000000000000000 ) ) ;
#43145 = ADVANCED_FACE ( 'NONE', ( #66710 ), #996, .F. ) ;
#43146 = CARTESIAN_POINT ( 'NONE',  ( 12.00648345035340903, 7.813516549646560172, 455.0000000000000568 ) ) ;
#43147 = VERTEX_POINT ( 'NONE', #12257 ) ;
#43148 = AXIS2_PLACEMENT_3D ( 'NONE', #18661, #7004, #1373 ) ;
#43149 = EDGE_CURVE ( 'NONE', #14943, #48678, #33148, .T. ) ;
#43151 = MANIFOLD_SOLID_BREP ( 'LPattern1[17]', #17148 ) ;
#43150 = DIRECTION ( 'NONE',  ( 1.000000000000000000, -1.047444401652939849E-14, 0.000000000000000000 ) ) ;
#43152 = DIRECTION ( 'NONE',  ( 0.000000000000000000, 0.7071067811865474617, -0.7071067811865474617 ) ) ;
#43154 = EDGE_LOOP ( 'NONE', ( #21013, #53494, #40907, #5668 ) ) ;
#43153 = DIRECTION ( 'NONE',  ( -1.000000000000000000, 0.000000000000000000, 0.000000000000000000 ) ) ;
#43156 = ORIENTED_EDGE ( 'NONE', *, *, #11665, .F. ) ;
#43155 = CARTESIAN_POINT ( 'NONE',  ( -8.250000000000000000, 7.250000000000001776, -21.00000000000000000 ) ) ;
#43158 = DIRECTION ( 'NONE',  ( -1.836970198721029934E-16, -1.836970198721010706E-16, 1.000000000000000000 ) ) ;
#43157 = VECTOR ( 'NONE', #36755, 1000.000000000000000 ) ;
#43159 = LINE ( 'NONE', #42470, #54400 ) ;
#43160 = EDGE_CURVE ( 'NONE', #20722, #48934, #23228, .T. ) ;
#43161 = LINE ( 'NONE', #37868, #60670 ) ;
#43162 = LINE ( 'NONE', #64736, #13211 ) ;
#43163 = DIRECTION ( 'NONE',  ( 1.000000000000000000, 1.570596175624152290E-15, 5.770276737693577136E-31 ) ) ;
#43164 = FACE_OUTER_BOUND ( 'NONE', #69787, .T. ) ;
#43165 = ORIENTED_EDGE ( 'NONE', *, *, #64378, .F. ) ;
#43166 = CARTESIAN_POINT ( 'NONE',  ( 8.250000000000005329, 7.250000000000000888, -7.500000000000000000 ) ) ;
#43168 = ORIENTED_EDGE ( 'NONE', *, *, #47417, .T. ) ;
#43167 = CARTESIAN_POINT ( 'NONE',  ( 4.622483450353380263, -3.606483450353491271, 455.0000000000000568 ) ) ;
#43170 = ORIENTED_EDGE ( 'NONE', *, *, #32352, .F. ) ;
#43169 = CYLINDRICAL_SURFACE ( 'NONE', #15246, 4.000000000000000000 ) ;
#43171 = LINE ( 'NONE', #49182, #7536 ) ;
#43172 = DIRECTION ( 'NONE',  ( -0.000000000000000000, -0.000000000000000000, 1.000000000000000000 ) ) ;
#43173 = ORIENTED_EDGE ( 'NONE', *, *, #4899, .T. ) ;
#43174 = DIRECTION ( 'NONE',  ( 0.000000000000000000, 0.000000000000000000, -1.000000000000000000 ) ) ;
#43175 = LINE ( 'NONE', #54501, #50898 ) ;
#43176 = CIRCLE ( 'NONE', #10470, 0.2000000000000005107 ) ;
#43177 = VERTEX_POINT ( 'NONE', #28871 ) ;
#43178 = EDGE_CURVE ( 'NONE', #24440, #41462, #49761, .T. ) ;
#43179 = FACE_OUTER_BOUND ( 'NONE', #25637, .T. ) ;
#43180 = DIRECTION ( 'NONE',  ( 0.000000000000000000, 0.000000000000000000, 1.000000000000000000 ) ) ;
#43181 = CARTESIAN_POINT ( 'NONE',  ( -24.00000000000000000, -16.28999999999999915, -14.50000000000000000 ) ) ;
#43182 = VECTOR ( 'NONE', #58995, 1000.000000000000000 ) ;
#43183 = EDGE_CURVE ( 'NONE', #30940, #22451, #44436, .T. ) ;
#43184 = EDGE_LOOP ( 'NONE', ( #65219, #11734, #34478, #10670 ) ) ;
#43185 = DIRECTION ( 'NONE',  ( -0.7071067811865391350, 0.7071067811865560104, 1.750285133459120294E-30 ) ) ;
#43186 = ORIENTED_EDGE ( 'NONE', *, *, #6953, .T. ) ;
#43187 = ADVANCED_FACE ( 'NONE', ( #18261 ), #56109, .T. ) ;
#43188 = VERTEX_POINT ( 'NONE', #11566 ) ;
#43189 = VECTOR ( 'NONE', #38944, 1000.000000000000000 ) ;
#43190 = CARTESIAN_POINT ( 'NONE',  ( 8.211283450353379365, -6.006483450353490738, 455.0000000000000568 ) ) ;
#43191 = DIRECTION ( 'NONE',  ( 0.000000000000000000, 0.000000000000000000, 1.000000000000000000 ) ) ;
#43192 = ADVANCED_FACE ( 'NONE', ( #1328, #39152 ), #45481, .T. ) ;
#43193 = VECTOR ( 'NONE', #51737, 1000.000000000000000 ) ;
#43194 = CARTESIAN_POINT ( 'NONE',  ( -7.250000000000000888, 7.250000000000001776, -26.00000000000001066 ) ) ;
#43195 = EDGE_CURVE ( 'NONE', #55585, #34045, #2361, .T. ) ;
#43196 = LINE ( 'NONE', #21983, #57780 ) ;
#43197 = VERTEX_POINT ( 'NONE', #61758 ) ;
#43198 = ORIENTED_EDGE ( 'NONE', *, *, #65542, .F. ) ;
#43200 = ORIENTED_EDGE ( 'NONE', *, *, #52564, .F. ) ;
#43199 = DIRECTION ( 'NONE',  ( 1.000000000000000000, -0.000000000000000000, -0.000000000000000000 ) ) ;
#43201 = EDGE_LOOP ( 'NONE', ( #45803, #14651, #7647, #8791 ) ) ;
#43202 = DIRECTION ( 'NONE',  ( -0.000000000000000000, 1.000000000000000000, -0.000000000000000000 ) ) ;
#43203 = VECTOR ( 'NONE', #52235, 999.9999999999998863 ) ;
#43204 = CYLINDRICAL_SURFACE ( 'NONE', #42206, 0.5000000000079367624 ) ;
#43205 = LINE ( 'NONE', #53487, #7093 ) ;
#43206 = ADVANCED_FACE ( 'NONE', ( #18615 ), #35215, .F. ) ;
#43207 = EDGE_CURVE ( 'NONE', #8437, #33149, #49130, .T. ) ;
#43208 = CIRCLE ( 'NONE', #15001, 1.224999999999997868 ) ;
#43209 = DIRECTION ( 'NONE',  ( 0.000000000000000000, -0.000000000000000000, -1.000000000000000000 ) ) ;
#43211 = LINE ( 'NONE', #31577, #34544 ) ;
#43210 = FACE_OUTER_BOUND ( 'NONE', #30153, .T. ) ;
#43212 = AXIS2_PLACEMENT_3D ( 'NONE', #67924, #62973, #8513 ) ;
#43213 = ORIENTED_EDGE ( 'NONE', *, *, #52783, .T. ) ;
#43215 = ORIENTED_EDGE ( 'NONE', *, *, #53936, .T. ) ;
#43214 = LINE ( 'NONE', #60513, #63490 ) ;
#43216 = EDGE_LOOP ( 'NONE', ( #68033, #32118, #49532, #54511, #23654, #6498, #23722, #24007, #5569, #1945 ) ) ;
#43217 = VERTEX_POINT ( 'NONE', #36289 ) ;
#43218 = EDGE_CURVE ( 'NONE', #29125, #26913, #51858, .T. ) ;
#43219 = ADVANCED_FACE ( 'NONE', ( #13317 ), #25333, .F. ) ;
#43220 = DIRECTION ( 'NONE',  ( 1.000000000000000000, -8.728482790395504563E-15, 0.000000000000000000 ) ) ;
#43221 = VECTOR ( 'NONE', #45942, 1000.000000000000000 ) ;
#43222 = CARTESIAN_POINT ( 'NONE',  ( 49.00000000000000000, -21.00000000000000000, 13.86939075806900057 ) ) ;
#43223 = EDGE_CURVE ( 'NONE', #45713, #8019, #34869, .T. ) ;
#43224 =( NAMED_UNIT ( * ) SI_UNIT ( $, .STERADIAN. ) SOLID_ANGLE_UNIT ( ) );
#43225 = DIRECTION ( 'NONE',  ( -1.000000000000000000, 0.000000000000000000, 0.000000000000000000 ) ) ;
#43226 = VECTOR ( 'NONE', #24446, 1000.000000000000114 ) ;
#43227 = ORIENTED_EDGE ( 'NONE', *, *, #30443, .F. ) ;
#43228 = ORIENTED_EDGE ( 'NONE', *, *, #9602, .F. ) ;
#43229 = ORIENTED_EDGE ( 'NONE', *, *, #11487, .F. ) ;
#43230 = LINE ( 'NONE', #61115, #61017 ) ;
#43231 = FACE_OUTER_BOUND ( 'NONE', #32982, .T. ) ;
#43232 = DIRECTION ( 'NONE',  ( -0.000000000000000000, -0.000000000000000000, -1.000000000000000000 ) ) ;
#43233 = ORIENTED_EDGE ( 'NONE', *, *, #32605, .T. ) ;
#43234 = EDGE_LOOP ( 'NONE', ( #53044, #62430, #38286, #38598 ) ) ;
#43235 = LINE ( 'NONE', #4385, #3428 ) ;
#43236 = EDGE_CURVE ( 'NONE', #4021, #43477, #56794, .T. ) ;
#43237 = DIRECTION ( 'NONE',  ( 0.000000000000000000, 0.000000000000000000, -1.000000000000000000 ) ) ;
#43238 = EDGE_LOOP ( 'NONE', ( #49243, #44477, #63501, #26227 ) ) ;
#43239 = EDGE_CURVE ( 'NONE', #43994, #31863, #2700, .T. ) ;
#43240 = DIRECTION ( 'NONE',  ( -1.000000000000000000, 0.000000000000000000, 0.000000000000000000 ) ) ;
#43241 = CIRCLE ( 'NONE', #347, 0.3499999999999996447 ) ;
#43243 = ORIENTED_EDGE ( 'NONE', *, *, #68435, .F. ) ;
#43242 = DIRECTION ( 'NONE',  ( 0.000000000000000000, 0.000000000000000000, 1.000000000000000000 ) ) ;
#43244 = ORIENTED_EDGE ( 'NONE', *, *, #16600, .T. ) ;
#43245 = DIRECTION ( 'NONE',  ( -1.000000000000000000, 8.728482790395504563E-15, 0.000000000000000000 ) ) ;
#43246 = LINE ( 'NONE', #65849, #21045 ) ;
#43247 = CARTESIAN_POINT ( 'NONE',  ( 0.000000000000000000, -7.449999999999998401, -18.50000000000000000 ) ) ;
#43248 = CARTESIAN_POINT ( 'NONE',  ( 15.91242688423647955, -0.3152598339557988183, 23.70526090033903799 ) ) ;
#43249 = CARTESIAN_POINT ( 'NONE',  ( 283.0000000000000568, -30.80000000000000071, -12.20000000000000107 ) ) ;
#43250 = ORIENTED_EDGE ( 'NONE', *, *, #30977, .T. ) ;
#43251 = DIRECTION ( 'NONE',  ( -1.000000000000000000, 0.000000000000000000, 0.000000000000000000 ) ) ;
#43252 = ORIENTED_EDGE ( 'NONE', *, *, #28749, .T. ) ;
#43253 = CARTESIAN_POINT ( 'NONE',  ( -29.50000000000000355, -11.50000000000000000, -11.00000000000000000 ) ) ;
#43254 = AXIS2_PLACEMENT_3D ( 'NONE', #60156, #1125, #39285 ) ;
#43255 = DIRECTION ( 'NONE',  ( 1.000000000000000000, -0.000000000000000000, -0.000000000000000000 ) ) ;
#43256 = DIRECTION ( 'NONE',  ( 0.000000000000000000, -1.000000000000000000, 0.000000000000000000 ) ) ;
#43258 = CARTESIAN_POINT ( 'NONE',  ( -1.677516549646816291, -9.841277389592811176, 455.0000000000000568 ) ) ;
#43257 = AXIS2_PLACEMENT_3D ( 'NONE', #62560, #3540, #51973 ) ;
#43259 = MECHANICAL_DESIGN_GEOMETRIC_PRESENTATION_REPRESENTATION (  '', ( #68089 ), #12744 ) ;
#43260 = LINE ( 'NONE', #16393, #43819 ) ;
#43261 = VERTEX_POINT ( 'NONE', #62809 ) ;
#43262 = FACE_OUTER_BOUND ( 'NONE', #44929, .T. ) ;
#43263 = AXIS2_PLACEMENT_3D ( 'NONE', #45491, #18983, #39494 ) ;
#43264 = CARTESIAN_POINT ( 'NONE',  ( -4.947141984184539432, -7.357023737882807168, 54.00000000000000711 ) ) ;
#43265 = ADVANCED_FACE ( 'NONE', ( #3414 ), #40533, .F. ) ;
#43266 = VECTOR ( 'NONE', #43840, 1000.000000000000000 ) ;
#43267 = ORIENTED_EDGE ( 'NONE', *, *, #54492, .T. ) ;
#43268 = MANIFOLD_SOLID_BREP ( 'Move Face1[1]', #61136 ) ;
#43269 = CARTESIAN_POINT ( 'NONE',  ( -30.00000000000000000, -5.000000000000000000, -27.00000000000000000 ) ) ;
#43270 = CARTESIAN_POINT ( 'NONE',  ( 7.250000000000005329, -7.249999999999998224, -14.00000000000000000 ) ) ;
#43271 = ADVANCED_FACE ( 'NONE', ( #30292 ), #40883, .F. ) ;
#43272 = EDGE_LOOP ( 'NONE', ( #12974, #19904, #36524, #59397 ) ) ;
#43273 = DIRECTION ( 'NONE',  ( 0.000000000000000000, 0.000000000000000000, -1.000000000000000000 ) ) ;
#43274 = CARTESIAN_POINT ( 'NONE',  ( 0.000000000000000000, -7.449999999999998401, -11.50000000000000000 ) ) ;
#43275 = ORIENTED_EDGE ( 'NONE', *, *, #62750, .T. ) ;
#43276 = CARTESIAN_POINT ( 'NONE',  ( -9.189999999999999503, -9.750000000000001776, -5.000000000000000000 ) ) ;
#43277 = EDGE_CURVE ( 'NONE', #29771, #30686, #22031, .T. ) ;
#43278 = VECTOR ( 'NONE', #64767, 1000.000000000000000 ) ;
#43279 = EDGE_CURVE ( 'NONE', #5119, #54829, #52565, .T. ) ;
#43280 = CARTESIAN_POINT ( 'NONE',  ( 7.000000000000000000, -26.06132420600899735, 10.13999572156699891 ) ) ;
#43281 =( LENGTH_UNIT ( ) NAMED_UNIT ( * ) SI_UNIT ( .MILLI., .METRE. ) );
#43282 = EDGE_CURVE ( 'NONE', #43722, #54865, #6478, .T. ) ;
#43283 = DIRECTION ( 'NONE',  ( 0.000000000000000000, -1.000000000000000000, 0.000000000000000000 ) ) ;
#43284 = EDGE_CURVE ( 'NONE', #63336, #56487, #27689, .T. ) ;
#43285 = AXIS2_PLACEMENT_3D ( 'NONE', #33984, #19383, #40950 ) ;
#43286 = ORIENTED_EDGE ( 'NONE', *, *, #6029, .F. ) ;
#43288 = VERTEX_POINT ( 'NONE', #26042 ) ;
#43287 = CARTESIAN_POINT ( 'NONE',  ( 34.89999999999999858, -0.2000000000089119934, 8.909539772616881237E-12 ) ) ;
#43289 = LINE ( 'NONE', #27383, #65505 ) ;
#43290 = FACE_OUTER_BOUND ( 'NONE', #10029, .T. ) ;
#43291 = PLANE ( 'NONE',  #55612 ) ;
#43292 = VERTEX_POINT ( 'NONE', #28038 ) ;
#43293 = VECTOR ( 'NONE', #33894, 1000.000000000000000 ) ;
#43294 = CARTESIAN_POINT ( 'NONE',  ( 7.250000000000005329, 7.250000000000000888, -14.50000000000000000 ) ) ;
#43295 = CARTESIAN_POINT ( 'NONE',  ( 10.50702373788278265, 3.650476262117142934, 54.00000000000000711 ) ) ;
#43296 = ORIENTED_EDGE ( 'NONE', *, *, #52829, .F. ) ;
#43297 = ORIENTED_EDGE ( 'NONE', *, *, #5300, .T. ) ;
#43298 = VERTEX_POINT ( 'NONE', #54573 ) ;
#43299 = CARTESIAN_POINT ( 'NONE',  ( 1.690483450353344352, -10.74648345035336128, 195.0000000000000284 ) ) ;
#43300 = CARTESIAN_POINT ( 'NONE',  ( 39.00000000000000000, 0.000000000000000000, 0.000000000000000000 ) ) ;
#43301 = SHAPE_REPRESENTATION_RELATIONSHIP ( 'NONE' , 'NONE' ,  #35, #21682 ) ;
#43302 = VECTOR ( 'NONE', #15968, 1000.000000000000114 ) ;
#43303 = CIRCLE ( 'NONE', #52347, 25.39999999999999858 ) ;
#43304 = EDGE_LOOP ( 'NONE', ( #53288, #37898, #67238, #22828 ) ) ;
#43305 = ORIENTED_EDGE ( 'NONE', *, *, #50785, .T. ) ;
#43306 = VERTEX_POINT ( 'NONE', #47948 ) ;
#43307 = VECTOR ( 'NONE', #66739, 1000.000000000000000 ) ;
#43308 = CARTESIAN_POINT ( 'NONE',  ( -29.50000000000000355, -12.00000000000000000, -11.00000000000000000 ) ) ;
#43309 = VERTEX_POINT ( 'NONE', #38984 ) ;
#43310 = VECTOR ( 'NONE', #13265, 1000.000000000000114 ) ;
#43311 = EDGE_LOOP ( 'NONE', ( #29608, #33404, #5645, #58344 ) ) ;
#43312 = ORIENTED_EDGE ( 'NONE', *, *, #22793, .F. ) ;
#43313 = ORIENTED_EDGE ( 'NONE', *, *, #32325, .T. ) ;
#43314 = DIRECTION ( 'NONE',  ( 0.000000000000000000, 0.000000000000000000, 1.000000000000000000 ) ) ;
#43315 = VECTOR ( 'NONE', #1654, 1000.000000000000000 ) ;
#43316 = CIRCLE ( 'NONE', #46692, 0.1999999999999996503 ) ;
#43318 = ORIENTED_EDGE ( 'NONE', *, *, #27055, .T. ) ;
#43317 = CARTESIAN_POINT ( 'NONE',  ( 7.450000000000003730, -7.249999999999997335, -20.00000000000000000 ) ) ;
#43319 = CARTESIAN_POINT ( 'NONE',  ( -7.878491296477273309, 5.098491296477203782, 195.0000000000000284 ) ) ;
#43320 = EDGE_CURVE ( 'NONE', #28252, #1208, #31062, .T. ) ;
#43321 = LINE ( 'NONE', #44689, #26179 ) ;
#43322 = DIRECTION ( 'NONE',  ( -1.000000000000000000, 0.000000000000000000, 0.000000000000000000 ) ) ;
#43323 = EDGE_CURVE ( 'NONE', #32671, #52471, #842, .T. ) ;
#43324 = ORIENTED_EDGE ( 'NONE', *, *, #8588, .T. ) ;
#43325 = DIRECTION ( 'NONE',  ( 0.000000000000000000, 0.000000000000000000, 1.000000000000000000 ) ) ;
#43326 = DIRECTION ( 'NONE',  ( 0.000000000000000000, 1.000000000000000000, 0.000000000000000000 ) ) ;
#43327 = ORIENTED_EDGE ( 'NONE', *, *, #3664, .T. ) ;
#43328 = FACE_OUTER_BOUND ( 'NONE', #47109, .T. ) ;
#43329 = CARTESIAN_POINT ( 'NONE',  ( 69.92576880110416937, 10.00000000000000000, 335.4830310981152479 ) ) ;
#43330 = CARTESIAN_POINT ( 'NONE',  ( 9.249999999999998224, 8.250000000000001776, 5.000000000000000000 ) ) ;
#43331 = ORIENTED_EDGE ( 'NONE', *, *, #53138, .F. ) ;
#43332 = LINE ( 'NONE', #53273, #6468 ) ;
#43333 = DIRECTION ( 'NONE',  ( -1.000000000000000000, 0.000000000000000000, 0.000000000000000000 ) ) ;
#43334 = LINE ( 'NONE', #53969, #25715 ) ;
#43335 = CARTESIAN_POINT ( 'NONE',  ( 10.50702373788281996, -3.664523737882826815, 54.00000000000000711 ) ) ;
#43336 = CARTESIAN_POINT ( 'NONE',  ( 16.89999999999999858, -21.00000000000000000, 13.86939075806900057 ) ) ;
#43337 = DIRECTION ( 'NONE',  ( -1.047444401652940007E-14, -1.000000000000000000, -1.836970198721029934E-16 ) ) ;
#43338 = CARTESIAN_POINT ( 'NONE',  ( -4.135079735113209587, -6.836383711242997485, 26.00000000000000711 ) ) ;
#43339 = EDGE_CURVE ( 'NONE', #48215, #51726, #28372, .T. ) ;
#43340 = VECTOR ( 'NONE', #29594, 1000.000000000000000 ) ;
#43341 = VECTOR ( 'NONE', #53578, 1000.000000000000000 ) ;
#43342 = ORIENTED_EDGE ( 'NONE', *, *, #59513, .F. ) ;
#43343 = DIRECTION ( 'NONE',  ( 0.000000000000000000, 0.000000000000000000, -1.000000000000000000 ) ) ;
#43344 = CARTESIAN_POINT ( 'NONE',  ( -1.677516549646676625, 10.73351654964656987, 195.0000000000000284 ) ) ;
#43345 = CARTESIAN_POINT ( 'NONE',  ( 8.606483450353380249, -4.396432944014657451, 455.0000000000000568 ) ) ;
#43346 = CARTESIAN_POINT ( 'NONE',  ( 6.500000000000002665, 6.500000000000000888, -1.000000000000000000 ) ) ;
#43347 = CIRCLE ( 'NONE', #64825, 0.1999999999999987899 ) ;
#43348 = ORIENTED_EDGE ( 'NONE', *, *, #1750, .F. ) ;
#43349 = CIRCLE ( 'NONE', #65908, 25.39999999999999858 ) ;
#43350 = DIRECTION ( 'NONE',  ( 0.000000000000000000, 0.000000000000000000, 1.000000000000000000 ) ) ;
#43351 = CARTESIAN_POINT ( 'NONE',  ( -4.393516549646667713, 11.77351654964658856, 195.0000000000000284 ) ) ;
#43352 = ADVANCED_FACE ( 'NONE', ( #68819 ), #63524, .F. ) ;
#43353 = EDGE_CURVE ( 'NONE', #10322, #20182, #69516, .T. ) ;
#43354 = CARTESIAN_POINT ( 'NONE',  ( -13.00000000000000178, -16.64230188589299786, -14.64519951917100116 ) ) ;
#43355 = LINE ( 'NONE', #58935, #9581 ) ;
#43356 = VECTOR ( 'NONE', #1529, 1000.000000000000000 ) ;
#43358 = VECTOR ( 'NONE', #9982, 1000.000000000000114 ) ;
#43357 = DIRECTION ( 'NONE',  ( 1.836970198721029934E-16, 1.836970198721010706E-16, -1.000000000000000000 ) ) ;
#43359 = ADVANCED_FACE ( 'NONE', ( #53270 ), #22395, .T. ) ;
#43360 = DIRECTION ( 'NONE',  ( -1.000000000000000000, 0.000000000000000000, 0.000000000000000000 ) ) ;
#43361 = EDGE_CURVE ( 'NONE', #68958, #69246, #4820, .T. ) ;
#43362 = ORIENTED_EDGE ( 'NONE', *, *, #25202, .T. ) ;
#43363 = ORIENTED_EDGE ( 'NONE', *, *, #63155, .T. ) ;
#43364 = EDGE_CURVE ( 'NONE', #9367, #40219, #49599, .T. ) ;
#43365 = LINE ( 'NONE', #5894, #57513 ) ;
#43366 = DIRECTION ( 'NONE',  ( 0.000000000000000000, -1.000000000000000000, 0.000000000000000000 ) ) ;
#43367 = ORIENTED_EDGE ( 'NONE', *, *, #9036, .F. ) ;
#43368 = FACE_OUTER_BOUND ( 'NONE', #61433, .T. ) ;
#43369 = VECTOR ( 'NONE', #11713, 1000.000000000000000 ) ;
#43370 = CARTESIAN_POINT ( 'NONE',  ( 6.849523737882818430, 10.49297626211719603, 54.00000000000000711 ) ) ;
#43371 = VERTEX_POINT ( 'NONE', #10121 ) ;
#43372 = DIRECTION ( 'NONE',  ( 1.000000000000000000, 0.000000000000000000, 0.000000000000000000 ) ) ;
#43373 = ORIENTED_EDGE ( 'NONE', *, *, #52076, .F. ) ;
#43374 = ORIENTED_EDGE ( 'NONE', *, *, #20933, .F. ) ;
#43375 = CARTESIAN_POINT ( 'NONE',  ( 0.000000000000000000, 0.000000000000000000, -20.50000000000000000 ) ) ;
#43376 = ORIENTED_EDGE ( 'NONE', *, *, #26365, .T. ) ;
#43377 = DIRECTION ( 'NONE',  ( 0.6414496315691617934, 0.7671651518152962090, 0.000000000000000000 ) ) ;
#43378 = DIRECTION ( 'NONE',  ( 7.751221965937476285E-17, 1.000000000000000000, -0.000000000000000000 ) ) ;
#43379 = CARTESIAN_POINT ( 'NONE',  ( 38.90000000000000568, -0.1999999999911430404, -8.864436962241481021E-12 ) ) ;
#43380 = MANIFOLD_SOLID_BREP ( 'LPattern1[11]', #57781 ) ;
#43381 = ORIENTED_EDGE ( 'NONE', *, *, #37544, .F. ) ;
#43382 = ORIENTED_EDGE ( 'NONE', *, *, #21976, .F. ) ;
#43383 = CARTESIAN_POINT ( 'NONE',  ( 14.25000000000000000, -2.500000000000000000, 23.22168783648699986 ) ) ;
#43385 = LINE ( 'NONE', #64969, #39504 ) ;
#43384 = CARTESIAN_POINT ( 'NONE',  ( 7.357023737882817827, -6.665817930929295088, 26.00000000000000000 ) ) ;
#43386 = ORIENTED_EDGE ( 'NONE', *, *, #3609, .F. ) ;
#43387 = AXIS2_PLACEMENT_3D ( 'NONE', #41704, #53034, #47712 ) ;
#43388 = ORIENTED_EDGE ( 'NONE', *, *, #63743, .F. ) ;
#43390 = ORIENTED_EDGE ( 'NONE', *, *, #16010, .T. ) ;
#43389 = CONTEXT_DEPENDENT_SHAPE_REPRESENTATION ( #33195, #56127 ) ;
#43391 = CARTESIAN_POINT ( 'NONE',  ( 7.265214908726153276, 6.606374702650035680, 455.0000000000000568 ) ) ;
#43393 = ORIENTED_EDGE ( 'NONE', *, *, #69806, .F. ) ;
#43392 = DIRECTION ( 'NONE',  ( -1.000000000000000000, 0.000000000000000000, 0.000000000000000000 ) ) ;
#43394 = DIRECTION ( 'NONE',  ( 0.000000000000000000, 1.000000000000000000, 0.000000000000000000 ) ) ;
#43395 = CIRCLE ( 'NONE', #67110, 0.7112000000000124889 ) ;
#43396 = CIRCLE ( 'NONE', #12884, 1.224999999999999423 ) ;
#43397 = LINE ( 'NONE', #28177, #41862 ) ;
#43398 = ORIENTED_EDGE ( 'NONE', *, *, #27545, .T. ) ;
#43399 = ORIENTED_EDGE ( 'NONE', *, *, #42479, .F. ) ;
#43400 = EDGE_CURVE ( 'NONE', #62836, #2764, #24284, .T. ) ;
#43401 = EDGE_CURVE ( 'NONE', #12841, #5665, #65523, .T. ) ;
#43402 = VECTOR ( 'NONE', #32600, 1000.000000000000000 ) ;
#43403 = DIRECTION ( 'NONE',  ( -0.000000000000000000, -0.000000000000000000, -1.000000000000000000 ) ) ;
#43404 = EDGE_LOOP ( 'NONE', ( #65724, #36054, #51605, #41946 ) ) ;
#43405 = EDGE_CURVE ( 'NONE', #17638, #4595, #55943, .T. ) ;
#43406 = LINE ( 'NONE', #49065, #12289 ) ;
#43407 = CARTESIAN_POINT ( 'NONE',  ( 28.90000000000000213, 13.66939075806899950, 20.80000000000000426 ) ) ;
#43408 = VECTOR ( 'NONE', #13007, 1000.000000000000000 ) ;
#43409 = EDGE_LOOP ( 'NONE', ( #44001, #52603, #557, #55466, #8849, #39382, #32349, #39605, #28539, #42681, #4583, #18885, #65901, #67701, #52191, #10570, #68332, #56958 ) ) ;
#43410 = PLANE ( 'NONE',  #16607 ) ;
#43412 = ORIENTED_EDGE ( 'NONE', *, *, #51003, .T. ) ;
#43411 = CYLINDRICAL_SURFACE ( 'NONE', #50064, 0.1749999999999993783 ) ;
#43413 = ORIENTED_EDGE ( 'NONE', *, *, #15986, .T. ) ;
#43414 = CIRCLE ( 'NONE', #54734, 1.000000000000000000 ) ;
#43415 = CARTESIAN_POINT ( 'NONE',  ( 39.90000000000000568, -14.48845687959340012, -21.00000000000000000 ) ) ;
#43416 = LINE ( 'NONE', #43777, #31895 ) ;
#43417 = CYLINDRICAL_SURFACE ( 'NONE', #22336, 0.3500000000009988455 ) ;
#43418 = CARTESIAN_POINT ( 'NONE',  ( 275.0000000000000000, -31.30000000000045191, -8.900000000000430234 ) ) ;
#43419 = CARTESIAN_POINT ( 'NONE',  ( 25.90000000000000213, 0.000000000000000000, 1.939442395502021001E-15 ) ) ;
#43420 = ORIENTED_EDGE ( 'NONE', *, *, #18040, .T. ) ;
#43421 = LINE ( 'NONE', #11242, #55014 ) ;
#43422 = CARTESIAN_POINT ( 'NONE',  ( 4.186483450353335023, -12.00648345035347830, 455.0000000000000568 ) ) ;
#43423 = CARTESIAN_POINT ( 'NONE',  ( -17.00000000000000000, -17.50000000000000000, 15.70500000000000007 ) ) ;
#43425 = VERTEX_POINT ( 'NONE', #56639 ) ;
#43424 = DIRECTION ( 'NONE',  ( -1.000000000000000000, 0.000000000000000000, 0.000000000000000000 ) ) ;
#43426 = CARTESIAN_POINT ( 'NONE',  ( -10.49297626211729551, -6.849523737882748264, 54.00000000000000711 ) ) ;
#43427 = FACE_BOUND ( 'NONE', #60992, .T. ) ;
#43428 = AXIS2_PLACEMENT_3D ( 'NONE', #63296, #64681, #57983 ) ;
#43429 = FACE_OUTER_BOUND ( 'NONE', #34142, .T. ) ;
#43430 = FACE_OUTER_BOUND ( 'NONE', #442, .T. ) ;
#43431 = ORIENTED_EDGE ( 'NONE', *, *, #63833, .F. ) ;
#43432 = DIRECTION ( 'NONE',  ( 0.000000000000000000, 0.000000000000000000, 1.000000000000000000 ) ) ;
#43433 = CYLINDRICAL_SURFACE ( 'NONE', #2, 0.4999999999979829468 ) ;
#43434 = AXIS2_PLACEMENT_3D ( 'NONE', #34897, #56478, #8026 ) ;
#43435 = ORIENTED_EDGE ( 'NONE', *, *, #27244, .T. ) ;
#43436 = CARTESIAN_POINT ( 'NONE',  ( -1.466476262117315743, -8.612468434717266419, 54.00000000000000711 ) ) ;
#43437 = DIRECTION ( 'NONE',  ( 0.000000000000000000, 0.000000000000000000, -1.000000000000000000 ) ) ;
#43438 = DIRECTION ( 'NONE',  ( 0.000000000000000000, 1.000000000000000000, 0.000000000000000000 ) ) ;
#43439 = DIRECTION ( 'NONE',  ( 0.000000000000000000, -0.1111111111108840643, -0.9938079899999319178 ) ) ;
#43440 = EDGE_CURVE ( 'NONE', #21439, #25606, #64932, .T. ) ;
#43441 = CARTESIAN_POINT ( 'NONE',  ( 12.00000000000000000, 11.18999999999999950, -4.250000000000000000 ) ) ;
#43442 = VECTOR ( 'NONE', #63004, 1000.000000000000000 ) ;
#43443 = AXIS2_PLACEMENT_3D ( 'NONE', #25134, #62599, #57657 ) ;
#43444 = ORIENTED_EDGE ( 'NONE', *, *, #42329, .F. ) ;
#43445 = EDGE_CURVE ( 'NONE', #64218, #1941, #16375, .T. ) ;
#43446 = EDGE_LOOP ( 'NONE', ( #60484, #24150, #65418, #59623 ) ) ;
#43447 = CARTESIAN_POINT ( 'NONE',  ( -11.77351654964669514, -4.406483450353273490, 195.0000000000000284 ) ) ;
#43448 = ORIENTED_EDGE ( 'NONE', *, *, #15531, .T. ) ;
#43449 = CARTESIAN_POINT ( 'NONE',  ( 7.357023737882802727, 5.538810540049955655, 54.00000000000000711 ) ) ;
#43450 = EDGE_CURVE ( 'NONE', #64422, #63119, #2831, .T. ) ;
#43451 = EDGE_LOOP ( 'NONE', ( #53807, #19473, #53503, #62696 ) ) ;
#43452 = LINE ( 'NONE', #37471, #46065 ) ;
#43453 = CIRCLE ( 'NONE', #2814, 0.2000000000000000944 ) ;
#43454 = EDGE_CURVE ( 'NONE', #20164, #32475, #23065, .T. ) ;
#43455 = DIRECTION ( 'NONE',  ( -1.000000000000000000, 0.000000000000000000, 0.000000000000000000 ) ) ;
#43456 = VECTOR ( 'NONE', #62686, 1000.000000000000000 ) ;
#43457 = DIRECTION ( 'NONE',  ( 0.000000000000000000, 0.000000000000000000, -1.000000000000000000 ) ) ;
#43458 = ORIENTED_EDGE ( 'NONE', *, *, #53543, .F. ) ;
#43459 = ADVANCED_FACE ( 'NONE', ( #39666 ), #12787, .F. ) ;
#43460 = VERTEX_POINT ( 'NONE', #12440 ) ;
#43461 = CARTESIAN_POINT ( 'NONE',  ( -8.393516549646733438, -6.344579767990798480, 195.0000000000000284 ) ) ;
#43463 = EDGE_LOOP ( 'NONE', ( #16518, #47699, #26642, #5883 ) ) ;
#43462 = EDGE_CURVE ( 'NONE', #41832, #13102, #44620, .T. ) ;
#43464 = ORIENTED_EDGE ( 'NONE', *, *, #14685, .F. ) ;
#43465 = LINE ( 'NONE', #342, #37203 ) ;
#43466 = CARTESIAN_POINT ( 'NONE',  ( 14.75000000000000178, -0.2500000000000000000, -26.75000000000000000 ) ) ;
#43467 = LINE ( 'NONE', #10954, #3902 ) ;
#43468 = ORIENTED_EDGE ( 'NONE', *, *, #45787, .F. ) ;
#43469 = AXIS2_PLACEMENT_3D ( 'NONE', #7138, #44979, #28717 ) ;
#43470 = LINE ( 'NONE', #49131, #13106 ) ;
#43472 = LINE ( 'NONE', #49485, #45656 ) ;
#43471 = DIRECTION ( 'NONE',  ( 0.000000000000000000, 0.000000000000000000, 1.000000000000000000 ) ) ;
#43473 = ORIENTED_EDGE ( 'NONE', *, *, #22390, .T. ) ;
#43474 = ORIENTED_EDGE ( 'NONE', *, *, #41922, .F. ) ;
#43476 = ORIENTED_EDGE ( 'NONE', *, *, #60399, .T. ) ;
#43475 = CARTESIAN_POINT ( 'NONE',  ( 25.57999999999999829, 3.010794155703768650E-16, -2.458500000000000796 ) ) ;
#43477 = VERTEX_POINT ( 'NONE', #39332 ) ;
#43478 = DIRECTION ( 'NONE',  ( 0.000000000000000000, -1.000000000000000000, 0.000000000000000000 ) ) ;
#43479 = VERTEX_POINT ( 'NONE', #34014 ) ;
#43480 = EDGE_LOOP ( 'NONE', ( #893, #4638, #42088, #55403 ) ) ;
#43481 = DIRECTION ( 'NONE',  ( -0.000000000000000000, -0.000000000000000000, 1.000000000000000000 ) ) ;
#43482 = CARTESIAN_POINT ( 'NONE',  ( -11.11351654964668612, 8.693516549646636449, 195.0000000000000284 ) ) ;
#43483 = CIRCLE ( 'NONE', #9634, 24.99999999998794920 ) ;
#43484 = ORIENTED_EDGE ( 'NONE', *, *, #11857, .F. ) ;
#43485 = ADVANCED_FACE ( 'NONE', ( #2891 ), #35059, .F. ) ;
#43486 = DIRECTION ( 'NONE',  ( 0.000000000000000000, 0.000000000000000000, 1.000000000000000000 ) ) ;
#43487 = DIRECTION ( 'NONE',  ( -0.000000000000000000, -1.000000000000000000, -0.000000000000000000 ) ) ;
#43488 = AXIS2_PLACEMENT_3D ( 'NONE', #5630, #26854, #64666 ) ;
#43489 = CARTESIAN_POINT ( 'NONE',  ( 5.257023737882795977, 5.242976262117205799, 26.00000000000000711 ) ) ;
#43490 = ORIENTED_EDGE ( 'NONE', *, *, #60447, .F. ) ;
#43491 = AXIS2_PLACEMENT_3D ( 'NONE', #50437, #1998, #24259 ) ;
#43492 = VECTOR ( 'NONE', #26841, 1000.000000000000000 ) ;
#43493 = VECTOR ( 'NONE', #21148, 1000.000000000000000 ) ;
#43494 = CARTESIAN_POINT ( 'NONE',  ( 69.47321854994619628, 47.95351654967443977, 43.00000000000000000 ) ) ;
#43495 = DIRECTION ( 'NONE',  ( 0.000000000000000000, -1.000000000000000000, 0.000000000000000000 ) ) ;
#43497 = ORIENTED_EDGE ( 'NONE', *, *, #30936, .T. ) ;
#43496 = CARTESIAN_POINT ( 'NONE',  ( 32.89999999999999858, 0.000000000000000000, 0.000000000000000000 ) ) ;
#43499 = VERTEX_POINT ( 'NONE', #34715 ) ;
#43498 = LINE ( 'NONE', #65087, #43653 ) ;
#43500 = CARTESIAN_POINT ( 'NONE',  ( 30.00000000000000000, -15.97213595500069871, 14.50000000000000000 ) ) ;
#43501 = VECTOR ( 'NONE', #52624, 1000.000000000000000 ) ;
#43502 = CIRCLE ( 'NONE', #2863, 4.000000000000000000 ) ;
#43503 = EDGE_CURVE ( 'NONE', #66440, #68576, #23766, .T. ) ;
#43504 = CARTESIAN_POINT ( 'NONE',  ( 7.250000000000005329, 7.250000000000000888, -21.50000000000000000 ) ) ;
#43505 = CARTESIAN_POINT ( 'NONE',  ( 5.552858015815571591, 7.342976262117199227, 54.00000000000000711 ) ) ;
#43506 = CARTESIAN_POINT ( 'NONE',  ( 7.806483450353379538, -11.32648345035339155, 195.0000000000000284 ) ) ;
#43507 = DIRECTION ( 'NONE',  ( 1.000000000000000000, 0.000000000000000000, 0.000000000000000000 ) ) ;
#43508 = VECTOR ( 'NONE', #59833, 1000.000000000000000 ) ;
#43509 = ADVANCED_FACE ( 'NONE', ( #60887 ), #55600, .F. ) ;
#43510 = CARTESIAN_POINT ( 'NONE',  ( 7.250000000000005329, 7.250000000000000888, -19.50000000000000000 ) ) ;
#43511 = ORIENTED_EDGE ( 'NONE', *, *, #156, .T. ) ;
#43512 = CARTESIAN_POINT ( 'NONE',  ( -11.11351654964669322, -4.206483450353289300, 195.0000000000000284 ) ) ;
#43514 = ORIENTED_EDGE ( 'NONE', *, *, #16406, .F. ) ;
#43513 = DIRECTION ( 'NONE',  ( -0.000000000000000000, -0.000000000000000000, -1.000000000000000000 ) ) ;
#43516 = VERTEX_POINT ( 'NONE', #50285 ) ;
#43515 = DIRECTION ( 'NONE',  ( -1.000000000000000000, 0.000000000000000000, 0.000000000000000000 ) ) ;
#43517 = AXIS2_PLACEMENT_3D ( 'NONE', #44369, #39760, #50381 ) ;
#43518 = LINE ( 'NONE', #11677, #5298 ) ;
#43519 = LINE ( 'NONE', #11007, #69106 ) ;
#43520 = ORIENTED_EDGE ( 'NONE', *, *, #68122, .T. ) ;
#43521 = DIRECTION ( 'NONE',  ( -1.261617073437657735E-14, -1.000000000000000000, 0.000000000000000000 ) ) ;
#43522 = CARTESIAN_POINT ( 'NONE',  ( 0.000000000000000000, -42.00000000000000000, 30.00000000000000000 ) ) ;
#43523 = ADVANCED_FACE ( 'NONE', ( #45317 ), #23425, .F. ) ;
#43524 = ORIENTED_EDGE ( 'NONE', *, *, #42956, .F. ) ;
#43525 = DIRECTION ( 'NONE',  ( -1.000000000000000000, 0.000000000000000000, 0.000000000000000000 ) ) ;
#43526 = CARTESIAN_POINT ( 'NONE',  ( -10.73351654964671020, 1.677516549646604016, 455.0000000000000568 ) ) ;
#43527 = CARTESIAN_POINT ( 'NONE',  ( 49.00000000000000000, 20.60000000000000142, -13.86939075806900057 ) ) ;
#43528 = FACE_OUTER_BOUND ( 'NONE', #53178, .T. ) ;
#43529 = ORIENTED_EDGE ( 'NONE', *, *, #33550, .F. ) ;
#43530 = ADVANCED_FACE ( 'NONE', ( #67606 ), #19157, .T. ) ;
#43531 = CARTESIAN_POINT ( 'NONE',  ( 6.750000000000000000, 7.750000000000000000, -5.000000000000000000 ) ) ;
#43532 = ORIENTED_EDGE ( 'NONE', *, *, #55410, .F. ) ;
#43533 = TOROIDAL_SURFACE ( 'NONE', #4188, 3.299999999999474909, 0.2000000000005234813 ) ;
#43534 = ORIENTED_EDGE ( 'NONE', *, *, #45316, .T. ) ;
#43535 = DIRECTION ( 'NONE',  ( 0.000000000000000000, 1.000000000000000000, 0.000000000000000000 ) ) ;
#43536 = CARTESIAN_POINT ( 'NONE',  ( -5.242976262117275077, -5.257023737882800418, 26.00000000000000711 ) ) ;
#43537 = EDGE_CURVE ( 'NONE', #51205, #35164, #48022, .T. ) ;
#43538 = VECTOR ( 'NONE', #8387, 1000.000000000000000 ) ;
#43539 = DIRECTION ( 'NONE',  ( -1.356437060717832013E-15, -1.000000000000000000, -1.836970198721033878E-16 ) ) ;
#43540 = VECTOR ( 'NONE', #6229, 1000.000000000000000 ) ;
#43541 = DIRECTION ( 'NONE',  ( -1.000000000000000000, 0.000000000000000000, 0.000000000000000000 ) ) ;
#43542 = EDGE_LOOP ( 'NONE', ( #14611, #4205, #4254, #31649 ) ) ;
#43543 = EDGE_CURVE ( 'NONE', #35617, #7006, #56292, .T. ) ;
#43544 = ORIENTED_EDGE ( 'NONE', *, *, #44237, .T. ) ;
#43546 = VERTEX_POINT ( 'NONE', #61937 ) ;
#43545 = CARTESIAN_POINT ( 'NONE',  ( 152.0064834503532722, 2.160375375128253950, 5.000000000000000000 ) ) ;
#43548 = ORIENTED_EDGE ( 'NONE', *, *, #16730, .T. ) ;
#43547 = EDGE_CURVE ( 'NONE', #45109, #27729, #62285, .T. ) ;
#43549 = CIRCLE ( 'NONE', #8554, 1.000000000000003553 ) ;
#43550 = VECTOR ( 'NONE', #9082, 1000.000000000000000 ) ;
#43551 = VECTOR ( 'NONE', #35034, 1000.000000000000000 ) ;
#43552 = LINE ( 'NONE', #1799, #28101 ) ;
#43553 = DIRECTION ( 'NONE',  ( 0.000000000000000000, 0.000000000000000000, -1.000000000000000000 ) ) ;
#43554 = FACE_OUTER_BOUND ( 'NONE', #38377, .T. ) ;
#43555 = DIRECTION ( 'NONE',  ( 0.000000000000000000, 0.000000000000000000, 1.000000000000000000 ) ) ;
#43556 = VECTOR ( 'NONE', #7217, 1000.000000000000000 ) ;
#43557 = AXIS2_PLACEMENT_3D ( 'NONE', #67566, #19115, #56936 ) ;
#43559 = CARTESIAN_POINT ( 'NONE',  ( 11.32648345035337734, -7.806483450353490561, 455.0000000000000568 ) ) ;
#43558 = CARTESIAN_POINT ( 'NONE',  ( 6.006483450353401921, 5.993516549646582092, 455.0000000000000568 ) ) ;
#43560 = EDGE_LOOP ( 'NONE', ( #33475, #57315, #34305, #67388 ) ) ;
#43562 = VERTEX_POINT ( 'NONE', #35405 ) ;
#43561 = LINE ( 'NONE', #17375, #19459 ) ;
#43563 = ADVANCED_FACE ( 'NONE', ( #56978 ), #25172, .F. ) ;
#43564 = VERTEX_POINT ( 'NONE', #14552 ) ;
#43565 = VERTEX_POINT ( 'NONE', #46723 ) ;
#43566 = VECTOR ( 'NONE', #69927, 1000.000000000000000 ) ;
#43567 = CARTESIAN_POINT ( 'NONE',  ( 3.664523737882778853, -10.50702373788281285, 54.00000000000000711 ) ) ;
#43568 = LINE ( 'NONE', #65153, #16304 ) ;
#43569 = PRESENTATION_LAYER_ASSIGNMENT (  '', '', ( #10809 ) ) ;
#43570 = CARTESIAN_POINT ( 'NONE',  ( -29.50000000000000355, -11.70000000000000284, -11.00000000000000000 ) ) ;
#43571 = VERTEX_POINT ( 'NONE', #41425 ) ;
#43572 = ADVANCED_FACE ( 'NONE', ( #58750 ), #36119, .F. ) ;
#43573 = ORIENTED_EDGE ( 'NONE', *, *, #69644, .F. ) ;
#43574 = VERTEX_POINT ( 'NONE', #62635 ) ;
#43575 = VECTOR ( 'NONE', #10562, 1000.000000000000114 ) ;
#43576 = CARTESIAN_POINT ( 'NONE',  ( -7.250000000000000888, 7.250000000000001776, -10.00000000000000000 ) ) ;
#43577 = CARTESIAN_POINT ( 'NONE',  ( 9.929523737882751888, 0.9414762621171479662, 54.00000000000000711 ) ) ;
#43578 = DIRECTION ( 'NONE',  ( 1.836970198721029934E-16, -1.836970198721036344E-16, 1.000000000000000000 ) ) ;
#43579 = ORIENTED_EDGE ( 'NONE', *, *, #61991, .T. ) ;
#43580 = ADVANCED_FACE ( 'NONE', ( #35767, #63355 ), #30819, .T. ) ;
#43581 = ORIENTED_EDGE ( 'NONE', *, *, #23703, .F. ) ;
#43582 = DIRECTION ( 'NONE',  ( 0.000000000000000000, 0.000000000000000000, -1.000000000000000000 ) ) ;
#43583 = CARTESIAN_POINT ( 'NONE',  ( -11.50000000000000000, -12.00000000000000000, 11.00000000000000000 ) ) ;
#43584 = ORIENTED_EDGE ( 'NONE', *, *, #50264, .F. ) ;
#43585 = EDGE_CURVE ( 'NONE', #2849, #19378, #52393, .T. ) ;
#43586 = ADVANCED_BREP_SHAPE_REPRESENTATION ( '', ( #67347, #45918 ), #65174 ) ;
#43587 = CARTESIAN_POINT ( 'NONE',  ( 8.900000000000005684, 20.60000000000000142, -13.86939075806900057 ) ) ;
#43588 = EDGE_CURVE ( 'NONE', #33622, #16636, #52045, .T. ) ;
#43590 = VERTEX_POINT ( 'NONE', #58037 ) ;
#43589 = LINE ( 'NONE', #21333, #65650 ) ;
#43591 = ORIENTED_EDGE ( 'NONE', *, *, #5561, .T. ) ;
#43592 = DIRECTION ( 'NONE',  ( 0.000000000000000000, 0.000000000000000000, 1.000000000000000000 ) ) ;
#43593 = DIRECTION ( 'NONE',  ( -0.7071067811865514585, -0.7071067811865435759, -2.597868168706465806E-16 ) ) ;
#43594 = EDGE_CURVE ( 'NONE', #16332, #45036, #630, .T. ) ;
#43595 = CIRCLE ( 'NONE', #52642, 0.5000000000009284795 ) ;
#43596 = DIRECTION ( 'NONE',  ( 0.000000000000000000, 0.000000000000000000, -1.000000000000000000 ) ) ;
#43597 = DIRECTION ( 'NONE',  ( -8.612436249475772606E-15, -1.000000000000000000, -1.836970198721020566E-16 ) ) ;
#43598 = DIRECTION ( 'NONE',  ( 1.000000000000000000, -0.000000000000000000, -0.000000000000000000 ) ) ;
#43599 = CIRCLE ( 'NONE', #40189, 0.3999999999999993006 ) ;
#43600 = EDGE_CURVE ( 'NONE', #56111, #4682, #3248, .T. ) ;
#43601 = ORIENTED_EDGE ( 'NONE', *, *, #34592, .F. ) ;
#43602 = PLANE ( 'NONE',  #6644 ) ;
#43603 = VERTEX_POINT ( 'NONE', #52763 ) ;
#43604 = AXIS2_PLACEMENT_3D ( 'NONE', #45595, #34283, #39932 ) ;
#43605 = LINE ( 'NONE', #16747, #15209 ) ;
#43606 = DIRECTION ( 'NONE',  ( 3.491481338843133355E-15, 1.000000000000000000, 1.836970198721029934E-16 ) ) ;
#43607 = EDGE_CURVE ( 'NONE', #54089, #60836, #66124, .T. ) ;
#43608 = DIRECTION ( 'NONE',  ( 1.000000000000000000, -0.000000000000000000, -0.000000000000000000 ) ) ;
#43609 = EDGE_CURVE ( 'NONE', #61431, #4997, #17565, .T. ) ;
#43610 = CARTESIAN_POINT ( 'NONE',  ( -9.781776262117324094, -10.50702373788275779, 54.00000000000000711 ) ) ;
#43611 = AXIS2_PLACEMENT_3D ( 'NONE', #3065, #24632, #67752 ) ;
#43612 = CIRCLE ( 'NONE', #67334, 2.204799999999996540 ) ;
#43613 = CIRCLE ( 'NONE', #40203, 1.000000000000000000 ) ;
#43614 = DIRECTION ( 'NONE',  ( 1.000000000000000000, -0.000000000000000000, 0.000000000000000000 ) ) ;
#43615 = ADVANCED_FACE ( 'NONE', ( #68662 ), #20207, .T. ) ;
#43616 = EDGE_CURVE ( 'NONE', #38860, #10751, #60471, .T. ) ;
#43617 = EDGE_CURVE ( 'NONE', #14797, #37068, #9611, .T. ) ;
#43618 = ORIENTED_EDGE ( 'NONE', *, *, #17321, .F. ) ;
#43619 = AXIS2_PLACEMENT_3D ( 'NONE', #34077, #23832, #62005 ) ;
#43620 = LINE ( 'NONE', #27701, #14416 ) ;
#43621 = SURFACE_SIDE_STYLE ('',( #43956 ) ) ;
#43622 = EDGE_CURVE ( 'NONE', #38244, #68597, #41068, .T. ) ;
#43623 = CIRCLE ( 'NONE', #56030, 3.499999999999999556 ) ;
#43624 = VERTEX_POINT ( 'NONE', #8897 ) ;
#43625 = MANIFOLD_SOLID_BREP ( 'Scale1', #55513 ) ;
#43626 = EDGE_CURVE ( 'NONE', #52249, #55561, #37531, .T. ) ;
#43627 = DIRECTION ( 'NONE',  ( -1.000000000000000000, 0.000000000000000000, 0.000000000000000000 ) ) ;
#43628 = CARTESIAN_POINT ( 'NONE',  ( 4.456444791733522252E-16, 7.450000000000002842, -8.000000000000000000 ) ) ;
#43629 = ORIENTED_EDGE ( 'NONE', *, *, #68534, .F. ) ;
#43630 = EDGE_CURVE ( 'NONE', #65210, #33597, #28862, .T. ) ;
#43631 = PLANE ( 'NONE',  #49369 ) ;
#43632 = DIRECTION ( 'NONE',  ( 1.836970198721029934E-16, 1.836970198721010706E-16, -1.000000000000000000 ) ) ;
#43633 = ORIENTED_EDGE ( 'NONE', *, *, #1700, .F. ) ;
#43634 = LINE ( 'NONE', #38334, #20928 ) ;
#43635 = CARTESIAN_POINT ( 'NONE',  ( -10.91351654964670637, 2.693516549646604030, 195.0000000000000284 ) ) ;
#43636 = CARTESIAN_POINT ( 'NONE',  ( 8.250000000000005329, -7.249999999999998224, -12.50000000000000000 ) ) ;
#43637 = CARTESIAN_POINT ( 'NONE',  ( -11.99351654964671354, 4.173516549646604901, 455.0000000000000568 ) ) ;
#43638 = ADVANCED_FACE ( 'NONE', ( #59089 ), #5367, .F. ) ;
#43639 = EDGE_LOOP ( 'NONE', ( #16104, #41986, #34353, #51955 ) ) ;
#43641 = ORIENTED_EDGE ( 'NONE', *, *, #65245, .F. ) ;
#43640 = DIRECTION ( 'NONE',  ( 1.000000000000000000, -5.981805089575196197E-17, 0.000000000000000000 ) ) ;
#43642 = EDGE_CURVE ( 'NONE', #21330, #25093, #64743, .T. ) ;
#43643 = CARTESIAN_POINT ( 'NONE',  ( 275.0000000000000000, -32.95000000000000284, 7.700000000000000178 ) ) ;
#43644 = LINE ( 'NONE', #10424, #9786 ) ;
#43645 = DIRECTION ( 'NONE',  ( -1.000000000000000000, 0.000000000000000000, 0.000000000000000000 ) ) ;
#43646 = ORIENTED_EDGE ( 'NONE', *, *, #50732, .F. ) ;
#43647 = AXIS2_PLACEMENT_3D ( 'NONE', #54232, #43606, #44284 ) ;
#43648 = CARTESIAN_POINT ( 'NONE',  ( 8.465062094116053260, 7.744988412222763685, 195.0000000000000284 ) ) ;
#43649 = CARTESIAN_POINT ( 'NONE',  ( 50.83090410532631864, 3.657408540445001854, 0.8284271247461899579 ) ) ;
#43650 = CIRCLE ( 'NONE', #8660, 4.000000000000000000 ) ;
#43651 = EDGE_LOOP ( 'NONE', ( #65771, #8209, #44187, #38448 ) ) ;
#43652 = EDGE_LOOP ( 'NONE', ( #2423, #53785, #37072, #14957 ) ) ;
#43653 = VECTOR ( 'NONE', #60106, 1000.000000000000000 ) ;
#43654 = CIRCLE ( 'NONE', #764, 1.000000000000000000 ) ;
#43655 = ORIENTED_EDGE ( 'NONE', *, *, #42056, .T. ) ;
#43656 = CARTESIAN_POINT ( 'NONE',  ( 8.250000000000005329, 7.250000000000000888, -17.00000000000000000 ) ) ;
#43657 = DIRECTION ( 'NONE',  ( 1.000000000000000000, -1.952517519553884087E-14, 1.836970198720994435E-16 ) ) ;
#43658 = CARTESIAN_POINT ( 'NONE',  ( 5.257023737882819070, -5.257023737882815517, 26.00000000000000711 ) ) ;
#43659 =( LENGTH_UNIT ( ) NAMED_UNIT ( * ) SI_UNIT ( .MILLI., .METRE. ) );
#43660 = CIRCLE ( 'NONE', #21092, 0.4999999999945519691 ) ;
#43661 = AXIS2_PLACEMENT_3D ( 'NONE', #58762, #69727, #22330 ) ;
#43662 = AXIS2_PLACEMENT_3D ( 'NONE', #15844, #4550, #32189 ) ;
#43663 = ORIENTED_EDGE ( 'NONE', *, *, #65264, .T. ) ;
#43664 = ORIENTED_EDGE ( 'NONE', *, *, #61279, .F. ) ;
#43665 = VERTEX_POINT ( 'NONE', #53448 ) ;
#43666 = CARTESIAN_POINT ( 'NONE',  ( 4.186483450353422953, 11.77351654964658501, 455.0000000000000568 ) ) ;
#43667 = VECTOR ( 'NONE', #16527, 1000.000000000000000 ) ;
#43668 = ORIENTED_EDGE ( 'NONE', *, *, #8953, .F. ) ;
#43669 = VERTEX_POINT ( 'NONE', #16299 ) ;
#43670 = ORIENTED_EDGE ( 'NONE', *, *, #45339, .F. ) ;
#43671 = ORIENTED_EDGE ( 'NONE', *, *, #41645, .T. ) ;
#43672 = AXIS2_PLACEMENT_3D ( 'NONE', #22291, #38877, #6369 ) ;
#43673 = CARTESIAN_POINT ( 'NONE',  ( 11.50000000000000000, -11.50000000000000000, 15.00000000000000000 ) ) ;
#43674 = UNCERTAINTY_MEASURE_WITH_UNIT (LENGTH_MEASURE( 1.000000000000000082E-05 ), #6175, 'distance_accuracy_value', 'NONE');
#43676 = ORIENTED_EDGE ( 'NONE', *, *, #7110, .F. ) ;
#43675 = CARTESIAN_POINT ( 'NONE',  ( -7.250000000000000888, 7.250000000000001776, -12.50000000000000000 ) ) ;
#43677 = EDGE_CURVE ( 'NONE', #52255, #59339, #35628, .T. ) ;
#43678 = FACE_OUTER_BOUND ( 'NONE', #56243, .T. ) ;
#43679 = CIRCLE ( 'NONE', #13166, 24.99999999998784972 ) ;
#43680 = DIRECTION ( 'NONE',  ( -0.000000000000000000, -0.000000000000000000, -1.000000000000000000 ) ) ;
#43681 = CARTESIAN_POINT ( 'NONE',  ( 0.000000000000000000, 0.000000000000000000, -24.50000000000000000 ) ) ;
#43682 = ADVANCED_FACE ( 'NONE', ( #5707 ), #21617, .F. ) ;
#43683 = ORIENTED_EDGE ( 'NONE', *, *, #46389, .F. ) ;
#43684 = EDGE_CURVE ( 'NONE', #22317, #21676, #33258, .T. ) ;
#43685 = CARTESIAN_POINT ( 'NONE',  ( 25.50000000000000355, 0.000000000000000000, -22.50000000000000000 ) ) ;
#43686 = ADVANCED_FACE ( 'NONE', ( #37876 ), #6388, .F. ) ;
#43687 = ORIENTED_EDGE ( 'NONE', *, *, #23329, .T. ) ;
#43688 = LINE ( 'NONE', #3850, #47291 ) ;
#43689 = CARTESIAN_POINT ( 'NONE',  ( 30.00000000000000000, -12.00000000000000000, -11.03137303340310282 ) ) ;
#43690 = CARTESIAN_POINT ( 'NONE',  ( 7.826483450353421745, 11.77351654964657257, 455.0000000000000568 ) ) ;
#43691 = DIRECTION ( 'NONE',  ( -1.000000000000000000, 0.000000000000000000, 0.000000000000000000 ) ) ;
#43692 = ORIENTED_EDGE ( 'NONE', *, *, #48066, .T. ) ;
#43693 = LINE ( 'NONE', #54654, #60659 ) ;
#43694 = FACE_BOUND ( 'NONE', #26677, .T. ) ;
#43695 = PRESENTATION_LAYER_ASSIGNMENT (  '', '', ( #50445 ) ) ;
#43696 = CARTESIAN_POINT ( 'NONE',  ( 8.406483450353398723, 5.655420232009111814, 455.0000000000000568 ) ) ;
#43697 = EDGE_CURVE ( 'NONE', #35777, #22939, #11001, .T. ) ;
#43698 = AXIS2_PLACEMENT_3D ( 'NONE', #20039, #9794, #15086 ) ;
#43699 = AXIS2_PLACEMENT_3D ( 'NONE', #33145, #53351, #54045 ) ;
#43700 = CARTESIAN_POINT ( 'NONE',  ( 41.09999999999999432, 13.66939075806899950, -20.80000000000000426 ) ) ;
#43701 = DIRECTION ( 'NONE',  ( -1.000000000000000000, 0.000000000000000000, 0.000000000000000000 ) ) ;
#43702 = CARTESIAN_POINT ( 'NONE',  ( 8.250000000000005329, -7.249999999999998224, -15.00000000000000000 ) ) ;
#43703 = CARTESIAN_POINT ( 'NONE',  ( -11.00000000000000000, -17.35230188589299871, -15.35019951917099945 ) ) ;
#43704 = DIRECTION ( 'NONE',  ( 0.000000000000000000, -0.000000000000000000, 1.000000000000000000 ) ) ;
#43705 = VECTOR ( 'NONE', #24351, 1000.000000000000000 ) ;
#43706 = VERTEX_POINT ( 'NONE', #32914 ) ;
#43707 = DIRECTION ( 'NONE',  ( -1.000000000000000000, 0.000000000000000000, 0.000000000000000000 ) ) ;
#43708 = CARTESIAN_POINT ( 'NONE',  ( 7.357023737882817827, -3.848229544836335947, 26.00000000000000711 ) ) ;
#43709 = VECTOR ( 'NONE', #37184, 1000.000000000000000 ) ;
#43710 = CARTESIAN_POINT ( 'NONE',  ( 10.50702373788281996, -3.664523737882816157, 26.00000000000000711 ) ) ;
#43711 = AXIS2_PLACEMENT_3D ( 'NONE', #28241, #60074, #32866 ) ;
#43712 = CARTESIAN_POINT ( 'NONE',  ( -18.85410196625000268, -17.50000000000000000, 21.50000000000000000 ) ) ;
#43713 = ORIENTED_EDGE ( 'NONE', *, *, #44058, .T. ) ;
#43714 = DIRECTION ( 'NONE',  ( -0.000000000000000000, 1.000000000000000000, -0.000000000000000000 ) ) ;
#43715 = DIRECTION ( 'NONE',  ( 0.000000000000000000, -3.673940397442059868E-16, 1.000000000000000000 ) ) ;
#43716 = DIRECTION ( 'NONE',  ( 1.062171939662868407E-14, 1.000000000000000000, 0.000000000000000000 ) ) ;
#43717 = VECTOR ( 'NONE', #39818, 1000.000000000000000 ) ;
#43718 = DIRECTION ( 'NONE',  ( 0.000000000000000000, 1.000000000000000000, 0.000000000000000000 ) ) ;
#43719 = DIRECTION ( 'NONE',  ( 1.000000000000000000, -0.000000000000000000, -0.000000000000000000 ) ) ;
#43720 = CARTESIAN_POINT ( 'NONE',  ( 5.668387132715968058, 8.393516549646582448, 455.0000000000000568 ) ) ;
#43721 = EDGE_CURVE ( 'NONE', #34015, #47489, #54831, .T. ) ;
#43722 = VERTEX_POINT ( 'NONE', #48838 ) ;
#43723 = EDGE_CURVE ( 'NONE', #28927, #32858, #1088, .T. ) ;
#43724 = VECTOR ( 'NONE', #53012, 1000.000000000000114 ) ;
#43725 = ORIENTED_EDGE ( 'NONE', *, *, #51056, .T. ) ;
#43726 = LINE ( 'NONE', #38419, #33787 ) ;
#43727 = DIRECTION ( 'NONE',  ( -0.000000000000000000, 1.000000000000000000, -0.000000000000000000 ) ) ;
#43728 = ORIENTED_EDGE ( 'NONE', *, *, #67406, .F. ) ;
#43729 = EDGE_CURVE ( 'NONE', #56308, #24826, #393, .T. ) ;
#43730 = CARTESIAN_POINT ( 'NONE',  ( 283.0000000000000568, -20.85424868893542438, -17.35424868893542438 ) ) ;
#43731 = VERTEX_POINT ( 'NONE', #16663 ) ;
#43732 = LINE ( 'NONE', #37733, #63909 ) ;
#43733 = ORIENTED_EDGE ( 'NONE', *, *, #64533, .F. ) ;
#43734 = VERTEX_POINT ( 'NONE', #17330 ) ;
#43735 = DIRECTION ( 'NONE',  ( -3.614007241618349165E-15, -1.000000000000000000, 0.000000000000000000 ) ) ;
#43736 = VERTEX_POINT ( 'NONE', #59785 ) ;
#43737 = LINE ( 'NONE', #33117, #48969 ) ;
#43738 = CARTESIAN_POINT ( 'NONE',  ( 8.580623737882849156, 9.689726262117156708, 54.00000000000000711 ) ) ;
#43739 = CARTESIAN_POINT ( 'NONE',  ( 49.00000000000000000, 0.7500000000000000000, 4.943429983321300014 ) ) ;
#43740 = ORIENTED_EDGE ( 'NONE', *, *, #51847, .T. ) ;
#43741 = VERTEX_POINT ( 'NONE', #16999 ) ;
#43742 = CYLINDRICAL_SURFACE ( 'NONE', #780, 25.39999999999999858 ) ;
#43743 = DIRECTION ( 'NONE',  ( -0.000000000000000000, 0.000000000000000000, -1.000000000000000000 ) ) ;
#43744 = VERTEX_POINT ( 'NONE', #11333 ) ;
#43745 = ORIENTED_EDGE ( 'NONE', *, *, #43135, .T. ) ;
#43746 = VERTEX_POINT ( 'NONE', #38567 ) ;
#43747 = AXIS2_PLACEMENT_3D ( 'NONE', #67614, #11845, #33435 ) ;
#43748 = CIRCLE ( 'NONE', #22307, 24.99999999998784972 ) ;
#43749 = DIRECTION ( 'NONE',  ( 0.000000000000000000, 0.000000000000000000, -1.000000000000000000 ) ) ;
#43751 = ORIENTED_EDGE ( 'NONE', *, *, #30348, .T. ) ;
#43750 = PLANE ( 'NONE',  #19446 ) ;
#43752 = VECTOR ( 'NONE', #58518, 1000.000000000000000 ) ;
#43753 = EDGE_CURVE ( 'NONE', #45421, #33487, #54493, .T. ) ;
#43754 = AXIS2_PLACEMENT_3D ( 'NONE', #15688, #64141, #53519 ) ;
#43755 = CARTESIAN_POINT ( 'NONE',  ( 0.000000000000000000, 8.250000000000001776, -16.00000000000000000 ) ) ;
#43756 = LINE ( 'NONE', #55073, #2334 ) ;
#43757 = ORIENTED_EDGE ( 'NONE', *, *, #69227, .F. ) ;
#43758 = ORIENTED_EDGE ( 'NONE', *, *, #44132, .F. ) ;
#43759 = ADVANCED_FACE ( 'NONE', ( #60120 ), #12353, .F. ) ;
#43760 = CIRCLE ( 'NONE', #55027, 0.3999999999999993006 ) ;
#43761 = VECTOR ( 'NONE', #1294, 1000.000000000000000 ) ;
#43762 = EDGE_CURVE ( 'NONE', #49997, #37598, #61861, .T. ) ;
#43763 = EDGE_CURVE ( 'NONE', #9016, #65447, #24022, .T. ) ;
#43764 = VERTEX_POINT ( 'NONE', #40289 ) ;
#43765 = CARTESIAN_POINT ( 'NONE',  ( 39.00000000000000000, 0.000000000000000000, 0.000000000000000000 ) ) ;
#43766 = DIRECTION ( 'NONE',  ( 0.000000000000000000, 0.000000000000000000, 1.000000000000000000 ) ) ;
#43767 = EDGE_CURVE ( 'NONE', #62902, #18763, #32277, .T. ) ;
#43768 = ADVANCED_FACE ( 'NONE', ( #66119 ), #7059, .T. ) ;
#43769 = ORIENTED_EDGE ( 'NONE', *, *, #62045, .T. ) ;
#43770 = VECTOR ( 'NONE', #9787, 1000.000000000000000 ) ;
#43771 = ADVANCED_FACE ( 'NONE', ( #34270 ), #56552, .T. ) ;
#43772 = LINE ( 'NONE', #10545, #7543 ) ;
#43774 = ORIENTED_EDGE ( 'NONE', *, *, #50829, .T. ) ;
#43773 = DIRECTION ( 'NONE',  ( -1.000000000000000000, 0.000000000000000000, 0.000000000000000000 ) ) ;
#43775 = VERTEX_POINT ( 'NONE', #2804 ) ;
#43776 = CARTESIAN_POINT ( 'NONE',  ( 10.31452373788281562, -6.849523737882814878, 26.00000000000000000 ) ) ;
#43777 = CARTESIAN_POINT ( 'NONE',  ( -8.250000000000001776, 7.250000000000000888, -26.00000000000001066 ) ) ;
#43778 = LINE ( 'NONE', #65349, #41549 ) ;
#43779 = CARTESIAN_POINT ( 'NONE',  ( -30.00000000000000000, -11.50000000000000000, -15.00000000000000000 ) ) ;
#43780 = DIRECTION ( 'NONE',  ( -0.000000000000000000, -0.000000000000000000, 1.000000000000000000 ) ) ;
#43781 = ORIENTED_EDGE ( 'NONE', *, *, #11513, .T. ) ;
#43782 = FACE_OUTER_BOUND ( 'NONE', #27907, .T. ) ;
#43783 = CARTESIAN_POINT ( 'NONE',  ( 7.357023737882802727, 5.538810540049955655, 54.00000000000000711 ) ) ;
#43784 = CARTESIAN_POINT ( 'NONE',  ( -2.530476262117313357, -8.835729544836349092, 26.00000000000000711 ) ) ;
#43786 = VERTEX_POINT ( 'NONE', #7407 ) ;
#43785 = DIRECTION ( 'NONE',  ( -0.7071067811865451302, 0.7071067811865500152, 2.597868168706484541E-16 ) ) ;
#43787 = PLANE ( 'NONE',  #46002 ) ;
#43788 = AXIS2_PLACEMENT_3D ( 'NONE', #50994, #62297, #56993 ) ;
#43789 = CARTESIAN_POINT ( 'NONE',  ( -7.250000000000000888, 7.250000000000001776, -24.50000000000000000 ) ) ;
#43790 = DIRECTION ( 'NONE',  ( 0.000000000000000000, 0.000000000000000000, 1.000000000000000000 ) ) ;
#43791 = CARTESIAN_POINT ( 'NONE',  ( 4.186483450353375879, 11.77351654964663119, 195.0000000000000284 ) ) ;
#43792 = ORIENTED_EDGE ( 'NONE', *, *, #8159, .T. ) ;
#43793 = CARTESIAN_POINT ( 'NONE',  ( -15.08565937784311473, -0.3156604612129270127, 21.29584399676446083 ) ) ;
#43794 = LINE ( 'NONE', #22912, #30471 ) ;
#43795 = EDGE_LOOP ( 'NONE', ( #54608, #46372, #2521, #42497 ) ) ;
#43796 = CYLINDRICAL_SURFACE ( 'NONE', #46943, 0.1999999999999987899 ) ;
#43797 = CARTESIAN_POINT ( 'NONE',  ( -6.606374702650169795, 7.252248008019352099, 455.0000000000000568 ) ) ;
#43798 = LINE ( 'NONE', #65374, #39978 ) ;
#43799 = CARTESIAN_POINT ( 'NONE',  ( -7.250000000000001776, -7.249999999999998224, -14.50000000000000000 ) ) ;
#43800 = CARTESIAN_POINT ( 'NONE',  ( -7.394232575409600550, -3.724485858128637084, 26.00000000000000711 ) ) ;
#43801 = CYLINDRICAL_SURFACE ( 'NONE', #3779, 1.000000000000000000 ) ;
#43802 = EDGE_CURVE ( 'NONE', #10620, #40436, #45946, .T. ) ;
#43803 = ORIENTED_EDGE ( 'NONE', *, *, #48028, .F. ) ;
#43804 = CARTESIAN_POINT ( 'NONE',  ( 2.632023737882809744, -6.501044194225475081, 54.00000000000000711 ) ) ;
#43805 = DIRECTION ( 'NONE',  ( 0.5000000000000068834, 0.8660254037844345998, 6.723777587268309839E-17 ) ) ;
#43806 = ORIENTED_EDGE ( 'NONE', *, *, #40717, .F. ) ;
#43807 = EDGE_CURVE ( 'NONE', #16156, #33225, #24382, .T. ) ;
#43808 = DIRECTION ( 'NONE',  ( -1.000000000000000000, 1.254221251785257731E-14, 1.836970198721053107E-16 ) ) ;
#43809 = ADVANCED_FACE ( 'NONE', ( #34627 ), #39582, .F. ) ;
#43810 = VECTOR ( 'NONE', #1860, 1000.000000000000000 ) ;
#43811 = EDGE_CURVE ( 'NONE', #38349, #27791, #12014, .T. ) ;
#43812 = DIRECTION ( 'NONE',  ( 0.000000000000000000, 0.000000000000000000, -1.000000000000000000 ) ) ;
#43813 = CYLINDRICAL_SURFACE ( 'NONE', #44576, 0.5000000000009320322 ) ;
#43814 = ORIENTED_EDGE ( 'NONE', *, *, #38624, .T. ) ;
#43815 = VERTEX_POINT ( 'NONE', #18357 ) ;
#43816 = CARTESIAN_POINT ( 'NONE',  ( 8.250000000000005329, -8.249999999999998224, -26.00000000000001066 ) ) ;
#43817 = ORIENTED_EDGE ( 'NONE', *, *, #30269, .F. ) ;
#43818 = ORIENTED_EDGE ( 'NONE', *, *, #14178, .F. ) ;
#43819 = VECTOR ( 'NONE', #59874, 1000.000000000000000 ) ;
#43820 = LINE ( 'NONE', #54438, #53054 ) ;
#43821 = PLANE ( 'NONE',  #34659 ) ;
#43822 = PLANE ( 'NONE',  #6121 ) ;
#43823 = VERTEX_POINT ( 'NONE', #23337 ) ;
#43824 = CARTESIAN_POINT ( 'NONE',  ( 15.00000000000000000, -26.42999999999999972, 5.874955318979029784 ) ) ;
#43826 = CARTESIAN_POINT ( 'NONE',  ( 27.90000000000000213, 3.010794155703768650E-16, -2.458500000000000796 ) ) ;
#43825 = DIRECTION ( 'NONE',  ( 0.000000000000000000, 0.000000000000000000, 1.000000000000000000 ) ) ;
#43827 = ORIENTED_EDGE ( 'NONE', *, *, #40481, .F. ) ;
#43828 = ORIENTED_EDGE ( 'NONE', *, *, #48335, .T. ) ;
#43830 = ORIENTED_EDGE ( 'NONE', *, *, #59245, .F. ) ;
#43829 = CARTESIAN_POINT ( 'NONE',  ( 8.250000000000005329, -7.249999999999998224, -26.00000000000001066 ) ) ;
#43831 = VERTEX_POINT ( 'NONE', #2116 ) ;
#43832 = FACE_OUTER_BOUND ( 'NONE', #50295, .T. ) ;
#43833 = ADVANCED_FACE ( 'NONE', ( #45583 ), #44898, .F. ) ;
#43834 = DIRECTION ( 'NONE',  ( -0.000000000000000000, -0.000000000000000000, -1.000000000000000000 ) ) ;
#43835 = ORIENTED_EDGE ( 'NONE', *, *, #43993, .T. ) ;
#43836 = VERTEX_POINT ( 'NONE', #22983 ) ;
#43837 = DIRECTION ( 'NONE',  ( -0.3479852726768748461, 0.000000000000000000, -0.9375000000000006661 ) ) ;
#43838 = CARTESIAN_POINT ( 'NONE',  ( 275.0000000000000000, -0.5000000000000000000, 26.50000000000000000 ) ) ;
#43839 = ORIENTED_EDGE ( 'NONE', *, *, #63227, .T. ) ;
#43840 = DIRECTION ( 'NONE',  ( 0.000000000000000000, 0.000000000000000000, -1.000000000000000000 ) ) ;
#43841 = DIRECTION ( 'NONE',  ( -4.956352788505168198E-15, -1.000000000000000000, 0.000000000000000000 ) ) ;
#43842 = DIRECTION ( 'NONE',  ( 0.000000000000000000, -0.7071067811865454633, -0.7071067811865496822 ) ) ;
#43843 = EDGE_CURVE ( 'NONE', #67429, #26513, #66465, .T. ) ;
#43844 = ORIENTED_EDGE ( 'NONE', *, *, #4743, .F. ) ;
#43845 = VECTOR ( 'NONE', #26868, 1000.000000000000000 ) ;
#43846 = EDGE_CURVE ( 'NONE', #35523, #1729, #19842, .T. ) ;
#43848 = MANIFOLD_SOLID_BREP ( 'LPattern1[16]', #53262 ) ;
#43847 = CARTESIAN_POINT ( 'NONE',  ( 11.50000000000000000, -11.50000000000000000, 11.00000000000000000 ) ) ;
#43849 = CARTESIAN_POINT ( 'NONE',  ( -6.350872789121319251, -3.677663764522589140, 54.00000000000000711 ) ) ;
#43851 = ORIENTED_EDGE ( 'NONE', *, *, #35566, .T. ) ;
#43850 = DIRECTION ( 'NONE',  ( -0.000000000000000000, -0.000000000000000000, -1.000000000000000000 ) ) ;
#43853 = ORIENTED_EDGE ( 'NONE', *, *, #12214, .T. ) ;
#43852 = CARTESIAN_POINT ( 'NONE',  ( 9.703773737882785966, -8.580623737882856261, 54.00000000000000711 ) ) ;
#43854 = DIRECTION ( 'NONE',  ( 1.067128122525083795E-14, 1.000000000000000000, 0.000000000000000000 ) ) ;
#43855 = CIRCLE ( 'NONE', #19015, 2.204799999999997429 ) ;
#43856 = CARTESIAN_POINT ( 'NONE',  ( -8.750000000000001776, 7.250000000000000000, -30.00000000000001066 ) ) ;
#43857 = DIRECTION ( 'NONE',  ( 0.000000000000000000, -1.000000000000000000, 0.000000000000000000 ) ) ;
#43858 = CARTESIAN_POINT ( 'NONE',  ( 283.0000000000000568, -25.93000000000544958, 9.412893218815410634 ) ) ;
#43859 = CARTESIAN_POINT ( 'NONE',  ( -11.00000000000000000, -11.50000000000100009, 10.50000000000065903 ) ) ;
#43860 = CARTESIAN_POINT ( 'NONE',  ( 8.250000000000005329, -8.249999999999998224, -26.00000000000001066 ) ) ;
#43861 = ORIENTED_EDGE ( 'NONE', *, *, #36665, .F. ) ;
#43862 = LINE ( 'NONE', #66464, #22554 ) ;
#43863 = EDGE_LOOP ( 'NONE', ( #38020, #44734, #2930, #12004 ) ) ;
#43864 = AXIS2_PLACEMENT_3D ( 'NONE', #2547, #40387, #12116 ) ;
#43867 = ADVANCED_FACE ( 'NONE', ( #13058 ), #19759, .F. ) ;
#43866 = ORIENTED_EDGE ( 'NONE', *, *, #51363, .F. ) ;
#43865 = CARTESIAN_POINT ( 'NONE',  ( 282.8893988437589542, -25.27116123426317884, 17.22883876573682826 ) ) ;
#43868 = PLANE ( 'NONE',  #4181 ) ;
#43869 = CARTESIAN_POINT ( 'NONE',  ( 5.257023737882801306, 5.242976262117200470, 54.00000000000000711 ) ) ;
#43870 = EDGE_LOOP ( 'NONE', ( #69640, #48192, #12207, #47213 ) ) ;
#43871 = CARTESIAN_POINT ( 'NONE',  ( -7.250000000000000888, 7.250000000000001776, -15.50000000000000000 ) ) ;
#43872 = CYLINDRICAL_SURFACE ( 'NONE', #31753, 0.5249999999999990230 ) ;
#43873 = VERTEX_POINT ( 'NONE', #24732 ) ;
#43874 = LINE ( 'NONE', #65452, #16557 ) ;
#43875 = FACE_BOUND ( 'NONE', #10688, .T. ) ;
#43876 = DIRECTION ( 'NONE',  ( 0.000000000000000000, -0.1111111111108840643, -0.9938079899999319178 ) ) ;
#43877 = CARTESIAN_POINT ( 'NONE',  ( 283.0000000000000568, -37.15000000000001279, 7.700000000000000178 ) ) ;
#43878 = DIRECTION ( 'NONE',  ( -1.000000000000000000, 0.000000000000000000, 0.000000000000000000 ) ) ;
#43879 = ORIENTED_EDGE ( 'NONE', *, *, #22222, .F. ) ;
#43880 = LINE ( 'NONE', #5019, #55221 ) ;
#43881 = ORIENTED_EDGE ( 'NONE', *, *, #57607, .F. ) ;
#43882 = VERTEX_POINT ( 'NONE', #46289 ) ;
#43883 = ADVANCED_FACE ( 'NONE', ( #31455 ), #68574, .F. ) ;
#43884 = DIRECTION ( 'NONE',  ( 0.000000000000000000, 0.000000000000000000, -1.000000000000000000 ) ) ;
#43885 = PLANE ( 'NONE',  #3752 ) ;
#43886 = EDGE_CURVE ( 'NONE', #60715, #20779, #62203, .T. ) ;
#43887 = VECTOR ( 'NONE', #17126, 1000.000000000000000 ) ;
#43888 = DIRECTION ( 'NONE',  ( 7.751221965937476285E-17, -1.000000000000000000, -0.000000000000000000 ) ) ;
#43889 = CARTESIAN_POINT ( 'NONE',  ( -11.00000000000000000, -17.50000000000000000, -26.64999999999999858 ) ) ;
#43890 = VERTEX_POINT ( 'NONE', #30386 ) ;
#43891 = EDGE_LOOP ( 'NONE', ( #48842, #67748, #24704, #65951 ) ) ;
#43893 = ORIENTED_EDGE ( 'NONE', *, *, #46386, .T. ) ;
#43892 = CARTESIAN_POINT ( 'NONE',  ( 30.00000000000000000, -14.04000000000000092, 14.80000000000000071 ) ) ;
#43894 = EDGE_LOOP ( 'NONE', ( #30676, #3256, #45977, #43781 ) ) ;
#43895 = AXIS2_PLACEMENT_3D ( 'NONE', #63035, #18479, #67291 ) ;
#43896 = LINE ( 'NONE', #27639, #50698 ) ;
#43897 = PLANE ( 'NONE',  #6073 ) ;
#43898 = FACE_BOUND ( 'NONE', #30347, .T. ) ;
#43899 = AXIS2_PLACEMENT_3D ( 'NONE', #41152, #58125, #2988 ) ;
#43900 = PLANE ( 'NONE',  #42451 ) ;
#43902 = LINE ( 'NONE', #38609, #14233 ) ;
#43901 = CARTESIAN_POINT ( 'NONE',  ( -6.651770455163739548, 7.342976262117183239, 54.00000000000000711 ) ) ;
#43903 = EDGE_LOOP ( 'NONE', ( #53481, #14560, #39110, #68610, #46463, #33552, #40873, #2083 ) ) ;
#43905 = ORIENTED_EDGE ( 'NONE', *, *, #1939, .T. ) ;
#43904 = DIRECTION ( 'NONE',  ( 0.000000000000000000, -1.000000000000000000, 0.000000000000000000 ) ) ;
#43906 = ORIENTED_EDGE ( 'NONE', *, *, #56272, .F. ) ;
#43907 = ORIENTED_EDGE ( 'NONE', *, *, #18513, .T. ) ;
#43908 = VECTOR ( 'NONE', #51265, 1000.000000000000000 ) ;
#43909 = ADVANCED_FACE ( 'NONE', ( #25795 ), #25087, .F. ) ;
#43910 = DIRECTION ( 'NONE',  ( 1.000000000000000000, 2.135044278125301343E-15, -0.000000000000000000 ) ) ;
#43911 = DIRECTION ( 'NONE',  ( 1.000000000000000000, 0.000000000000000000, -0.000000000000000000 ) ) ;
#43912 = VECTOR ( 'NONE', #25716, 1000.000000000000000 ) ;
#43913 = CARTESIAN_POINT ( 'NONE',  ( 0.000000000000000000, -7.449999999999998401, -24.00000000000000000 ) ) ;
#43914 = LINE ( 'NONE', #6446, #7121 ) ;
#43915 = ORIENTED_EDGE ( 'NONE', *, *, #29385, .F. ) ;
#43916 = ORIENTED_EDGE ( 'NONE', *, *, #62649, .F. ) ;
#43917 = VECTOR ( 'NONE', #4319, 1000.000000000000000 ) ;
#43918 = CARTESIAN_POINT ( 'NONE',  ( 11.00000000000000000, -14.04000000000000092, 17.04524521594300523 ) ) ;
#43919 = CARTESIAN_POINT ( 'NONE',  ( 0.000000000000000000, 0.000000000000000000, 0.000000000000000000 ) ) ;
#43920 = VERTEX_POINT ( 'NONE', #25432 ) ;
#43921 = ORIENTED_EDGE ( 'NONE', *, *, #26747, .F. ) ;
#43922 = CARTESIAN_POINT ( 'NONE',  ( 146.5599459900709860, 5.000000000000000000, 284.4801873289890182 ) ) ;
#43923 = CARTESIAN_POINT ( 'NONE',  ( -7.250000000000001776, -7.249999999999998224, -18.00000000000000000 ) ) ;
#43924 = ORIENTED_EDGE ( 'NONE', *, *, #55234, .T. ) ;
#43925 = EDGE_CURVE ( 'NONE', #48692, #41078, #51608, .T. ) ;
#43926 = EDGE_CURVE ( 'NONE', #32685, #57125, #32327, .T. ) ;
#43927 = CARTESIAN_POINT ( 'NONE',  ( 7.000000000000000000, -20.49999999999999645, -16.03137303340311348 ) ) ;
#43928 = EDGE_CURVE ( 'NONE', #33150, #42432, #62544, .T. ) ;
#43930 = ORIENTED_EDGE ( 'NONE', *, *, #38033, .T. ) ;
#43929 = CARTESIAN_POINT ( 'NONE',  ( 7.250000000000005329, -7.449999999999998401, -13.50000000000000178 ) ) ;
#43931 = ORIENTED_EDGE ( 'NONE', *, *, #2117, .F. ) ;
#43932 = CARTESIAN_POINT ( 'NONE',  ( -7.250000000000001776, -7.249999999999998224, -8.500000000000000000 ) ) ;
#43933 = DIRECTION ( 'NONE',  ( 0.000000000000000000, 1.000000000000000000, 0.000000000000000000 ) ) ;
#43934 = ADVANCED_FACE ( 'NONE', ( #35314 ), #68214, .F. ) ;
#43935 = DIRECTION ( 'NONE',  ( 0.000000000000000000, 0.000000000000000000, 1.000000000000000000 ) ) ;
#43936 = CARTESIAN_POINT ( 'NONE',  ( 7.357023737882817827, -4.961189459950053227, 26.00000000000000711 ) ) ;
#43937 = VECTOR ( 'NONE', #66691, 1000.000000000000000 ) ;
#43938 = LINE ( 'NONE', #54918, #48577 ) ;
#43939 = EDGE_CURVE ( 'NONE', #9110, #36010, #9171, .T. ) ;
#43940 = ORIENTED_EDGE ( 'NONE', *, *, #63563, .F. ) ;
#43941 = CARTESIAN_POINT ( 'NONE',  ( 277.0217896459287203, -20.81978353999699749, -17.31978353999699749 ) ) ;
#43942 = EDGE_CURVE ( 'NONE', #15565, #43142, #3170, .T. ) ;
#43943 = AXIS2_PLACEMENT_3D ( 'NONE', #30856, #21301, #48518 ) ;
#43945 = VERTEX_POINT ( 'NONE', #46997 ) ;
#43944 = DIRECTION ( 'NONE',  ( -1.836970198721029934E-16, 1.836970198721036344E-16, -1.000000000000000000 ) ) ;
#43946 = CARTESIAN_POINT ( 'NONE',  ( 8.250000000000005329, 0.000000000000000000, -9.500000000000001776 ) ) ;
#43947 = CARTESIAN_POINT ( 'NONE',  ( 9.306483450353379538, -10.92648345035348534, 455.0000000000000568 ) ) ;
#43948 = CARTESIAN_POINT ( 'NONE',  ( 7.000000000000000000, -20.50000000000000000, -17.00000000000000000 ) ) ;
#43949 = DIRECTION ( 'NONE',  ( -0.000000000000000000, 3.673940397442059868E-16, -1.000000000000000000 ) ) ;
#43950 = AXIS2_PLACEMENT_3D ( 'NONE', #14550, #3955, #25526 ) ;
#43951 = PLANE ( 'NONE',  #46127 ) ;
#43952 = EDGE_LOOP ( 'NONE', ( #7552, #6995, #18638, #6535 ) ) ;
#43953 = EDGE_LOOP ( 'NONE', ( #14735, #68799, #46223, #58181 ) ) ;
#43954 = VECTOR ( 'NONE', #52920, 1000.000000000000000 ) ;
#43955 = CARTESIAN_POINT ( 'NONE',  ( -11.75000000000000000, -5.000000000000000000, 60.00000000000000000 ) ) ;
#43956 = SURFACE_STYLE_FILL_AREA ( #18117 ) ;
#43957 = AXIS2_PLACEMENT_3D ( 'NONE', #55693, #17867, #34112 ) ;
#43958 = EDGE_LOOP ( 'NONE', ( #48010, #48421, #11230, #4774 ) ) ;
#43959 = MANIFOLD_SOLID_BREP ( 'LPattern1[9]', #3582 ) ;
#43960 = DIRECTION ( 'NONE',  ( -0.000000000000000000, -0.000000000000000000, -1.000000000000000000 ) ) ;
#43961 = EDGE_CURVE ( 'NONE', #49212, #4106, #64651, .T. ) ;
#43962 = LINE ( 'NONE', #64505, #6141 ) ;
#43963 = ORIENTED_EDGE ( 'NONE', *, *, #66614, .F. ) ;
#43964 = DIRECTION ( 'NONE',  ( 0.000000000000000000, -1.000000000000000000, 0.000000000000000000 ) ) ;
#43965 = CIRCLE ( 'NONE', #48474, 24.99999999998784972 ) ;
#43966 = LINE ( 'NONE', #38331, #21780 ) ;
#43967 = EDGE_LOOP ( 'NONE', ( #17553, #66552, #17066, #50314 ) ) ;
#43968 = CYLINDRICAL_SURFACE ( 'NONE', #40082, 1.399999999999998579 ) ;
#43969 = CARTESIAN_POINT ( 'NONE',  ( 11.08848345035334404, -9.804883450353528929, 455.0000000000000568 ) ) ;
#43970 = FILL_AREA_STYLE ('',( #16768 ) ) ;
#43971 = CARTESIAN_POINT ( 'NONE',  ( 4.155633711806655306, 4.706725378239160484, 54.00000000000000711 ) ) ;
#43972 = VERTEX_POINT ( 'NONE', #41688 ) ;
#43974 = ORIENTED_EDGE ( 'NONE', *, *, #65796, .T. ) ;
#43973 = LINE ( 'NONE', #65884, #10307 ) ;
#43975 = CARTESIAN_POINT ( 'NONE',  ( -1.677516549646778099, -10.74648345035342167, 195.0000000000000284 ) ) ;
#43976 = DIRECTION ( 'NONE',  ( 0.000000000000000000, 0.000000000000000000, -1.000000000000000000 ) ) ;
#43977 = VECTOR ( 'NONE', #48106, 1000.000000000000000 ) ;
#43978 = PLANE ( 'NONE',  #48870 ) ;
#43979 = ORIENTED_EDGE ( 'NONE', *, *, #52154, .T. ) ;
#43980 = CARTESIAN_POINT ( 'NONE',  ( -4.173516549646669738, 11.77351654964658678, 455.0000000000000568 ) ) ;
#43981 = DIRECTION ( 'NONE',  ( -1.000000000000000000, 0.000000000000000000, 0.000000000000000000 ) ) ;
#43982 = ORIENTED_EDGE ( 'NONE', *, *, #51300, .F. ) ;
#43983 = ORIENTED_EDGE ( 'NONE', *, *, #38372, .F. ) ;
#43984 = ORIENTED_EDGE ( 'NONE', *, *, #41331, .F. ) ;
#43985 = EDGE_CURVE ( 'NONE', #5159, #45736, #22224, .T. ) ;
#43986 = CARTESIAN_POINT ( 'NONE',  ( 5.668387132715918320, -8.406483450353487541, 455.0000000000000568 ) ) ;
#43987 = FACE_OUTER_BOUND ( 'NONE', #34403, .T. ) ;
#43988 = AXIS2_PLACEMENT_3D ( 'NONE', #953, #50051, #1609 ) ;
#43989 = VECTOR ( 'NONE', #19796, 1000.000000000000000 ) ;
#43990 = DIRECTION ( 'NONE',  ( -0.7071067811865398012, 0.7071067811865552333, 2.597868168706484541E-16 ) ) ;
#43991 = ORIENTED_EDGE ( 'NONE', *, *, #20304, .T. ) ;
#43993 = EDGE_CURVE ( 'NONE', #16593, #15802, #11244, .T. ) ;
#43992 = EDGE_LOOP ( 'NONE', ( #30016, #17256, #30725, #54047, #65579, #23479 ) ) ;
#43994 = VERTEX_POINT ( 'NONE', #38483 ) ;
#43995 = AXIS2_PLACEMENT_3D ( 'NONE', #50557, #2115, #3868 ) ;
#43996 = FACE_OUTER_BOUND ( 'NONE', #49872, .T. ) ;
#43997 = ORIENTED_EDGE ( 'NONE', *, *, #40807, .T. ) ;
#43998 = EDGE_CURVE ( 'NONE', #11705, #43019, #5275, .T. ) ;
#43999 = ORIENTED_EDGE ( 'NONE', *, *, #31945, .F. ) ;
#44000 = EDGE_CURVE ( 'NONE', #18538, #4880, #13064, .T. ) ;
#44001 = ORIENTED_EDGE ( 'NONE', *, *, #31127, .T. ) ;
#44002 = VECTOR ( 'NONE', #57270, 1000.000000000000000 ) ;
#44003 = EDGE_LOOP ( 'NONE', ( #50850, #65507, #47788, #39198 ) ) ;
#44004 = DIRECTION ( 'NONE',  ( 0.000000000000000000, 0.000000000000000000, 1.000000000000000000 ) ) ;
#44006 = ORIENTED_EDGE ( 'NONE', *, *, #7346, .F. ) ;
#44005 = DIRECTION ( 'NONE',  ( 0.000000000000000000, 0.000000000000000000, 1.000000000000000000 ) ) ;
#44007 = CARTESIAN_POINT ( 'NONE',  ( -11.77351654964674310, -7.606483450353318965, 195.0000000000000284 ) ) ;
#44008 = CARTESIAN_POINT ( 'NONE',  ( 5.793274621760843957, -4.155633711806661523, 26.00000000000000711 ) ) ;
#44009 = ADVANCED_FACE ( 'NONE', ( #15541 ), #49084, .F. ) ;
#44010 = CARTESIAN_POINT ( 'NONE',  ( 9.750000000000001776, 9.690000000000001279, -4.250000000000000000 ) ) ;
#44011 = ORIENTED_EDGE ( 'NONE', *, *, #38391, .F. ) ;
#44012 = EDGE_CURVE ( 'NONE', #15758, #52731, #60032, .T. ) ;
#44013 = CARTESIAN_POINT ( 'NONE',  ( 8.250000000000005329, -7.249999999999998224, -25.50000000000000355 ) ) ;
#44014 = DIRECTION ( 'NONE',  ( -0.000000000000000000, -0.000000000000000000, -1.000000000000000000 ) ) ;
#44015 = DIRECTION ( 'NONE',  ( 1.000000000000000000, 0.000000000000000000, -0.000000000000000000 ) ) ;
#44016 = EDGE_CURVE ( 'NONE', #28088, #1387, #37102, .T. ) ;
#44017 = ORIENTED_EDGE ( 'NONE', *, *, #10332, .F. ) ;
#44018 = DIRECTION ( 'NONE',  ( -0.000000000000000000, 0.000000000000000000, -1.000000000000000000 ) ) ;
#44019 = EDGE_CURVE ( 'NONE', #55229, #43831, #16912, .T. ) ;
#44020 = CARTESIAN_POINT ( 'NONE',  ( -22.14589803375000088, -17.50000000000000000, 21.50000000000000000 ) ) ;
#44021 = DIRECTION ( 'NONE',  ( -1.000000000000000000, 0.000000000000000000, 0.000000000000000000 ) ) ;
#44022 = ORIENTED_EDGE ( 'NONE', *, *, #61020, .T. ) ;
#44023 = CARTESIAN_POINT ( 'NONE',  ( 5.668387132715920096, 8.393516549646628633, 195.0000000000000284 ) ) ;
#44024 = DIRECTION ( 'NONE',  ( 3.491481338843133355E-15, 1.000000000000000000, 1.836970198721029934E-16 ) ) ;
#44025 = CARTESIAN_POINT ( 'NONE',  ( -3.834182069070765309, 7.342976262117171693, 54.00000000000000711 ) ) ;
#44026 = ADVANCED_FACE ( 'NONE', ( #32133 ), #53706, .F. ) ;
#44027 = APPLICATION_CONTEXT ( 'automotive_design' ) ;
#44028 = DIRECTION ( 'NONE',  ( -3.491481338843133355E-15, -1.000000000000000000, -1.836970198721029934E-16 ) ) ;
#44029 = LINE ( 'NONE', #65608, #69301 ) ;
#44030 = CYLINDRICAL_SURFACE ( 'NONE', #26045, 1.224999999999999423 ) ;
#44031 = VECTOR ( 'NONE', #5122, 1000.000000000000000 ) ;
#44032 = LINE ( 'NONE', #61326, #7357 ) ;
#44033 = VECTOR ( 'NONE', #60325, 1000.000000000000000 ) ;
#44034 = DIRECTION ( 'NONE',  ( -0.7671651518152962090, -0.6414496315691619044, 0.000000000000000000 ) ) ;
#44035 = CIRCLE ( 'NONE', #52079, 0.5000000000000000000 ) ;
#44036 = ORIENTED_EDGE ( 'NONE', *, *, #23559, .T. ) ;
#44037 = DIRECTION ( 'NONE',  ( 1.000000000000000000, -0.000000000000000000, 0.000000000000000000 ) ) ;
#44038 = DIRECTION ( 'NONE',  ( -0.000000000000000000, 0.000000000000000000, -1.000000000000000000 ) ) ;
#44039 = AXIS2_PLACEMENT_3D ( 'NONE', #31795, #63623, #21519 ) ;
#44040 = CARTESIAN_POINT ( 'NONE',  ( 39.00000000000000000, 21.00000000000000000, 16.96999999999999886 ) ) ;
#44041 = CARTESIAN_POINT ( 'NONE',  ( 11.32648345035335780, 7.793516549646610336, 195.0000000000000284 ) ) ;
#44042 = EDGE_LOOP ( 'NONE', ( #10669, #215, #52960, #24290 ) ) ;
#44043 = DIRECTION ( 'NONE',  ( 0.000000000000000000, 0.000000000000000000, 1.000000000000000000 ) ) ;
#44044 = DIRECTION ( 'NONE',  ( 0.000000000000000000, 1.000000000000000000, 0.000000000000000000 ) ) ;
#44045 = CARTESIAN_POINT ( 'NONE',  ( 13.00000000000000178, -15.50000000000000000, 2.000000000000000000 ) ) ;
#44046 = AXIS2_PLACEMENT_3D ( 'NONE', #62470, #29957, #40567 ) ;
#44047 = EDGE_CURVE ( 'NONE', #46469, #53664, #54056, .T. ) ;
#44048 = DIRECTION ( 'NONE',  ( 1.819560449471430698E-15, 1.000000000000000000, 1.836970198721032892E-16 ) ) ;
#44049 = CARTESIAN_POINT ( 'NONE',  ( -11.77351654964670935, 7.593516549646604830, 195.0000000000000284 ) ) ;
#44050 = VECTOR ( 'NONE', #60951, 1000.000000000000114 ) ;
#44051 = ORIENTED_EDGE ( 'NONE', *, *, #40047, .T. ) ;
#44052 = AXIS2_PLACEMENT_3D ( 'NONE', #28308, #50582, #33954 ) ;
#44053 = EDGE_CURVE ( 'NONE', #56837, #26653, #5613, .T. ) ;
#44054 = VERTEX_POINT ( 'NONE', #21866 ) ;
#44055 = LINE ( 'NONE', #16849, #45086 ) ;
#44056 = DIRECTION ( 'NONE',  ( 1.000000000000000000, 0.000000000000000000, 0.000000000000000000 ) ) ;
#44057 = ORIENTED_EDGE ( 'NONE', *, *, #54874, .T. ) ;
#44058 = EDGE_CURVE ( 'NONE', #16445, #26978, #44709, .T. ) ;
#44059 = AXIS2_PLACEMENT_3D ( 'NONE', #41418, #24813, #67602 ) ;
#44060 = CIRCLE ( 'NONE', #64375, 1.399999999999999245 ) ;
#44061 = LINE ( 'NONE', #22844, #51062 ) ;
#44062 = ADVANCED_FACE ( 'NONE', ( #5952 ), #27870, .F. ) ;
#44063 = ORIENTED_EDGE ( 'NONE', *, *, #10123, .T. ) ;
#44064 = CARTESIAN_POINT ( 'NONE',  ( 15.50000000000129852, -15.50000000000000000, -22.50000000000000000 ) ) ;
#44065 = VERTEX_POINT ( 'NONE', #42386 ) ;
#44066 = ADVANCED_FACE ( 'NONE', ( #21184 ), #31797, .F. ) ;
#44067 = ORIENTED_EDGE ( 'NONE', *, *, #40536, .T. ) ;
#44068 = DIRECTION ( 'NONE',  ( 1.836970198721029934E-16, -1.836970198721036344E-16, 1.000000000000000000 ) ) ;
#44069 = ORIENTED_EDGE ( 'NONE', *, *, #21117, .F. ) ;
#44070 = DIRECTION ( 'NONE',  ( 0.000000000000000000, 0.000000000000000000, -1.000000000000000000 ) ) ;
#44071 = CARTESIAN_POINT ( 'NONE',  ( 0.000000000000000000, 0.000000000000000000, -26.00000000000001066 ) ) ;
#44072 = FACE_OUTER_BOUND ( 'NONE', #47175, .T. ) ;
#44073 = MANIFOLD_SOLID_BREP ( 'Fillet1', #69094 ) ;
#44074 = CIRCLE ( 'NONE', #11317, 4.000000000000000888 ) ;
#44075 = VERTEX_POINT ( 'NONE', #23242 ) ;
#44076 = EDGE_CURVE ( 'NONE', #32954, #62786, #21010, .T. ) ;
#44077 = ORIENTED_EDGE ( 'NONE', *, *, #2548, .F. ) ;
#44078 = LINE ( 'NONE', #21137, #38024 ) ;
#44079 = EDGE_CURVE ( 'NONE', #34291, #46362, #44453, .T. ) ;
#44080 = CARTESIAN_POINT ( 'NONE',  ( 8.900000000000002132, 21.00000000000000000, -18.00000000000000355 ) ) ;
#44081 = VERTEX_POINT ( 'NONE', #39836 ) ;
#44082 = ORIENTED_EDGE ( 'NONE', *, *, #49365, .T. ) ;
#44083 = EDGE_CURVE ( 'NONE', #7898, #23630, #2376, .T. ) ;
#44084 = EDGE_CURVE ( 'NONE', #10363, #67274, #56125, .T. ) ;
#44085 = ORIENTED_EDGE ( 'NONE', *, *, #48658, .T. ) ;
#44086 = PLANE ( 'NONE',  #59302 ) ;
#44087 = CIRCLE ( 'NONE', #3466, 1.620999999999997332 ) ;
#44089 = ORIENTED_EDGE ( 'NONE', *, *, #37080, .F. ) ;
#44088 = CARTESIAN_POINT ( 'NONE',  ( 8.465062094116069247, -7.757955312929635028, 455.0000000000000568 ) ) ;
#44090 = EDGE_CURVE ( 'NONE', #30799, #6900, #58267, .T. ) ;
#44091 = CARTESIAN_POINT ( 'NONE',  ( -9.750000000000000000, -9.690000000000001279, -4.250000000000000000 ) ) ;
#44092 = AXIS2_PLACEMENT_3D ( 'NONE', #27793, #11512, #60305 ) ;
#44093 = DIRECTION ( 'NONE',  ( -1.000000000000000000, 0.000000000000000000, 0.000000000000000000 ) ) ;
#44094 = ORIENTED_EDGE ( 'NONE', *, *, #14484, .T. ) ;
#44095 = ORIENTED_EDGE ( 'NONE', *, *, #56486, .F. ) ;
#44096 = AXIS2_PLACEMENT_3D ( 'NONE', #36481, #58051, #9622 ) ;
#44097 = VECTOR ( 'NONE', #29878, 1000.000000000000000 ) ;
#44098 = CARTESIAN_POINT ( 'NONE',  ( 28.00000000000000000, -17.50000000000000000, -15.70500000000000007 ) ) ;
#44099 = CARTESIAN_POINT ( 'NONE',  ( 0.000000000000000000, 8.250000000000001776, -7.500000000000000000 ) ) ;
#44100 = EDGE_CURVE ( 'NONE', #23076, #67807, #33848, .T. ) ;
#44101 = EDGE_LOOP ( 'NONE', ( #352, #35193, #22552, #2113 ) ) ;
#44102 = EDGE_CURVE ( 'NONE', #9064, #34571, #11927, .T. ) ;
#44103 = DIRECTION ( 'NONE',  ( 0.000000000000000000, -0.000000000000000000, -1.000000000000000000 ) ) ;
#44104 = DIRECTION ( 'NONE',  ( 0.000000000000000000, 1.000000000000000000, 0.000000000000000000 ) ) ;
#44106 = EDGE_LOOP ( 'NONE', ( #44681, #69837 ) ) ;
#44105 = CARTESIAN_POINT ( 'NONE',  ( 170.5922698879802510, -35.25383818724482410, 5.000000000000000000 ) ) ;
#44107 = ORIENTED_EDGE ( 'NONE', *, *, #68261, .F. ) ;
#44108 = CARTESIAN_POINT ( 'NONE',  ( 4.456444791733522252E-16, 7.450000000000002842, -19.50000000000000000 ) ) ;
#44109 = CIRCLE ( 'NONE', #1180, 0.3499999999999996447 ) ;
#44110 = DIRECTION ( 'NONE',  ( 0.000000000000000000, 1.000000000000000000, 0.000000000000000000 ) ) ;
#44111 = DIRECTION ( 'NONE',  ( -1.000000000000000000, 0.000000000000000000, 0.000000000000000000 ) ) ;
#44112 = CARTESIAN_POINT ( 'NONE',  ( 7.450000000000006395, 7.250000000000000888, -17.50000000000000000 ) ) ;
#44113 = CARTESIAN_POINT ( 'NONE',  ( 2.005523737882793256, -8.612468434717211352, 26.00000000000000000 ) ) ;
#44114 = ORIENTED_EDGE ( 'NONE', *, *, #8445, .F. ) ;
#44115 = CARTESIAN_POINT ( 'NONE',  ( 6.849523737882814878, 10.30047626211719702, 26.00000000000000711 ) ) ;
#44116 = LINE ( 'NONE', #49083, #62097 ) ;
#44117 = LINE ( 'NONE', #65694, #17544 ) ;
#44118 = VECTOR ( 'NONE', #35641, 1000.000000000000000 ) ;
#44119 = DIRECTION ( 'NONE',  ( 0.7071067811865441310, -0.7071067811865510144, -2.597868168706485034E-16 ) ) ;
#44120 = CARTESIAN_POINT ( 'NONE',  ( 15.50000000000000000, 998.9628421096749662, -22.50000000000000000 ) ) ;
#44121 = DIRECTION ( 'NONE',  ( 0.000000000000000000, 0.000000000000000000, 1.000000000000000000 ) ) ;
#44122 = ORIENTED_EDGE ( 'NONE', *, *, #19176, .F. ) ;
#44123 = DIRECTION ( 'NONE',  ( 1.000000000000000000, -0.000000000000000000, 0.000000000000000000 ) ) ;
#44124 = DIRECTION ( 'NONE',  ( 0.000000000000000000, 3.673940397442059868E-16, -1.000000000000000000 ) ) ;
#44125 = EDGE_LOOP ( 'NONE', ( #40846, #58048, #18331, #3544 ) ) ;
#44126 = LINE ( 'NONE', #54415, #34512 ) ;
#44127 = CARTESIAN_POINT ( 'NONE',  ( 0.000000000000000000, 0.000000000000000000, -12.00000000000000000 ) ) ;
#44128 = DIRECTION ( 'NONE',  ( 0.000000000000000000, 0.000000000000000000, 1.000000000000000000 ) ) ;
#44129 = CARTESIAN_POINT ( 'NONE',  ( 14.74999999999998046, -42.24999999999999289, -26.74999999999998934 ) ) ;
#44130 = DIRECTION ( 'NONE',  ( -0.000000000000000000, -0.000000000000000000, -1.000000000000000000 ) ) ;
#44131 = AXIS2_PLACEMENT_3D ( 'NONE', #67676, #29840, #40804 ) ;
#44132 = EDGE_CURVE ( 'NONE', #27390, #21280, #16476, .T. ) ;
#44133 = DIRECTION ( 'NONE',  ( 1.000000000000000000, -1.047444401652940007E-14, 1.836970198721010706E-16 ) ) ;
#44134 = VERTEX_POINT ( 'NONE', #39166 ) ;
#44135 = DIRECTION ( 'NONE',  ( 1.000000000000000000, 0.000000000000000000, 0.000000000000000000 ) ) ;
#44136 = ORIENTED_EDGE ( 'NONE', *, *, #37793, .T. ) ;
#44138 = ADVANCED_FACE ( 'NONE', ( #65692 ), #6973, .F. ) ;
#44137 = CIRCLE ( 'NONE', #13654, 0.5000000000023396840 ) ;
#44139 = DIRECTION ( 'NONE',  ( 0.000000000000000000, -1.901256929667036381E-12, 1.000000000000000000 ) ) ;
#44140 = EDGE_CURVE ( 'NONE', #60691, #31600, #61060, .T. ) ;
#44141 = ADVANCED_FACE ( 'NONE', ( #28542 ), #50116, .F. ) ;
#44142 = AXIS2_PLACEMENT_3D ( 'NONE', #30937, #10419, #52507 ) ;
#44143 = VECTOR ( 'NONE', #34839, 1000.000000000000000 ) ;
#44144 = DIRECTION ( 'NONE',  ( 1.000000000000000000, 0.000000000000000000, 0.000000000000000000 ) ) ;
#44145 = CARTESIAN_POINT ( 'NONE',  ( 7.000000000000000000, -38.64999999999999858, -12.69999999999999929 ) ) ;
#44146 = ORIENTED_EDGE ( 'NONE', *, *, #56202, .T. ) ;
#44147 = EDGE_CURVE ( 'NONE', #4772, #12650, #55875, .T. ) ;
#44148 = EDGE_LOOP ( 'NONE', ( #32074, #64578, #29562, #6243 ) ) ;
#44149 = EDGE_CURVE ( 'NONE', #42714, #67332, #49774, .T. ) ;
#44150 = DIRECTION ( 'NONE',  ( 1.000000000000000000, -3.491481338843133355E-15, -1.836970198721036344E-16 ) ) ;
#44151 = ORIENTED_EDGE ( 'NONE', *, *, #1696, .F. ) ;
#44152 = CIRCLE ( 'NONE', #35154, 1.000000000000001776 ) ;
#44153 = VERTEX_POINT ( 'NONE', #33515 ) ;
#44154 = CARTESIAN_POINT ( 'NONE',  ( 8.250000000000005329, -8.249999999999998224, -26.00000000000001066 ) ) ;
#44155 = DIRECTION ( 'NONE',  ( -0.6414496315691445849, -0.7671651518153106419, -2.818519042764040096E-16 ) ) ;
#44156 = FACE_OUTER_BOUND ( 'NONE', #42643, .T. ) ;
#44157 = ORIENTED_EDGE ( 'NONE', *, *, #55234, .F. ) ;
#44158 = DIRECTION ( 'NONE',  ( 0.000000000000000000, 0.000000000000000000, 1.000000000000000000 ) ) ;
#44159 = VECTOR ( 'NONE', #24562, 1000.000000000000114 ) ;
#44161 = CARTESIAN_POINT ( 'NONE',  ( -7.813516549646836395, -11.78648345035340661, 455.0000000000000568 ) ) ;
#44160 = DIRECTION ( 'NONE',  ( 1.000000000000000000, -0.000000000000000000, -0.000000000000000000 ) ) ;
#44162 = EDGE_LOOP ( 'NONE', ( #47571, #16801, #44337, #15674, #59109, #9314, #51266, #11493, #31762, #40070, #26424, #3425, #51387, #50174, #51979, #56668, #6102 ) ) ;
#44164 = ORIENTED_EDGE ( 'NONE', *, *, #56847, .T. ) ;
#44163 = DIRECTION ( 'NONE',  ( 1.000000000000000000, -0.000000000000000000, -0.000000000000000000 ) ) ;
#44165 = EDGE_LOOP ( 'NONE', ( #3567, #62711, #60344, #25828 ) ) ;
#44166 = CARTESIAN_POINT ( 'NONE',  ( -2.355476262117229158, 9.547976262117156665, 26.00000000000000711 ) ) ;
#44167 = DIRECTION ( 'NONE',  ( 1.000000000000000000, -0.000000000000000000, -0.000000000000000000 ) ) ;
#44168 = VECTOR ( 'NONE', #48988, 1000.000000000000000 ) ;
#44169 = VERTEX_POINT ( 'NONE', #41247 ) ;
#44170 = ORIENTED_EDGE ( 'NONE', *, *, #14313, .F. ) ;
#44171 = DIRECTION ( 'NONE',  ( 0.000000000000000000, 0.000000000000000000, 1.000000000000000000 ) ) ;
#44172 = CARTESIAN_POINT ( 'NONE',  ( 275.0000000000000000, -38.65000000000095781, -14.49999999999903899 ) ) ;
#44173 = ORIENTED_EDGE ( 'NONE', *, *, #59856, .T. ) ;
#44174 = CARTESIAN_POINT ( 'NONE',  ( -16.75000000000000000, -2.500000000000000000, -23.22168783648699986 ) ) ;
#44175 = CARTESIAN_POINT ( 'NONE',  ( -10.03972626211722918, 9.689726262117183353, 26.00000000000000711 ) ) ;
#44176 = CARTESIAN_POINT ( 'NONE',  ( 290.0000000000000000, -42.50000000000000000, -27.00000000000000000 ) ) ;
#44177 = VECTOR ( 'NONE', #7828, 1000.000000000000000 ) ;
#44178 = ORIENTED_EDGE ( 'NONE', *, *, #49299, .T. ) ;
#44179 = ADVANCED_FACE ( 'NONE', ( #67774 ), #24995, .F. ) ;
#44181 = MANIFOLD_SOLID_BREP ( 'LPattern1[2]', #47640 ) ;
#44180 = LINE ( 'NONE', #43494, #49316 ) ;
#44182 = DIRECTION ( 'NONE',  ( 0.000000000000000000, 0.000000000000000000, -1.000000000000000000 ) ) ;
#44185 = ORIENTED_EDGE ( 'NONE', *, *, #5982, .F. ) ;
#44184 = EDGE_CURVE ( 'NONE', #31486, #45669, #63536, .T. ) ;
#44183 = CARTESIAN_POINT ( 'NONE',  ( -5.779227145995285753, 4.141586236041028712, 54.00000000000000711 ) ) ;
#44187 = ORIENTED_EDGE ( 'NONE', *, *, #28333, .F. ) ;
#44186 = CARTESIAN_POINT ( 'NONE',  ( 4.740315990920131561, -7.811466277050838514, 455.0000000000000568 ) ) ;
#44188 = CARTESIAN_POINT ( 'NONE',  ( -3.667976262117323305, -9.737023737882815055, 26.00000000000000000 ) ) ;
#44189 = CARTESIAN_POINT ( 'NONE',  ( 6.849523737882817542, -10.50702373788281463, 26.00000000000000000 ) ) ;
#44190 = DIRECTION ( 'NONE',  ( 1.000000000000000000, 0.000000000000000000, 0.000000000000000000 ) ) ;
#44191 = LINE ( 'NONE', #12009, #57230 ) ;
#44192 = VECTOR ( 'NONE', #53140, 1000.000000000000000 ) ;
#44193 = CLOSED_SHELL ( 'NONE', ( #12372, #839, #54601, #58039, #28615, #27498, #58280, #55034, #44141, #53584, #66534, #49945, #35256, #29638, #37224, #44472, #8169, #24078, #20285, #55928, #64469, #9370, #30036, #30165, #62520, #1859, #36317, #69523, #21665, #3525, #34089, #9043, #68688, #43145, #69687, #11819, #27111, #9201, #15545, #32829, #48392, #33627, #40152, #23336, #28363, #25667, #48803, #46739, #37834, #16841, #67940, #38332, #42008, #59994, #3119, #28745, #31891, #46567, #59521, #6176, #57117, #37616, #12595, #18130, #21097, #46140, #18315, #66986, #58428, #12292, #50000, #14878, #47504, #64924, #53194, #59489, #46300, #62802, #22205, #40121, #56842, #32992, #55126, #54823, #53152, #35038, #3461, #6674, #5532, #35283, #30350, #11504, #20503, #4390, #61042, #40501, #12179, #59205, #53274, #36163, #31055, #49825, #48135, #37557, #50339, #20719, #17028, #14081, #9293, #16276, #919, #36365, #66780, #17490, #69457, #51694, #12072, #10096, #38026, #48418, #43615, #20217, #19349, #49137, #29380, #43206, #60112, #16943, #39603, #50053, #53267, #40650, #9051, #20501, #2464, #892, #21162, #68832, #39813, #40410, #52343, #60685, #33766, #15999, #18375, #20698, #25061, #1247, #12847, #25067, #59601, #34687, #5448, #8339, #26761, #27501, #12344, #13320, #20303, #52889, #359, #20646, #60239, #47189, #68838, #13325, #40358, #14707, #47369, #46717, #2980, #23437, #60512, #31823, #21038, #67374, #32307, #60069, #12171, #38540, #9109, #47985, #59196, #36969, #18928, #68117, #60040, #44616, #50384, #46432, #37115, #26236, #49447, #15813, #11864, #68826, #19216, #1135, #15635, #21571, #40881, #52852, #1069, #15023, #21899, #20706, #39644, #59481, #48873, #49481, #25973, #53537, #37642, #34437, #16732, #60149, #36420, #35420, #12154, #19, #3935, #25010, #1032, #34950, #48268, #17249, #48839, #52476, #13451, #37979, #47722, #68075, #12075, #31546, #8707, #67421, #8708, #47448, #55580, #27340, #36452, #4349, #27190, #21130, #40489, #24467, #67601, #8284, #54394, #64853, #1227, #15191, #54886, #49213, #50739, #34377, #58942, #6027, #45250, #10579, #62555, #66275, #31582, #31202, #48794, #775, #3530, #63693, #44706, #39475, #43759, #7988, #2631, #5038, #40621, #43686, #25854, #42301, #44577, #12588, #65409, #31957, #14238, #12856, #57758, #16877, #2246, #68769, #13735, #31203, #14569, #9306, #26226, #48738, #68684, #39688, #34110, #51359, #41931, #35971, #50340, #59643, #51222, #7556, #31598, #38357, #8471, #21382, #18859, #65961, #45103, #17813, #2996, #5521, #28654, #8839, #5196, #54462, #43768, #47080, #31061, #4020, #48887, #35428, #57695, #22700, #49430, #43192, #50399, #822, #66881, #68918, #43580, #39048, #507, #2414, #16503, #5953, #24460, #41859, #48574, #69889, #61238, #47247, #40552, #7902, #41750, #54873, #64194, #32028, #43271, #33240, #51130, #24812, #23676, #3604, #15096, #6088, #58203, #19278, #54887, #8025, #64866, #10725, #13131, #49238, #34240, #15971, #40672, #11132, #5628, #7264, #18949, #24616, #38918, #24270, #68704, #65238, #65285, #32908, #10717, #9859, #45896, #21575, #45890, #11952, #66188, #51375, #33069, #31001, #19928, #55664, #4119, #12200, #3041, #40077 ) ) ;
#44194 = DIRECTION ( 'NONE',  ( 1.000000000000000000, 0.000000000000000000, 0.000000000000000000 ) ) ;
#44195 = DIRECTION ( 'NONE',  ( -1.000000000000000000, 0.000000000000000000, 0.000000000000000000 ) ) ;
#44196 = VERTEX_POINT ( 'NONE', #14027 ) ;
#44197 = CYLINDRICAL_SURFACE ( 'NONE', #57520, 1.999999999999312994 ) ;
#44198 = CIRCLE ( 'NONE', #43051, 3.299999999999473577 ) ;
#44200 = ORIENTED_EDGE ( 'NONE', *, *, #11430, .T. ) ;
#44199 = CARTESIAN_POINT ( 'NONE',  ( -8.250000000000001776, 0.000000000000000000, -22.00000000000000000 ) ) ;
#44202 = ORIENTED_EDGE ( 'NONE', *, *, #33074, .F. ) ;
#44201 = CARTESIAN_POINT ( 'NONE',  ( -1.466476262117318852, -9.404523737882838574, 26.00000000000000711 ) ) ;
#44203 = DIRECTION ( 'NONE',  ( 0.000000000000000000, 1.000000000000000000, -0.000000000000000000 ) ) ;
#44204 = LINE ( 'NONE', #65779, #31871 ) ;
#44205 = CIRCLE ( 'NONE', #49817, 0.9999999999984534593 ) ;
#44206 = VERTEX_POINT ( 'NONE', #41957 ) ;
#44207 = CARTESIAN_POINT ( 'NONE',  ( 181.4833316329832940, 5.000000000000000000, 320.8239988703753056 ) ) ;
#44208 = CARTESIAN_POINT ( 'NONE',  ( -7.250000000000001776, -7.249999999999998224, -17.00000000000000000 ) ) ;
#44209 = ORIENTED_EDGE ( 'NONE', *, *, #44947, .F. ) ;
#44210 = DIRECTION ( 'NONE',  ( 0.000000000000000000, 0.000000000000000000, -1.000000000000000000 ) ) ;
#44211 = DIRECTION ( 'NONE',  ( 0.000000000000000000, 1.000000000000000000, 0.000000000000000000 ) ) ;
#44212 = CARTESIAN_POINT ( 'NONE',  ( 1.090483450353338268, -11.34648345035345329, 455.0000000000000568 ) ) ;
#44213 = DIRECTION ( 'NONE',  ( -0.000000000000000000, 0.000000000000000000, 1.000000000000000000 ) ) ;
#44214 = EDGE_CURVE ( 'NONE', #15601, #46187, #35585, .T. ) ;
#44215 = CARTESIAN_POINT ( 'NONE',  ( -8.250000000000000000, 7.250000000000001776, -19.00000000000000000 ) ) ;
#44216 = EDGE_LOOP ( 'NONE', ( #57491, #21, #18113, #21474 ) ) ;
#44217 = CIRCLE ( 'NONE', #23926, 4.500000000000191847 ) ;
#44218 = DIRECTION ( 'NONE',  ( 0.000000000000000000, -1.000000000000000000, 0.000000000000000000 ) ) ;
#44219 = ORIENTED_EDGE ( 'NONE', *, *, #41483, .F. ) ;
#44220 = VERTEX_POINT ( 'NONE', #14395 ) ;
#44221 = CARTESIAN_POINT ( 'NONE',  ( -9.293516549646779978, -10.92648345035333790, 195.0000000000000284 ) ) ;
#44222 = DIRECTION ( 'NONE',  ( -0.000000000000000000, -0.7071067811865474617, 0.7071067811865474617 ) ) ;
#44223 = FACE_OUTER_BOUND ( 'NONE', #51050, .T. ) ;
#44224 = CARTESIAN_POINT ( 'NONE',  ( 8.250000000000005329, -8.249999999999998224, -26.00000000000001066 ) ) ;
#44225 = ORIENTED_EDGE ( 'NONE', *, *, #23355, .T. ) ;
#44226 = EDGE_CURVE ( 'NONE', #65577, #10775, #41187, .T. ) ;
#44227 = ORIENTED_EDGE ( 'NONE', *, *, #2896, .F. ) ;
#44228 = EDGE_CURVE ( 'NONE', #31017, #66383, #57168, .T. ) ;
#44229 = VECTOR ( 'NONE', #16989, 1000.000000000000000 ) ;
#44231 = ORIENTED_EDGE ( 'NONE', *, *, #22900, .F. ) ;
#44230 = DIRECTION ( 'NONE',  ( -1.000000000000000000, 0.000000000000000000, 0.000000000000000000 ) ) ;
#44232 = VERTEX_POINT ( 'NONE', #8733 ) ;
#44233 = PRODUCT ( 'Aluminum Extrusions (T-Slot Profiles)_5537T808', 'Aluminum Extrusions (T-Slot Profiles)_5537T808', '', ( #54027 ) ) ;
#44234 = AXIS2_PLACEMENT_3D ( 'NONE', #34258, #13402, #49845 ) ;
#44235 = CARTESIAN_POINT ( 'NONE',  ( -9.942044687070668019, -9.247904806590694804, 455.0000000000000568 ) ) ;
#44236 = DIRECTION ( 'NONE',  ( -1.000000000000000000, 1.185108578570163402E-14, 1.836970198721051628E-16 ) ) ;
#44237 = EDGE_CURVE ( 'NONE', #28648, #33046, #35953, .T. ) ;
#44238 = LINE ( 'NONE', #17725, #48921 ) ;
#44239 = DIRECTION ( 'NONE',  ( -0.7071067811865474617, 0.7071067811865474617, 2.597868168706479611E-16 ) ) ;
#44241 = CARTESIAN_POINT ( 'NONE',  ( -30.00000000000000000, -5.599999999999999645, 27.00000000000000000 ) ) ;
#44240 = DIRECTION ( 'NONE',  ( 0.8660254037844510311, 0.4999999999999785727, 1.836970198720951294E-16 ) ) ;
#44242 = VERTEX_POINT ( 'NONE', #3772 ) ;
#44244 = ORIENTED_EDGE ( 'NONE', *, *, #64407, .T. ) ;
#44243 = FACE_OUTER_BOUND ( 'NONE', #34958, .T. ) ;
#44245 = ORIENTED_EDGE ( 'NONE', *, *, #31431, .F. ) ;
#44246 = ORIENTED_EDGE ( 'NONE', *, *, #28569, .F. ) ;
#44247 = VECTOR ( 'NONE', #957, 1000.000000000000000 ) ;
#44248 = CIRCLE ( 'NONE', #13758, 24.99999999998784972 ) ;
#44249 = LINE ( 'NONE', #64797, #29920 ) ;
#44250 = LINE ( 'NONE', #65825, #15201 ) ;
#44251 = CIRCLE ( 'NONE', #30582, 1.000000000000000000 ) ;
#44252 = CARTESIAN_POINT ( 'NONE',  ( 35.89999999999999858, -0.2000000000089119934, -8.913009219568841313E-12 ) ) ;
#44253 = CARTESIAN_POINT ( 'NONE',  ( -3.417780618358722933, -7.852485183457003970, 455.0000000000000568 ) ) ;
#44254 = ORIENTED_EDGE ( 'NONE', *, *, #23728, .F. ) ;
#44255 = ORIENTED_EDGE ( 'NONE', *, *, #40635, .T. ) ;
#44256 = AXIS2_PLACEMENT_3D ( 'NONE', #13065, #55523, #7065 ) ;
#44257 = CARTESIAN_POINT ( 'NONE',  ( -11.11351654964671098, 4.193516549646605363, 195.0000000000000284 ) ) ;
#44258 = DIRECTION ( 'NONE',  ( -1.000000000000000000, 0.000000000000000000, 0.000000000000000000 ) ) ;
#44259 = VERTEX_POINT ( 'NONE', #51871 ) ;
#44260 = ORIENTED_EDGE ( 'NONE', *, *, #55803, .T. ) ;
#44261 = DIRECTION ( 'NONE',  ( 1.000000000000000000, 2.135044278125299371E-15, 7.844025423732057781E-31 ) ) ;
#44262 = CARTESIAN_POINT ( 'NONE',  ( -4.193516549646675529, 11.11351654964658842, 455.0000000000000568 ) ) ;
#44263 = ORIENTED_EDGE ( 'NONE', *, *, #54480, .F. ) ;
#44264 = CARTESIAN_POINT ( 'NONE',  ( 11.78648345035337819, -4.186483450353492231, 455.0000000000000568 ) ) ;
#44267 = ORIENTED_EDGE ( 'NONE', *, *, #62382, .F. ) ;
#44266 = EDGE_CURVE ( 'NONE', #28651, #43043, #3429, .T. ) ;
#44265 = CARTESIAN_POINT ( 'NONE',  ( 8.250000000000005329, 7.250000000000000888, -10.00000000000000000 ) ) ;
#44268 = ORIENTED_EDGE ( 'NONE', *, *, #32836, .T. ) ;
#44269 = EDGE_CURVE ( 'NONE', #11693, #4189, #33327, .T. ) ;
#44270 = EDGE_CURVE ( 'NONE', #24121, #32538, #32172, .T. ) ;
#44271 = CARTESIAN_POINT ( 'NONE',  ( 25.90000000000000213, -21.00000000000000000, 13.86939075806900057 ) ) ;
#44272 = CARTESIAN_POINT ( 'NONE',  ( 6.006483450353401921, 5.993516549646582092, 455.0000000000000568 ) ) ;
#44273 = CARTESIAN_POINT ( 'NONE',  ( 11.90000000000000036, -21.00000000000000000, 13.86939075806900057 ) ) ;
#44274 = VECTOR ( 'NONE', #37756, 1000.000000000000000 ) ;
#44275 = CARTESIAN_POINT ( 'NONE',  ( 16.54633693294649532, -0.2717122460102548986, 23.33927276307431598 ) ) ;
#44276 = ADVANCED_FACE ( 'NONE', ( #46549 ), #36300, .F. ) ;
#44277 = LINE ( 'NONE', #18436, #9037 ) ;
#44278 = CIRCLE ( 'NONE', #1389, 4.000000000000000000 ) ;
#44279 = ORIENTED_EDGE ( 'NONE', *, *, #44954, .T. ) ;
#44280 = DIRECTION ( 'NONE',  ( -1.836970198721029934E-16, 1.836970198721036590E-16, -1.000000000000000000 ) ) ;
#44282 = ORIENTED_EDGE ( 'NONE', *, *, #64356, .T. ) ;
#44281 =( NAMED_UNIT ( * ) SI_UNIT ( $, .STERADIAN. ) SOLID_ANGLE_UNIT ( ) );
#44283 = DIRECTION ( 'NONE',  ( -0.000000000000000000, 3.673940397442059868E-16, -1.000000000000000000 ) ) ;
#44284 = DIRECTION ( 'NONE',  ( -1.000000000000000000, 3.491481338843133355E-15, 0.000000000000000000 ) ) ;
#44285 = LINE ( 'NONE', #28376, #31410 ) ;
#44286 = AXIS2_PLACEMENT_3D ( 'NONE', #7101, #28679, #18064 ) ;
#44287 = CARTESIAN_POINT ( 'NONE',  ( 0.000000000000000000, 4.428935149116389924E-16, 3.233000000000000096 ) ) ;
#44288 = CYLINDRICAL_SURFACE ( 'NONE', #61922, 24.99999999998794920 ) ;
#44289 = VERTEX_POINT ( 'NONE', #57863 ) ;
#44290 = AXIS2_PLACEMENT_3D ( 'NONE', #55987, #67996, #24858 ) ;
#44291 = EDGE_LOOP ( 'NONE', ( #4665, #34998, #17025, #12843 ) ) ;
#44292 = LINE ( 'NONE', #16399, #47179 ) ;
#44293 = FILL_AREA_STYLE_COLOUR ( '', #23161 ) ;
#44294 = CIRCLE ( 'NONE', #47746, 0.1749999999999998224 ) ;
#44295 = VERTEX_POINT ( 'NONE', #9430 ) ;
#44296 = MANIFOLD_SOLID_BREP ( 'SAWC-0630-20060_welle', #13708 ) ;
#44297 = DIRECTION ( 'NONE',  ( 1.000000000000000000, 0.000000000000000000, 0.000000000000000000 ) ) ;
#44298 = ORIENTED_EDGE ( 'NONE', *, *, #34476, .F. ) ;
#44299 = VERTEX_POINT ( 'NONE', #4833 ) ;
#44300 = CIRCLE ( 'NONE', #48828, 0.3500000000002719824 ) ;
#44301 = DIRECTION ( 'NONE',  ( 0.000000000000000000, 0.000000000000000000, 1.000000000000000000 ) ) ;
#44302 = CARTESIAN_POINT ( 'NONE',  ( 7.000000000000000000, -42.00000000000000000, 7.000000000000000000 ) ) ;
#44303 = ORIENTED_EDGE ( 'NONE', *, *, #10623, .T. ) ;
#44304 = DIRECTION ( 'NONE',  ( 0.000000000000000000, 0.000000000000000000, -1.000000000000000000 ) ) ;
#44305 = CARTESIAN_POINT ( 'NONE',  ( -4.188533722949421723, -7.272650909786664286, 455.0000000000000568 ) ) ;
#44306 = PRESENTATION_STYLE_ASSIGNMENT (( #27028 ) ) ;
#44307 = DIRECTION ( 'NONE',  ( -0.000000000000000000, -0.000000000000000000, -1.000000000000000000 ) ) ;
#44308 = VERTEX_POINT ( 'NONE', #42653 ) ;
#44310 = ORIENTED_EDGE ( 'NONE', *, *, #18867, .F. ) ;
#44309 = CARTESIAN_POINT ( 'NONE',  ( 7.250000000000005329, -7.249999999999998224, -26.00000000000001066 ) ) ;
#44311 = ADVANCED_FACE ( 'NONE', ( #29941 ), #59620, .F. ) ;
#44312 = LINE ( 'NONE', #21377, #31650 ) ;
#44313 = EDGE_CURVE ( 'NONE', #34946, #24260, #16370, .T. ) ;
#44314 = DIRECTION ( 'NONE',  ( 0.7071067811865539010, 0.7071067811865411334, -1.887411345499491136E-30 ) ) ;
#44315 = LINE ( 'NONE', #51024, #54525 ) ;
#44316 = VERTEX_POINT ( 'NONE', #47611 ) ;
#44317 = EDGE_CURVE ( 'NONE', #43624, #14837, #48315, .T. ) ;
#44318 = CARTESIAN_POINT ( 'NONE',  ( 4.622483450353380263, -3.606483450353491271, 455.0000000000000568 ) ) ;
#44319 = LINE ( 'NONE', #33720, #4796 ) ;
#44320 = EDGE_CURVE ( 'NONE', #48682, #14923, #47962, .T. ) ;
#44321 = CIRCLE ( 'NONE', #68060, 1.000000000000000000 ) ;
#44322 = ORIENTED_EDGE ( 'NONE', *, *, #29253, .T. ) ;
#44323 = ORIENTED_EDGE ( 'NONE', *, *, #24145, .T. ) ;
#44324 = VERTEX_POINT ( 'NONE', #32735 ) ;
#44325 = CYLINDRICAL_SURFACE ( 'NONE', #33275, 24.99999999998784972 ) ;
#44326 = EDGE_CURVE ( 'NONE', #16506, #46286, #26746, .T. ) ;
#44327 = VECTOR ( 'NONE', #43333, 1000.000000000000000 ) ;
#44328 = CARTESIAN_POINT ( 'NONE',  ( -4.734785091273957747, 5.380658396643156038, 455.0000000000000568 ) ) ;
#44329 = EDGE_CURVE ( 'NONE', #56086, #35347, #58922, .T. ) ;
#44330 = DIRECTION ( 'NONE',  ( 0.000000000000000000, 0.000000000000000000, -1.000000000000000000 ) ) ;
#44331 = VERTEX_POINT ( 'NONE', #69870 ) ;
#44332 = ORIENTED_EDGE ( 'NONE', *, *, #49581, .T. ) ;
#44333 = ORIENTED_EDGE ( 'NONE', *, *, #49989, .F. ) ;
#44334 = CARTESIAN_POINT ( 'NONE',  ( -6.344366288193410419, 4.706725378239148050, 54.00000000000000711 ) ) ;
#44335 = EDGE_LOOP ( 'NONE', ( #42513, #33522, #22358, #40365 ) ) ;
#44336 = ORIENTED_EDGE ( 'NONE', *, *, #15675, .F. ) ;
#44337 = ORIENTED_EDGE ( 'NONE', *, *, #10013, .F. ) ;
#44338 = EDGE_LOOP ( 'NONE', ( #58600, #22095 ) ) ;
#44339 = CARTESIAN_POINT ( 'NONE',  ( -11.25000000000000000, 11.18999999999999950, -4.250000000000000000 ) ) ;
#44341 = ORIENTED_EDGE ( 'NONE', *, *, #39356, .T. ) ;
#44340 = CARTESIAN_POINT ( 'NONE',  ( 11.00000000000000000, -5.599999999999379696, -26.60000000000059828 ) ) ;
#44342 = FACE_OUTER_BOUND ( 'NONE', #28550, .T. ) ;
#44344 = DIRECTION ( 'NONE',  ( -1.836970198721029934E-16, 1.836970198721036590E-16, -1.000000000000000000 ) ) ;
#44343 = CIRCLE ( 'NONE', #47792, 0.1999999999999987899 ) ;
#44345 = DIRECTION ( 'NONE',  ( -1.000000000000000000, 0.000000000000000000, 0.000000000000000000 ) ) ;
#44346 = ORIENTED_EDGE ( 'NONE', *, *, #11174, .F. ) ;
#44347 = VECTOR ( 'NONE', #46204, 1000.000000000000000 ) ;
#44348 = VECTOR ( 'NONE', #18291, 1000.000000000000000 ) ;
#44349 = CARTESIAN_POINT ( 'NONE',  ( 275.0000000000000000, -39.79999999999954952, 8.900000000000419575 ) ) ;
#44350 = DIRECTION ( 'NONE',  ( 5.013651664672856055E-16, -1.000000000000000000, -3.673940397442059868E-16 ) ) ;
#44351 = DIRECTION ( 'NONE',  ( -9.050731179009442381E-15, -1.000000000000000000, 0.000000000000000000 ) ) ;
#44352 = VECTOR ( 'NONE', #21862, 1000.000000000000000 ) ;
#44353 = ORIENTED_EDGE ( 'NONE', *, *, #45452, .T. ) ;
#44354 = CARTESIAN_POINT ( 'NONE',  ( -7.517976262117260333, 3.834182069070703580, 26.00000000000000711 ) ) ;
#44355 = CARTESIAN_POINT ( 'NONE',  ( -11.50000000000000000, -12.00000000000000000, -11.03137303340310282 ) ) ;
#44356 = CONICAL_SURFACE ( 'NONE', #19537, 2.000000000000001776, 0.7853981633974503884 ) ;
#44357 = DIRECTION ( 'NONE',  ( 0.000000000000000000, -1.000000000000000000, 0.000000000000000000 ) ) ;
#44358 = ORIENTED_EDGE ( 'NONE', *, *, #36690, .F. ) ;
#44359 = CARTESIAN_POINT ( 'NONE',  ( 30.00000000000000000, -16.28999999999710369, 15.00000000000794920 ) ) ;
#44360 = EDGE_CURVE ( 'NONE', #53303, #40434, #21435, .T. ) ;
#44361 = FACE_BOUND ( 'NONE', #32627, .T. ) ;
#44362 = DIRECTION ( 'NONE',  ( -1.000000000000000000, 0.000000000000000000, 0.000000000000000000 ) ) ;
#44363 = AXIS2_PLACEMENT_3D ( 'NONE', #18468, #61600, #23087 ) ;
#44364 = EDGE_CURVE ( 'NONE', #37823, #52634, #65283, .T. ) ;
#44365 = CARTESIAN_POINT ( 'NONE',  ( 9.690000000000001279, 9.750000000000000000, -5.000000000000000000 ) ) ;
#44366 = PLANE ( 'NONE',  #22306 ) ;
#44367 = FACE_OUTER_BOUND ( 'NONE', #61968, .T. ) ;
#44368 = AXIS2_PLACEMENT_3D ( 'NONE', #18542, #42124, #58044 ) ;
#44369 = CARTESIAN_POINT ( 'NONE',  ( 9.795823737882805915, -9.795823737882811244, 54.00000000000000711 ) ) ;
#44370 = DIRECTION ( 'NONE',  ( -1.000000000000000000, 9.973078850062113474E-15, -1.836970198721011692E-16 ) ) ;
#44371 = VERTEX_POINT ( 'NONE', #16130 ) ;
#44372 = DIRECTION ( 'NONE',  ( 1.000000000000000000, 0.000000000000000000, 0.000000000000000000 ) ) ;
#44373 = LINE ( 'NONE', #28464, #1455 ) ;
#44374 = AXIS2_PLACEMENT_3D ( 'NONE', #37492, #32182, #26889 ) ;
#44375 = PLANE ( 'NONE',  #35769 ) ;
#44376 = CARTESIAN_POINT ( 'NONE',  ( 7.000000000000000000, -25.60000000000000142, -17.60000000000000142 ) ) ;
#44377 = ORIENTED_EDGE ( 'NONE', *, *, #11805, .T. ) ;
#44378 = CARTESIAN_POINT ( 'NONE',  ( 7.616533956692213003, -8.406483450353396947, 195.0000000000000284 ) ) ;
#44379 = DIRECTION ( 'NONE',  ( -0.7071067811865446862, 0.7071067811865503483, -0.000000000000000000 ) ) ;
#44380 = EDGE_CURVE ( 'NONE', #16502, #9404, #10821, .T. ) ;
#44381 = CARTESIAN_POINT ( 'NONE',  ( 0.000000000000000000, -8.249999999999998224, -12.00000000000000000 ) ) ;
#44382 = DIRECTION ( 'NONE',  ( -0.000000000000000000, 0.000000000000000000, 1.000000000000000000 ) ) ;
#44383 = CARTESIAN_POINT ( 'NONE',  ( 11.18999999999999950, -11.18999999999999950, 0.000000000000000000 ) ) ;
#44384 = EDGE_LOOP ( 'NONE', ( #3347, #31910, #21135, #56018, #51878, #51995, #43984, #45334 ) ) ;
#44385 = VECTOR ( 'NONE', #9649, 1000.000000000000000 ) ;
#44386 = CYLINDRICAL_SURFACE ( 'NONE', #4487, 1.000000000000002665 ) ;
#44387 = EDGE_CURVE ( 'NONE', #34666, #19227, #16829, .T. ) ;
#44388 = CARTESIAN_POINT ( 'NONE',  ( -29.25000000000000000, -5.000000000000000000, 11.75000000000000000 ) ) ;
#44389 = VERTEX_POINT ( 'NONE', #59953 ) ;
#44390 = AXIS2_PLACEMENT_3D ( 'NONE', #35691, #8833, #9190 ) ;
#44391 = CIRCLE ( 'NONE', #13928, 0.2999999999994937827 ) ;
#44392 = DIRECTION ( 'NONE',  ( -0.000000000000000000, 1.000000000000000000, -0.000000000000000000 ) ) ;
#44393 = AXIS2_PLACEMENT_3D ( 'NONE', #38281, #59835, #33652 ) ;
#44394 = VERTEX_POINT ( 'NONE', #43703 ) ;
#44395 = DIRECTION ( 'NONE',  ( 1.000000000000000000, 0.000000000000000000, 0.000000000000000000 ) ) ;
#44397 = VERTEX_POINT ( 'NONE', #16484 ) ;
#44396 = VECTOR ( 'NONE', #17227, 1000.000000000000000 ) ;
#44398 = VECTOR ( 'NONE', #12961, 1000.000000000000000 ) ;
#44399 = ORIENTED_EDGE ( 'NONE', *, *, #13805, .T. ) ;
#44401 = ADVANCED_FACE ( 'NONE', ( #10135 ), #38396, .T. ) ;
#44400 = DIRECTION ( 'NONE',  ( -1.836970198721029934E-16, -1.836970198721010706E-16, 1.000000000000000000 ) ) ;
#44402 = PLANE ( 'NONE',  #16199 ) ;
#44403 = ADVANCED_FACE ( 'NONE', ( #26058 ), #42300, .F. ) ;
#44404 = CYLINDRICAL_SURFACE ( 'NONE', #29337, 1.500000000000000444 ) ;
#44405 = CARTESIAN_POINT ( 'NONE',  ( -8.250000000000001776, 0.000000000000000000, -25.50000000000000355 ) ) ;
#44406 = MANIFOLD_SOLID_BREP ( 'LPattern1[24]', #2453 ) ;
#44407 = ORIENTED_EDGE ( 'NONE', *, *, #50547, .F. ) ;
#44408 = EDGE_LOOP ( 'NONE', ( #33963, #38695, #14616, #42062 ) ) ;
#44409 = CARTESIAN_POINT ( 'NONE',  ( 49.00000000000000000, -0.2000000000089119934, -8.913009219568841313E-12 ) ) ;
#44410 = DIRECTION ( 'NONE',  ( 1.000000000000000000, -3.016910393003147986E-15, 0.000000000000000000 ) ) ;
#44411 = ORIENTED_EDGE ( 'NONE', *, *, #34647, .F. ) ;
#44412 = EDGE_CURVE ( 'NONE', #55597, #66058, #58162, .T. ) ;
#44413 = ORIENTED_EDGE ( 'NONE', *, *, #21979, .F. ) ;
#44414 = ORIENTED_EDGE ( 'NONE', *, *, #52326, .T. ) ;
#44415 = CARTESIAN_POINT ( 'NONE',  ( -11.00000000000000000, -16.28999999999999915, 14.50000000000000000 ) ) ;
#44416 = CARTESIAN_POINT ( 'NONE',  ( -7.259684009079930611, 4.188533722949235205, 455.0000000000000568 ) ) ;
#44418 = ORIENTED_EDGE ( 'NONE', *, *, #13575, .T. ) ;
#44417 = FACE_OUTER_BOUND ( 'NONE', #68317, .T. ) ;
#44419 = DIRECTION ( 'NONE',  ( 0.000000000000000000, 0.000000000000000000, -1.000000000000000000 ) ) ;
#44420 = DIRECTION ( 'NONE',  ( -7.457533623526253657E-15, -1.000000000000000000, -1.836970198721024757E-16 ) ) ;
#44421 = ORIENTED_EDGE ( 'NONE', *, *, #17948, .T. ) ;
#44422 = VERTEX_POINT ( 'NONE', #66991 ) ;
#44423 = AXIS2_PLACEMENT_3D ( 'NONE', #62034, #13254, #2642 ) ;
#44424 = ORIENTED_EDGE ( 'NONE', *, *, #5256, .F. ) ;
#44425 = AXIS2_PLACEMENT_3D ( 'NONE', #68821, #21077, #20379 ) ;
#44426 = EDGE_CURVE ( 'NONE', #38926, #68454, #33085, .T. ) ;
#44427 = CARTESIAN_POINT ( 'NONE',  ( 5.257023737882819070, -5.257023737882815517, 26.00000000000000711 ) ) ;
#44428 = CARTESIAN_POINT ( 'NONE',  ( 3.664523737882820598, 10.49297626211720491, 54.00000000000000711 ) ) ;
#44429 = PLANE ( 'NONE',  #28153 ) ;
#44430 = EDGE_CURVE ( 'NONE', #3728, #67414, #31057, .T. ) ;
#44431 = ADVANCED_BREP_SHAPE_REPRESENTATION ( '', ( #66405, #45918 ), #64023 ) ;
#44432 = AXIS2_PLACEMENT_3D ( 'NONE', #55866, #19431, #23346 ) ;
#44433 = VECTOR ( 'NONE', #35909, 1000.000000000000000 ) ;
#44434 = CARTESIAN_POINT ( 'NONE',  ( 28.00000000000000000, -15.50000000000000000, 14.50000000000000000 ) ) ;
#44435 = CARTESIAN_POINT ( 'NONE',  ( 15.50000000000000000, -5.000000000000000000, 22.50000000000000000 ) ) ;
#44437 = ORIENTED_EDGE ( 'NONE', *, *, #63349, .T. ) ;
#44436 = LINE ( 'NONE', #50457, #13933 ) ;
#44438 = ORIENTED_EDGE ( 'NONE', *, *, #18939, .T. ) ;
#44439 = ADVANCED_FACE ( 'NONE', ( #22820 ), #28459, .F. ) ;
#44440 = DIRECTION ( 'NONE',  ( -1.000000000000000000, 0.000000000000000000, 0.000000000000000000 ) ) ;
#44441 = PRESENTATION_LAYER_ASSIGNMENT (  '', '', ( #11749 ) ) ;
#44442 = LINE ( 'NONE', #38476, #36364 ) ;
#44443 = ADVANCED_FACE ( 'NONE', ( #34108 ), #6217, .T. ) ;
#44444 = DIRECTION ( 'NONE',  ( 0.000000000000000000, -1.000000000000000000, 0.000000000000000000 ) ) ;
#44445 = DIRECTION ( 'NONE',  ( -1.000000000000000000, 8.728482790395504563E-15, 0.000000000000000000 ) ) ;
#44446 = CIRCLE ( 'NONE', #23014, 3.232999999999965901 ) ;
#44447 = CIRCLE ( 'NONE', #13979, 1.224999999999999423 ) ;
#44448 = EDGE_CURVE ( 'NONE', #48595, #39506, #24278, .T. ) ;
#44449 = CARTESIAN_POINT ( 'NONE',  ( -25.50000000000000355, -5.578999999999999737, 24.12099999999999866 ) ) ;
#44450 = EDGE_LOOP ( 'NONE', ( #27241, #40069, #51390, #22533 ) ) ;
#44451 = CYLINDRICAL_SURFACE ( 'NONE', #36954, 1.929199999999998028 ) ;
#44452 = CARTESIAN_POINT ( 'NONE',  ( 35.89999999999999858, -21.00000000000000000, 13.86939075806900057 ) ) ;
#44453 = LINE ( 'NONE', #44803, #4066 ) ;
#44454 = LINE ( 'NONE', #54403, #5154 ) ;
#44455 = LINE ( 'NONE', #60374, #55223 ) ;
#44456 = EDGE_CURVE ( 'NONE', #7568, #30669, #54835, .T. ) ;
#44457 = DIRECTION ( 'NONE',  ( 0.000000000000000000, 0.000000000000000000, -1.000000000000000000 ) ) ;
#44458 = ADVANCED_FACE ( 'NONE', ( #23512 ), #12197, .T. ) ;
#44459 = LINE ( 'NONE', #65021, #47670 ) ;
#44460 = VERTEX_POINT ( 'NONE', #45069 ) ;
#44461 = CARTESIAN_POINT ( 'NONE',  ( 275.0000000000000000, -42.00000000000000000, 26.50000000000000000 ) ) ;
#44462 = CARTESIAN_POINT ( 'NONE',  ( 151.5599459900709860, 0.000000000000000000, 324.6739988703752715 ) ) ;
#44463 = EDGE_CURVE ( 'NONE', #52731, #48724, #34451, .T. ) ;
#44464 = ORIENTED_EDGE ( 'NONE', *, *, #56932, .F. ) ;
#44465 = CARTESIAN_POINT ( 'NONE',  ( 8.250000000000005329, -8.249999999999998224, -26.00000000000001066 ) ) ;
#44466 = EDGE_CURVE ( 'NONE', #54250, #58687, #44032, .T. ) ;
#44467 = EDGE_CURVE ( 'NONE', #51741, #18742, #45419, .T. ) ;
#44468 = PLANE ( 'NONE',  #12978 ) ;
#44469 = LINE ( 'NONE', #50819, #10691 ) ;
#44470 = CARTESIAN_POINT ( 'NONE',  ( 30.00000000000000000, -12.00000000000000000, -12.20000000000000107 ) ) ;
#44471 = DIRECTION ( 'NONE',  ( 1.000000000000000000, 0.000000000000000000, 0.000000000000000000 ) ) ;
#44472 = ADVANCED_FACE ( 'NONE', ( #38730 ), #62688, .F. ) ;
#44473 = CARTESIAN_POINT ( 'NONE',  ( 11.50000000000000000, -11.50000000000000000, 15.00000000000000000 ) ) ;
#44474 = ORIENTED_EDGE ( 'NONE', *, *, #5137, .F. ) ;
#44475 = ADVANCED_FACE ( 'NONE', ( #56733 ), #26571, .F. ) ;
#44476 = DIRECTION ( 'NONE',  ( 0.000000000000000000, 0.000000000000000000, 1.000000000000000000 ) ) ;
#44477 = ORIENTED_EDGE ( 'NONE', *, *, #23874, .F. ) ;
#44478 = CYLINDRICAL_SURFACE ( 'NONE', #60743, 3.499999999999999556 ) ;
#44479 = CARTESIAN_POINT ( 'NONE',  ( -11.18999999999999950, 11.18999999999999950, -5.000000000000000000 ) ) ;
#44480 = DIRECTION ( 'NONE',  ( 1.836970198721029934E-16, 1.836970198721010706E-16, -1.000000000000000000 ) ) ;
#44481 = ORIENTED_EDGE ( 'NONE', *, *, #12073, .F. ) ;
#44482 = ORIENTED_EDGE ( 'NONE', *, *, #6442, .T. ) ;
#44484 = EDGE_CURVE ( 'NONE', #38571, #19166, #63094, .T. ) ;
#44483 = CARTESIAN_POINT ( 'NONE',  ( 12.00648345035340903, 7.813516549646560172, 455.0000000000000568 ) ) ;
#44485 = VERTEX_POINT ( 'NONE', #45774 ) ;
#44486 = ORIENTED_EDGE ( 'NONE', *, *, #9778, .F. ) ;
#44487 = EDGE_CURVE ( 'NONE', #59410, #4281, #29512, .T. ) ;
#44488 = CARTESIAN_POINT ( 'NONE',  ( 8.606483450353380249, -4.396432944014562416, 195.0000000000000284 ) ) ;
#44489 = LINE ( 'NONE', #1714, #39207 ) ;
#44490 = AXIS2_PLACEMENT_3D ( 'NONE', #6647, #49784, #43091 ) ;
#44491 = AXIS2_PLACEMENT_3D ( 'NONE', #18154, #12157, #39716 ) ;
#44492 = CARTESIAN_POINT ( 'NONE',  ( 3.677663764522614454, -4.149127210878770455, 54.00000000000000711 ) ) ;
#44493 = EDGE_LOOP ( 'NONE', ( #1469, #51599, #22530, #67888 ) ) ;
#44494 = DIRECTION ( 'NONE',  ( 1.000000000000000000, -0.000000000000000000, 0.000000000000000000 ) ) ;
#44496 = CARTESIAN_POINT ( 'NONE',  ( 9.562023737882766383, 2.530476262117153485, 54.00000000000000711 ) ) ;
#44495 = DIRECTION ( 'NONE',  ( -1.000000000000000000, 3.491481338843133355E-15, 1.836970198721036344E-16 ) ) ;
#44497 = COLOUR_RGB ( '', 0.72549020, 0.75294118, 0.79215686) ;
#44499 = ORIENTED_EDGE ( 'NONE', *, *, #62848, .F. ) ;
#44498 = CIRCLE ( 'NONE', #20794, 1.499999999997024602 ) ;
#44501 = EDGE_LOOP ( 'NONE', ( #58171, #5955, #66755, #35920, #16357, #27894, #22590 ) ) ;
#44500 = CARTESIAN_POINT ( 'NONE',  ( 9.841277389592722358, -1.690483450353490680, 455.0000000000000568 ) ) ;
#44502 = ORIENTED_EDGE ( 'NONE', *, *, #6497, .F. ) ;
#44503 = DIRECTION ( 'NONE',  ( 1.000000000000000000, 0.000000000000000000, 0.000000000000000000 ) ) ;
#44504 = AXIS2_PLACEMENT_3D ( 'NONE', #17630, #39203, #51198 ) ;
#44505 = CARTESIAN_POINT ( 'NONE',  ( 40.90000000000000568, 20.60000000000000142, -13.86939075806900057 ) ) ;
#44506 = DIRECTION ( 'NONE',  ( 1.000000000000000000, 0.000000000000000000, 0.000000000000000000 ) ) ;
#44507 = EDGE_LOOP ( 'NONE', ( #24073, #4425, #1878, #39210 ) ) ;
#44508 = ORIENTED_EDGE ( 'NONE', *, *, #68938, .F. ) ;
#44509 = CIRCLE ( 'NONE', #47968, 2.204799999999997429 ) ;
#44510 = LINE ( 'NONE', #45557, #42548 ) ;
#44511 = FACE_OUTER_BOUND ( 'NONE', #5736, .T. ) ;
#44512 = ORIENTED_EDGE ( 'NONE', *, *, #46913, .F. ) ;
#44513 = LINE ( 'NONE', #11312, #16171 ) ;
#44514 = CYLINDRICAL_SURFACE ( 'NONE', #43672, 3.499999999999055866 ) ;
#44515 = CARTESIAN_POINT ( 'NONE',  ( -11.00000000000000000, -11.70000000000000284, 12.50000000000000000 ) ) ;
#44516 = VERTEX_POINT ( 'NONE', #51435 ) ;
#44517 = EDGE_CURVE ( 'NONE', #42310, #65332, #68357, .T. ) ;
#44518 = DIRECTION ( 'NONE',  ( 0.000000000000000000, -0.5017180897718488408, -0.8650311892618017806 ) ) ;
#44519 = PLANE ( 'NONE',  #43034 ) ;
#44520 = AXIS2_PLACEMENT_3D ( 'NONE', #15904, #47726, #68949 ) ;
#44522 = VERTEX_POINT ( 'NONE', #14653 ) ;
#44521 = LINE ( 'NONE', #50878, #56654 ) ;
#44524 = VERTEX_POINT ( 'NONE', #3345 ) ;
#44523 = FACE_OUTER_BOUND ( 'NONE', #22925, .T. ) ;
#44525 = EDGE_CURVE ( 'NONE', #46957, #39153, #62377, .T. ) ;
#44526 = CARTESIAN_POINT ( 'NONE',  ( -10.08346604330787777, 2.693516549646604918, 455.0000000000000568 ) ) ;
#44527 = LINE ( 'NONE', #61854, #35184 ) ;
#44528 = EDGE_CURVE ( 'NONE', #40439, #48107, #30225, .T. ) ;
#44529 = AXIS2_PLACEMENT_3D ( 'NONE', #35965, #57530, #30316 ) ;
#44530 = FACE_OUTER_BOUND ( 'NONE', #31537, .T. ) ;
#44531 = DIRECTION ( 'NONE',  ( 1.000000000000000000, -0.000000000000000000, -0.000000000000000000 ) ) ;
#44532 = DIRECTION ( 'NONE',  ( 1.671920889371702854E-15, -1.000000000000000000, 0.000000000000000000 ) ) ;
#44533 = EDGE_CURVE ( 'NONE', #41138, #64942, #46886, .T. ) ;
#44534 = DIRECTION ( 'NONE',  ( 0.000000000000000000, 0.000000000000000000, 1.000000000000000000 ) ) ;
#44535 = ORIENTED_EDGE ( 'NONE', *, *, #27887, .F. ) ;
#44536 = CARTESIAN_POINT ( 'NONE',  ( 4.206483450353343478, -11.12648345035338160, 195.0000000000000284 ) ) ;
#44537 = CARTESIAN_POINT ( 'NONE',  ( -17.51999999999999957, -15.50000000000000000, 26.00000000000000355 ) ) ;
#44538 = CARTESIAN_POINT ( 'NONE',  ( 8.835729544836325999, 7.955476262117193720, 26.00000000000000711 ) ) ;
#44540 = ORIENTED_EDGE ( 'NONE', *, *, #5863, .T. ) ;
#44539 = LINE ( 'NONE', #17686, #5098 ) ;
#44541 = AXIS2_PLACEMENT_3D ( 'NONE', #944, #43007, #47972 ) ;
#44542 = VECTOR ( 'NONE', #51298, 1000.000000000000000 ) ;
#44543 = DIRECTION ( 'NONE',  ( -0.9583148474998870459, 0.000000000000000000, 0.2857142857143623593 ) ) ;
#44544 = DIRECTION ( 'NONE',  ( -8.339399738404102667E-15, -1.000000000000000000, -1.836970198721025990E-16 ) ) ;
#44545 = VECTOR ( 'NONE', #67305, 1000.000000000000000 ) ;
#44546 = ORIENTED_EDGE ( 'NONE', *, *, #68261, .T. ) ;
#44547 = DIRECTION ( 'NONE',  ( -1.000000000000000000, 0.000000000000000000, 0.000000000000000000 ) ) ;
#44548 = CARTESIAN_POINT ( 'NONE',  ( 39.00000000000000000, 0.000000000000000000, 3.500000000000000000 ) ) ;
#44549 = VERTEX_POINT ( 'NONE', #62028 ) ;
#44550 = ADVANCED_FACE ( 'NONE', ( #35499 ), #51077, .F. ) ;
#44551 = CARTESIAN_POINT ( 'NONE',  ( 18.85410196625000268, -15.50000000000000000, 21.50000000000000000 ) ) ;
#44552 = DIRECTION ( 'NONE',  ( -1.000000000000000000, 1.794541526872559352E-16, 0.000000000000000000 ) ) ;
#44553 = CIRCLE ( 'NONE', #47957, 2.204799999999999205 ) ;
#44554 = CARTESIAN_POINT ( 'NONE',  ( -7.517976262117260333, 3.834182069070703580, 54.00000000000000711 ) ) ;
#44555 = CARTESIAN_POINT ( 'NONE',  ( 0.000000000000000000, -7.449999999999998401, -14.50000000000000000 ) ) ;
#44556 = DIRECTION ( 'NONE',  ( 1.000000000000000000, -0.000000000000000000, 0.000000000000000000 ) ) ;
#44557 = PRESENTATION_LAYER_ASSIGNMENT (  '', '', ( #35526 ) ) ;
#44558 = ORIENTED_EDGE ( 'NONE', *, *, #23811, .F. ) ;
#44559 = DIRECTION ( 'NONE',  ( 0.000000000000000000, 0.7057491738665943037, -0.7084617869628675457 ) ) ;
#44560 = ORIENTED_EDGE ( 'NONE', *, *, #10666, .T. ) ;
#44561 = ORIENTED_EDGE ( 'NONE', *, *, #12390, .T. ) ;
#44562 = AXIS2_PLACEMENT_3D ( 'NONE', #67911, #62589, #68963 ) ;
#44563 = LINE ( 'NONE', #54854, #40357 ) ;
#44564 = CARTESIAN_POINT ( 'NONE',  ( -7.793516549646827940, -11.12648345035340647, 455.0000000000000568 ) ) ;
#44565 = DIRECTION ( 'NONE',  ( -1.000000000000000000, 1.920885163218982051E-15, 1.836970198721033385E-16 ) ) ;
#44566 = DIRECTION ( 'NONE',  ( 0.000000000000000000, 0.000000000000000000, 1.000000000000000000 ) ) ;
#44567 = ORIENTED_EDGE ( 'NONE', *, *, #25487, .T. ) ;
#44568 = VERTEX_POINT ( 'NONE', #4057 ) ;
#44570 = ADVANCED_FACE ( 'NONE', ( #24570 ), #25627, .F. ) ;
#44569 = CARTESIAN_POINT ( 'NONE',  ( 17.24945551514599984, -15.50000000000000000, 25.53140320652400064 ) ) ;
#44571 = ORIENTED_EDGE ( 'NONE', *, *, #16936, .F. ) ;
#44572 = EDGE_CURVE ( 'NONE', #35627, #34716, #61682, .T. ) ;
#44573 = CARTESIAN_POINT ( 'NONE',  ( 30.00000000000000000, -10.85999999999999943, 9.350000000000269651 ) ) ;
#44574 = DIRECTION ( 'NONE',  ( -0.000000000000000000, -0.000000000000000000, -1.000000000000000000 ) ) ;
#44575 = LINE ( 'NONE', #55553, #12737 ) ;
#44576 = AXIS2_PLACEMENT_3D ( 'NONE', #38178, #32525, #1038 ) ;
#44577 = ADVANCED_FACE ( 'NONE', ( #40471 ), #34805, .T. ) ;
#44579 = CARTESIAN_POINT ( 'NONE',  ( 8.930623737882839919, 8.916576262117192897, 26.00000000000000711 ) ) ;
#44578 = FACE_OUTER_BOUND ( 'NONE', #46805, .T. ) ;
#44580 = ORIENTED_EDGE ( 'NONE', *, *, #59715, .T. ) ;
#44582 = VERTEX_POINT ( 'NONE', #57085 ) ;
#44581 = DIRECTION ( 'NONE',  ( -1.000000000000000000, 0.000000000000000000, 0.000000000000000000 ) ) ;
#44583 = VECTOR ( 'NONE', #4766, 1000.000000000000000 ) ;
#44584 = VERTEX_POINT ( 'NONE', #19254 ) ;
#44585 = ORIENTED_EDGE ( 'NONE', *, *, #5442, .F. ) ;
#44586 = DIRECTION ( 'NONE',  ( 2.135044278125299371E-15, -1.000000000000000000, -3.673940397442060361E-16 ) ) ;
#44587 = VECTOR ( 'NONE', #45947, 1000.000000000000000 ) ;
#44588 = CARTESIAN_POINT ( 'NONE',  ( -0.9414762621172296786, 9.390476262117148920, 26.00000000000000711 ) ) ;
#44589 = CIRCLE ( 'NONE', #35725, 4.500000000000191847 ) ;
#44590 = CARTESIAN_POINT ( 'NONE',  ( 41.09999999999999432, -21.00000000000000000, -13.86939075806900057 ) ) ;
#44591 = ORIENTED_EDGE ( 'NONE', *, *, #39315, .T. ) ;
#44592 = ORIENTED_EDGE ( 'NONE', *, *, #448, .T. ) ;
#44593 = CIRCLE ( 'NONE', #31105, 1.999999999999314770 ) ;
#44594 = AXIS2_PLACEMENT_3D ( 'NONE', #60400, #333, #11275 ) ;
#44595 = CARTESIAN_POINT ( 'NONE',  ( 10.31452373788281562, -3.857023737882824932, 54.00000000000000711 ) ) ;
#44596 = CARTESIAN_POINT ( 'NONE',  ( 16.33565937784172917, -0.3156604612126716614, -21.53909249377372959 ) ) ;
#44597 = ORIENTED_EDGE ( 'NONE', *, *, #7274, .F. ) ;
#44598 = ORIENTED_EDGE ( 'NONE', *, *, #2801, .F. ) ;
#44599 = DIRECTION ( 'NONE',  ( -1.034072152899300274E-14, -1.000000000000000000, 0.000000000000000000 ) ) ;
#44600 = CARTESIAN_POINT ( 'NONE',  ( 4.149127210878725158, -3.677663764522648648, 54.00000000000000711 ) ) ;
#44601 = EDGE_LOOP ( 'NONE', ( #53775, #63320, #35234, #19453 ) ) ;
#44602 = EDGE_CURVE ( 'NONE', #34574, #44814, #40823, .T. ) ;
#44603 = LINE ( 'NONE', #39651, #10893 ) ;
#44605 = EDGE_LOOP ( 'NONE', ( #46492, #42475, #64114, #57058 ) ) ;
#44604 = CARTESIAN_POINT ( 'NONE',  ( 41.09999999999999432, -14.06939075806901940, -20.80000000000000426 ) ) ;
#44606 = VECTOR ( 'NONE', #9780, 1000.000000000000000 ) ;
#44607 = EDGE_LOOP ( 'NONE', ( #12054, #31261, #61390, #64546 ) ) ;
#44608 = DIRECTION ( 'NONE',  ( -0.000000000000000000, -0.000000000000000000, 1.000000000000000000 ) ) ;
#44609 = DIRECTION ( 'NONE',  ( -0.000000000000000000, -1.000000000000000000, -0.000000000000000000 ) ) ;
#44610 = LINE ( 'NONE', #44273, #30617 ) ;
#44611 = ADVANCED_FACE ( 'NONE', ( #14314 ), #24912, .F. ) ;
#44612 = DIRECTION ( 'NONE',  ( 0.000000000000000000, 0.000000000000000000, 1.000000000000000000 ) ) ;
#44613 = EDGE_CURVE ( 'NONE', #18754, #63213, #52135, .T. ) ;
#44614 = FACE_OUTER_BOUND ( 'NONE', #1107, .T. ) ;
#44615 = DIRECTION ( 'NONE',  ( -1.000000000000000000, 0.000000000000000000, 0.000000000000000000 ) ) ;
#44616 = ADVANCED_FACE ( 'NONE', ( #62734 ), #25265, .F. ) ;
#44617 = ADVANCED_FACE ( 'NONE', ( #32663 ), #21004, .F. ) ;
#44618 = ORIENTED_EDGE ( 'NONE', *, *, #39862, .F. ) ;
#44619 = CARTESIAN_POINT ( 'NONE',  ( 29.50000000000000355, -15.46862696659690073, -14.50000000000000000 ) ) ;
#44621 = ORIENTED_EDGE ( 'NONE', *, *, #58200, .F. ) ;
#44620 = LINE ( 'NONE', #66207, #11855 ) ;
#44622 = CARTESIAN_POINT ( 'NONE',  ( 6.006483450353379716, -6.006483450353490738, 455.0000000000000568 ) ) ;
#44623 = LINE ( 'NONE', #44983, #8597 ) ;
#44624 = EDGE_CURVE ( 'NONE', #56702, #49332, #51437, .T. ) ;
#44625 = LINE ( 'NONE', #50290, #30234 ) ;
#44626 = CARTESIAN_POINT ( 'NONE',  ( 4.206483450353422526, 11.31351654964658415, 455.0000000000000568 ) ) ;
#44627 = DIRECTION ( 'NONE',  ( -1.836970198721029934E-16, 1.836970198721036590E-16, -1.000000000000000000 ) ) ;
#44628 = VERTEX_POINT ( 'NONE', #25976 ) ;
#44629 = EDGE_LOOP ( 'NONE', ( #12816, #64893, #23900, #33291 ) ) ;
#44630 = AXIS2_PLACEMENT_3D ( 'NONE', #23596, #12629, #28220 ) ;
#44631 = DIRECTION ( 'NONE',  ( 0.000000000000000000, 0.000000000000000000, 1.000000000000000000 ) ) ;
#44632 = CARTESIAN_POINT ( 'NONE',  ( 7.250000000000005329, -7.249999999999998224, -21.50000000000000000 ) ) ;
#44633 = VECTOR ( 'NONE', #1921, 1000.000000000000000 ) ;
#44634 = VECTOR ( 'NONE', #40640, 1000.000000000000000 ) ;
#44635 = AXIS2_PLACEMENT_3D ( 'NONE', #68011, #47156, #63058 ) ;
#44636 = PLANE ( 'NONE',  #15003 ) ;
#44637 = ORIENTED_EDGE ( 'NONE', *, *, #22324, .F. ) ;
#44638 = MANIFOLD_SOLID_BREP ( 'LPattern1[14]', #52131 ) ;
#44639 = DIRECTION ( 'NONE',  ( 1.000000000000000000, -0.000000000000000000, -0.000000000000000000 ) ) ;
#44640 = ORIENTED_EDGE ( 'NONE', *, *, #44463, .T. ) ;
#44641 = ORIENTED_EDGE ( 'NONE', *, *, #10808, .F. ) ;
#44642 = DIRECTION ( 'NONE',  ( 0.000000000000000000, -0.000000000000000000, 1.000000000000000000 ) ) ;
#44643 = CARTESIAN_POINT ( 'NONE',  ( 2.369523737882786918, -9.562023737882798358, 54.00000000000000711 ) ) ;
#44644 = AXIS2_PLACEMENT_3D ( 'NONE', #31740, #63202, #10159 ) ;
#44645 = VECTOR ( 'NONE', #7537, 1000.000000000000000 ) ;
#44646 = ORIENTED_EDGE ( 'NONE', *, *, #54013, .F. ) ;
#44647 = CARTESIAN_POINT ( 'NONE',  ( 8.465062094116069247, -4.255011587777349114, 455.0000000000000568 ) ) ;
#44648 = VECTOR ( 'NONE', #52314, 1000.000000000000000 ) ;
#44649 = DIRECTION ( 'NONE',  ( 0.000000000000000000, -0.9239212585478484563, -0.3825826812642726948 ) ) ;
#44650 = VERTEX_POINT ( 'NONE', #53207 ) ;
#44652 = EDGE_LOOP ( 'NONE', ( #13773, #53001, #43448, #5717, #51713, #62397, #64460, #24861 ) ) ;
#44651 = CARTESIAN_POINT ( 'NONE',  ( 0.000000000000000000, 8.250000000000001776, -11.50000000000000000 ) ) ;
#44653 = AXIS2_PLACEMENT_3D ( 'NONE', #5967, #49097, #48757 ) ;
#44654 = DIRECTION ( 'NONE',  ( 0.000000000000000000, 1.000000000000000000, 3.673940397442059868E-16 ) ) ;
#44655 = LINE ( 'NONE', #17804, #24865 ) ;
#44656 = LINE ( 'NONE', #55982, #32348 ) ;
#44657 = LINE ( 'NONE', #56329, #24003 ) ;
#44658 = VERTEX_POINT ( 'NONE', #32321 ) ;
#44659 = EDGE_CURVE ( 'NONE', #40699, #16092, #36941, .T. ) ;
#44660 = STYLED_ITEM ( 'NONE', ( #20909 ), #43625 ) ;
#44661 = EDGE_CURVE ( 'NONE', #8538, #37841, #42218, .T. ) ;
#44662 = PLANE ( 'NONE',  #33365 ) ;
#44663 = CARTESIAN_POINT ( 'NONE',  ( -7.252248008019492431, -6.619341603356823533, 455.0000000000000568 ) ) ;
#44664 = ORIENTED_EDGE ( 'NONE', *, *, #33454, .F. ) ;
#44665 = ORIENTED_EDGE ( 'NONE', *, *, #35860, .T. ) ;
#44666 = EDGE_CURVE ( 'NONE', #10486, #37791, #15710, .T. ) ;
#44667 = EDGE_LOOP ( 'NONE', ( #62967, #41548, #21502, #18137 ) ) ;
#44668 = CARTESIAN_POINT ( 'NONE',  ( 11.50000000000000000, -15.46862696659690073, -14.50000000000000000 ) ) ;
#44669 = DIRECTION ( 'NONE',  ( 1.836970198721029934E-16, -1.836970198721036344E-16, 1.000000000000000000 ) ) ;
#44670 = DIRECTION ( 'NONE',  ( 1.000000000000000000, 0.000000000000000000, 0.000000000000000000 ) ) ;
#44671 = LINE ( 'NONE', #1549, #63199 ) ;
#44672 = ORIENTED_EDGE ( 'NONE', *, *, #58050, .T. ) ;
#44673 = ORIENTED_EDGE ( 'NONE', *, *, #42126, .F. ) ;
#44674 = AXIS2_PLACEMENT_3D ( 'NONE', #12870, #40095, #34436 ) ;
#44675 = ORIENTED_EDGE ( 'NONE', *, *, #45537, .T. ) ;
#44676 = CARTESIAN_POINT ( 'NONE',  ( -28.00000000000000000, -16.64230188589299786, -14.64519951917100116 ) ) ;
#44677 = EDGE_LOOP ( 'NONE', ( #53872, #52266, #64418, #6226 ) ) ;
#44678 = CIRCLE ( 'NONE', #1786, 1.000000000000000000 ) ;
#44679 = ORIENTED_EDGE ( 'NONE', *, *, #29063, .T. ) ;
#44680 = VERTEX_POINT ( 'NONE', #63448 ) ;
#44681 = ORIENTED_EDGE ( 'NONE', *, *, #48403, .T. ) ;
#44682 = VECTOR ( 'NONE', #33448, 1000.000000000000000 ) ;
#44683 = DIRECTION ( 'NONE',  ( 0.000000000000000000, 0.000000000000000000, 1.000000000000000000 ) ) ;
#44685 = ORIENTED_EDGE ( 'NONE', *, *, #47759, .T. ) ;
#44684 = DIRECTION ( 'NONE',  ( -1.000000000000000000, 0.000000000000000000, 0.000000000000000000 ) ) ;
#44686 = CARTESIAN_POINT ( 'NONE',  ( -3.142976262117251451, 6.486996718459839606, 26.00000000000000711 ) ) ;
#44687 = CIRCLE ( 'NONE', #14220, 0.1999999999999996503 ) ;
#44688 = AXIS2_PLACEMENT_3D ( 'NONE', #68487, #21437, #46901 ) ;
#44689 = CARTESIAN_POINT ( 'NONE',  ( 28.00000000000000000, -15.50000000000000000, -14.49999999999999645 ) ) ;
#44690 = CARTESIAN_POINT ( 'NONE',  ( 8.250000000000005329, -8.249999999999998224, -26.00000000000001066 ) ) ;
#44692 = EDGE_LOOP ( 'NONE', ( #20896, #49820 ) ) ;
#44691 = DIRECTION ( 'NONE',  ( -1.000000000000000000, 0.000000000000000000, 0.000000000000000000 ) ) ;
#44693 = AXIS2_PLACEMENT_3D ( 'NONE', #53954, #30979, #9772 ) ;
#44694 = VECTOR ( 'NONE', #53490, 1000.000000000000000 ) ;
#44695 = CIRCLE ( 'NONE', #9707, 5.000000000000000000 ) ;
#44696 = DIRECTION ( 'NONE',  ( 0.000000000000000000, 0.000000000000000000, -1.000000000000000000 ) ) ;
#44697 = DIRECTION ( 'NONE',  ( -0.000000000000000000, -0.000000000000000000, -1.000000000000000000 ) ) ;
#44698 = LINE ( 'NONE', #55672, #2219 ) ;
#44699 = AXIS2_PLACEMENT_3D ( 'NONE', #27412, #17141, #48987 ) ;
#44700 = ADVANCED_FACE ( 'NONE', ( #15007 ), #36565, .F. ) ;
#44701 = ORIENTED_EDGE ( 'NONE', *, *, #5564, .F. ) ;
#44702 = FACE_OUTER_BOUND ( 'NONE', #10884, .T. ) ;
#44703 = AXIS2_PLACEMENT_3D ( 'NONE', #20053, #40908, #41618 ) ;
#44704 = PLANE ( 'NONE',  #34297 ) ;
#44705 = CARTESIAN_POINT ( 'NONE',  ( 9.306483450353379538, -10.92648345035348534, 455.0000000000000568 ) ) ;
#44706 = ADVANCED_FACE ( 'NONE', ( #10404 ), #54241, .F. ) ;
#44707 = ADVANCED_FACE ( 'NONE', ( #48582, #48237 ), #53898, .F. ) ;
#44708 = ORIENTED_EDGE ( 'NONE', *, *, #67747, .F. ) ;
#44709 = CIRCLE ( 'NONE', #33428, 24.99999999998784972 ) ;
#44710 = DIRECTION ( 'NONE',  ( 0.000000000000000000, -0.7071067811865480168, 0.7071067811865470176 ) ) ;
#44711 = PLANE ( 'NONE',  #27393 ) ;
#44712 = LINE ( 'NONE', #13242, #25770 ) ;
#44713 = ORIENTED_EDGE ( 'NONE', *, *, #69132, .T. ) ;
#44714 = LINE ( 'NONE', #18199, #38809 ) ;
#44715 = LINE ( 'NONE', #16128, #57630 ) ;
#44717 = EDGE_CURVE ( 'NONE', #43043, #4784, #50271, .T. ) ;
#44716 = DIRECTION ( 'NONE',  ( 1.000000000000000000, -0.000000000000000000, 0.000000000000000000 ) ) ;
#44718 = FACE_OUTER_BOUND ( 'NONE', #52165, .T. ) ;
#44719 = ORIENTED_EDGE ( 'NONE', *, *, #2425, .F. ) ;
#44720 = CARTESIAN_POINT ( 'NONE',  ( 10.50702373788280752, 6.835476262117182067, 54.00000000000000711 ) ) ;
#44721 = DIRECTION ( 'NONE',  ( 0.000000000000000000, 0.7071067811865074937, 0.7071067811865876518 ) ) ;
#44722 = COLOUR_RGB ( '', 0.40784314, 0.44705882, 0.49803922) ;
#44723 = DIRECTION ( 'NONE',  ( 1.000000000000000000, 0.000000000000000000, 0.000000000000000000 ) ) ;
#44724 = CARTESIAN_POINT ( 'NONE',  ( -2.693516549646675529, 10.91351654964657314, 455.0000000000000568 ) ) ;
#44725 = DIRECTION ( 'NONE',  ( 0.000000000000000000, -0.7096009616570518874, 0.7046037717862339012 ) ) ;
#44726 = ORIENTED_EDGE ( 'NONE', *, *, #48254, .T. ) ;
#44727 = FACE_OUTER_BOUND ( 'NONE', #1195, .T. ) ;
#44728 = CARTESIAN_POINT ( 'NONE',  ( -8.250000000000001776, -7.249999999999998224, -26.00000000000001066 ) ) ;
#44729 = AXIS2_PLACEMENT_3D ( 'NONE', #12484, #7874, #2583 ) ;
#44730 = LINE ( 'NONE', #55702, #61587 ) ;
#44731 = AXIS2_PLACEMENT_3D ( 'NONE', #58733, #15608, #19838 ) ;
#44732 = DIRECTION ( 'NONE',  ( -0.000000000000000000, -1.000000000000000000, 0.000000000000000000 ) ) ;
#44733 = CARTESIAN_POINT ( 'NONE',  ( 7.250000000000005329, -7.449999999999998401, -8.500000000000000000 ) ) ;
#44734 = ORIENTED_EDGE ( 'NONE', *, *, #54954, .F. ) ;
#44735 = ORIENTED_EDGE ( 'NONE', *, *, #52442, .F. ) ;
#44736 = AXIS2_PLACEMENT_3D ( 'NONE', #63596, #3149, #9146 ) ;
#44737 = DIRECTION ( 'NONE',  ( -0.000000000000000000, 0.000000000000000000, -1.000000000000000000 ) ) ;
#44738 = CARTESIAN_POINT ( 'NONE',  ( -6.642976262117260333, 10.30047626211718104, 54.00000000000000711 ) ) ;
#44739 = VERTEX_POINT ( 'NONE', #5800 ) ;
#44740 = VECTOR ( 'NONE', #65186, 1000.000000000000000 ) ;
#44741 = VECTOR ( 'NONE', #6, 1000.000000000000000 ) ;
#44742 = DIRECTION ( 'NONE',  ( 0.000000000000000000, -1.000000000000000000, 0.000000000000000000 ) ) ;
#44743 = ORIENTED_EDGE ( 'NONE', *, *, #46630, .F. ) ;
#44744 = EDGE_CURVE ( 'NONE', #17547, #64954, #48933, .T. ) ;
#44745 = VECTOR ( 'NONE', #29651, 1000.000000000000000 ) ;
#44746 = DIRECTION ( 'NONE',  ( 0.000000000000000000, 0.000000000000000000, 1.000000000000000000 ) ) ;
#44747 = ORIENTED_EDGE ( 'NONE', *, *, #47720, .F. ) ;
#44748 = ORIENTED_EDGE ( 'NONE', *, *, #36692, .F. ) ;
#44749 = LINE ( 'NONE', #28492, #33992 ) ;
#44750 = CARTESIAN_POINT ( 'NONE',  ( 39.90000000000000568, -0.2000000000000000111, 0.000000000000000000 ) ) ;
#44751 = DIRECTION ( 'NONE',  ( 0.000000000000000000, 0.000000000000000000, -1.000000000000000000 ) ) ;
#44752 = CARTESIAN_POINT ( 'NONE',  ( 158.0064834503532722, -35.83962462487175316, 5.000000000000000000 ) ) ;
#44753 = AXIS2_PLACEMENT_3D ( 'NONE', #13226, #34788, #61295 ) ;
#44754 = MANIFOLD_SOLID_BREP ( 'Cut-Extrude8', #60051 ) ;
#44755 = EDGE_LOOP ( 'NONE', ( #64545, #15684, #57747, #12583 ) ) ;
#44756 = ORIENTED_EDGE ( 'NONE', *, *, #1630, .T. ) ;
#44757 = DIRECTION ( 'NONE',  ( -0.4998444328988824181, 0.000000000000000000, 0.8661152018640445593 ) ) ;
#44758 = CARTESIAN_POINT ( 'NONE',  ( 283.0000000000000568, -20.40000000000000213, -12.40000000000000213 ) ) ;
#44759 = ADVANCED_FACE ( 'NONE', ( #65870 ), #4413, .F. ) ;
#44760 = ORIENTED_EDGE ( 'NONE', *, *, #54891, .T. ) ;
#44761 = ORIENTED_EDGE ( 'NONE', *, *, #35706, .T. ) ;
#44762 = VERTEX_POINT ( 'NONE', #38322 ) ;
#44763 = ADVANCED_FACE ( 'NONE', ( #17089 ), #23436, .F. ) ;
#44764 = CARTESIAN_POINT ( 'NONE',  ( -4.188533722949335569, 7.259684009079808931, 455.0000000000000568 ) ) ;
#44766 = EDGE_LOOP ( 'NONE', ( #12476, #24600, #55395, #65637 ) ) ;
#44765 = DIRECTION ( 'NONE',  ( 0.000000000000000000, -5.800915303574361727E-12, 1.000000000000000000 ) ) ;
#44767 = LINE ( 'NONE', #16538, #19832 ) ;
#44768 = DIRECTION ( 'NONE',  ( 0.000000000000000000, 1.000000000000000000, 0.000000000000000000 ) ) ;
#44769 = AXIS2_PLACEMENT_3D ( 'NONE', #14916, #52048, #52398 ) ;
#44770 = ORIENTED_EDGE ( 'NONE', *, *, #47280, .T. ) ;
#44771 = ORIENTED_EDGE ( 'NONE', *, *, #8638, .T. ) ;
#44772 = AXIS2_PLACEMENT_3D ( 'NONE', #50454, #29924, #18258 ) ;
#44773 = CARTESIAN_POINT ( 'NONE',  ( 283.0000000000000568, -32.95000000000000284, -14.50000000000000000 ) ) ;
#44774 = CARTESIAN_POINT ( 'NONE',  ( 7.450000000000006395, 7.250000000000000888, -13.50000000000000178 ) ) ;
#44775 = AXIS2_PLACEMENT_3D ( 'NONE', #7405, #50556, #61859 ) ;
#44776 = AXIS2_PLACEMENT_3D ( 'NONE', #26203, #4640, #64049 ) ;
#44777 = CARTESIAN_POINT ( 'NONE',  ( -25.50000000000000355, -5.578999999999999737, 20.87899999999999778 ) ) ;
#44778 = EDGE_CURVE ( 'NONE', #57965, #25895, #55955, .T. ) ;
#44779 = AXIS2_PLACEMENT_3D ( 'NONE', #19963, #66998, #24920 ) ;
#44780 = AXIS2_PLACEMENT_3D ( 'NONE', #15931, #37502, #5677 ) ;
#44781 = CARTESIAN_POINT ( 'NONE',  ( 14.25000000000000178, -0.2714405302574884327, 22.98746066354537732 ) ) ;
#44783 = DIRECTION ( 'NONE',  ( 0.000000000000000000, 1.000000000000000000, 0.000000000000000000 ) ) ;
#44782 =( GEOMETRIC_REPRESENTATION_CONTEXT ( 3 ) GLOBAL_UNCERTAINTY_ASSIGNED_CONTEXT ( ( #47928 ) ) GLOBAL_UNIT_ASSIGNED_CONTEXT ( ( #55997, #24164, #50680 ) ) REPRESENTATION_CONTEXT ( 'NONE', 'WORKASPACE' ) );
#44784 = EDGE_CURVE ( 'NONE', #35155, #36053, #33009, .T. ) ;
#44785 = EDGE_CURVE ( 'NONE', #51180, #61547, #59877, .T. ) ;
#44787 = VERTEX_POINT ( 'NONE', #6492 ) ;
#44786 = CARTESIAN_POINT ( 'NONE',  ( 39.90000000000000568, 16.96999999999999886, -21.00000000000000000 ) ) ;
#44788 = VERTEX_POINT ( 'NONE', #54588 ) ;
#44789 = DIRECTION ( 'NONE',  ( 1.000000000000000000, -5.981805089575196197E-17, 0.000000000000000000 ) ) ;
#44790 = VECTOR ( 'NONE', #2704, 1000.000000000000000 ) ;
#44791 = VECTOR ( 'NONE', #29358, 1000.000000000000000 ) ;
#44792 = CARTESIAN_POINT ( 'NONE',  ( 0.000000000000000000, -8.249999999999998224, -17.50000000000000000 ) ) ;
#44793 = EDGE_CURVE ( 'NONE', #15217, #22970, #17782, .T. ) ;
#44794 = CARTESIAN_POINT ( 'NONE',  ( 7.250000000000005329, 7.250000000000000888, -8.000000000000000000 ) ) ;
#44795 = LINE ( 'NONE', #49078, #39609 ) ;
#44796 = EDGE_CURVE ( 'NONE', #48238, #34255, #38996, .T. ) ;
#44797 = VECTOR ( 'NONE', #27497, 1000.000000000000114 ) ;
#44798 = DIRECTION ( 'NONE',  ( -1.000000000000000000, 0.000000000000000000, 0.000000000000000000 ) ) ;
#44799 = ADVANCED_FACE ( 'NONE', ( #23079 ), #60217, .F. ) ;
#44800 = ORIENTED_EDGE ( 'NONE', *, *, #3055, .F. ) ;
#44801 = DIRECTION ( 'NONE',  ( -1.000000000000000000, 0.000000000000000000, 0.000000000000000000 ) ) ;
#44802 = DIRECTION ( 'NONE',  ( -5.013651664672856055E-16, 1.000000000000000000, 0.000000000000000000 ) ) ;
#44804 = ADVANCED_FACE ( 'NONE', ( #7513 ), #12120, .F. ) ;
#44803 = CARTESIAN_POINT ( 'NONE',  ( 283.0000000000000568, -25.56180396883900130, -14.25872597390799967 ) ) ;
#44805 = DIRECTION ( 'NONE',  ( 1.000000000000000000, 0.000000000000000000, 0.000000000000000000 ) ) ;
#44806 = PRODUCT ( 'SAWC-0630-60S_wagen', 'SAWC-0630-60S_wagen', '', ( #3825 ) ) ;
#44807 = AXIS2_PLACEMENT_3D ( 'NONE', #52384, #20200, #58743 ) ;
#44808 = LINE ( 'NONE', #35588, #24733 ) ;
#44809 = CARTESIAN_POINT ( 'NONE',  ( -15.50000000000000000, -5.000000000000000000, 22.50000000000000000 ) ) ;
#44810 = DIRECTION ( 'NONE',  ( -1.000000000000000000, 0.000000000000000000, 0.000000000000000000 ) ) ;
#44811 = ORIENTED_EDGE ( 'NONE', *, *, #48560, .T. ) ;
#44812 = CARTESIAN_POINT ( 'NONE',  ( 39.00000000000000000, 21.00000000000000000, 16.96999999999999886 ) ) ;
#44813 = DIRECTION ( 'NONE',  ( 0.000000000000000000, 1.000000000000000000, 0.000000000000000000 ) ) ;
#44814 = VERTEX_POINT ( 'NONE', #33354 ) ;
#44815 = PLANE ( 'NONE',  #677 ) ;
#44816 = DIRECTION ( 'NONE',  ( 1.000000000000000000, 0.000000000000000000, 0.000000000000000000 ) ) ;
#44817 = DIRECTION ( 'NONE',  ( -1.836970198721029934E-16, 1.836970198721036344E-16, -1.000000000000000000 ) ) ;
#44818 = CARTESIAN_POINT ( 'NONE',  ( 50.83090410532631864, 63.65740854044501162, 0.8284271247461908461 ) ) ;
#44819 = FACE_OUTER_BOUND ( 'NONE', #809, .T. ) ;
#44820 = VERTEX_POINT ( 'NONE', #54939 ) ;
#44821 = CARTESIAN_POINT ( 'NONE',  ( -8.250000000000001776, -7.249999999999998224, -7.500000000000000000 ) ) ;
#44822 = ORIENTED_EDGE ( 'NONE', *, *, #32760, .F. ) ;
#44823 = FACE_OUTER_BOUND ( 'NONE', #40936, .T. ) ;
#44824 = EDGE_CURVE ( 'NONE', #18463, #62655, #30034, .T. ) ;
#44825 = STYLED_ITEM ( 'NONE', ( #40106 ), #20823 ) ;
#44826 = VERTEX_POINT ( 'NONE', #55610 ) ;
#44827 = DIRECTION ( 'NONE',  ( 1.000000000000000000, -5.120954910632640039E-15, 0.000000000000000000 ) ) ;
#44828 = EDGE_CURVE ( 'NONE', #59074, #40124, #7156, .T. ) ;
#44829 = DIRECTION ( 'NONE',  ( 0.000000000000000000, 0.000000000000000000, 1.000000000000000000 ) ) ;
#44830 = CIRCLE ( 'NONE', #14371, 0.1749999999999989342 ) ;
#44831 = VECTOR ( 'NONE', #69610, 1000.000000000000000 ) ;
#44832 = CARTESIAN_POINT ( 'NONE',  ( -6.775514141871427753, -7.408280051175141878, 54.00000000000000711 ) ) ;
#44833 = VERTEX_POINT ( 'NONE', #47358 ) ;
#44834 = EDGE_LOOP ( 'NONE', ( #21006, #17058, #37561, #42448 ) ) ;
#44835 = LINE ( 'NONE', #65727, #61037 ) ;
#44836 = VERTEX_POINT ( 'NONE', #35072 ) ;
#44837 = ADVANCED_FACE ( 'NONE', ( #14842 ), #31810, .T. ) ;
#44838 = ORIENTED_EDGE ( 'NONE', *, *, #67231, .T. ) ;
#44839 = VECTOR ( 'NONE', #21716, 1000.000000000000000 ) ;
#44840 = VECTOR ( 'NONE', #38376, 1000.000000000000000 ) ;
#44841 = DIRECTION ( 'NONE',  ( -1.836970198721029934E-16, 1.836970198721036344E-16, -1.000000000000000000 ) ) ;
#44842 = DIRECTION ( 'NONE',  ( 1.000000000000000000, 0.000000000000000000, 0.000000000000000000 ) ) ;
#44843 = CARTESIAN_POINT ( 'NONE',  ( -9.689726262117227762, 8.566576262117216345, 54.00000000000000711 ) ) ;
#44844 = EDGE_CURVE ( 'NONE', #1369, #30511, #58176, .T. ) ;
#44845 = EDGE_LOOP ( 'NONE', ( #54457, #35983, #62546, #25130 ) ) ;
#44846 = FACE_OUTER_BOUND ( 'NONE', #23903, .T. ) ;
#44847 = AXIS2_PLACEMENT_3D ( 'NONE', #39411, #1253, #22812 ) ;
#44848 = VECTOR ( 'NONE', #23975, 1000.000000000000000 ) ;
#44850 = CARTESIAN_POINT ( 'NONE',  ( 146.5599459900709860, 0.000000000000000000, 316.5239988703752942 ) ) ;
#44849 = DIRECTION ( 'NONE',  ( 1.000000000000000000, 0.000000000000000000, 0.000000000000000000 ) ) ;
#44851 = ORIENTED_EDGE ( 'NONE', *, *, #40229, .T. ) ;
#44853 = ORIENTED_EDGE ( 'NONE', *, *, #47931, .F. ) ;
#44852 = CARTESIAN_POINT ( 'NONE',  ( 78.77321854994620765, 47.95351654967443977, 15.00000000000000000 ) ) ;
#44854 = VERTEX_POINT ( 'NONE', #4587 ) ;
#44855 =( NAMED_UNIT ( * ) SI_UNIT ( $, .STERADIAN. ) SOLID_ANGLE_UNIT ( ) );
#44856 = ADVANCED_FACE ( 'NONE', ( #68586 ), #45332, .F. ) ;
#44857 = PLANE ( 'NONE',  #41219 ) ;
#44858 = ORIENTED_EDGE ( 'NONE', *, *, #29939, .F. ) ;
#44859 = VECTOR ( 'NONE', #25788, 1000.000000000000000 ) ;
#44860 = DIRECTION ( 'NONE',  ( 0.000000000000000000, 0.000000000000000000, -1.000000000000000000 ) ) ;
#44861 = CARTESIAN_POINT ( 'NONE',  ( 7.450000000000006395, 7.250000000000000888, -7.500000000000000000 ) ) ;
#44862 = ORIENTED_EDGE ( 'NONE', *, *, #44016, .F. ) ;
#44863 = EDGE_CURVE ( 'NONE', #10779, #20267, #11947, .T. ) ;
#44864 = VERTEX_POINT ( 'NONE', #66901 ) ;
#44865 = ADVANCED_FACE ( 'NONE', ( #68931 ), #13517, .F. ) ;
#44866 = CARTESIAN_POINT ( 'NONE',  ( -8.250000000000000000, 7.250000000000001776, -10.00000000000000000 ) ) ;
#44867 = PLANE ( 'NONE',  #26704 ) ;
#44868 = EDGE_CURVE ( 'NONE', #16007, #18237, #30753, .T. ) ;
#44869 = EDGE_CURVE ( 'NONE', #23171, #51803, #25808, .T. ) ;
#44870 = EDGE_CURVE ( 'NONE', #42714, #20373, #20486, .T. ) ;
#44871 = ORIENTED_EDGE ( 'NONE', *, *, #55239, .F. ) ;
#44872 = LINE ( 'NONE', #38876, #68099 ) ;
#44873 = CARTESIAN_POINT ( 'NONE',  ( 7.000000000000000000, -27.13000000000000611, -15.49999999999930012 ) ) ;
#44874 = CARTESIAN_POINT ( 'NONE',  ( 8.250000000000005329, -7.249999999999998224, -22.50000000000000000 ) ) ;
#44875 = ORIENTED_EDGE ( 'NONE', *, *, #26941, .T. ) ;
#44876 = EDGE_CURVE ( 'NONE', #53195, #60406, #25447, .T. ) ;
#44878 = MANIFOLD_SOLID_BREP ( 'Move Face1[2]', #45347 ) ;
#44877 = DIRECTION ( 'NONE',  ( 0.000000000000000000, 0.000000000000000000, -1.000000000000000000 ) ) ;
#44879 = EDGE_CURVE ( 'NONE', #19218, #28927, #42405, .T. ) ;
#44880 = FACE_OUTER_BOUND ( 'NONE', #3526, .T. ) ;
#44881 = AXIS2_PLACEMENT_3D ( 'NONE', #47186, #3694, #9350 ) ;
#44883 = ORIENTED_EDGE ( 'NONE', *, *, #60152, .T. ) ;
#44882 = DIRECTION ( 'NONE',  ( 1.000000000000000000, -0.000000000000000000, 0.000000000000000000 ) ) ;
#44885 = ORIENTED_EDGE ( 'NONE', *, *, #60518, .T. ) ;
#44884 = DIRECTION ( 'NONE',  ( -1.836970198721029934E-16, 1.836970198721036344E-16, -1.000000000000000000 ) ) ;
#44886 = EDGE_CURVE ( 'NONE', #33439, #45646, #13165, .T. ) ;
#44887 = DIRECTION ( 'NONE',  ( 0.000000000000000000, 0.000000000000000000, 1.000000000000000000 ) ) ;
#44888 = DIRECTION ( 'NONE',  ( 0.000000000000000000, 1.000000000000000000, 0.000000000000000000 ) ) ;
#44889 = CARTESIAN_POINT ( 'NONE',  ( 29.50000000000000355, -11.50000000000000000, 15.00000000000000000 ) ) ;
#44890 = DIRECTION ( 'NONE',  ( -0.7071067811865503483, 0.7071067811865446862, 0.000000000000000000 ) ) ;
#44891 = AXIS2_PLACEMENT_3D ( 'NONE', #28185, #38130, #988 ) ;
#44892 = VECTOR ( 'NONE', #63866, 1000.000000000000000 ) ;
#44893 = LINE ( 'NONE', #13760, #31976 ) ;
#44894 = EDGE_CURVE ( 'NONE', #51193, #47490, #24129, .T. ) ;
#44895 = ORIENTED_EDGE ( 'NONE', *, *, #19729, .F. ) ;
#44896 = CARTESIAN_POINT ( 'NONE',  ( -7.450000000000001954, 7.250000000000000000, -25.50000000000000355 ) ) ;
#44897 = PLANE ( 'NONE',  #68841 ) ;
#44899 = EDGE_CURVE ( 'NONE', #8098, #40022, #56305, .T. ) ;
#44898 = PLANE ( 'NONE',  #10813 ) ;
#44900 = AXIS2_PLACEMENT_3D ( 'NONE', #4678, #32238, #68321 ) ;
#44903 = ORIENTED_EDGE ( 'NONE', *, *, #50536, .T. ) ;
#44902 = DIRECTION ( 'NONE',  ( -1.000000000000000000, 0.000000000000000000, 0.000000000000000000 ) ) ;
#44901 = AXIS2_PLACEMENT_3D ( 'NONE', #35389, #44965, #2522 ) ;
#44904 = DIRECTION ( 'NONE',  ( -1.000000000000000000, 0.000000000000000000, 0.000000000000000000 ) ) ;
#44905 = AXIS2_PLACEMENT_3D ( 'NONE', #49510, #54819, #66457 ) ;
#44906 = CARTESIAN_POINT ( 'NONE',  ( -11.00000000000000000, -9.199999999999999289, -12.69999999999986073 ) ) ;
#44907 = AXIS2_PLACEMENT_3D ( 'NONE', #46038, #13508, #67610 ) ;
#44908 = VECTOR ( 'NONE', #39875, 1000.000000000000000 ) ;
#44909 = ORIENTED_EDGE ( 'NONE', *, *, #59660, .T. ) ;
#44910 = CARTESIAN_POINT ( 'NONE',  ( 7.749999999999998224, -7.348062532928000934, 0.000000000000000000 ) ) ;
#44911 = CARTESIAN_POINT ( 'NONE',  ( 6.006483450353379716, -6.006483450353490738, 455.0000000000000568 ) ) ;
#44912 = ADVANCED_FACE ( 'NONE', ( #17257 ), #11940, .F. ) ;
#44913 = ORIENTED_EDGE ( 'NONE', *, *, #13001, .T. ) ;
#44914 = LINE ( 'NONE', #11683, #14284 ) ;
#44915 = DIRECTION ( 'NONE',  ( -0.000000000000000000, -0.000000000000000000, 1.000000000000000000 ) ) ;
#44916 = CARTESIAN_POINT ( 'NONE',  ( -11.11351654964679270, -7.806483450353373321, 455.0000000000000568 ) ) ;
#44917 = DIRECTION ( 'NONE',  ( -1.000000000000000000, 0.000000000000000000, 0.000000000000000000 ) ) ;
#44918 = VECTOR ( 'NONE', #10554, 1000.000000000000114 ) ;
#44919 = CARTESIAN_POINT ( 'NONE',  ( 7.450000000000004619, -1.336933437520057563E-15, -23.50000000000000000 ) ) ;
#44920 = ORIENTED_EDGE ( 'NONE', *, *, #11910, .T. ) ;
#44921 = CARTESIAN_POINT ( 'NONE',  ( -3.663616288757055806, 6.350872789121238426, 54.00000000000000711 ) ) ;
#44922 = ORIENTED_EDGE ( 'NONE', *, *, #17652, .T. ) ;
#44923 = ORIENTED_EDGE ( 'NONE', *, *, #57610, .T. ) ;
#44924 = LINE ( 'NONE', #55881, #26860 ) ;
#44925 = EDGE_CURVE ( 'NONE', #1191, #24869, #14186, .T. ) ;
#44926 = LINE ( 'NONE', #39612, #64873 ) ;
#44927 = CARTESIAN_POINT ( 'NONE',  ( 15.00000000000000000, -20.40000000000000213, -17.60000000000000142 ) ) ;
#44928 = ORIENTED_EDGE ( 'NONE', *, *, #62161, .F. ) ;
#44929 = EDGE_LOOP ( 'NONE', ( #47829, #21323, #68328, #11550 ) ) ;
#44930 = FACE_OUTER_BOUND ( 'NONE', #20545, .T. ) ;
#44931 = VERTEX_POINT ( 'NONE', #16225 ) ;
#44932 = EDGE_CURVE ( 'NONE', #36248, #16269, #22577, .T. ) ;
#44933 = DIRECTION ( 'NONE',  ( -1.000000000000000000, 0.000000000000000000, 0.000000000000000000 ) ) ;
#44934 = CARTESIAN_POINT ( 'NONE',  ( 1.690483450353344352, -10.74648345035345720, 455.0000000000000568 ) ) ;
#44935 = CARTESIAN_POINT ( 'NONE',  ( 0.000000000000000000, 0.000000000000000000, -25.50000000000000355 ) ) ;
#44936 = CIRCLE ( 'NONE', #50596, 4.500000000000190958 ) ;
#44937 = EDGE_CURVE ( 'NONE', #40641, #6826, #69976, .T. ) ;
#44938 = CARTESIAN_POINT ( 'NONE',  ( 7.000000000000000000, -21.00000000000000000, 0.000000000000000000 ) ) ;
#44940 = CARTESIAN_POINT ( 'NONE',  ( -7.250000000000000888, -8.249999999999998224, -26.00000000000001066 ) ) ;
#44939 = LINE ( 'NONE', #40685, #65969 ) ;
#44941 = ORIENTED_EDGE ( 'NONE', *, *, #64488, .T. ) ;
#44942 = EDGE_CURVE ( 'NONE', #31244, #39907, #44126, .T. ) ;
#44944 = EDGE_LOOP ( 'NONE', ( #45169, #32237, #20866, #8922 ) ) ;
#44943 = FACE_OUTER_BOUND ( 'NONE', #61434, .T. ) ;
#44945 = ORIENTED_EDGE ( 'NONE', *, *, #27244, .F. ) ;
#44946 = ORIENTED_EDGE ( 'NONE', *, *, #59084, .F. ) ;
#44947 = EDGE_CURVE ( 'NONE', #55886, #63655, #60047, .T. ) ;
#44948 = DIRECTION ( 'NONE',  ( 1.000000000000000000, 0.000000000000000000, 0.000000000000000000 ) ) ;
#44949 = CIRCLE ( 'NONE', #29148, 1.000000000000000000 ) ;
#44950 = CYLINDRICAL_SURFACE ( 'NONE', #42201, 0.6000000000000003109 ) ;
#44951 = DIRECTION ( 'NONE',  ( 0.000000000000000000, 0.000000000000000000, -1.000000000000000000 ) ) ;
#44952 = ORIENTED_EDGE ( 'NONE', *, *, #51097, .T. ) ;
#44953 = VERTEX_POINT ( 'NONE', #27531 ) ;
#44954 = EDGE_CURVE ( 'NONE', #66792, #13533, #21198, .T. ) ;
#44955 = AXIS2_PLACEMENT_3D ( 'NONE', #41304, #66772, #68179 ) ;
#44956 = LINE ( 'NONE', #50613, #48984 ) ;
#44957 = DIRECTION ( 'NONE',  ( 0.000000000000000000, 0.000000000000000000, 1.000000000000000000 ) ) ;
#44958 = ORIENTED_EDGE ( 'NONE', *, *, #68169, .F. ) ;
#44959 = EDGE_CURVE ( 'NONE', #6331, #34313, #50322, .T. ) ;
#44960 = VERTEX_POINT ( 'NONE', #54754 ) ;
#44961 = CARTESIAN_POINT ( 'NONE',  ( -5.242976262117280406, -5.257023737882805747, 54.00000000000000711 ) ) ;
#44962 = LINE ( 'NONE', #39647, #18081 ) ;
#44963 = VERTEX_POINT ( 'NONE', #42753 ) ;
#44964 = VECTOR ( 'NONE', #40467, 1000.000000000000000 ) ;
#44965 = DIRECTION ( 'NONE',  ( 0.000000000000000000, 0.000000000000000000, 1.000000000000000000 ) ) ;
#44967 = ORIENTED_EDGE ( 'NONE', *, *, #67466, .F. ) ;
#44966 = FACE_OUTER_BOUND ( 'NONE', #51000, .T. ) ;
#44968 = ORIENTED_EDGE ( 'NONE', *, *, #57423, .F. ) ;
#44969 = DIRECTION ( 'NONE',  ( 0.000000000000000000, 0.000000000000000000, 1.000000000000000000 ) ) ;
#44970 = CARTESIAN_POINT ( 'NONE',  ( 176.0064834503533575, 2.160375375128253950, 5.000000000000000000 ) ) ;
#44971 = CARTESIAN_POINT ( 'NONE',  ( 41.09999999999999432, -0.2000000000000000111, 0.000000000000000000 ) ) ;
#44972 = FACE_OUTER_BOUND ( 'NONE', #62198, .T. ) ;
#44973 = DIRECTION ( 'NONE',  ( -1.000000000000000000, 0.000000000000000000, 0.000000000000000000 ) ) ;
#44974 = FACE_OUTER_BOUND ( 'NONE', #40388, .T. ) ;
#44975 = FACE_OUTER_BOUND ( 'NONE', #6914, .T. ) ;
#44976 = EDGE_CURVE ( 'NONE', #50067, #39463, #48061, .T. ) ;
#44977 = ORIENTED_EDGE ( 'NONE', *, *, #42956, .T. ) ;
#44978 = CARTESIAN_POINT ( 'NONE',  ( 8.000000000000000000, 8.000000000000001776, -1.000000000000000000 ) ) ;
#44981 = ORIENTED_EDGE ( 'NONE', *, *, #8953, .T. ) ;
#44980 = EDGE_CURVE ( 'NONE', #67623, #16263, #318, .T. ) ;
#44979 = DIRECTION ( 'NONE',  ( 0.7071067811865475727, -0.7071067811865475727, 0.000000000000000000 ) ) ;
#44982 = CARTESIAN_POINT ( 'NONE',  ( 7.500000000000000000, -25.60000000000000142, -20.00000000000000000 ) ) ;
#44983 = CARTESIAN_POINT ( 'NONE',  ( 176.0064834503533575, 2.160375375128253950, 5.000000000000000000 ) ) ;
#44984 = CARTESIAN_POINT ( 'NONE',  ( 11.00000000000000000, -11.50000000000100009, -15.00000000000084910 ) ) ;
#44985 = CARTESIAN_POINT ( 'NONE',  ( 11.00000000000000000, -15.46862696659690073, 14.50000000000000000 ) ) ;
#44986 = CYLINDRICAL_SURFACE ( 'NONE', #43864, 2.000000000000001776 ) ;
#44987 = ORIENTED_EDGE ( 'NONE', *, *, #28175, .T. ) ;
#44988 = ORIENTED_EDGE ( 'NONE', *, *, #11194, .T. ) ;
#44989 = CARTESIAN_POINT ( 'NONE',  ( 25.50000000000000355, -5.578999999999999737, 22.50000000000000000 ) ) ;
#44990 = PRESENTATION_STYLE_ASSIGNMENT (( #28728 ) ) ;
#44991 = VECTOR ( 'NONE', #4167, 1000.000000000000000 ) ;
#44992 = CARTESIAN_POINT ( 'NONE',  ( 8.250000000000005329, 8.250000000000001776, -26.00000000000001066 ) ) ;
#44993 = ORIENTED_EDGE ( 'NONE', *, *, #60013, .F. ) ;
#44994 = LINE ( 'NONE', #1514, #33849 ) ;
#44995 = VERTEX_POINT ( 'NONE', #65706 ) ;
#44996 = ORIENTED_EDGE ( 'NONE', *, *, #59182, .T. ) ;
#44997 = AXIS2_PLACEMENT_3D ( 'NONE', #69859, #33068, #41672 ) ;
#44998 = PLANE ( 'NONE',  #67424 ) ;
#44999 = DIRECTION ( 'NONE',  ( 0.000000000000000000, 0.000000000000000000, 1.000000000000000000 ) ) ;
#45000 = ORIENTED_EDGE ( 'NONE', *, *, #63892, .T. ) ;
#45001 = CARTESIAN_POINT ( 'NONE',  ( 46.39999999999999858, 33.00000000000000000, -2.750000000000000444 ) ) ;
#45002 = CARTESIAN_POINT ( 'NONE',  ( -7.250000000000000888, 7.450000000000003730, -23.50000000000000000 ) ) ;
#45003 = DIRECTION ( 'NONE',  ( 0.000000000000000000, 1.000000000000000000, 0.000000000000000000 ) ) ;
#45004 = ORIENTED_EDGE ( 'NONE', *, *, #56442, .F. ) ;
#45006 = ORIENTED_EDGE ( 'NONE', *, *, #68521, .T. ) ;
#45005 = DIRECTION ( 'NONE',  ( -0.7071067811865348052, 0.7071067811865602293, 0.000000000000000000 ) ) ;
#45007 = AXIS2_PLACEMENT_3D ( 'NONE', #24483, #53371, #62643 ) ;
#45008 = ADVANCED_FACE ( 'NONE', ( #38824 ), #43094, .F. ) ;
#45009 = DIRECTION ( 'NONE',  ( 1.000000000000000000, 0.000000000000000000, 0.000000000000000000 ) ) ;
#45010 = LINE ( 'NONE', #62321, #33878 ) ;
#45011 = CARTESIAN_POINT ( 'NONE',  ( -7.415254214038336400, 3.593516549646602609, 195.0000000000000284 ) ) ;
#45012 = CARTESIAN_POINT ( 'NONE',  ( -11.00000000000000000, -5.599999999999999645, 9.000000000000001776 ) ) ;
#45013 = EDGE_CURVE ( 'NONE', #50, #35620, #4931, .T. ) ;
#45014 = CARTESIAN_POINT ( 'NONE',  ( -5.993516549646711766, 5.993516549646603409, 455.0000000000000568 ) ) ;
#45015 = FACE_OUTER_BOUND ( 'NONE', #39578, .T. ) ;
#45016 = EDGE_CURVE ( 'NONE', #29071, #25480, #10927, .T. ) ;
#45017 = EDGE_LOOP ( 'NONE', ( #8205, #24969, #25625, #253 ) ) ;
#45018 = ORIENTED_EDGE ( 'NONE', *, *, #38398, .F. ) ;
#45019 = EDGE_CURVE ( 'NONE', #10292, #69139, #54072, .T. ) ;
#45020 = ORIENTED_EDGE ( 'NONE', *, *, #54846, .T. ) ;
#45021 = LINE ( 'NONE', #39715, #37871 ) ;
#45022 = EDGE_CURVE ( 'NONE', #52921, #47907, #21878, .T. ) ;
#45023 = ADVANCED_FACE ( 'NONE', ( #38160 ), #43796, .T. ) ;
#45024 = CARTESIAN_POINT ( 'NONE',  ( 25.57999999999999829, 0.000000000000000000, 0.000000000000000000 ) ) ;
#45025 = CARTESIAN_POINT ( 'NONE',  ( 48.50000000000000000, 0.7500000000000000000, 3.418698582794335028 ) ) ;
#45026 =( LENGTH_UNIT ( ) NAMED_UNIT ( * ) SI_UNIT ( .MILLI., .METRE. ) );
#45027 = EDGE_CURVE ( 'NONE', #51768, #23407, #65371, .T. ) ;
#45028 = ORIENTED_EDGE ( 'NONE', *, *, #13739, .F. ) ;
#45029 = ORIENTED_EDGE ( 'NONE', *, *, #40522, .T. ) ;
#45030 = ORIENTED_EDGE ( 'NONE', *, *, #58554, .F. ) ;
#45031 = FACE_OUTER_BOUND ( 'NONE', #6367, .T. ) ;
#45032 = ORIENTED_EDGE ( 'NONE', *, *, #59154, .F. ) ;
#45033 = VERTEX_POINT ( 'NONE', #11596 ) ;
#45034 = VERTEX_POINT ( 'NONE', #33179 ) ;
#45035 = AXIS2_PLACEMENT_3D ( 'NONE', #22441, #21394, #48967 ) ;
#45036 = VERTEX_POINT ( 'NONE', #2729 ) ;
#45037 = PLANE ( 'NONE',  #28256 ) ;
#45039 = ORIENTED_EDGE ( 'NONE', *, *, #11008, .T. ) ;
#45038 = DIRECTION ( 'NONE',  ( 0.000000000000000000, 1.000000000000000000, 1.500535806722250850E-12 ) ) ;
#45040 = AXIS2_PLACEMENT_3D ( 'NONE', #61526, #2491, #62580 ) ;
#45041 = DIRECTION ( 'NONE',  ( 0.000000000000000000, 0.000000000000000000, -1.000000000000000000 ) ) ;
#45042 = FACE_BOUND ( 'NONE', #41820, .T. ) ;
#45043 = DIRECTION ( 'NONE',  ( 1.836970198721029934E-16, -1.836970198721036344E-16, 1.000000000000000000 ) ) ;
#45045 = ORIENTED_EDGE ( 'NONE', *, *, #39226, .F. ) ;
#45044 = DIRECTION ( 'NONE',  ( 1.000000000000000000, -0.000000000000000000, 0.000000000000000000 ) ) ;
#45046 = ORIENTED_EDGE ( 'NONE', *, *, #11263, .T. ) ;
#45047 = VECTOR ( 'NONE', #12785, 1000.000000000000000 ) ;
#45048 = LINE ( 'NONE', #56715, #15939 ) ;
#45049 = CARTESIAN_POINT ( 'NONE',  ( 0.000000000000000000, -7.449999999999998401, -18.00000000000000000 ) ) ;
#45050 = AXIS2_PLACEMENT_3D ( 'NONE', #67754, #14719, #25693 ) ;
#45051 = DIRECTION ( 'NONE',  ( 0.8660254037844482555, 0.000000000000000000, -0.4999999999999831801 ) ) ;
#45052 = EDGE_LOOP ( 'NONE', ( #17799, #35575, #24692, #28980 ) ) ;
#45053 = DIRECTION ( 'NONE',  ( -0.000000000000000000, 3.673940397442059868E-16, -1.000000000000000000 ) ) ;
#45055 = VECTOR ( 'NONE', #21499, 1000.000000000000000 ) ;
#45054 = AXIS2_PLACEMENT_3D ( 'NONE', #47615, #9433, #58584 ) ;
#45056 = ADVANCED_FACE ( 'NONE', ( #45159 ), #23949, .F. ) ;
#45057 = DIRECTION ( 'NONE',  ( -0.8660254037844375974, 0.5000000000000019984, 1.836970198721037330E-16 ) ) ;
#45058 = CARTESIAN_POINT ( 'NONE',  ( 275.0000000000000000, -32.94999999999885176, 8.199999999997979572 ) ) ;
#45059 = ORIENTED_EDGE ( 'NONE', *, *, #15841, .F. ) ;
#45060 = ADVANCED_FACE ( 'NONE', ( #56138 ), #44815, .T. ) ;
#45061 = FACE_OUTER_BOUND ( 'NONE', #28391, .T. ) ;
#45062 = EDGE_CURVE ( 'NONE', #58819, #65043, #4059, .T. ) ;
#45063 = AXIS2_PLACEMENT_3D ( 'NONE', #43860, #53794, #65436 ) ;
#45064 = DIRECTION ( 'NONE',  ( -1.000000000000000000, 0.000000000000000000, 0.000000000000000000 ) ) ;
#45065 = DIRECTION ( 'NONE',  ( 0.000000000000000000, 0.000000000000000000, 1.000000000000000000 ) ) ;
#45066 = EDGE_CURVE ( 'NONE', #30786, #9070, #28554, .T. ) ;
#45067 = ORIENTED_EDGE ( 'NONE', *, *, #39307, .F. ) ;
#45068 = DIRECTION ( 'NONE',  ( 0.000000000000000000, 0.000000000000000000, 1.000000000000000000 ) ) ;
#45069 = CARTESIAN_POINT ( 'NONE',  ( 11.32648345035340398, 7.593516549646563085, 455.0000000000000568 ) ) ;
#45070 = DIRECTION ( 'NONE',  ( -0.000000000000000000, -0.000000000000000000, -1.000000000000000000 ) ) ;
#45071 = ORIENTED_EDGE ( 'NONE', *, *, #42170, .F. ) ;
#45072 = VECTOR ( 'NONE', #30442, 1000.000000000000000 ) ;
#45073 = CYLINDRICAL_SURFACE ( 'NONE', #12336, 24.99999999998784972 ) ;
#45074 = CARTESIAN_POINT ( 'NONE',  ( -7.250000000000000000, -7.449999999999998401, -13.50000000000000178 ) ) ;
#45075 = DIRECTION ( 'NONE',  ( 9.912705577010312730E-15, 1.000000000000000000, 0.000000000000000000 ) ) ;
#45076 = DIRECTION ( 'NONE',  ( -0.000000000000000000, -0.000000000000000000, 1.000000000000000000 ) ) ;
#45077 = FACE_OUTER_BOUND ( 'NONE', #47224, .T. ) ;
#45078 = ORIENTED_EDGE ( 'NONE', *, *, #20985, .F. ) ;
#45079 = CARTESIAN_POINT ( 'NONE',  ( -8.000000000000000000, -8.000000000000000000, -1.000000000000000000 ) ) ;
#45080 = CARTESIAN_POINT ( 'NONE',  ( 8.406483450353379183, -4.396432944014657451, 455.0000000000000568 ) ) ;
#45081 = FACE_OUTER_BOUND ( 'NONE', #15125, .T. ) ;
#45082 = CIRCLE ( 'NONE', #28140, 0.2000000000000005107 ) ;
#45083 = CARTESIAN_POINT ( 'NONE',  ( 283.0000000000000568, -31.30000000000000071, -12.69999999999999929 ) ) ;
#45084 = LINE ( 'NONE', #34825, #33944 ) ;
#45085 = ORIENTED_EDGE ( 'NONE', *, *, #33948, .T. ) ;
#45086 = VECTOR ( 'NONE', #17528, 1000.000000000000000 ) ;
#45088 = ORIENTED_EDGE ( 'NONE', *, *, #54796, .T. ) ;
#45087 = DIRECTION ( 'NONE',  ( 0.000000000000000000, 0.000000000000000000, -1.000000000000000000 ) ) ;
#45089 = AXIS2_PLACEMENT_3D ( 'NONE', #51284, #24420, #67560 ) ;
#45090 = ADVANCED_FACE ( 'NONE', ( #6650 ), #50480, .T. ) ;
#45091 = DIRECTION ( 'NONE',  ( 0.000000000000000000, -3.673940397442059868E-16, 1.000000000000000000 ) ) ;
#45092 = DIRECTION ( 'NONE',  ( -0.000000000000000000, -0.000000000000000000, 1.000000000000000000 ) ) ;
#45093 = ORIENTED_EDGE ( 'NONE', *, *, #39271, .T. ) ;
#45094 = AXIS2_PLACEMENT_3D ( 'NONE', #29319, #35675, #67865 ) ;
#45095 = DIRECTION ( 'NONE',  ( -8.673617379884013384E-15, -1.000000000000000000, 0.000000000000000000 ) ) ;
#45096 = ORIENTED_EDGE ( 'NONE', *, *, #64441, .F. ) ;
#45097 = CIRCLE ( 'NONE', #20288, 0.2000000000000005107 ) ;
#45098 = PLANE ( 'NONE',  #54932 ) ;
#45099 = ORIENTED_EDGE ( 'NONE', *, *, #56919, .T. ) ;
#45100 = ORIENTED_EDGE ( 'NONE', *, *, #14568, .F. ) ;
#45101 = DIRECTION ( 'NONE',  ( -1.000000000000000000, 0.000000000000000000, 0.000000000000000000 ) ) ;
#45102 = ADVANCED_FACE ( 'NONE', ( #7328 ), #12280, .F. ) ;
#45103 = ADVANCED_FACE ( 'NONE', ( #66731, #61786 ), #66396, .F. ) ;
#45104 = DIRECTION ( 'NONE',  ( 1.000000000000000000, -0.000000000000000000, 0.000000000000000000 ) ) ;
#45105 = CIRCLE ( 'NONE', #16865, 0.3000000000005387246 ) ;
#45106 = CARTESIAN_POINT ( 'NONE',  ( -8.593516549646711411, 4.383466043307770121, 455.0000000000000568 ) ) ;
#45107 = CARTESIAN_POINT ( 'NONE',  ( -15.50000000000000000, -5.000000000000000000, 22.50000000000000000 ) ) ;
#45108 = EDGE_CURVE ( 'NONE', #50347, #68595, #55783, .T. ) ;
#45109 = VERTEX_POINT ( 'NONE', #1683 ) ;
#45110 = ORIENTED_EDGE ( 'NONE', *, *, #57868, .T. ) ;
#45111 = LINE ( 'NONE', #18240, #51583 ) ;
#45112 = CARTESIAN_POINT ( 'NONE',  ( 9.899999999999998579, -14.06939075806900874, 20.80000000000001137 ) ) ;
#45113 = ORIENTED_EDGE ( 'NONE', *, *, #21945, .F. ) ;
#45114 = EDGE_LOOP ( 'NONE', ( #1437, #60231, #31739, #34940, #65531, #29184, #46499, #66362 ) ) ;
#45115 = VERTEX_POINT ( 'NONE', #55106 ) ;
#45116 = CARTESIAN_POINT ( 'NONE',  ( 9.562023737882766383, 2.530476262117153485, 54.00000000000000711 ) ) ;
#45118 = ORIENTED_EDGE ( 'NONE', *, *, #54549, .F. ) ;
#45117 = CARTESIAN_POINT ( 'NONE',  ( 7.450000000000003730, -7.249999999999997335, -10.50000000000000000 ) ) ;
#45119 = DIRECTION ( 'NONE',  ( 0.000000000000000000, 0.000000000000000000, 1.000000000000000000 ) ) ;
#45120 = CARTESIAN_POINT ( 'NONE',  ( 289.5000000000000000, -42.50000000000000000, -26.50000000000000000 ) ) ;
#45121 = AXIS2_PLACEMENT_3D ( 'NONE', #69145, #5843, #43314 ) ;
#45122 = VERTEX_POINT ( 'NONE', #28903 ) ;
#45123 = VERTEX_POINT ( 'NONE', #40560 ) ;
#45124 = CARTESIAN_POINT ( 'NONE',  ( 69.92576880110368620, 10.00000000000000000, 281.4830310981151911 ) ) ;
#45125 = CARTESIAN_POINT ( 'NONE',  ( 14.25000000000000000, -2.500000000000000000, -23.22168783648699986 ) ) ;
#45126 = DIRECTION ( 'NONE',  ( 0.000000000000000000, 0.000000000000000000, -1.000000000000000000 ) ) ;
#45127 = VECTOR ( 'NONE', #6517, 1000.000000000000000 ) ;
#45128 = VECTOR ( 'NONE', #20770, 1000.000000000000114 ) ;
#45129 = VECTOR ( 'NONE', #11258, 1000.000000000000000 ) ;
#45130 = CARTESIAN_POINT ( 'NONE',  ( -3.142976262117267883, -4.046023737882828542, 54.00000000000000711 ) ) ;
#45131 = LINE ( 'NONE', #1326, #21147 ) ;
#45133 = ORIENTED_EDGE ( 'NONE', *, *, #23994, .F. ) ;
#45132 = DIRECTION ( 'NONE',  ( 0.000000000000000000, -1.000000000000000000, 0.000000000000000000 ) ) ;
#45134 = ORIENTED_EDGE ( 'NONE', *, *, #65408, .F. ) ;
#45135 = EDGE_CURVE ( 'NONE', #64234, #5555, #40218, .T. ) ;
#45136 = CARTESIAN_POINT ( 'NONE',  ( 280.0000000000000000, -25.60000000000000142, -16.00000000000000711 ) ) ;
#45137 = CIRCLE ( 'NONE', #44039, 0.5000000000009302559 ) ;
#45138 = ADVANCED_FACE ( 'NONE', ( #39848 ), #66036, .T. ) ;
#45139 = EDGE_CURVE ( 'NONE', #14789, #19943, #17944, .T. ) ;
#45140 = DIRECTION ( 'NONE',  ( 0.000000000000000000, -0.1499999999999998002, -0.9886859966642594921 ) ) ;
#45141 = CARTESIAN_POINT ( 'NONE',  ( 10.31452373788281562, -3.857023737882824932, 54.00000000000000711 ) ) ;
#45142 = EDGE_CURVE ( 'NONE', #41898, #37433, #34894, .T. ) ;
#45143 = VECTOR ( 'NONE', #38248, 999.9999999999998863 ) ;
#45144 = CARTESIAN_POINT ( 'NONE',  ( 15.00000000000000000, -21.00000000000000000, 5.000000000000000000 ) ) ;
#45145 = ORIENTED_EDGE ( 'NONE', *, *, #53912, .F. ) ;
#45146 = CARTESIAN_POINT ( 'NONE',  ( -4.141586236041100655, 4.706725378239165813, 26.00000000000000711 ) ) ;
#45147 = CARTESIAN_POINT ( 'NONE',  ( 0.000000000000000000, 0.000000000000000000, -15.50000000000000000 ) ) ;
#45148 = PRESENTATION_STYLE_ASSIGNMENT (( #1008 ) ) ;
#45149 = AXIS2_PLACEMENT_3D ( 'NONE', #13869, #15284, #62652 ) ;
#45150 = CARTESIAN_POINT ( 'NONE',  ( -9.690000000000001279, 8.750000000000000000, -7.000000000000000000 ) ) ;
#45151 = DIRECTION ( 'NONE',  ( 1.000000000000000000, 0.000000000000000000, 0.000000000000000000 ) ) ;
#45152 = DIRECTION ( 'NONE',  ( 0.000000000000000000, -1.000000000000000000, 0.000000000000000000 ) ) ;
#45153 = VECTOR ( 'NONE', #8975, 1000.000000000000000 ) ;
#45154 = FACE_OUTER_BOUND ( 'NONE', #32282, .T. ) ;
#45155 = ORIENTED_EDGE ( 'NONE', *, *, #48918, .F. ) ;
#45156 = CYLINDRICAL_SURFACE ( 'NONE', #1590, 0.2999999999998732569 ) ;
#45157 = DIRECTION ( 'NONE',  ( 0.000000000000000000, -1.000000000000000000, 0.000000000000000000 ) ) ;
#45158 = ORIENTED_EDGE ( 'NONE', *, *, #48517, .T. ) ;
#45159 = FACE_OUTER_BOUND ( 'NONE', #29550, .T. ) ;
#45160 = CARTESIAN_POINT ( 'NONE',  ( -9.722976262117258628, 3.667976262117184749, 26.00000000000000711 ) ) ;
#45161 = DIRECTION ( 'NONE',  ( 0.000000000000000000, 1.000000000000000000, 0.000000000000000000 ) ) ;
#45162 = CARTESIAN_POINT ( 'NONE',  ( 8.689999999999999503, -8.750000000000000000, -5.000000000000000000 ) ) ;
#45163 = LINE ( 'NONE', #2390, #10195 ) ;
#45164 = ORIENTED_EDGE ( 'NONE', *, *, #11965, .T. ) ;
#45165 = CARTESIAN_POINT ( 'NONE',  ( 15.89999999999999680, -0.1999999999911430404, -8.864436962241481021E-12 ) ) ;
#45166 = VERTEX_POINT ( 'NONE', #61071 ) ;
#45167 = VECTOR ( 'NONE', #9671, 1000.000000000000114 ) ;
#45168 = DIRECTION ( 'NONE',  ( -0.7071067811865464625, 0.7071067811865486830, 0.000000000000000000 ) ) ;
#45169 = ORIENTED_EDGE ( 'NONE', *, *, #38830, .T. ) ;
#45170 = DIRECTION ( 'NONE',  ( 4.745709458399858621E-16, 1.000000000000000000, 1.836970198721035604E-16 ) ) ;
#45171 = FILL_AREA_STYLE_COLOUR ( '', #559 ) ;
#45172 = CARTESIAN_POINT ( 'NONE',  ( 7.806483450353418618, 11.11351654964657421, 455.0000000000000568 ) ) ;
#45173 = ORIENTED_EDGE ( 'NONE', *, *, #53616, .F. ) ;
#45174 = ORIENTED_EDGE ( 'NONE', *, *, #2176, .F. ) ;
#45175 = DIRECTION ( 'NONE',  ( 0.000000000000000000, -9.159339953149780582E-13, 1.000000000000000000 ) ) ;
#45176 = VECTOR ( 'NONE', #52372, 1000.000000000000000 ) ;
#45177 = EDGE_LOOP ( 'NONE', ( #30282, #2517, #23018, #44260 ) ) ;
#45178 = VERTEX_POINT ( 'NONE', #1351 ) ;
#45179 = EDGE_CURVE ( 'NONE', #62585, #58374, #49787, .T. ) ;
#45180 = CARTESIAN_POINT ( 'NONE',  ( -10.19191654964680360, -9.804883450353337082, 195.0000000000000284 ) ) ;
#45181 = DIRECTION ( 'NONE',  ( -0.8660254037844510311, -0.4999999999999785727, 0.000000000000000000 ) ) ;
#45183 = DIRECTION ( 'NONE',  ( -1.000000000000000000, 0.000000000000000000, 0.000000000000000000 ) ) ;
#45182 = VECTOR ( 'NONE', #44379, 1000.000000000000114 ) ;
#45184 = EDGE_CURVE ( 'NONE', #61271, #47033, #67083, .T. ) ;
#45185 = EDGE_CURVE ( 'NONE', #28299, #54080, #8023, .T. ) ;
#45186 = ORIENTED_EDGE ( 'NONE', *, *, #18686, .F. ) ;
#45187 = AXIS2_PLACEMENT_3D ( 'NONE', #65609, #17164, #38728 ) ;
#45188 = CARTESIAN_POINT ( 'NONE',  ( 75.42576880091934299, 10.00000000000000000, 334.4830310981790831 ) ) ;
#45190 = CARTESIAN_POINT ( 'NONE',  ( 4.186483450353335023, -12.00648345035347830, 455.0000000000000568 ) ) ;
#45189 = DIRECTION ( 'NONE',  ( 0.000000000000000000, 0.000000000000000000, 1.000000000000000000 ) ) ;
#45191 = EDGE_LOOP ( 'NONE', ( #62403, #65037, #26633, #65440 ) ) ;
#45194 = ORIENTED_EDGE ( 'NONE', *, *, #42402, .F. ) ;
#45193 = EDGE_CURVE ( 'NONE', #42184, #56927, #21064, .T. ) ;
#45192 = PLANE ( 'NONE',  #36477 ) ;
#45195 = ORIENTED_EDGE ( 'NONE', *, *, #16790, .F. ) ;
#45196 = VECTOR ( 'NONE', #66735, 999.9999999999998863 ) ;
#45197 = DIRECTION ( 'NONE',  ( 0.000000000000000000, 0.000000000000000000, 1.000000000000000000 ) ) ;
#45198 = EDGE_CURVE ( 'NONE', #8330, #8968, #63184, .T. ) ;
#45199 = EDGE_CURVE ( 'NONE', #10277, #7833, #19683, .T. ) ;
#45201 = VECTOR ( 'NONE', #11404, 1000.000000000000000 ) ;
#45200 = FACE_OUTER_BOUND ( 'NONE', #21286, .T. ) ;
#45202 = EDGE_CURVE ( 'NONE', #59591, #7598, #46559, .T. ) ;
#45203 = ORIENTED_EDGE ( 'NONE', *, *, #67542, .F. ) ;
#45204 = FACE_OUTER_BOUND ( 'NONE', #46167, .T. ) ;
#45205 = PLANE ( 'NONE',  #37337 ) ;
#45206 = ORIENTED_EDGE ( 'NONE', *, *, #32565, .T. ) ;
#45207 = ORIENTED_EDGE ( 'NONE', *, *, #32605, .F. ) ;
#45208 = VECTOR ( 'NONE', #25873, 1000.000000000000000 ) ;
#45209 = VECTOR ( 'NONE', #65905, 1000.000000000000000 ) ;
#45210 = DIRECTION ( 'NONE',  ( 1.000000000000000000, -0.000000000000000000, -0.000000000000000000 ) ) ;
#45211 = CARTESIAN_POINT ( 'NONE',  ( 14.50000000000000000, -0.4999999999999923950, -27.00000000000000711 ) ) ;
#45212 = ORIENTED_EDGE ( 'NONE', *, *, #50221, .F. ) ;
#45213 = DIRECTION ( 'NONE',  ( 0.000000000000000000, 1.000000000000000000, -0.000000000000000000 ) ) ;
#45214 = DIRECTION ( 'NONE',  ( 0.000000000000000000, 0.000000000000000000, 1.000000000000000000 ) ) ;
#45215 = CARTESIAN_POINT ( 'NONE',  ( 9.737023737882816832, -6.832023737882823688, 54.00000000000000711 ) ) ;
#45216 = ORIENTED_EDGE ( 'NONE', *, *, #35709, .F. ) ;
#45217 = CARTESIAN_POINT ( 'NONE',  ( 11.50000000000000000, -12.00000000000000000, 11.00000000000000000 ) ) ;
#45218 = VECTOR ( 'NONE', #19728, 1000.000000000000000 ) ;
#45219 = DIRECTION ( 'NONE',  ( -1.000000000000000000, 0.000000000000000000, 0.000000000000000000 ) ) ;
#45221 = EDGE_LOOP ( 'NONE', ( #14446, #30600, #41882, #16398, #30219, #7045, #14693, #11071 ) ) ;
#45220 = FACE_OUTER_BOUND ( 'NONE', #20809, .T. ) ;
#45223 = ORIENTED_EDGE ( 'NONE', *, *, #48818, .F. ) ;
#45222 = CARTESIAN_POINT ( 'NONE',  ( 39.00000000000000000, 0.000000000000000000, 0.000000000000000000 ) ) ;
#45224 = CARTESIAN_POINT ( 'NONE',  ( 49.00000000000000000, -0.2000000000089119934, -8.913009219568841313E-12 ) ) ;
#45225 = LINE ( 'NONE', #66795, #17181 ) ;
#45226 = PLANE ( 'NONE',  #34667 ) ;
#45227 = CARTESIAN_POINT ( 'NONE',  ( 283.0000000000000568, -26.06128899128900045, -10.14003097807800025 ) ) ;
#45228 = DIRECTION ( 'NONE',  ( 0.000000000000000000, 0.000000000000000000, -1.000000000000000000 ) ) ;
#45229 = ORIENTED_EDGE ( 'NONE', *, *, #11274, .T. ) ;
#45230 = CARTESIAN_POINT ( 'NONE',  ( -15.50000000000000000, -5.000000000000000000, -22.50000000000000000 ) ) ;
#45231 = CARTESIAN_POINT ( 'NONE',  ( 5.257023737882795977, 5.242976262117205799, 26.00000000000000711 ) ) ;
#45232 = CIRCLE ( 'NONE', #41871, 1.399999999999999245 ) ;
#45233 = CARTESIAN_POINT ( 'NONE',  ( -7.250000000000000000, -7.449999999999998401, -16.50000000000000000 ) ) ;
#45235 = ORIENTED_EDGE ( 'NONE', *, *, #19159, .T. ) ;
#45234 = DIRECTION ( 'NONE',  ( 0.000000000000000000, 0.000000000000000000, -1.000000000000000000 ) ) ;
#45236 = AXIS2_PLACEMENT_3D ( 'NONE', #47763, #69331, #15249 ) ;
#45237 = DIRECTION ( 'NONE',  ( -0.000000000000000000, 1.000000000000000000, -0.000000000000000000 ) ) ;
#45238 = CARTESIAN_POINT ( 'NONE',  ( 8.465062094116099445, 7.744988412222715723, 455.0000000000000568 ) ) ;
#45239 = CIRCLE ( 'NONE', #55459, 0.1749999999999998224 ) ;
#45240 = EDGE_CURVE ( 'NONE', #37106, #52181, #47276, .T. ) ;
#45241 = ORIENTED_EDGE ( 'NONE', *, *, #59327, .T. ) ;
#45242 = CARTESIAN_POINT ( 'NONE',  ( -2.989207322240233555, -6.872275254348434892, 54.00000000000000711 ) ) ;
#45243 = CARTESIAN_POINT ( 'NONE',  ( 7.408280051175138325, 3.710438382363051790, 54.00000000000000711 ) ) ;
#45244 = ORIENTED_EDGE ( 'NONE', *, *, #62391, .T. ) ;
#45245 = AXIS2_PLACEMENT_3D ( 'NONE', #35892, #25278, #63464 ) ;
#45246 = VECTOR ( 'NONE', #31032, 1000.000000000000000 ) ;
#45247 = DIRECTION ( 'NONE',  ( -1.000000000000000000, 0.000000000000000000, 0.000000000000000000 ) ) ;
#45248 = DIRECTION ( 'NONE',  ( 0.000000000000000000, 0.000000000000000000, 1.000000000000000000 ) ) ;
#45249 = FACE_BOUND ( 'NONE', #63740, .T. ) ;
#45250 = ADVANCED_FACE ( 'NONE', ( #25723 ), #62837, .F. ) ;
#45251 = DIRECTION ( 'NONE',  ( -1.000000000000000000, 0.000000000000000000, 0.000000000000000000 ) ) ;
#45252 = AXIS2_PLACEMENT_3D ( 'NONE', #51361, #29100, #45005 ) ;
#45253 = FACE_OUTER_BOUND ( 'NONE', #23135, .T. ) ;
#45254 = ORIENTED_EDGE ( 'NONE', *, *, #14559, .T. ) ;
#45255 = PLANE ( 'NONE',  #12282 ) ;
#45256 = VERTEX_POINT ( 'NONE', #67788 ) ;
#45257 = EDGE_CURVE ( 'NONE', #65777, #67217, #4154, .T. ) ;
#45258 = ORIENTED_EDGE ( 'NONE', *, *, #44317, .F. ) ;
#45259 = CARTESIAN_POINT ( 'NONE',  ( 6.501044194225450212, 3.142976262117187058, 54.00000000000000711 ) ) ;
#45260 = AXIS2_PLACEMENT_3D ( 'NONE', #15868, #46992, #37437 ) ;
#45261 = EDGE_CURVE ( 'NONE', #39983, #65543, #13691, .T. ) ;
#45262 = DIRECTION ( 'NONE',  ( 0.000000000000000000, 1.000000000000000000, 0.000000000000000000 ) ) ;
#45264 = DIRECTION ( 'NONE',  ( 0.5000000000000111022, 0.8660254037844322683, 2.509347957447867944E-16 ) ) ;
#45263 = DIRECTION ( 'NONE',  ( 1.000000000000000000, -5.981805089575194965E-17, 0.000000000000000000 ) ) ;
#45265 = ORIENTED_EDGE ( 'NONE', *, *, #2596, .T. ) ;
#45266 = ORIENTED_EDGE ( 'NONE', *, *, #30598, .F. ) ;
#45267 = CYLINDRICAL_SURFACE ( 'NONE', #40824, 0.3500000000002719824 ) ;
#45268 = ORIENTED_EDGE ( 'NONE', *, *, #12454, .T. ) ;
#45269 = PLANE ( 'NONE',  #30369 ) ;
#45270 = LINE ( 'NONE', #2841, #7204 ) ;
#45271 = EDGE_CURVE ( 'NONE', #25515, #48269, #9093, .T. ) ;
#45272 = LINE ( 'NONE', #50595, #42138 ) ;
#45273 = FACE_OUTER_BOUND ( 'NONE', #44335, .T. ) ;
#45275 = DIRECTION ( 'NONE',  ( 1.836970198721029934E-16, 1.836970198721010706E-16, -1.000000000000000000 ) ) ;
#45274 = CARTESIAN_POINT ( 'NONE',  ( -7.250000000000001776, -7.249999999999998224, -24.00000000000000000 ) ) ;
#45276 = ORIENTED_EDGE ( 'NONE', *, *, #51806, .T. ) ;
#45278 = EDGE_LOOP ( 'NONE', ( #29130, #10812, #19179, #18039 ) ) ;
#45277 = CARTESIAN_POINT ( 'NONE',  ( -7.250000000000000888, -8.249999999999998224, -26.00000000000001066 ) ) ;
#45279 = ORIENTED_EDGE ( 'NONE', *, *, #3754, .T. ) ;
#45280 = ORIENTED_EDGE ( 'NONE', *, *, #49480, .T. ) ;
#45281 = EDGE_CURVE ( 'NONE', #38702, #7725, #52225, .T. ) ;
#45282 = DIRECTION ( 'NONE',  ( -1.000000000000000000, 0.000000000000000000, 0.000000000000000000 ) ) ;
#45283 = CIRCLE ( 'NONE', #34027, 2.204799999999999205 ) ;
#45284 = EDGE_CURVE ( 'NONE', #37597, #52878, #43623, .T. ) ;
#45285 = CYLINDRICAL_SURFACE ( 'NONE', #56387, 0.2000000000000005107 ) ;
#45286 = VECTOR ( 'NONE', #59850, 1000.000000000000000 ) ;
#45287 = ORIENTED_EDGE ( 'NONE', *, *, #54110, .F. ) ;
#45288 = ORIENTED_EDGE ( 'NONE', *, *, #24599, .F. ) ;
#45289 = VECTOR ( 'NONE', #5286, 1000.000000000000000 ) ;
#45290 = LINE ( 'NONE', #44595, #18458 ) ;
#45291 = CARTESIAN_POINT ( 'NONE',  ( 7.250000000000005329, -7.249999999999998224, -12.50000000000000000 ) ) ;
#45292 = ADVANCED_FACE ( 'NONE', ( #35238 ), #41968, .T. ) ;
#45293 = ORIENTED_EDGE ( 'NONE', *, *, #33032, .F. ) ;
#45294 = AXIS2_PLACEMENT_3D ( 'NONE', #6150, #59556, #65882 ) ;
#45295 = AXIS2_PLACEMENT_3D ( 'NONE', #33467, #55052, #1290 ) ;
#45296 = ORIENTED_EDGE ( 'NONE', *, *, #17340, .T. ) ;
#45297 = DIRECTION ( 'NONE',  ( 0.000000000000000000, 0.000000000000000000, -1.000000000000000000 ) ) ;
#45298 = DIRECTION ( 'NONE',  ( 0.000000000000000000, 0.000000000000000000, -1.000000000000000000 ) ) ;
#45299 = ORIENTED_EDGE ( 'NONE', *, *, #68876, .F. ) ;
#45300 = CARTESIAN_POINT ( 'NONE',  ( 3.677663764522608680, 6.350872789121272177, 54.00000000000000711 ) ) ;
#45301 = LINE ( 'NONE', #66871, #67820 ) ;
#45303 = ORIENTED_EDGE ( 'NONE', *, *, #10920, .T. ) ;
#45302 = SURFACE_STYLE_FILL_AREA ( #61925 ) ;
#45304 = VERTEX_POINT ( 'NONE', #68140 ) ;
#45306 = CARTESIAN_POINT ( 'NONE',  ( -7.450000000000001954, -7.249999999999998224, -19.50000000000000000 ) ) ;
#45305 = CIRCLE ( 'NONE', #14857, 0.9999999999999991118 ) ;
#45307 = LINE ( 'NONE', #34006, #25599 ) ;
#45308 = CARTESIAN_POINT ( 'NONE',  ( 9.737023737882815055, -2.544523737882825820, 54.00000000000000711 ) ) ;
#45309 = LINE ( 'NONE', #50631, #31281 ) ;
#45310 = LINE ( 'NONE', #39328, #57176 ) ;
#45311 = EDGE_CURVE ( 'NONE', #51641, #16435, #63547, .T. ) ;
#45312 = CARTESIAN_POINT ( 'NONE',  ( -7.250000000000000888, -8.249999999999998224, -24.00000000000000000 ) ) ;
#45313 = DIRECTION ( 'NONE',  ( 1.000000000000000000, 0.000000000000000000, 0.000000000000000000 ) ) ;
#45314 = ORIENTED_EDGE ( 'NONE', *, *, #2316, .F. ) ;
#45315 = LINE ( 'NONE', #6797, #45047 ) ;
#45316 = EDGE_CURVE ( 'NONE', #52106, #65495, #27826, .T. ) ;
#45318 = ORIENTED_EDGE ( 'NONE', *, *, #22469, .T. ) ;
#45317 = FACE_OUTER_BOUND ( 'NONE', #50638, .T. ) ;
#45319 = DIRECTION ( 'NONE',  ( -0.000000000000000000, -0.000000000000000000, 1.000000000000000000 ) ) ;
#45320 = PLANE ( 'NONE',  #31243 ) ;
#45321 = AXIS2_PLACEMENT_3D ( 'NONE', #46874, #3748, #25320 ) ;
#45323 = ADVANCED_FACE ( 'NONE', ( #51533 ), #14407, .F. ) ;
#45322 = FACE_OUTER_BOUND ( 'NONE', #5397, .T. ) ;
#45324 = LINE ( 'NONE', #23073, #29519 ) ;
#45325 = DIRECTION ( 'NONE',  ( -0.000000000000000000, -1.000000000000000000, -0.000000000000000000 ) ) ;
#45326 = EDGE_CURVE ( 'NONE', #9530, #48443, #23268, .T. ) ;
#45327 = ORIENTED_EDGE ( 'NONE', *, *, #69540, .T. ) ;
#45328 = EDGE_LOOP ( 'NONE', ( #41388, #37229, #13778, #2878, #19169, #43275, #52996, #40110 ) ) ;
#45329 = LINE ( 'NONE', #35422, #7631 ) ;
#45330 = EDGE_CURVE ( 'NONE', #48598, #11140, #58325, .T. ) ;
#45331 = AXIS2_PLACEMENT_3D ( 'NONE', #54135, #5695, #48830 ) ;
#45332 = CYLINDRICAL_SURFACE ( 'NONE', #1766, 2.215251240775983899 ) ;
#45333 = DIRECTION ( 'NONE',  ( -9.799566706031580591E-15, -1.000000000000000000, 0.000000000000000000 ) ) ;
#45334 = ORIENTED_EDGE ( 'NONE', *, *, #46099, .F. ) ;
#45335 = CARTESIAN_POINT ( 'NONE',  ( 5.257023737882798642, 6.467976262117199227, 54.00000000000000711 ) ) ;
#45336 = ORIENTED_EDGE ( 'NONE', *, *, #64367, .F. ) ;
#45337 = EDGE_CURVE ( 'NONE', #62137, #39966, #19894, .T. ) ;
#45338 = ORIENTED_EDGE ( 'NONE', *, *, #12211, .T. ) ;
#45339 = EDGE_CURVE ( 'NONE', #29653, #32973, #2615, .T. ) ;
#45340 = DIRECTION ( 'NONE',  ( 0.000000000000000000, -1.000000000000000000, 0.000000000000000000 ) ) ;
#45341 = DIRECTION ( 'NONE',  ( 1.836970198721029934E-16, 1.836970198721010706E-16, -1.000000000000000000 ) ) ;
#45342 = ORIENTED_EDGE ( 'NONE', *, *, #60966, .F. ) ;
#45343 = DIRECTION ( 'NONE',  ( 1.000000000000000000, 0.000000000000000000, 0.000000000000000000 ) ) ;
#45345 = EDGE_CURVE ( 'NONE', #51749, #32671, #1568, .T. ) ;
#45344 = CIRCLE ( 'NONE', #11443, 24.99999999998789946 ) ;
#45346 = ADVANCED_FACE ( 'NONE', ( #60957 ), #40801, .T. ) ;
#45347 = CLOSED_SHELL ( 'NONE', ( #37571, #56585, #16852, #48899, #51633, #62184, #67302, #8842, #8714, #32774, #25481, #3740, #32070, #19414, #50484, #11218, #22078, #34910, #64908, #50689, #69004, #20021, #53405, #29641, #13829, #28575, #37270, #35198, #36460, #22270, #29859, #24718, #49528, #42925, #53588, #56846, #66742, #52988, #3703, #13493 ) ) ;
#45348 = DIRECTION ( 'NONE',  ( -1.794541526872559352E-16, -1.000000000000000000, 0.000000000000000000 ) ) ;
#45349 = CARTESIAN_POINT ( 'NONE',  ( 15.50000000000000000, 0.000000000000000000, 18.50000000000000000 ) ) ;
#45350 = ORIENTED_EDGE ( 'NONE', *, *, #18112, .F. ) ;
#45351 = ORIENTED_EDGE ( 'NONE', *, *, #12508, .T. ) ;
#45353 = VERTEX_POINT ( 'NONE', #67672 ) ;
#45352 = CARTESIAN_POINT ( 'NONE',  ( 7.357023737882817827, -6.665817930929303969, 54.00000000000000711 ) ) ;
#45354 = ADVANCED_FACE ( 'NONE', ( #51405 ), #23837, .T. ) ;
#45355 = VERTEX_POINT ( 'NONE', #19233 ) ;
#45356 = DIRECTION ( 'NONE',  ( -1.000000000000000000, 0.000000000000000000, 0.000000000000000000 ) ) ;
#45357 = CARTESIAN_POINT ( 'NONE',  ( 8.900000000000002132, 21.00000000000000000, -18.00000000000000355 ) ) ;
#45358 = DIRECTION ( 'NONE',  ( -1.836970198721029934E-16, -1.836970198721010706E-16, 1.000000000000000000 ) ) ;
#45359 = LINE ( 'NONE', #23101, #63554 ) ;
#45360 = AXIS2_PLACEMENT_3D ( 'NONE', #64413, #10312, #4663 ) ;
#45361 = LINE ( 'NONE', #24156, #52226 ) ;
#45362 = VERTEX_POINT ( 'NONE', #34423 ) ;
#45363 = VERTEX_POINT ( 'NONE', #62358 ) ;
#45364 = ORIENTED_EDGE ( 'NONE', *, *, #36928, .F. ) ;
#45365 = ORIENTED_EDGE ( 'NONE', *, *, #47569, .T. ) ;
#45366 = CARTESIAN_POINT ( 'NONE',  ( 7.000000000000000000, -32.44999999999905071, -13.20000000000091944 ) ) ;
#45367 = APPLICATION_CONTEXT ( 'automotive_design' ) ;
#45368 = EDGE_CURVE ( 'NONE', #24527, #27762, #31227, .T. ) ;
#45369 = DIRECTION ( 'NONE',  ( -1.836970198721029934E-16, 1.836970198721036344E-16, -1.000000000000000000 ) ) ;
#45370 = DIRECTION ( 'NONE',  ( 0.000000000000000000, 1.000000000000000000, 0.000000000000000000 ) ) ;
#45372 = EDGE_CURVE ( 'NONE', #18037, #25620, #7464, .T. ) ;
#45371 =( NAMED_UNIT ( * ) PLANE_ANGLE_UNIT ( ) SI_UNIT ( $, .RADIAN. ) );
#45373 = CARTESIAN_POINT ( 'NONE',  ( -5.242976262117259978, 5.242976262117182706, 54.00000000000000711 ) ) ;
#45374 = VECTOR ( 'NONE', #19932, 1000.000000000000000 ) ;
#45375 = ORIENTED_EDGE ( 'NONE', *, *, #50578, .T. ) ;
#45376 = EDGE_LOOP ( 'NONE', ( #13465, #38886, #38007, #26587 ) ) ;
#45377 = ORIENTED_EDGE ( 'NONE', *, *, #68175, .F. ) ;
#45378 = LINE ( 'NONE', #56002, #29420 ) ;
#45379 = ORIENTED_EDGE ( 'NONE', *, *, #53762, .F. ) ;
#45380 = VERTEX_POINT ( 'NONE', #1928 ) ;
#45381 = VECTOR ( 'NONE', #46554, 1000.000000000000000 ) ;
#45382 = VERTEX_POINT ( 'NONE', #66285 ) ;
#45383 = EDGE_LOOP ( 'NONE', ( #8561, #5272, #64543, #61760 ) ) ;
#45384 = DIRECTION ( 'NONE',  ( 0.000000000000000000, 0.000000000000000000, -1.000000000000000000 ) ) ;
#45385 = CIRCLE ( 'NONE', #12666, 1.224999999999997868 ) ;
#45387 = ORIENTED_EDGE ( 'NONE', *, *, #31648, .T. ) ;
#45386 = CARTESIAN_POINT ( 'NONE',  ( -8.130476262117259267, 9.547976262117177981, 26.00000000000000711 ) ) ;
#45388 = DIRECTION ( 'NONE',  ( -1.000000000000000000, 0.000000000000000000, 0.000000000000000000 ) ) ;
#45389 = EDGE_CURVE ( 'NONE', #4520, #68247, #49287, .T. ) ;
#45390 = CARTESIAN_POINT ( 'NONE',  ( 7.000000000000000000, -42.50000000000000000, 10.20000000000000107 ) ) ;
#45391 = CARTESIAN_POINT ( 'NONE',  ( -5.779227145995322168, -6.358413763958943754, 26.00000000000000711 ) ) ;
#45392 = VECTOR ( 'NONE', #6762, 1000.000000000000000 ) ;
#45394 = VERTEX_POINT ( 'NONE', #23494 ) ;
#45393 = DIRECTION ( 'NONE',  ( 0.000000000000000000, 0.7278708115913771204, 0.6857142857147648929 ) ) ;
#45395 = ORIENTED_EDGE ( 'NONE', *, *, #64646, .T. ) ;
#45396 = PLANE ( 'NONE',  #100 ) ;
#45397 = CIRCLE ( 'NONE', #42035, 2.000000000000001776 ) ;
#45398 = DIRECTION ( 'NONE',  ( 0.000000000000000000, 0.000000000000000000, 1.000000000000000000 ) ) ;
#45399 = DIRECTION ( 'NONE',  ( 0.000000000000000000, -1.000000000000000000, 0.000000000000000000 ) ) ;
#45400 = EDGE_LOOP ( 'NONE', ( #9641, #51454, #63338, #65628 ) ) ;
#45401 = VECTOR ( 'NONE', #12302, 1000.000000000000000 ) ;
#45402 = FACE_BOUND ( 'NONE', #31487, .T. ) ;
#45403 = EDGE_CURVE ( 'NONE', #62211, #38554, #41340, .T. ) ;
#45404 = DIRECTION ( 'NONE',  ( 1.000000000000000000, -0.000000000000000000, -0.000000000000000000 ) ) ;
#45405 = AXIS2_PLACEMENT_3D ( 'NONE', #25018, #3450, #51179 ) ;
#45406 = CYLINDRICAL_SURFACE ( 'NONE', #25585, 0.1749999999999998224 ) ;
#45407 = VERTEX_POINT ( 'NONE', #12519 ) ;
#45409 = EDGE_CURVE ( 'NONE', #67467, #57392, #66962, .T. ) ;
#45408 = PLANE ( 'NONE',  #42646 ) ;
#45410 = VECTOR ( 'NONE', #23589, 1000.000000000000000 ) ;
#45411 = DIRECTION ( 'NONE',  ( -0.000000000000000000, 3.673940397442059868E-16, -1.000000000000000000 ) ) ;
#45412 = DIRECTION ( 'NONE',  ( 0.000000000000000000, 1.000000000000000000, 0.000000000000000000 ) ) ;
#45413 = ADVANCED_FACE ( 'NONE', ( #18521 ), #56712, .F. ) ;
#45414 = ORIENTED_EDGE ( 'NONE', *, *, #35205, .F. ) ;
#45415 = PLANE ( 'NONE',  #69698 ) ;
#45416 = PLANE ( 'NONE',  #23015 ) ;
#45417 = EDGE_CURVE ( 'NONE', #62878, #39983, #11999, .T. ) ;
#45418 = ADVANCED_FACE ( 'NONE', ( #12858 ), #24189, .T. ) ;
#45419 = LINE ( 'NONE', #17165, #36773 ) ;
#45420 = LINE ( 'NONE', #63013, #5204 ) ;
#45421 = VERTEX_POINT ( 'NONE', #62008 ) ;
#45422 = LINE ( 'NONE', #50386, #55274 ) ;
#45423 = CARTESIAN_POINT ( 'NONE',  ( 17.24945551514599984, -15.50000000000000000, -25.53140320652400064 ) ) ;
#45424 = CARTESIAN_POINT ( 'NONE',  ( -9.547976262117222390, -2.544523737882724124, 26.00000000000000711 ) ) ;
#45425 = FACE_OUTER_BOUND ( 'NONE', #12762, .T. ) ;
#45426 = CARTESIAN_POINT ( 'NONE',  ( 8.000000000000000000, 8.000000000000001776, 0.000000000000000000 ) ) ;
#45427 = VERTEX_POINT ( 'NONE', #13578 ) ;
#45428 = CARTESIAN_POINT ( 'NONE',  ( -7.415254214038356828, -3.606483450353401121, 455.0000000000000568 ) ) ;
#45429 = CARTESIAN_POINT ( 'NONE',  ( 1.090483450353418426, 10.73351654964659829, 455.0000000000000568 ) ) ;
#45430 = AXIS2_PLACEMENT_3D ( 'NONE', #11859, #65949, #17520 ) ;
#45431 = DIRECTION ( 'NONE',  ( 1.000000000000000000, 0.000000000000000000, 0.000000000000000000 ) ) ;
#45432 = DIRECTION ( 'NONE',  ( -1.000000000000000000, 0.000000000000000000, 0.000000000000000000 ) ) ;
#45433 = LINE ( 'NONE', #18566, #5765 ) ;
#45434 = AXIS2_PLACEMENT_3D ( 'NONE', #35579, #13323, #56802 ) ;
#45435 = ORIENTED_EDGE ( 'NONE', *, *, #64390, .F. ) ;
#45437 = ORIENTED_EDGE ( 'NONE', *, *, #62194, .T. ) ;
#45436 = DIRECTION ( 'NONE',  ( 0.000000000000000000, 0.000000000000000000, 1.000000000000000000 ) ) ;
#45438 = CYLINDRICAL_SURFACE ( 'NONE', #63223, 24.99999999998784972 ) ;
#45439 = DIRECTION ( 'NONE',  ( 0.000000000000000000, -0.000000000000000000, 1.000000000000000000 ) ) ;
#45440 = ORIENTED_EDGE ( 'NONE', *, *, #33695, .T. ) ;
#45441 = AXIS2_PLACEMENT_3D ( 'NONE', #20872, #25482, #47393 ) ;
#45442 = FACE_OUTER_BOUND ( 'NONE', #49473, .T. ) ;
#45443 = ORIENTED_EDGE ( 'NONE', *, *, #67727, .F. ) ;
#45444 = CARTESIAN_POINT ( 'NONE',  ( 24.90000000000000213, 20.60000000000000142, -13.86939075806900057 ) ) ;
#45445 = ORIENTED_EDGE ( 'NONE', *, *, #18138, .F. ) ;
#45446 = VERTEX_POINT ( 'NONE', #8261 ) ;
#45447 = DIRECTION ( 'NONE',  ( 0.000000000000000000, -0.000000000000000000, 1.000000000000000000 ) ) ;
#45448 = EDGE_CURVE ( 'NONE', #62779, #5488, #26289, .T. ) ;
#45449 = CARTESIAN_POINT ( 'NONE',  ( 11.08848345035337246, 11.07551654964657573, 195.0000000000000284 ) ) ;
#45450 = DIRECTION ( 'NONE',  ( -0.000000000000000000, 0.000000000000000000, -1.000000000000000000 ) ) ;
#45452 = EDGE_CURVE ( 'NONE', #58124, #6525, #69630, .T. ) ;
#45451 = FACE_BOUND ( 'NONE', #65524, .T. ) ;
#45453 = CIRCLE ( 'NONE', #29654, 0.1999999999999987899 ) ;
#45454 = ORIENTED_EDGE ( 'NONE', *, *, #48478, .F. ) ;
#45456 = EDGE_CURVE ( 'NONE', #66058, #27819, #9685, .T. ) ;
#45455 = ORIENTED_EDGE ( 'NONE', *, *, #25349, .F. ) ;
#45457 = DIRECTION ( 'NONE',  ( -1.000000000000000000, 0.000000000000000000, 0.000000000000000000 ) ) ;
#45458 = AXIS2_PLACEMENT_3D ( 'NONE', #61688, #13255, #19603 ) ;
#45459 = CARTESIAN_POINT ( 'NONE',  ( 30.00000000000000000, -8.959999999999999076, -12.95475478405700009 ) ) ;
#45460 = ORIENTED_EDGE ( 'NONE', *, *, #38878, .F. ) ;
#45461 = AXIS2_PLACEMENT_3D ( 'NONE', #19872, #41791, #63368 ) ;
#45462 = ORIENTED_EDGE ( 'NONE', *, *, #29118, .F. ) ;
#45463 = ORIENTED_EDGE ( 'NONE', *, *, #50142, .F. ) ;
#45464 = LINE ( 'NONE', #44415, #57609 ) ;
#45465 = AXIS2_PLACEMENT_3D ( 'NONE', #35672, #30382, #51954 ) ;
#45467 = EDGE_LOOP ( 'NONE', ( #42489, #63072, #24700, #17315, #53843, #8525, #48816, #30702 ) ) ;
#45466 = CARTESIAN_POINT ( 'NONE',  ( -24.00000000000000000, -16.28999999999710369, -15.00000000000794920 ) ) ;
#45468 = LINE ( 'NONE', #41217, #11894 ) ;
#45469 = CIRCLE ( 'NONE', #54543, 0.9999999999999991118 ) ;
#45470 = DIRECTION ( 'NONE',  ( 8.673617379884087537E-15, 1.000000000000000000, 0.000000000000000000 ) ) ;
#45471 = EDGE_LOOP ( 'NONE', ( #43866, #31658, #48012, #39727, #2226, #52917, #11343, #67815 ) ) ;
#45472 = EDGE_LOOP ( 'NONE', ( #62151, #30000, #48225, #68264 ) ) ;
#45473 = AXIS2_PLACEMENT_3D ( 'NONE', #7862, #51006, #2565 ) ;
#45474 = DIRECTION ( 'NONE',  ( 1.836970198721029934E-16, 1.836970198721010706E-16, -1.000000000000000000 ) ) ;
#45475 = LINE ( 'NONE', #40528, #43717 ) ;
#45476 = AXIS2_PLACEMENT_3D ( 'NONE', #24699, #23034, #65494 ) ;
#45477 = CARTESIAN_POINT ( 'NONE',  ( 15.50000000000000000, -0.4000000000005274892, 22.50000000000000000 ) ) ;
#45478 = EDGE_CURVE ( 'NONE', #16868, #50939, #41143, .T. ) ;
#45479 = FACE_OUTER_BOUND ( 'NONE', #25647, .T. ) ;
#45480 = CYLINDRICAL_SURFACE ( 'NONE', #42588, 0.1999999999999987899 ) ;
#45482 = EDGE_LOOP ( 'NONE', ( #4265, #16253 ) ) ;
#45481 = PLANE ( 'NONE',  #52361 ) ;
#45483 = ORIENTED_EDGE ( 'NONE', *, *, #50170, .F. ) ;
#45484 = VECTOR ( 'NONE', #52265, 1000.000000000000000 ) ;
#45485 = DIRECTION ( 'NONE',  ( -1.794541526872559352E-16, -1.000000000000000000, 0.000000000000000000 ) ) ;
#45486 = EDGE_CURVE ( 'NONE', #68065, #32954, #9328, .T. ) ;
#45487 = FACE_OUTER_BOUND ( 'NONE', #6683, .T. ) ;
#45488 = FACE_OUTER_BOUND ( 'NONE', #21634, .T. ) ;
#45489 = EDGE_CURVE ( 'NONE', #54344, #69663, #3324, .T. ) ;
#45490 = ADVANCED_FACE ( 'NONE', ( #57763 ), #42551, .T. ) ;
#45491 = CARTESIAN_POINT ( 'NONE',  ( -7.250000000000001776, -7.249999999999998224, -16.00000000000000000 ) ) ;
#45493 = ORIENTED_EDGE ( 'NONE', *, *, #29625, .F. ) ;
#45492 = EDGE_CURVE ( 'NONE', #2465, #24086, #31607, .T. ) ;
#45494 = CARTESIAN_POINT ( 'NONE',  ( -8.393516549646745872, -4.396432944014549093, 455.0000000000000568 ) ) ;
#45495 = EDGE_CURVE ( 'NONE', #43873, #25493, #10863, .T. ) ;
#45496 = FACE_OUTER_BOUND ( 'NONE', #15093, .T. ) ;
#45497 = DIRECTION ( 'NONE',  ( 1.000000000000000000, -0.000000000000000000, -0.000000000000000000 ) ) ;
#45498 = LINE ( 'NONE', #18276, #10841 ) ;
#45499 = AXIS2_PLACEMENT_3D ( 'NONE', #433, #64440, #20944 ) ;
#45500 = ADVANCED_FACE ( 'NONE', ( #4033 ), #52112, .T. ) ;
#45501 = FACE_OUTER_BOUND ( 'NONE', #38284, .T. ) ;
#45502 = DIRECTION ( 'NONE',  ( 8.673617379884013384E-15, 1.000000000000000000, 0.000000000000000000 ) ) ;
#45503 = AXIS2_PLACEMENT_3D ( 'NONE', #36946, #25634, #43878 ) ;
#45504 = DIRECTION ( 'NONE',  ( -0.000000000000000000, 0.000000000000000000, 1.000000000000000000 ) ) ;
#45505 = VECTOR ( 'NONE', #5199, 1000.000000000000000 ) ;
#45506 = EDGE_LOOP ( 'NONE', ( #67743, #40346, #36726, #67544 ) ) ;
#45507 = LINE ( 'NONE', #39845, #15149 ) ;
#45508 = DIRECTION ( 'NONE',  ( 1.000000000000000000, -0.000000000000000000, 0.000000000000000000 ) ) ;
#45509 = ORIENTED_EDGE ( 'NONE', *, *, #40588, .F. ) ;
#45510 = CARTESIAN_POINT ( 'NONE',  ( -11.99351654964671354, 4.173516549646604901, 195.0000000000000284 ) ) ;
#45511 = DIRECTION ( 'NONE',  ( 0.000000000000000000, 0.000000000000000000, 1.000000000000000000 ) ) ;
#45512 = CARTESIAN_POINT ( 'NONE',  ( -8.566576262117349572, -8.930623737882770641, 54.00000000000000711 ) ) ;
#45514 = AXIS2_PLACEMENT_3D ( 'NONE', #58918, #15439, #64232 ) ;
#45513 = DIRECTION ( 'NONE',  ( 1.000000000000000000, 0.000000000000000000, 0.000000000000000000 ) ) ;
#45515 = CARTESIAN_POINT ( 'NONE',  ( -29.50000000000000355, -11.50000000000100009, -10.50000000000065903 ) ) ;
#45516 = ORIENTED_EDGE ( 'NONE', *, *, #60394, .F. ) ;
#45517 = CARTESIAN_POINT ( 'NONE',  ( 7.811466277050743479, 4.727349090213326832, 455.0000000000000568 ) ) ;
#45518 = ORIENTED_EDGE ( 'NONE', *, *, #55458, .T. ) ;
#45519 = CARTESIAN_POINT ( 'NONE',  ( 9.912023737882783792, 3.842976262117149044, 54.00000000000000711 ) ) ;
#45520 = ORIENTED_EDGE ( 'NONE', *, *, #58023, .F. ) ;
#45521 = CARTESIAN_POINT ( 'NONE',  ( 1.000000000000000000, -21.00000000000000000, -4.000000000000000000 ) ) ;
#45522 = AXIS2_PLACEMENT_3D ( 'NONE', #47454, #30145, #30845 ) ;
#45523 = VERTEX_POINT ( 'NONE', #47505 ) ;
#45524 = LINE ( 'NONE', #67101, #7294 ) ;
#45525 = DIRECTION ( 'NONE',  ( 0.000000000000000000, 1.000000000000000000, 0.000000000000000000 ) ) ;
#45526 = ORIENTED_EDGE ( 'NONE', *, *, #42043, .F. ) ;
#45527 = ORIENTED_EDGE ( 'NONE', *, *, #43400, .F. ) ;
#45528 = VECTOR ( 'NONE', #21873, 1000.000000000000114 ) ;
#45529 = DIRECTION ( 'NONE',  ( 1.000000000000000000, 0.000000000000000000, 0.000000000000000000 ) ) ;
#45530 = ORIENTED_EDGE ( 'NONE', *, *, #61939, .T. ) ;
#45531 = ORIENTED_EDGE ( 'NONE', *, *, #58215, .T. ) ;
#45532 = CARTESIAN_POINT ( 'NONE',  ( -7.250000000000000888, 7.450000000000003730, -20.50000000000000000 ) ) ;
#45533 = FACE_OUTER_BOUND ( 'NONE', #11719, .T. ) ;
#45534 = DIRECTION ( 'NONE',  ( -1.000000000000000000, 1.813998472013049822E-14, -1.836970198720996654E-16 ) ) ;
#45535 = ORIENTED_EDGE ( 'NONE', *, *, #16758, .T. ) ;
#45536 = VECTOR ( 'NONE', #58513, 1000.000000000000000 ) ;
#45537 = EDGE_CURVE ( 'NONE', #11471, #20459, #26770, .T. ) ;
#45538 = DIRECTION ( 'NONE',  ( 0.000000000000000000, 0.000000000000000000, -1.000000000000000000 ) ) ;
#45539 = EDGE_CURVE ( 'NONE', #68300, #37771, #8620, .T. ) ;
#45541 = CARTESIAN_POINT ( 'NONE',  ( 7.250000000000005329, -7.249999999999998224, -9.500000000000001776 ) ) ;
#45540 = CARTESIAN_POINT ( 'NONE',  ( -30.00000000000000000, -17.50000000000000000, -15.70500000000000007 ) ) ;
#45542 = ORIENTED_EDGE ( 'NONE', *, *, #17669, .T. ) ;
#45544 = ORIENTED_EDGE ( 'NONE', *, *, #46966, .T. ) ;
#45543 = CARTESIAN_POINT ( 'NONE',  ( 4.201500623656053257, 4.727349090213338378, 455.0000000000000568 ) ) ;
#45545 = ORIENTED_EDGE ( 'NONE', *, *, #67231, .F. ) ;
#45546 = EDGE_CURVE ( 'NONE', #26698, #52016, #30895, .T. ) ;
#45547 = APPLICATION_PROTOCOL_DEFINITION ( 'draft international standard', 'automotive_design', 1998, #46719 ) ;
#45548 = CARTESIAN_POINT ( 'NONE',  ( 1.866219381641426533, -9.417013320880872840, 455.0000000000000568 ) ) ;
#45549 = ORIENTED_EDGE ( 'NONE', *, *, #33423, .F. ) ;
#45550 = CARTESIAN_POINT ( 'NONE',  ( -6.500000000000002665, 6.500000000000002665, -1.000000000000000000 ) ) ;
#45551 = VECTOR ( 'NONE', #59097, 1000.000000000000000 ) ;
#45552 = VECTOR ( 'NONE', #33801, 1000.000000000000000 ) ;
#45553 = FACE_OUTER_BOUND ( 'NONE', #36708, .T. ) ;
#45554 = ORIENTED_EDGE ( 'NONE', *, *, #57435, .F. ) ;
#45555 = VERTEX_POINT ( 'NONE', #58116 ) ;
#45557 = CARTESIAN_POINT ( 'NONE',  ( 3.857023737882817827, 10.30047626211720413, 54.00000000000000711 ) ) ;
#45556 = CIRCLE ( 'NONE', #53475, 0.4000000000000600298 ) ;
#45558 = VECTOR ( 'NONE', #8438, 1000.000000000000000 ) ;
#45559 = DIRECTION ( 'NONE',  ( 0.000000000000000000, 0.000000000000000000, -1.000000000000000000 ) ) ;
#45560 = ORIENTED_EDGE ( 'NONE', *, *, #30495, .T. ) ;
#45561 = CARTESIAN_POINT ( 'NONE',  ( 9.247904806590677040, 9.942044687070474396, 195.0000000000000284 ) ) ;
#45562 = CARTESIAN_POINT ( 'NONE',  ( -5.993516549646776603, -6.006483450353426790, 455.0000000000000568 ) ) ;
#45563 = CIRCLE ( 'NONE', #62524, 4.500000000000191847 ) ;
#45564 = AXIS2_PLACEMENT_3D ( 'NONE', #33318, #64465, #10706 ) ;
#45565 = LINE ( 'NONE', #18698, #13645 ) ;
#45566 = EDGE_LOOP ( 'NONE', ( #60631, #58961, #29879, #1784 ) ) ;
#45567 = CARTESIAN_POINT ( 'NONE',  ( 6.836383711242997485, 6.350872789121265960, 26.00000000000000711 ) ) ;
#45568 = LINE ( 'NONE', #41320, #49511 ) ;
#45570 = EDGE_LOOP ( 'NONE', ( #35493, #57397, #42080, #43814 ) ) ;
#45569 = DIRECTION ( 'NONE',  ( 1.000000000000000000, 0.000000000000000000, 0.000000000000000000 ) ) ;
#45572 = VERTEX_POINT ( 'NONE', #63777 ) ;
#45571 = CARTESIAN_POINT ( 'NONE',  ( 6.501044194225490180, -2.632023737882815517, 26.00000000000000711 ) ) ;
#45573 = CARTESIAN_POINT ( 'NONE',  ( 8.250000000000005329, 7.250000000000000888, -26.00000000000001066 ) ) ;
#45574 = DIRECTION ( 'NONE',  ( 0.000000000000000000, 1.000000000000000000, 0.000000000000000000 ) ) ;
#45575 = DIRECTION ( 'NONE',  ( 1.203165845134433084E-14, 1.000000000000000000, 0.000000000000000000 ) ) ;
#45576 = DIRECTION ( 'NONE',  ( 1.261617073437657735E-14, 1.000000000000000000, 3.673940397442059868E-16 ) ) ;
#45577 = LINE ( 'NONE', #23332, #33065 ) ;
#45578 = ORIENTED_EDGE ( 'NONE', *, *, #65116, .T. ) ;
#45579 = DIRECTION ( 'NONE',  ( 0.000000000000000000, 0.000000000000000000, 1.000000000000000000 ) ) ;
#45580 = EDGE_CURVE ( 'NONE', #1599, #32551, #30196, .T. ) ;
#45581 = DIRECTION ( 'NONE',  ( 0.000000000000000000, 1.000000000000000000, 0.000000000000000000 ) ) ;
#45582 = EDGE_CURVE ( 'NONE', #43101, #55737, #59476, .T. ) ;
#45583 = FACE_OUTER_BOUND ( 'NONE', #24402, .T. ) ;
#45585 = VERTEX_POINT ( 'NONE', #41504 ) ;
#45584 = CARTESIAN_POINT ( 'NONE',  ( -4.706725378239251967, -4.155633711806651753, 54.00000000000000711 ) ) ;
#45586 = CARTESIAN_POINT ( 'NONE',  ( -2.500000000000000000, 0.000000000000000000, -29.90000000000000924 ) ) ;
#45587 = EDGE_CURVE ( 'NONE', #9547, #5555, #14627, .T. ) ;
#45588 = EDGE_CURVE ( 'NONE', #42164, #57112, #47168, .T. ) ;
#45589 = LINE ( 'NONE', #3876, #58963 ) ;
#45590 = ORIENTED_EDGE ( 'NONE', *, *, #53594, .T. ) ;
#45591 = VERTEX_POINT ( 'NONE', #41845 ) ;
#45592 = DIRECTION ( 'NONE',  ( -0.000000000000000000, -0.000000000000000000, -1.000000000000000000 ) ) ;
#45593 = DIRECTION ( 'NONE',  ( 0.000000000000000000, 0.000000000000000000, 1.000000000000000000 ) ) ;
#45594 = ORIENTED_EDGE ( 'NONE', *, *, #27093, .F. ) ;
#45595 = CARTESIAN_POINT ( 'NONE',  ( 283.0000000000000568, -39.79999999999954952, -8.900000000000419575 ) ) ;
#45596 = CARTESIAN_POINT ( 'NONE',  ( 7.250000000000005329, -7.249999999999998224, -14.50000000000000000 ) ) ;
#45597 = EDGE_CURVE ( 'NONE', #13055, #17772, #24489, .T. ) ;
#45598 = CARTESIAN_POINT ( 'NONE',  ( 88.07321854994620480, 47.95351654967443977, 43.00000000000000000 ) ) ;
#45599 = ADVANCED_FACE ( 'NONE', ( #42195 ), #34345, .T. ) ;
#45600 = DIRECTION ( 'NONE',  ( 0.000000000000000000, 1.000000000000000000, 0.000000000000000000 ) ) ;
#45601 = VECTOR ( 'NONE', #21875, 1000.000000000000000 ) ;
#45602 = AXIS2_PLACEMENT_3D ( 'NONE', #61273, #67304, #51381 ) ;
#45603 = ORIENTED_EDGE ( 'NONE', *, *, #20653, .T. ) ;
#45604 = DIRECTION ( 'NONE',  ( 0.000000000000000000, 0.000000000000000000, -1.000000000000000000 ) ) ;
#45605 = EDGE_LOOP ( 'NONE', ( #59786, #69490, #49281, #51715 ) ) ;
#45606 = ORIENTED_EDGE ( 'NONE', *, *, #15984, .T. ) ;
#45607 = DIRECTION ( 'NONE',  ( 0.000000000000000000, 0.000000000000000000, 1.000000000000000000 ) ) ;
#45608 = VECTOR ( 'NONE', #50317, 1000.000000000000000 ) ;
#45609 = AXIS2_PLACEMENT_3D ( 'NONE', #69252, #20808, #9872 ) ;
#45610 = AXIS2_PLACEMENT_3D ( 'NONE', #44934, #19111, #40679 ) ;
#45612 = CARTESIAN_POINT ( 'NONE',  ( 0.000000000000000000, 0.000000000000000000, -29.90000000000000924 ) ) ;
#45611 = CARTESIAN_POINT ( 'NONE',  ( 10.31452373788280674, 6.835476262117182067, 54.00000000000000711 ) ) ;
#45613 = ORIENTED_EDGE ( 'NONE', *, *, #9513, .T. ) ;
#45614 = ORIENTED_EDGE ( 'NONE', *, *, #32527, .F. ) ;
#45615 = DIRECTION ( 'NONE',  ( 1.349135440953254805E-14, 1.000000000000000000, 1.836970198721035604E-16 ) ) ;
#45616 = EDGE_LOOP ( 'NONE', ( #6669, #49309, #24740, #29261, #69816, #41868, #39058, #22778 ) ) ;
#45617 = DIRECTION ( 'NONE',  ( 0.000000000000000000, -0.7071067811865455743, 0.7071067811865495711 ) ) ;
#45618 = CARTESIAN_POINT ( 'NONE',  ( 3.848229544836323512, -7.357023737882803616, 26.00000000000000000 ) ) ;
#45619 = CARTESIAN_POINT ( 'NONE',  ( -8.130476262117319664, -9.562023737882764607, 26.00000000000000000 ) ) ;
#45620 = DIRECTION ( 'NONE',  ( 0.000000000000000000, 0.000000000000000000, 1.000000000000000000 ) ) ;
#45621 = ORIENTED_EDGE ( 'NONE', *, *, #11771, .T. ) ;
#45622 = AXIS2_PLACEMENT_3D ( 'NONE', #6085, #48876, #27997 ) ;
#45623 = CARTESIAN_POINT ( 'NONE',  ( 7.749999999999998224, -7.348062532928000934, 0.000000000000000000 ) ) ;
#45625 = CARTESIAN_POINT ( 'NONE',  ( 8.250000000000005329, 7.250000000000000888, -8.500000000000000000 ) ) ;
#45624 = LINE ( 'NONE', #12742, #27627 ) ;
#45626 = ORIENTED_EDGE ( 'NONE', *, *, #44572, .F. ) ;
#45628 = VERTEX_POINT ( 'NONE', #52036 ) ;
#45627 = CARTESIAN_POINT ( 'NONE',  ( 8.250000000000005329, 7.250000000000000888, -19.00000000000000000 ) ) ;
#45629 = EDGE_LOOP ( 'NONE', ( #22692, #27291, #62117, #31031, #10721, #54571, #35022 ) ) ;
#45630 = ORIENTED_EDGE ( 'NONE', *, *, #60975, .F. ) ;
#45631 = EDGE_CURVE ( 'NONE', #37791, #56148, #51323, .T. ) ;
#45632 = LINE ( 'NONE', #34319, #61439 ) ;
#45633 =( BOUNDED_CURVE ( )  B_SPLINE_CURVE ( 3, ( #21070, #42630, #64216, #15766 ),
 .UNSPECIFIED., .F., .F. ) 
 B_SPLINE_CURVE_WITH_KNOTS ( ( 4, 4 ),
 ( 2.245927859731927878, 2.418858405776376674 ),
 .UNSPECIFIED. ) 
 CURVE ( )  GEOMETRIC_REPRESENTATION_ITEM ( )  RATIONAL_B_SPLINE_CURVE ( ( 1.000000000000000000, 0.9975094710839674805, 0.9975094710839674805, 1.000000000000000000 ) ) 
 REPRESENTATION_ITEM ( '' )  );
#45634 = CARTESIAN_POINT ( 'NONE',  ( 283.0000000000000568, -25.50000000000000355, -17.00000000000000000 ) ) ;
#45635 = VERTEX_POINT ( 'NONE', #2191 ) ;
#45636 = ORIENTED_EDGE ( 'NONE', *, *, #41431, .F. ) ;
#45637 = EDGE_CURVE ( 'NONE', #53899, #59557, #35758, .T. ) ;
#45638 = PLANE ( 'NONE',  #3792 ) ;
#45639 = CARTESIAN_POINT ( 'NONE',  ( 0.000000000000000000, -0.5000000000000000000, -26.50000000000000000 ) ) ;
#45640 =( GEOMETRIC_REPRESENTATION_CONTEXT ( 3 ) GLOBAL_UNCERTAINTY_ASSIGNED_CONTEXT ( ( #37332 ) ) GLOBAL_UNIT_ASSIGNED_CONTEXT ( ( #67173, #29334, #18736 ) ) REPRESENTATION_CONTEXT ( 'NONE', 'WORKASPACE' ) );
#45641 = EDGE_LOOP ( 'NONE', ( #8992, #40586, #33561, #7214 ) ) ;
#45642 = VERTEX_POINT ( 'NONE', #13139 ) ;
#45643 = CARTESIAN_POINT ( 'NONE',  ( 11.08848345035334404, -9.804883450353433005, 195.0000000000000284 ) ) ;
#45644 = EDGE_CURVE ( 'NONE', #961, #35523, #50978, .T. ) ;
#45645 = CARTESIAN_POINT ( 'NONE',  ( 24.90000000000000213, -14.06939075806900874, 20.80000000000001137 ) ) ;
#45646 = VERTEX_POINT ( 'NONE', #12778 ) ;
#45647 = VECTOR ( 'NONE', #9442, 1000.000000000000000 ) ;
#45648 = VECTOR ( 'NONE', #68003, 1000.000000000000114 ) ;
#45649 = LINE ( 'NONE', #60872, #53815 ) ;
#45650 = DIRECTION ( 'NONE',  ( 0.000000000000000000, 0.000000000000000000, -1.000000000000000000 ) ) ;
#45652 = ORIENTED_EDGE ( 'NONE', *, *, #66083, .T. ) ;
#45651 = DIRECTION ( 'NONE',  ( -1.000000000000000000, 0.000000000000000000, 0.000000000000000000 ) ) ;
#45653 = ORIENTED_EDGE ( 'NONE', *, *, #18420, .F. ) ;
#45654 = DIRECTION ( 'NONE',  ( -7.457533623526253657E-15, -1.000000000000000000, -1.836970198721024757E-16 ) ) ;
#45655 = CARTESIAN_POINT ( 'NONE',  ( 283.0000000000000568, -53.81370849898476649, -17.35424868893542438 ) ) ;
#45656 = VECTOR ( 'NONE', #33211, 1000.000000000000000 ) ;
#45657 = AXIS2_PLACEMENT_3D ( 'NONE', #1115, #44565, #22344 ) ;
#45658 = VECTOR ( 'NONE', #58499, 1000.000000000000000 ) ;
#45659 = CARTESIAN_POINT ( 'NONE',  ( -4.135079735113210475, -6.836383711242997485, 26.00000000000000711 ) ) ;
#45660 = DIRECTION ( 'NONE',  ( -0.000000000000000000, -0.000000000000000000, 1.000000000000000000 ) ) ;
#45661 = EDGE_CURVE ( 'NONE', #8473, #46156, #40718, .T. ) ;
#45662 = DIRECTION ( 'NONE',  ( 0.000000000000000000, 0.000000000000000000, -1.000000000000000000 ) ) ;
#45663 = DIRECTION ( 'NONE',  ( -0.000000000000000000, -1.000000000000000000, 0.000000000000000000 ) ) ;
#45664 = VECTOR ( 'NONE', #24334, 1000.000000000000000 ) ;
#45665 = DIRECTION ( 'NONE',  ( 0.000000000000000000, 0.000000000000000000, -1.000000000000000000 ) ) ;
#45666 = ORIENTED_EDGE ( 'NONE', *, *, #14921, .T. ) ;
#45667 = DIRECTION ( 'NONE',  ( -1.000000000000000000, 0.000000000000000000, 0.000000000000000000 ) ) ;
#45669 = VERTEX_POINT ( 'NONE', #24099 ) ;
#45668 = DIRECTION ( 'NONE',  ( 1.000000000000000000, 0.000000000000000000, 0.000000000000000000 ) ) ;
#45670 = DIRECTION ( 'NONE',  ( -1.836970198721029934E-16, 1.836970198721036590E-16, -1.000000000000000000 ) ) ;
#45671 = DIRECTION ( 'NONE',  ( 0.000000000000000000, 0.000000000000000000, 1.000000000000000000 ) ) ;
#45672 = EDGE_CURVE ( 'NONE', #1043, #29792, #34709, .T. ) ;
#45673 = EDGE_CURVE ( 'NONE', #5244, #65035, #68294, .T. ) ;
#45674 = CARTESIAN_POINT ( 'NONE',  ( 7.450000000000004619, -1.336933437520057563E-15, -16.00000000000000000 ) ) ;
#45675 = DIRECTION ( 'NONE',  ( 1.000000000000000000, -0.000000000000000000, -0.000000000000000000 ) ) ;
#45676 = CARTESIAN_POINT ( 'NONE',  ( -7.744988412222944874, -8.465062094116097668, 455.0000000000000568 ) ) ;
#45677 = EDGE_CURVE ( 'NONE', #41506, #5501, #2884, .T. ) ;
#45678 = ORIENTED_EDGE ( 'NONE', *, *, #46433, .F. ) ;
#45679 = DIRECTION ( 'NONE',  ( 0.000000000000000000, -0.000000000000000000, 1.000000000000000000 ) ) ;
#45680 = ORIENTED_EDGE ( 'NONE', *, *, #17497, .F. ) ;
#45681 = CARTESIAN_POINT ( 'NONE',  ( 30.00000000000000000, -17.50000000000000000, 26.64999999999999858 ) ) ;
#45682 = EDGE_CURVE ( 'NONE', #8950, #69402, #62278, .T. ) ;
#45683 = SURFACE_SIDE_STYLE ('',( #40020 ) ) ;
#45684 = EDGE_CURVE ( 'NONE', #47684, #26595, #46367, .T. ) ;
#45685 = DIRECTION ( 'NONE',  ( 0.000000000000000000, 0.000000000000000000, -1.000000000000000000 ) ) ;
#45686 = VERTEX_POINT ( 'NONE', #19148 ) ;
#45687 = FACE_OUTER_BOUND ( 'NONE', #6598, .T. ) ;
#45688 = ORIENTED_EDGE ( 'NONE', *, *, #37024, .T. ) ;
#45689 = AXIS2_PLACEMENT_3D ( 'NONE', #62574, #57285, #34662 ) ;
#45690 = ORIENTED_EDGE ( 'NONE', *, *, #35423, .F. ) ;
#45691 = DIRECTION ( 'NONE',  ( 3.491481338843132961E-15, 1.000000000000000000, 0.000000000000000000 ) ) ;
#45692 = CARTESIAN_POINT ( 'NONE',  ( -6.642976262117260333, 9.897976262117179402, 54.00000000000000711 ) ) ;
#45693 = EDGE_LOOP ( 'NONE', ( #16150, #36133, #27687, #15005 ) ) ;
#45694 = DIRECTION ( 'NONE',  ( 0.000000000000000000, -1.000000000000000000, 0.000000000000000000 ) ) ;
#45695 = EDGE_CURVE ( 'NONE', #7061, #187, #66878, .T. ) ;
#45696 = DIRECTION ( 'NONE',  ( 0.000000000000000000, -0.000000000000000000, 1.000000000000000000 ) ) ;
#45697 = FACE_OUTER_BOUND ( 'NONE', #39036, .T. ) ;
#45698 = ORIENTED_EDGE ( 'NONE', *, *, #23298, .F. ) ;
#45699 = ORIENTED_EDGE ( 'NONE', *, *, #50368, .T. ) ;
#45701 = ORIENTED_EDGE ( 'NONE', *, *, #14327, .F. ) ;
#45700 = CARTESIAN_POINT ( 'NONE',  ( -11.00000000000000000, -10.85999999999999943, 9.000000000000001776 ) ) ;
#45702 = EDGE_LOOP ( 'NONE', ( #4981, #22745, #42982, #23808 ) ) ;
#45703 = CIRCLE ( 'NONE', #46872, 25.39999999999999858 ) ;
#45704 = DIRECTION ( 'NONE',  ( 1.836970198721029934E-16, 1.836970198721010706E-16, -1.000000000000000000 ) ) ;
#45705 = LINE ( 'NONE', #45357, #57570 ) ;
#45706 = PLANE ( 'NONE',  #5248 ) ;
#45707 = EDGE_CURVE ( 'NONE', #4332, #856, #24463, .T. ) ;
#45708 = DIRECTION ( 'NONE',  ( 0.000000000000000000, 0.000000000000000000, -1.000000000000000000 ) ) ;
#45709 = LINE ( 'NONE', #30160, #55916 ) ;
#45710 = AXIS2_PLACEMENT_3D ( 'NONE', #44479, #34208, #51187 ) ;
#45711 = DIRECTION ( 'NONE',  ( 1.000000000000000000, 0.000000000000000000, 0.000000000000000000 ) ) ;
#45712 = ORIENTED_EDGE ( 'NONE', *, *, #61052, .T. ) ;
#45713 = VERTEX_POINT ( 'NONE', #2531 ) ;
#45714 = ORIENTED_EDGE ( 'NONE', *, *, #6160, .T. ) ;
#45715 = EDGE_CURVE ( 'NONE', #29937, #25227, #5336, .T. ) ;
#45716 = VERTEX_POINT ( 'NONE', #29749 ) ;
#45717 = CARTESIAN_POINT ( 'NONE',  ( 9.899999999999998579, -21.00000000000000000, 13.86939075806900057 ) ) ;
#45718 = CARTESIAN_POINT ( 'NONE',  ( 4.747751991980655895, 6.606374702650043673, 455.0000000000000568 ) ) ;
#45719 = EDGE_CURVE ( 'NONE', #65838, #15525, #45309, .T. ) ;
#45720 = SHAPE_REPRESENTATION_RELATIONSHIP ( 'NONE' , 'NONE' ,  #26379, #63000 ) ;
#45721 = CARTESIAN_POINT ( 'NONE',  ( 283.0000000000000568, -39.79999999999905214, -12.19999999999906315 ) ) ;
#45722 = EDGE_LOOP ( 'NONE', ( #42866, #11283, #35111, #25614 ) ) ;
#45723 = VERTEX_POINT ( 'NONE', #18433 ) ;
#45724 = ORIENTED_EDGE ( 'NONE', *, *, #28455, .F. ) ;
#45725 = EDGE_CURVE ( 'NONE', #49372, #64729, #35399, .T. ) ;
#45726 = AXIS2_PLACEMENT_3D ( 'NONE', #3074, #9419, #24982 ) ;
#45727 = DIRECTION ( 'NONE',  ( -1.000000000000000000, 0.000000000000000000, 0.000000000000000000 ) ) ;
#45728 = ORIENTED_EDGE ( 'NONE', *, *, #69463, .T. ) ;
#45729 = EDGE_LOOP ( 'NONE', ( #27246, #20575, #19120, #57741 ) ) ;
#45730 = CARTESIAN_POINT ( 'NONE',  ( -7.250000000000000888, -8.249999999999998224, -20.00000000000000000 ) ) ;
#45731 = ORIENTED_EDGE ( 'NONE', *, *, #9151, .T. ) ;
#45732 = VERTEX_POINT ( 'NONE', #19495 ) ;
#45733 = DIRECTION ( 'NONE',  ( 0.000000000000000000, 0.000000000000000000, -1.000000000000000000 ) ) ;
#45734 = EDGE_CURVE ( 'NONE', #58511, #45115, #28966, .T. ) ;
#45736 = VERTEX_POINT ( 'NONE', #56632 ) ;
#45735 = CARTESIAN_POINT ( 'NONE',  ( -9.390476262117203987, -1.480523737882726731, 26.00000000000000711 ) ) ;
#45737 = ORIENTED_EDGE ( 'NONE', *, *, #52798, .F. ) ;
#45738 = LINE ( 'NONE', #35129, #65131 ) ;
#45739 = FACE_OUTER_BOUND ( 'NONE', #65442, .T. ) ;
#45740 = DIRECTION ( 'NONE',  ( 0.000000000000000000, 1.000000000000000000, 0.000000000000000000 ) ) ;
#45741 = EDGE_CURVE ( 'NONE', #59830, #59223, #56969, .T. ) ;
#45743 = ORIENTED_EDGE ( 'NONE', *, *, #68169, .T. ) ;
#45742 = DIRECTION ( 'NONE',  ( 1.000000000000000000, 0.000000000000000000, -0.000000000000000000 ) ) ;
#45744 = EDGE_CURVE ( 'NONE', #21817, #67535, #8530, .T. ) ;
#45745 = ORIENTED_EDGE ( 'NONE', *, *, #69769, .F. ) ;
#45746 = EDGE_CURVE ( 'NONE', #19545, #54169, #47057, .T. ) ;
#45747 = AXIS2_PLACEMENT_3D ( 'NONE', #6146, #27375, #49297 ) ;
#45748 = DIRECTION ( 'NONE',  ( 0.000000000000000000, 0.000000000000000000, 1.000000000000000000 ) ) ;
#45749 = EDGE_CURVE ( 'NONE', #5714, #24664, #41761, .T. ) ;
#45750 = EDGE_CURVE ( 'NONE', #52724, #19489, #1870, .T. ) ;
#45751 = DIRECTION ( 'NONE',  ( -1.000000000000000000, 0.000000000000000000, 0.000000000000000000 ) ) ;
#45752 = CARTESIAN_POINT ( 'NONE',  ( 10.31452373788281562, -3.664523737882826815, 54.00000000000000711 ) ) ;
#45753 = VECTOR ( 'NONE', #56141, 1000.000000000000000 ) ;
#45754 = ORIENTED_EDGE ( 'NONE', *, *, #29026, .F. ) ;
#45755 = CARTESIAN_POINT ( 'NONE',  ( 1.090483450353343819, -10.74648345035345365, 455.0000000000000568 ) ) ;
#45756 = EDGE_CURVE ( 'NONE', #10719, #41033, #9251, .T. ) ;
#45757 = AXIS2_PLACEMENT_3D ( 'NONE', #5505, #60265, #53946 ) ;
#45758 = VECTOR ( 'NONE', #28210, 1000.000000000000000 ) ;
#45760 = CARTESIAN_POINT ( 'NONE',  ( 7.250000000000005329, -8.249999999999998224, -26.00000000000001066 ) ) ;
#45759 = VECTOR ( 'NONE', #21485, 1000.000000000000000 ) ;
#45761 = DIRECTION ( 'NONE',  ( 0.000000000000000000, -1.000000000000000000, 0.000000000000000000 ) ) ;
#45762 = ADVANCED_FACE ( 'NONE', ( #42114, #19847, #4649, #14906, #63343, #68654 ), #52754, .T. ) ;
#45763 = EDGE_LOOP ( 'NONE', ( #11867, #31312, #42118, #24431 ) ) ;
#45764 = CYLINDRICAL_SURFACE ( 'NONE', #65228, 0.3499999999999996447 ) ;
#45765 = EDGE_CURVE ( 'NONE', #3117, #52106, #30138, .T. ) ;
#45766 = CIRCLE ( 'NONE', #50261, 24.99999999998784972 ) ;
#45767 = AXIS2_PLACEMENT_3D ( 'NONE', #66247, #6836, #28405 ) ;
#45768 = CARTESIAN_POINT ( 'NONE',  ( 8.465062094116069247, -7.757955312929635028, 455.0000000000000568 ) ) ;
#45769 = DIRECTION ( 'NONE',  ( -1.280238727658158432E-15, -1.000000000000000000, 0.000000000000000000 ) ) ;
#45770 = ORIENTED_EDGE ( 'NONE', *, *, #63227, .F. ) ;
#45771 = VECTOR ( 'NONE', #25771, 1000.000000000000000 ) ;
#45772 = CARTESIAN_POINT ( 'NONE',  ( -2.752095193409461071, -9.955011587777271131, 195.0000000000000284 ) ) ;
#45773 = EDGE_CURVE ( 'NONE', #18655, #27811, #57239, .T. ) ;
#45774 = CARTESIAN_POINT ( 'NONE',  ( 41.09999999999999432, 20.60000000000000142, -13.86939075806900057 ) ) ;
#45775 = ADVANCED_FACE ( 'NONE', ( #53440 ), #26561, .F. ) ;
#45776 = AXIS2_PLACEMENT_3D ( 'NONE', #37980, #59540, #9712 ) ;
#45777 = ORIENTED_EDGE ( 'NONE', *, *, #5304, .T. ) ;
#45778 = DIRECTION ( 'NONE',  ( -1.000000000000000000, 0.000000000000000000, 0.000000000000000000 ) ) ;
#45779 = LINE ( 'NONE', #6902, #27541 ) ;
#45780 = CARTESIAN_POINT ( 'NONE',  ( -9.390476262117259054, 1.466476262117183627, 54.00000000000000711 ) ) ;
#45781 = AXIS2_PLACEMENT_3D ( 'NONE', #26568, #48140, #54142 ) ;
#45782 = DIRECTION ( 'NONE',  ( 1.000000000000000000, 5.013651664672856055E-16, 0.000000000000000000 ) ) ;
#45783 = DIRECTION ( 'NONE',  ( 0.000000000000000000, 0.000000000000000000, -1.000000000000000000 ) ) ;
#45784 = ORIENTED_EDGE ( 'NONE', *, *, #7688, .F. ) ;
#45785 = LINE ( 'NONE', #67001, #28746 ) ;
#45786 = CARTESIAN_POINT ( 'NONE',  ( -5.779227145995281312, -4.155633711806634878, 26.00000000000000711 ) ) ;
#45787 = EDGE_CURVE ( 'NONE', #60403, #42593, #4316, .T. ) ;
#45788 = CARTESIAN_POINT ( 'NONE',  ( 15.50000000000000000, -2.500000000000000000, -23.94337567297399971 ) ) ;
#45789 = FACE_OUTER_BOUND ( 'NONE', #43238, .T. ) ;
#45790 = LINE ( 'NONE', #55705, #27214 ) ;
#45791 = ORIENTED_EDGE ( 'NONE', *, *, #55799, .T. ) ;
#45793 = ORIENTED_EDGE ( 'NONE', *, *, #40844, .F. ) ;
#45792 = FACE_OUTER_BOUND ( 'NONE', #33445, .T. ) ;
#45794 = DIRECTION ( 'NONE',  ( -1.836970198721029934E-16, 1.836970198721036590E-16, -1.000000000000000000 ) ) ;
#45795 = FACE_OUTER_BOUND ( 'NONE', #64011, .T. ) ;
#45796 = ORIENTED_EDGE ( 'NONE', *, *, #27692, .T. ) ;
#45797 = VECTOR ( 'NONE', #41943, 1000.000000000000000 ) ;
#45798 = DIRECTION ( 'NONE',  ( 1.000000000000000000, 0.000000000000000000, 0.000000000000000000 ) ) ;
#45799 = VECTOR ( 'NONE', #56150, 1000.000000000000114 ) ;
#45800 = ORIENTED_EDGE ( 'NONE', *, *, #5921, .F. ) ;
#45801 = AXIS2_PLACEMENT_3D ( 'NONE', #29874, #2309, #57449 ) ;
#45802 = DIRECTION ( 'NONE',  ( -1.000000000000000000, 3.491481338843133355E-15, 1.836970198721036590E-16 ) ) ;
#45803 = ORIENTED_EDGE ( 'NONE', *, *, #53145, .F. ) ;
#45804 = ORIENTED_EDGE ( 'NONE', *, *, #30918, .F. ) ;
#45805 = LINE ( 'NONE', #57465, #56711 ) ;
#45806 = CARTESIAN_POINT ( 'NONE',  ( 35.89999999999999858, -0.000000000000000000, 20.80000000000000426 ) ) ;
#45807 = EDGE_CURVE ( 'NONE', #4376, #38741, #42816, .T. ) ;
#45808 = DIRECTION ( 'NONE',  ( 0.000000000000000000, 0.000000000000000000, 1.000000000000000000 ) ) ;
#45809 = LINE ( 'NONE', #67394, #51734 ) ;
#45810 = VECTOR ( 'NONE', #64135, 1000.000000000000000 ) ;
#45811 = AXIS2_PLACEMENT_3D ( 'NONE', #8365, #24294, #41248 ) ;
#45812 = CIRCLE ( 'NONE', #69552, 0.1749999999999998224 ) ;
#45813 = EDGE_LOOP ( 'NONE', ( #52796, #21887, #14462, #20227 ) ) ;
#45814 = ORIENTED_EDGE ( 'NONE', *, *, #62202, .T. ) ;
#45815 = EDGE_CURVE ( 'NONE', #43665, #69628, #38038, .T. ) ;
#45816 = DIRECTION ( 'NONE',  ( 0.000000000000000000, 0.000000000000000000, -1.000000000000000000 ) ) ;
#45817 = CARTESIAN_POINT ( 'NONE',  ( -8.130476262117259267, 8.821682069070703847, 54.00000000000000711 ) ) ;
#45818 = VECTOR ( 'NONE', #44697, 1000.000000000000000 ) ;
#45819 = AXIS2_PLACEMENT_3D ( 'NONE', #598, #38092, #21811 ) ;
#45820 = ORIENTED_EDGE ( 'NONE', *, *, #51267, .F. ) ;
#45821 = EDGE_CURVE ( 'NONE', #24533, #6680, #64398, .T. ) ;
#45822 = ORIENTED_EDGE ( 'NONE', *, *, #49222, .F. ) ;
#45823 = ORIENTED_EDGE ( 'NONE', *, *, #59107, .T. ) ;
#45824 = CIRCLE ( 'NONE', #54888, 0.1999999999999987899 ) ;
#45825 = CARTESIAN_POINT ( 'NONE',  ( 7.250000000000004441, 7.450000000000001954, -13.50000000000000178 ) ) ;
#45826 = ADVANCED_FACE ( 'NONE', ( #68992 ), #63700, .T. ) ;
#45828 = ORIENTED_EDGE ( 'NONE', *, *, #30931, .T. ) ;
#45827 = CARTESIAN_POINT ( 'NONE',  ( 41.09999999999999432, -21.00000000000000000, 14.57806571531351914 ) ) ;
#45829 = CARTESIAN_POINT ( 'NONE',  ( -8.750000000000003553, -7.348062532927999158, -5.000000000000000000 ) ) ;
#45830 = AXIS2_PLACEMENT_3D ( 'NONE', #60736, #50816, #51171 ) ;
#45831 = LINE ( 'NONE', #56093, #12562 ) ;
#45832 = VERTEX_POINT ( 'NONE', #31530 ) ;
#45833 = VECTOR ( 'NONE', #59349, 1000.000000000000114 ) ;
#45834 = ORIENTED_EDGE ( 'NONE', *, *, #25342, .T. ) ;
#45835 = ADVANCED_FACE ( 'NONE', ( #69340 ), #26917, .F. ) ;
#45836 = LINE ( 'NONE', #61748, #29249 ) ;
#45837 = CARTESIAN_POINT ( 'NONE',  ( 8.606483450353382025, 4.383466043307719495, 455.0000000000000568 ) ) ;
#45838 = DIRECTION ( 'NONE',  ( 0.000000000000000000, 0.000000000000000000, -1.000000000000000000 ) ) ;
#45839 = CARTESIAN_POINT ( 'NONE',  ( 39.90000000000000568, 0.000000000000000000, 3.447897592003593022E-15 ) ) ;
#45840 = DIRECTION ( 'NONE',  ( 1.836970198721029934E-16, 1.836970198721010706E-16, -1.000000000000000000 ) ) ;
#45841 = PRESENTATION_LAYER_ASSIGNMENT (  '', '', ( #15429 ) ) ;
#45843 = ORIENTED_EDGE ( 'NONE', *, *, #16883, .F. ) ;
#45842 = SURFACE_STYLE_FILL_AREA ( #29926 ) ;
#45844 = EDGE_LOOP ( 'NONE', ( #50435, #64336, #63924, #56725 ) ) ;
#45845 = CARTESIAN_POINT ( 'NONE',  ( 7.250000000000005329, 8.250000000000001776, -8.500000000000000000 ) ) ;
#45846 = LINE ( 'NONE', #18620, #5325 ) ;
#45847 = DIRECTION ( 'NONE',  ( 1.836970198721029934E-16, 1.836970198721010706E-16, -1.000000000000000000 ) ) ;
#45848 = DIRECTION ( 'NONE',  ( 1.000000000000000000, 0.000000000000000000, 0.000000000000000000 ) ) ;
#45849 = CARTESIAN_POINT ( 'NONE',  ( 8.144523737882815695, 9.547976262117185087, 54.00000000000000711 ) ) ;
#45850 = ORIENTED_EDGE ( 'NONE', *, *, #41819, .F. ) ;
#45851 = CARTESIAN_POINT ( 'NONE',  ( 7.000000000000000000, -42.00000000000000000, -15.00000000000000000 ) ) ;
#45852 = CARTESIAN_POINT ( 'NONE',  ( 30.00000000000000000, -16.28999999999710369, -15.00000000000794920 ) ) ;
#45853 = EDGE_CURVE ( 'NONE', #45736, #19628, #15953, .T. ) ;
#45854 = CARTESIAN_POINT ( 'NONE',  ( 9.417013320880792904, -1.866219381641561759, 455.0000000000000568 ) ) ;
#45855 = CARTESIAN_POINT ( 'NONE',  ( 15.50000000000000000, -0.1999999999999999556, 22.50000000000000000 ) ) ;
#45856 = EDGE_CURVE ( 'NONE', #25494, #62779, #43679, .T. ) ;
#45857 = AXIS2_PLACEMENT_3D ( 'NONE', #34642, #9437, #31005 ) ;
#45858 = AXIS2_PLACEMENT_3D ( 'NONE', #3885, #57967, #68226 ) ;
#45859 = VECTOR ( 'NONE', #66084, 1000.000000000000000 ) ;
#45860 = FACE_OUTER_BOUND ( 'NONE', #25102, .T. ) ;
#45861 = LINE ( 'NONE', #24653, #44347 ) ;
#45862 = AXIS2_PLACEMENT_3D ( 'NONE', #18799, #1843, #23420 ) ;
#45863 = AXIS2_PLACEMENT_3D ( 'NONE', #51109, #50754, #35180 ) ;
#45864 = CIRCLE ( 'NONE', #34545, 0.2000000000000005107 ) ;
#45865 = CARTESIAN_POINT ( 'NONE',  ( 34.89999999999999858, 20.60000000000000142, -13.86939075806900057 ) ) ;
#45866 = EDGE_LOOP ( 'NONE', ( #59388, #40053 ) ) ;
#45867 = DIRECTION ( 'NONE',  ( 0.000000000000000000, 0.000000000000000000, -1.000000000000000000 ) ) ;
#45868 = DIRECTION ( 'NONE',  ( 0.000000000000000000, 0.000000000000000000, 1.000000000000000000 ) ) ;
#45869 = ORIENTED_EDGE ( 'NONE', *, *, #46738, .F. ) ;
#45870 = DIRECTION ( 'NONE',  ( 0.000000000000000000, 1.000000000000000000, 0.000000000000000000 ) ) ;
#45871 = DIRECTION ( 'NONE',  ( -1.836970198721029934E-16, 1.836970198721036344E-16, -1.000000000000000000 ) ) ;
#45872 = AXIS2_PLACEMENT_3D ( 'NONE', #53949, #54642, #33743 ) ;
#45873 = CARTESIAN_POINT ( 'NONE',  ( 7.357023737882817827, -4.961189459950063885, 54.00000000000000711 ) ) ;
#45874 = DIRECTION ( 'NONE',  ( 0.000000000000000000, 0.000000000000000000, 1.000000000000000000 ) ) ;
#45875 = ORIENTED_EDGE ( 'NONE', *, *, #63115, .T. ) ;
#45876 = CARTESIAN_POINT ( 'NONE',  ( -6.835476262117330393, -10.50702373788278265, 26.00000000000000000 ) ) ;
#45877 = AXIS2_PLACEMENT_3D ( 'NONE', #3097, #24659, #35963 ) ;
#45878 = ORIENTED_EDGE ( 'NONE', *, *, #32561, .T. ) ;
#45879 = CARTESIAN_POINT ( 'NONE',  ( -7.250000000000000888, 7.450000000000003730, -14.00000000000000000 ) ) ;
#45880 = CARTESIAN_POINT ( 'NONE',  ( 40.90000000000000568, -21.00000000000000000, -16.96999999999999886 ) ) ;
#45881 = ORIENTED_EDGE ( 'NONE', *, *, #43939, .F. ) ;
#45882 = DIRECTION ( 'NONE',  ( 0.000000000000000000, 0.000000000000000000, 1.000000000000000000 ) ) ;
#45883 = ORIENTED_EDGE ( 'NONE', *, *, #52519, .F. ) ;
#45884 = CYLINDRICAL_SURFACE ( 'NONE', #58251, 1.399999999999999245 ) ;
#45885 = ORIENTED_EDGE ( 'NONE', *, *, #53323, .T. ) ;
#45886 = ORIENTED_EDGE ( 'NONE', *, *, #49358, .T. ) ;
#45887 = DIRECTION ( 'NONE',  ( -1.000000000000000000, 0.000000000000000000, 0.000000000000000000 ) ) ;
#45888 = ORIENTED_EDGE ( 'NONE', *, *, #8670, .F. ) ;
#45889 = VERTEX_POINT ( 'NONE', #64735 ) ;
#45890 = ADVANCED_FACE ( 'NONE', ( #60457 ), #386, .F. ) ;
#45891 = DIRECTION ( 'NONE',  ( -1.000000000000000000, 0.000000000000000000, 0.000000000000000000 ) ) ;
#45892 = CARTESIAN_POINT ( 'NONE',  ( -30.00000000000000000, -11.50000000000000000, -11.00000000000000000 ) ) ;
#45893 = CARTESIAN_POINT ( 'NONE',  ( 17.00000000000000000, -17.35230188589299871, 15.35019951917099945 ) ) ;
#45894 = VECTOR ( 'NONE', #29077, 1000.000000000000000 ) ;
#45895 = ORIENTED_EDGE ( 'NONE', *, *, #21381, .F. ) ;
#45896 = ADVANCED_FACE ( 'NONE', ( #6038 ), #27596, .F. ) ;
#45897 = DIRECTION ( 'NONE',  ( 1.000000000000000000, -0.000000000000000000, 0.000000000000000000 ) ) ;
#45899 = DIRECTION ( 'NONE',  ( 1.000000000000000000, 0.000000000000000000, 0.000000000000000000 ) ) ;
#45898 = DIRECTION ( 'NONE',  ( -1.000000000000000000, 0.000000000000000000, 0.000000000000000000 ) ) ;
#45900 = EDGE_LOOP ( 'NONE', ( #16026, #4083, #57539, #64682 ) ) ;
#45902 = EDGE_LOOP ( 'NONE', ( #40233, #11278 ) ) ;
#45901 = DIRECTION ( 'NONE',  ( -1.000000000000000000, 0.000000000000000000, 0.000000000000000000 ) ) ;
#45903 = AXIS2_PLACEMENT_3D ( 'NONE', #3641, #2934, #67641 ) ;
#45904 = EDGE_CURVE ( 'NONE', #32467, #59441, #21943, .T. ) ;
#45905 = ORIENTED_EDGE ( 'NONE', *, *, #45478, .T. ) ;
#45906 = ADVANCED_FACE ( 'NONE', ( #38559 ), #741, .T. ) ;
#45907 = APPLICATION_PROTOCOL_DEFINITION ( 'draft international standard', 'automotive_design', 1998, #49005 ) ;
#45908 = CIRCLE ( 'NONE', #21084, 0.1999999999999996503 ) ;
#45909 = EDGE_CURVE ( 'NONE', #62934, #63019, #39169, .T. ) ;
#45910 = EDGE_CURVE ( 'NONE', #48042, #24514, #8688, .T. ) ;
#45911 = DIRECTION ( 'NONE',  ( 0.000000000000000000, 0.000000000000000000, 1.000000000000000000 ) ) ;
#45912 = ORIENTED_EDGE ( 'NONE', *, *, #42170, .T. ) ;
#45913 = AXIS2_PLACEMENT_3D ( 'NONE', #20740, #4149, #25718 ) ;
#45914 = CIRCLE ( 'NONE', #49324, 1.000000000000001776 ) ;
#45915 = DIRECTION ( 'NONE',  ( -1.000000000000000000, 0.000000000000000000, 0.000000000000000000 ) ) ;
#45916 = ADVANCED_FACE ( 'NONE', ( #22303 ), #6710, .F. ) ;
#45917 = DIRECTION ( 'NONE',  ( 0.000000000000000000, -1.000000000000000000, 0.000000000000000000 ) ) ;
#45918 = AXIS2_PLACEMENT_3D ( 'NONE', #22775, #53934, #32355 ) ;
#45919 = ORIENTED_EDGE ( 'NONE', *, *, #39431, .T. ) ;
#45920 = VERTEX_POINT ( 'NONE', #65091 ) ;
#45921 = VECTOR ( 'NONE', #67600, 1000.000000000000000 ) ;
#45922 = CIRCLE ( 'NONE', #15456, 3.499999999999849454 ) ;
#45923 = CARTESIAN_POINT ( 'NONE',  ( -11.31351654964674402, -7.806483450353324471, 195.0000000000000284 ) ) ;
#45924 = LINE ( 'NONE', #31064, #53819 ) ;
#45925 = VERTEX_POINT ( 'NONE', #28282 ) ;
#45926 = CARTESIAN_POINT ( 'NONE',  ( 8.250000000000005329, -8.249999999999998224, -26.00000000000001066 ) ) ;
#45928 = CIRCLE ( 'NONE', #42506, 0.2000000000000000944 ) ;
#45927 = CARTESIAN_POINT ( 'NONE',  ( -29.25000000000000000, -5.200000000000001066, -11.75000000000000000 ) ) ;
#45929 = CARTESIAN_POINT ( 'NONE',  ( 6.501044194225490180, -2.632023737882825287, 54.00000000000000711 ) ) ;
#45930 = EDGE_LOOP ( 'NONE', ( #34653, #51254, #13043, #63590 ) ) ;
#45931 = VECTOR ( 'NONE', #31875, 1000.000000000000000 ) ;
#45932 = DIRECTION ( 'NONE',  ( -1.000000000000000000, 0.000000000000000000, 0.000000000000000000 ) ) ;
#45933 = LINE ( 'NONE', #67512, #42695 ) ;
#45935 = ORIENTED_EDGE ( 'NONE', *, *, #24931, .T. ) ;
#45934 = CARTESIAN_POINT ( 'NONE',  ( 106.4257688009193430, 0.000000000000000000, 330.9830310981789694 ) ) ;
#45937 = EDGE_LOOP ( 'NONE', ( #35798, #48986, #65137, #1120, #15222, #68862, #31334, #14391, #68511, #26830, #35968, #3249, #59377, #17745, #53858 ) ) ;
#45936 = DIRECTION ( 'NONE',  ( -1.000000000000000000, 0.000000000000000000, 0.000000000000000000 ) ) ;
#45938 = DIRECTION ( 'NONE',  ( -1.000000000000000000, 0.000000000000000000, 0.000000000000000000 ) ) ;
#45939 = CARTESIAN_POINT ( 'NONE',  ( 283.0000000000000568, -21.00000000000000000, -12.50000000000000000 ) ) ;
#45940 = LINE ( 'NONE', #29665, #51646 ) ;
#45941 = PLANE ( 'NONE',  #20394 ) ;
#45942 = DIRECTION ( 'NONE',  ( -0.000000000000000000, 3.673940397442059868E-16, -1.000000000000000000 ) ) ;
#45943 = ORIENTED_EDGE ( 'NONE', *, *, #16480, .F. ) ;
#45944 = FACE_OUTER_BOUND ( 'NONE', #9475, .T. ) ;
#45945 = PLANE ( 'NONE',  #36075 ) ;
#45946 = LINE ( 'NONE', #50199, #13009 ) ;
#45948 = ORIENTED_EDGE ( 'NONE', *, *, #69535, .T. ) ;
#45947 = DIRECTION ( 'NONE',  ( 0.000000000000000000, -1.000000000000000000, 0.000000000000000000 ) ) ;
#45949 = EDGE_CURVE ( 'NONE', #57533, #64711, #16633, .T. ) ;
#45950 = DIRECTION ( 'NONE',  ( 0.000000000000000000, 0.000000000000000000, 1.000000000000000000 ) ) ;
#45951 =( GEOMETRIC_REPRESENTATION_CONTEXT ( 3 ) GLOBAL_UNCERTAINTY_ASSIGNED_CONTEXT ( ( #35923 ) ) GLOBAL_UNIT_ASSIGNED_CONTEXT ( ( #397, #53451, #11339 ) ) REPRESENTATION_CONTEXT ( 'NONE', 'WORKASPACE' ) );
#45952 = ADVANCED_FACE ( 'NONE', ( #44530 ), #28625, .F. ) ;
#45953 = DIRECTION ( 'NONE',  ( -0.000000000000000000, 1.000000000000000000, -0.000000000000000000 ) ) ;
#45954 = EDGE_CURVE ( 'NONE', #41571, #61801, #61776, .T. ) ;
#45955 = ORIENTED_EDGE ( 'NONE', *, *, #35433, .F. ) ;
#45956 = ORIENTED_EDGE ( 'NONE', *, *, #34444, .T. ) ;
#45957 = DIRECTION ( 'NONE',  ( 1.000000000000000000, -0.000000000000000000, -0.000000000000000000 ) ) ;
#45958 = LINE ( 'NONE', #3184, #52032 ) ;
#45960 = EDGE_LOOP ( 'NONE', ( #38143, #22042, #56410, #69347 ) ) ;
#45959 = EDGE_CURVE ( 'NONE', #47586, #61728, #38893, .T. ) ;
#45961 = LINE ( 'NONE', #3187, #47035 ) ;
#45962 = AXIS2_PLACEMENT_3D ( 'NONE', #28206, #12614, #17931 ) ;
#45963 = VECTOR ( 'NONE', #53693, 1000.000000000000000 ) ;
#45964 = DIRECTION ( 'NONE',  ( -1.000000000000000000, 0.000000000000000000, 0.000000000000000000 ) ) ;
#45965 = DIRECTION ( 'NONE',  ( -1.836970198721029934E-16, 1.836970198721036590E-16, -1.000000000000000000 ) ) ;
#45966 = AXIS2_PLACEMENT_3D ( 'NONE', #36223, #57791, #39006 ) ;
#45968 = CARTESIAN_POINT ( 'NONE',  ( 84.77321854994620765, 47.95351654967443977, 29.00000000000000000 ) ) ;
#45967 = AXIS2_PLACEMENT_3D ( 'NONE', #28780, #45043, #12517 ) ;
#45969 = ORIENTED_EDGE ( 'NONE', *, *, #58241, .F. ) ;
#45970 = CARTESIAN_POINT ( 'NONE',  ( 6.849523737882817542, -10.50702373788282529, 54.00000000000000711 ) ) ;
#45971 = PLANE ( 'NONE',  #23906 ) ;
#45972 = VERTEX_POINT ( 'NONE', #33589 ) ;
#45973 = LINE ( 'NONE', #29008, #65269 ) ;
#45974 = VECTOR ( 'NONE', #62490, 1000.000000000000000 ) ;
#45975 = CARTESIAN_POINT ( 'NONE',  ( 7.000000000000000000, -26.42999999999999972, -9.412893218813501051 ) ) ;
#45976 = DIRECTION ( 'NONE',  ( 0.000000000000000000, 0.000000000000000000, -1.000000000000000000 ) ) ;
#45977 = ORIENTED_EDGE ( 'NONE', *, *, #21418, .F. ) ;
#45978 = VERTEX_POINT ( 'NONE', #12346 ) ;
#45979 = DIRECTION ( 'NONE',  ( -0.000000000000000000, 3.673940397442059868E-16, -1.000000000000000000 ) ) ;
#45980 = ORIENTED_EDGE ( 'NONE', *, *, #60608, .T. ) ;
#45981 = VERTEX_POINT ( 'NONE', #65433 ) ;
#45982 = CIRCLE ( 'NONE', #36980, 3.499999999999850342 ) ;
#45983 = EDGE_CURVE ( 'NONE', #20681, #29049, #59023, .T. ) ;
#45984 = LINE ( 'NONE', #8135, #60839 ) ;
#45985 = CYLINDRICAL_SURFACE ( 'NONE', #31321, 2.204799999999997873 ) ;
#45986 = DIRECTION ( 'NONE',  ( -1.000000000000000000, 0.000000000000000000, 0.000000000000000000 ) ) ;
#45987 = CARTESIAN_POINT ( 'NONE',  ( -8.598420958951637161, -2.005523737882740409, 26.00000000000000711 ) ) ;
#45988 = EDGE_LOOP ( 'NONE', ( #43376, #64583, #20274, #2126 ) ) ;
#45989 = DIRECTION ( 'NONE',  ( 0.000000000000000000, 0.000000000000000000, 1.000000000000000000 ) ) ;
#45991 = DIRECTION ( 'NONE',  ( 0.000000000000000000, -0.9938079899998859545, 0.1111111111112941946 ) ) ;
#45990 = DIRECTION ( 'NONE',  ( 0.000000000000000000, 0.000000000000000000, -1.000000000000000000 ) ) ;
#45992 = ORIENTED_EDGE ( 'NONE', *, *, #20540, .F. ) ;
#45994 = ORIENTED_EDGE ( 'NONE', *, *, #46744, .T. ) ;
#45993 = CARTESIAN_POINT ( 'NONE',  ( 7.250000000000005329, 7.250000000000000888, -26.00000000000001066 ) ) ;
#45995 = ORIENTED_EDGE ( 'NONE', *, *, #65586, .T. ) ;
#45996 = ORIENTED_EDGE ( 'NONE', *, *, #1401, .F. ) ;
#45997 = EDGE_CURVE ( 'NONE', #30310, #68810, #27945, .T. ) ;
#45998 = DIRECTION ( 'NONE',  ( 1.836970198721029934E-16, 1.836970198721010706E-16, -1.000000000000000000 ) ) ;
#45999 = CARTESIAN_POINT ( 'NONE',  ( 15.50000000000000000, -2.500000000000000000, -23.94337567297399971 ) ) ;
#46000 = EDGE_CURVE ( 'NONE', #35196, #21984, #43161, .T. ) ;
#46001 = EDGE_LOOP ( 'NONE', ( #4610, #14116, #43827, #36240, #65309, #5878 ) ) ;
#46002 = AXIS2_PLACEMENT_3D ( 'NONE', #16915, #48401, #59355 ) ;
#46003 = ORIENTED_EDGE ( 'NONE', *, *, #26580, .T. ) ;
#46004 = CARTESIAN_POINT ( 'NONE',  ( 0.000000000000000000, 0.000000000000000000, -10.50000000000000000 ) ) ;
#46005 = CARTESIAN_POINT ( 'NONE',  ( -10.08346604330787777, 9.293516549646602343, 455.0000000000000568 ) ) ;
#46006 = ORIENTED_EDGE ( 'NONE', *, *, #48403, .F. ) ;
#46007 = VERTEX_POINT ( 'NONE', #22639 ) ;
#46008 = AXIS2_PLACEMENT_3D ( 'NONE', #50534, #40616, #30365 ) ;
#46009 = CIRCLE ( 'NONE', #1547, 2.204799999999999205 ) ;
#46011 = PLANE ( 'NONE',  #27424 ) ;
#46010 = VECTOR ( 'NONE', #13498, 1000.000000000000000 ) ;
#46012 = CARTESIAN_POINT ( 'NONE',  ( 276.8775010008008053, -21.00000000000000000, -17.50000000000000000 ) ) ;
#46013 = VERTEX_POINT ( 'NONE', #10993 ) ;
#46014 = VECTOR ( 'NONE', #55540, 1000.000000000000000 ) ;
#46015 = CIRCLE ( 'NONE', #2001, 2.204799999999997873 ) ;
#46016 = CARTESIAN_POINT ( 'NONE',  ( 10.50702373788280752, 6.835476262117182067, 54.00000000000000711 ) ) ;
#46017 = CARTESIAN_POINT ( 'NONE',  ( -1.853252480934758584, 9.404046420173985510, 195.0000000000000284 ) ) ;
#46018 = DIRECTION ( 'NONE',  ( 0.000000000000000000, 0.000000000000000000, 1.000000000000000000 ) ) ;
#46020 = VERTEX_POINT ( 'NONE', #55167 ) ;
#46019 = CARTESIAN_POINT ( 'NONE',  ( 283.0000000000000568, -26.50000000000000000, -0.5000000000000000000 ) ) ;
#46021 = VERTEX_POINT ( 'NONE', #35668 ) ;
#46022 = CARTESIAN_POINT ( 'NONE',  ( 31.89999999999999858, 0.000000000000000000, 0.000000000000000000 ) ) ;
#46023 = AXIS2_PLACEMENT_3D ( 'NONE', #141, #42911, #58502 ) ;
#46024 = LINE ( 'NONE', #1837, #24417 ) ;
#46025 = VECTOR ( 'NONE', #46586, 1000.000000000000000 ) ;
#46026 = DIRECTION ( 'NONE',  ( -1.000000000000000000, 0.000000000000000000, 0.000000000000000000 ) ) ;
#46027 = DIRECTION ( 'NONE',  ( 1.000000000000000000, -0.000000000000000000, 0.000000000000000000 ) ) ;
#46028 = CARTESIAN_POINT ( 'NONE',  ( 39.00000000000000000, 16.96999999999999886, 21.00000000000000000 ) ) ;
#46029 = CARTESIAN_POINT ( 'NONE',  ( 22.14589803375000088, -17.50000000000000000, -21.50000000000000000 ) ) ;
#46030 = CARTESIAN_POINT ( 'NONE',  ( 11.00000000000000000, -17.35230188589299871, -15.35019951917099945 ) ) ;
#46031 = ORIENTED_EDGE ( 'NONE', *, *, #25034, .T. ) ;
#46032 = PLANE ( 'NONE',  #34888 ) ;
#46034 = ORIENTED_EDGE ( 'NONE', *, *, #15980, .F. ) ;
#46033 = DIRECTION ( 'NONE',  ( 0.000000000000000000, 0.000000000000000000, 1.000000000000000000 ) ) ;
#46035 = AXIS2_PLACEMENT_3D ( 'NONE', #10128, #3421, #8728 ) ;
#46036 = DIRECTION ( 'NONE',  ( 1.000000000000000000, -0.000000000000000000, 0.000000000000000000 ) ) ;
#46037 = DIRECTION ( 'NONE',  ( -1.000000000000000000, 0.000000000000000000, 0.000000000000000000 ) ) ;
#46038 = CARTESIAN_POINT ( 'NONE',  ( 78.77321854994620765, 47.95351654967443977, 20.00000000000000000 ) ) ;
#46039 = EDGE_CURVE ( 'NONE', #54618, #62633, #45982, .T. ) ;
#46040 = CARTESIAN_POINT ( 'NONE',  ( 25.57999999999999829, 0.000000000000000000, 2.458500000000000796 ) ) ;
#46041 = CARTESIAN_POINT ( 'NONE',  ( 49.00000000000000000, -21.00000000000000000, 13.86939075806900057 ) ) ;
#46042 = ORIENTED_EDGE ( 'NONE', *, *, #54380, .F. ) ;
#46043 = LINE ( 'NONE', #56649, #39242 ) ;
#46044 = DIRECTION ( 'NONE',  ( -1.000000000000000000, 0.000000000000000000, 0.000000000000000000 ) ) ;
#46046 = ORIENTED_EDGE ( 'NONE', *, *, #62759, .T. ) ;
#46045 = EDGE_CURVE ( 'NONE', #54282, #55886, #18887, .T. ) ;
#46047 = CARTESIAN_POINT ( 'NONE',  ( 6.501044194225490180, -3.157023737882824754, 54.00000000000000711 ) ) ;
#46048 = CARTESIAN_POINT ( 'NONE',  ( 5.793274621760835963, 6.344366288193353576, 26.00000000000000711 ) ) ;
#46049 = ORIENTED_EDGE ( 'NONE', *, *, #48994, .T. ) ;
#46050 = CARTESIAN_POINT ( 'NONE',  ( 146.5599459900709860, 9.000000000000001776, 320.8239988703753056 ) ) ;
#46051 = EDGE_LOOP ( 'NONE', ( #57012, #63583, #49232, #41919 ) ) ;
#46052 = MECHANICAL_DESIGN_GEOMETRIC_PRESENTATION_REPRESENTATION (  '', ( #49448 ), #64159 ) ;
#46053 = EDGE_LOOP ( 'NONE', ( #34468, #16683, #30005, #50650 ) ) ;
#46054 = DIRECTION ( 'NONE',  ( 0.000000000000000000, 0.5017180897718488408, -0.8650311892618017806 ) ) ;
#46055 = PLANE ( 'NONE',  #63582 ) ;
#46056 = DIRECTION ( 'NONE',  ( -0.4285714285711681448, 0.000000000000000000, -0.9035079029053748600 ) ) ;
#46057 = LINE ( 'NONE', #66578, #41076 ) ;
#46058 = ADVANCED_FACE ( 'NONE', ( #66459, #67859 ), #45226, .T. ) ;
#46059 = DIRECTION ( 'NONE',  ( 1.000000000000000000, -8.540177112501197482E-15, 0.000000000000000000 ) ) ;
#46060 = ORIENTED_EDGE ( 'NONE', *, *, #46818, .T. ) ;
#46061 = EDGE_LOOP ( 'NONE', ( #52825, #16780, #30885, #28687 ) ) ;
#46063 = VERTEX_POINT ( 'NONE', #51237 ) ;
#46062 = LINE ( 'NONE', #2227, #23816 ) ;
#46064 = ORIENTED_EDGE ( 'NONE', *, *, #67241, .F. ) ;
#46065 = VECTOR ( 'NONE', #22926, 1000.000000000000000 ) ;
#46066 = DIRECTION ( 'NONE',  ( -1.000000000000000000, 0.000000000000000000, 0.000000000000000000 ) ) ;
#46067 = CARTESIAN_POINT ( 'NONE',  ( 35.89999999999999858, 0.000000000000000000, 0.000000000000000000 ) ) ;
#46068 = DIRECTION ( 'NONE',  ( 1.836970198721029934E-16, -1.836970198721036344E-16, 1.000000000000000000 ) ) ;
#46069 = LINE ( 'NONE', #19899, #17296 ) ;
#46070 = CIRCLE ( 'NONE', #55119, 0.1749999999999980738 ) ;
#46072 = CARTESIAN_POINT ( 'NONE',  ( -7.517976262117260333, 3.834182069070703580, 54.00000000000000711 ) ) ;
#46071 = AXIS2_PLACEMENT_3D ( 'NONE', #10095, #41909, #37662 ) ;
#46073 = CARTESIAN_POINT ( 'NONE',  ( -11.75000000000000000, -5.000000000000000000, 26.25000000000000000 ) ) ;
#46074 = ORIENTED_EDGE ( 'NONE', *, *, #56854, .T. ) ;
#46075 = VERTEX_POINT ( 'NONE', #40283 ) ;
#46076 = ORIENTED_EDGE ( 'NONE', *, *, #10403, .T. ) ;
#46077 = ORIENTED_EDGE ( 'NONE', *, *, #45478, .F. ) ;
#46078 = CARTESIAN_POINT ( 'NONE',  ( 3.606483450353354048, 5.993516549646638047, 195.0000000000000284 ) ) ;
#46079 = CARTESIAN_POINT ( 'NONE',  ( 11.00000000000000000, -17.00000000000000000, -15.70499999999969809 ) ) ;
#46080 = EDGE_CURVE ( 'NONE', #2041, #62471, #24014, .T. ) ;
#46081 =( NAMED_UNIT ( * ) PLANE_ANGLE_UNIT ( ) SI_UNIT ( $, .RADIAN. ) );
#46082 = AXIS2_PLACEMENT_3D ( 'NONE', #36938, #8987, #57432 ) ;
#46083 = DIRECTION ( 'NONE',  ( 0.000000000000000000, 3.673940397442059868E-16, -1.000000000000000000 ) ) ;
#46084 = EDGE_CURVE ( 'NONE', #48981, #29034, #66796, .T. ) ;
#46085 = ORIENTED_EDGE ( 'NONE', *, *, #19729, .T. ) ;
#46086 = VERTEX_POINT ( 'NONE', #13051 ) ;
#46087 = ADVANCED_FACE ( 'NONE', ( #19411 ), #18349, .F. ) ;
#46088 = ORIENTED_EDGE ( 'NONE', *, *, #69008, .F. ) ;
#46089 = CARTESIAN_POINT ( 'NONE',  ( 24.00000000000000000, -16.64230188589299786, -14.64519951917100116 ) ) ;
#46090 = ORIENTED_EDGE ( 'NONE', *, *, #42893, .T. ) ;
#46091 = ADVANCED_FACE ( 'NONE', ( #46283 ), #67153, .F. ) ;
#46092 = ORIENTED_EDGE ( 'NONE', *, *, #10466, .T. ) ;
#46093 = LINE ( 'NONE', #67660, #7337 ) ;
#46095 = EDGE_LOOP ( 'NONE', ( #32248, #69489, #27403, #19662 ) ) ;
#46094 = EDGE_CURVE ( 'NONE', #20214, #29928, #18713, .T. ) ;
#46096 = ORIENTED_EDGE ( 'NONE', *, *, #40054, .F. ) ;
#46098 = EDGE_CURVE ( 'NONE', #6078, #39010, #17773, .T. ) ;
#46097 = DIRECTION ( 'NONE',  ( 0.000000000000000000, -0.7071067811865875408, 0.7071067811865076047 ) ) ;
#46099 = EDGE_CURVE ( 'NONE', #44854, #54026, #4218, .T. ) ;
#46101 = EDGE_LOOP ( 'NONE', ( #15731, #7680, #25584, #51658 ) ) ;
#46100 = CARTESIAN_POINT ( 'NONE',  ( -7.415254214038336400, 2.993516549646603853, 195.0000000000000284 ) ) ;
#46103 = EDGE_LOOP ( 'NONE', ( #16330, #60742, #36503, #23230, #39800, #44981, #40073, #53471 ) ) ;
#46102 = EDGE_CURVE ( 'NONE', #55318, #61234, #61483, .T. ) ;
#46104 = DIRECTION ( 'NONE',  ( 0.000000000000000000, -1.000000000000000000, 0.000000000000000000 ) ) ;
#46105 = DIRECTION ( 'NONE',  ( 0.000000000000000000, 0.000000000000000000, 1.000000000000000000 ) ) ;
#46106 = FACE_OUTER_BOUND ( 'NONE', #46918, .T. ) ;
#46108 = EDGE_LOOP ( 'NONE', ( #27650, #60588, #40758, #39374, #38491, #65535, #24703, #8049 ) ) ;
#46107 = DIRECTION ( 'NONE',  ( 1.836970198721029934E-16, 1.836970198721010706E-16, -1.000000000000000000 ) ) ;
#46109 = ORIENTED_EDGE ( 'NONE', *, *, #11141, .T. ) ;
#46110 = DIRECTION ( 'NONE',  ( -1.084202172485504434E-16, 1.000000000000000000, 0.000000000000000000 ) ) ;
#46111 = CARTESIAN_POINT ( 'NONE',  ( 30.00000000000000000, -12.00000000000000000, 12.20000000000000107 ) ) ;
#46112 = DIRECTION ( 'NONE',  ( 0.000000000000000000, 1.000000000000000000, -0.000000000000000000 ) ) ;
#46113 = ORIENTED_EDGE ( 'NONE', *, *, #1028, .F. ) ;
#46114 = CARTESIAN_POINT ( 'NONE',  ( 7.969523737882818537, -9.562023737882809016, 26.00000000000000000 ) ) ;
#46115 = AXIS2_PLACEMENT_3D ( 'NONE', #4515, #26080, #57540 ) ;
#46116 = CARTESIAN_POINT ( 'NONE',  ( 7.250000000000004441, 7.450000000000001954, -18.00000000000000000 ) ) ;
#46117 = LINE ( 'NONE', #34097, #65050 ) ;
#46118 = EDGE_CURVE ( 'NONE', #14935, #15308, #40975, .T. ) ;
#46119 = ORIENTED_EDGE ( 'NONE', *, *, #12286, .T. ) ;
#46120 = LINE ( 'NONE', #2995, #52823 ) ;
#46121 = CYLINDRICAL_SURFACE ( 'NONE', #8006, 1.621000000000000885 ) ;
#46122 = AXIS2_PLACEMENT_3D ( 'NONE', #34094, #29496, #50370 ) ;
#46123 = CARTESIAN_POINT ( 'NONE',  ( -8.916576262117345664, -8.580623737882765667, 54.00000000000000711 ) ) ;
#46124 = VERTEX_POINT ( 'NONE', #28976 ) ;
#46125 = CARTESIAN_POINT ( 'NONE',  ( 6.657023737882816761, 9.897976262117193613, 54.00000000000000711 ) ) ;
#46126 = DIRECTION ( 'NONE',  ( -0.000000000000000000, -0.000000000000000000, -1.000000000000000000 ) ) ;
#46127 = AXIS2_PLACEMENT_3D ( 'NONE', #65530, #38656, #20999 ) ;
#46128 = ORIENTED_EDGE ( 'NONE', *, *, #16645, .T. ) ;
#46129 = CARTESIAN_POINT ( 'NONE',  ( 24.90000000000000213, 20.60000000000000142, 13.86939075806900057 ) ) ;
#46130 = DIRECTION ( 'NONE',  ( 5.120954910632640039E-15, 1.000000000000000000, -0.000000000000000000 ) ) ;
#46131 = DIRECTION ( 'NONE',  ( 8.951101527228106186E-17, -1.000000000000000000, 0.000000000000000000 ) ) ;
#46132 = CARTESIAN_POINT ( 'NONE',  ( 25.57999999999999829, 3.010794155703768650E-16, -2.458500000000000796 ) ) ;
#46133 = CARTESIAN_POINT ( 'NONE',  ( 18.89999999999999858, 0.000000000000000000, 1.077467997501122647E-15 ) ) ;
#46135 = ORIENTED_EDGE ( 'NONE', *, *, #64668, .T. ) ;
#46134 = EDGE_CURVE ( 'NONE', #37432, #16302, #45940, .T. ) ;
#46136 = CARTESIAN_POINT ( 'NONE',  ( 7.249999999999995559, 8.250000000000001776, 0.000000000000000000 ) ) ;
#46137 = CARTESIAN_POINT ( 'NONE',  ( 75.42576880091937142, 0.000000000000000000, 285.9830310981789125 ) ) ;
#46138 = DIRECTION ( 'NONE',  ( -0.8660254037844482555, 0.000000000000000000, 0.4999999999999831801 ) ) ;
#46139 = CARTESIAN_POINT ( 'NONE',  ( 283.0000000000000568, -20.50000000000000000, 17.00000000000000000 ) ) ;
#46140 = ADVANCED_FACE ( 'NONE', ( #24725 ), #19066, .T. ) ;
#46141 = DIRECTION ( 'NONE',  ( 0.000000000000000000, 0.7071067811865450192, 0.7071067811865500152 ) ) ;
#46142 = ORIENTED_EDGE ( 'NONE', *, *, #45746, .F. ) ;
#46144 = VERTEX_POINT ( 'NONE', #35307 ) ;
#46143 = CARTESIAN_POINT ( 'NONE',  ( 41.09999999999999432, 20.60000000000000142, 13.86939075806900057 ) ) ;
#46145 = CARTESIAN_POINT ( 'NONE',  ( -9.897976262117257562, 6.817976262117182884, 26.00000000000000711 ) ) ;
#46146 = CARTESIAN_POINT ( 'NONE',  ( -3.834182069070823040, -7.357023737882818715, 54.00000000000000711 ) ) ;
#46147 = LINE ( 'NONE', #67716, #40916 ) ;
#46149 = ORIENTED_EDGE ( 'NONE', *, *, #68324, .T. ) ;
#46148 = EDGE_CURVE ( 'NONE', #37385, #13530, #56886, .T. ) ;
#46150 = CARTESIAN_POINT ( 'NONE',  ( -13.00000000000000178, -17.50000000000000000, -15.70500000000000007 ) ) ;
#46151 = EDGE_CURVE ( 'NONE', #47575, #21656, #51602, .T. ) ;
#46152 = ORIENTED_EDGE ( 'NONE', *, *, #19421, .T. ) ;
#46153 = EDGE_CURVE ( 'NONE', #42109, #23844, #55850, .T. ) ;
#46154 = VECTOR ( 'NONE', #68438, 1000.000000000000000 ) ;
#46155 = EDGE_LOOP ( 'NONE', ( #7816, #56158, #13439, #64777 ) ) ;
#46156 = VERTEX_POINT ( 'NONE', #64309 ) ;
#46157 = LINE ( 'NONE', #56416, #14845 ) ;
#46158 = DIRECTION ( 'NONE',  ( 0.6414496315691539108, -0.7671651518153028704, -2.587583378555131256E-16 ) ) ;
#46159 = DIRECTION ( 'NONE',  ( 0.000000000000000000, 1.000000000000000000, 0.000000000000000000 ) ) ;
#46160 = DIRECTION ( 'NONE',  ( -1.000000000000000000, 0.000000000000000000, 0.000000000000000000 ) ) ;
#46161 = EDGE_CURVE ( 'NONE', #54627, #22368, #15532, .T. ) ;
#46162 = ORIENTED_EDGE ( 'NONE', *, *, #30479, .T. ) ;
#46163 = ORIENTED_EDGE ( 'NONE', *, *, #12904, .F. ) ;
#46164 = CARTESIAN_POINT ( 'NONE',  ( 16.54686605390242349, -0.2715358723599871626, 21.66103272505201716 ) ) ;
#46165 = VECTOR ( 'NONE', #136, 1000.000000000000000 ) ;
#46166 = DIRECTION ( 'NONE',  ( 1.000000000000000000, 0.000000000000000000, 0.000000000000000000 ) ) ;
#46167 = EDGE_LOOP ( 'NONE', ( #10317, #50393, #32891, #17281 ) ) ;
#46168 = ORIENTED_EDGE ( 'NONE', *, *, #32741, .F. ) ;
#46169 = EDGE_LOOP ( 'NONE', ( #47992, #55584, #47634, #5315 ) ) ;
#46170 = VECTOR ( 'NONE', #35694, 1000.000000000000000 ) ;
#46171 = CARTESIAN_POINT ( 'NONE',  ( -7.250000000000001776, -7.249999999999998224, -30.00000000000001066 ) ) ;
#46172 = EDGE_CURVE ( 'NONE', #60418, #11608, #9514, .T. ) ;
#46174 = ORIENTED_EDGE ( 'NONE', *, *, #15362, .T. ) ;
#46173 = CYLINDRICAL_SURFACE ( 'NONE', #606, 0.1999999999999987899 ) ;
#46175 = EDGE_CURVE ( 'NONE', #65210, #68276, #36739, .T. ) ;
#46176 = AXIS2_PLACEMENT_3D ( 'NONE', #61064, #61777, #29944 ) ;
#46177 = FACE_OUTER_BOUND ( 'NONE', #60261, .T. ) ;
#46178 = DIRECTION ( 'NONE',  ( -1.000000000000000000, 0.000000000000000000, 0.000000000000000000 ) ) ;
#46179 = VERTEX_POINT ( 'NONE', #19753 ) ;
#46180 = VERTEX_POINT ( 'NONE', #14472 ) ;
#46181 = AXIS2_PLACEMENT_3D ( 'NONE', #11492, #33072, #18437 ) ;
#46182 = DIRECTION ( 'NONE',  ( -1.000000000000000000, 0.000000000000000000, 0.000000000000000000 ) ) ;
#46183 = CARTESIAN_POINT ( 'NONE',  ( 7.000000000000000000, -20.50000000000000000, -13.00000000000000178 ) ) ;
#46184 = CARTESIAN_POINT ( 'NONE',  ( 10.00000000000000000, -18.00000000000000355, 21.00000000000000000 ) ) ;
#46185 = CARTESIAN_POINT ( 'NONE',  ( 7.250000000000005329, 7.250000000000000888, -26.00000000000001066 ) ) ;
#46186 = LINE ( 'NONE', #3073, #41477 ) ;
#46187 = VERTEX_POINT ( 'NONE', #41680 ) ;
#46188 = ORIENTED_EDGE ( 'NONE', *, *, #7123, .T. ) ;
#46189 = DIRECTION ( 'NONE',  ( 4.121462285523434951E-16, 1.000000000000000000, 3.673940397442059868E-16 ) ) ;
#46190 = CARTESIAN_POINT ( 'NONE',  ( 5.668387132715918320, -8.406483450353393394, 195.0000000000000284 ) ) ;
#46191 = CARTESIAN_POINT ( 'NONE',  ( 23.90000000000000213, -21.00000000000000000, 13.86939075806900057 ) ) ;
#46192 = DIRECTION ( 'NONE',  ( 0.000000000000000000, 0.000000000000000000, 1.000000000000000000 ) ) ;
#46193 = VECTOR ( 'NONE', #21631, 1000.000000000000114 ) ;
#46194 = EDGE_CURVE ( 'NONE', #33821, #64137, #58313, .T. ) ;
#46195 = DIRECTION ( 'NONE',  ( -1.254221251785257574E-14, -1.000000000000000000, -1.836970198721013417E-16 ) ) ;
#46196 = VERTEX_POINT ( 'NONE', #57598 ) ;
#46197 = LINE ( 'NONE', #62820, #26803 ) ;
#46198 = FACE_OUTER_BOUND ( 'NONE', #24658, .T. ) ;
#46199 = DIRECTION ( 'NONE',  ( 0.7071067811865465735, -0.7071067811865485719, 0.000000000000000000 ) ) ;
#46200 = VECTOR ( 'NONE', #56586, 1000.000000000000000 ) ;
#46201 = EDGE_CURVE ( 'NONE', #44787, #33655, #47339, .T. ) ;
#46202 = CARTESIAN_POINT ( 'NONE',  ( 0.000000000000000000, -21.00000000000000000, 5.000000000000000000 ) ) ;
#46203 = DIRECTION ( 'NONE',  ( 1.000000000000000000, -0.000000000000000000, 0.000000000000000000 ) ) ;
#46204 = DIRECTION ( 'NONE',  ( 0.000000000000000000, 0.000000000000000000, -1.000000000000000000 ) ) ;
#46205 = EDGE_CURVE ( 'NONE', #51302, #59628, #52665, .T. ) ;
#46206 = AXIS2_PLACEMENT_3D ( 'NONE', #1762, #32912, #6045 ) ;
#46207 = PLANE ( 'NONE',  #56700 ) ;
#46208 = ORIENTED_EDGE ( 'NONE', *, *, #48606, .T. ) ;
#46209 = LINE ( 'NONE', #20398, #55811 ) ;
#46210 = EDGE_CURVE ( 'NONE', #30360, #23736, #31084, .T. ) ;
#46211 = DIRECTION ( 'NONE',  ( 0.000000000000000000, 0.000000000000000000, -1.000000000000000000 ) ) ;
#46212 = VERTEX_POINT ( 'NONE', #9164 ) ;
#46213 = DIRECTION ( 'NONE',  ( 1.836970198721029934E-16, 1.836970198721010706E-16, -1.000000000000000000 ) ) ;
#46214 = DIRECTION ( 'NONE',  ( -1.000000000000000000, 0.000000000000000000, 0.000000000000000000 ) ) ;
#46215 = CIRCLE ( 'NONE', #55270, 1.000000000000000000 ) ;
#46216 = CARTESIAN_POINT ( 'NONE',  ( -8.079219948824961861, -8.711985858128649340, 54.00000000000000711 ) ) ;
#46217 = DIRECTION ( 'NONE',  ( -1.000000000000000000, 0.000000000000000000, 0.000000000000000000 ) ) ;
#46218 = EDGE_CURVE ( 'NONE', #66965, #53158, #25078, .T. ) ;
#46219 = LINE ( 'NONE', #14041, #47442 ) ;
#46220 = ORIENTED_EDGE ( 'NONE', *, *, #15762, .T. ) ;
#46221 = AXIS2_PLACEMENT_3D ( 'NONE', #41170, #9355, #4759 ) ;
#46222 = CARTESIAN_POINT ( 'NONE',  ( -30.00000000000000000, -11.50000000000100009, 19.50000000000103739 ) ) ;
#46223 = ORIENTED_EDGE ( 'NONE', *, *, #69090, .T. ) ;
#46224 = DIRECTION ( 'NONE',  ( -0.000000000000000000, -0.000000000000000000, -1.000000000000000000 ) ) ;
#46225 = DIRECTION ( 'NONE',  ( 1.000000000000000000, 0.000000000000000000, 0.000000000000000000 ) ) ;
#46227 = ORIENTED_EDGE ( 'NONE', *, *, #15534, .T. ) ;
#46226 = EDGE_CURVE ( 'NONE', #34054, #64, #21177, .T. ) ;
#46228 = DIRECTION ( 'NONE',  ( -0.7071067811865476838, 0.4999999999999997780, -0.4999999999999997780 ) ) ;
#46229 = EDGE_CURVE ( 'NONE', #52964, #2177, #68913, .T. ) ;
#46230 = AXIS2_PLACEMENT_3D ( 'NONE', #28937, #7362, #66764 ) ;
#46231 = ORIENTED_EDGE ( 'NONE', *, *, #23330, .F. ) ;
#46232 = EDGE_CURVE ( 'NONE', #62306, #27562, #41329, .T. ) ;
#46233 = EDGE_CURVE ( 'NONE', #12401, #36748, #20469, .T. ) ;
#46234 = LINE ( 'NONE', #12646, #69506 ) ;
#46235 = ORIENTED_EDGE ( 'NONE', *, *, #38870, .F. ) ;
#46236 = ORIENTED_EDGE ( 'NONE', *, *, #36628, .T. ) ;
#46237 = DIRECTION ( 'NONE',  ( -1.000000000000000000, 0.000000000000000000, 0.000000000000000000 ) ) ;
#46238 = ORIENTED_EDGE ( 'NONE', *, *, #20276, .F. ) ;
#46239 = EDGE_LOOP ( 'NONE', ( #31696, #12500, #43068, #1539 ) ) ;
#46240 = EDGE_CURVE ( 'NONE', #46180, #10693, #50471, .T. ) ;
#46241 = CARTESIAN_POINT ( 'NONE',  ( -15.50000000000000000, -5.000000000000000000, 22.50000000000000000 ) ) ;
#46242 = CARTESIAN_POINT ( 'NONE',  ( -11.00000000000000000, -5.200000000000001066, 60.00000000000000000 ) ) ;
#46243 = DIRECTION ( 'NONE',  ( -1.047444401652939849E-14, -1.000000000000000000, -1.836970198721029934E-16 ) ) ;
#46244 = AXIS2_PLACEMENT_3D ( 'NONE', #20876, #68971, #47058 ) ;
#46245 = ORIENTED_EDGE ( 'NONE', *, *, #23325, .F. ) ;
#46246 = DIRECTION ( 'NONE',  ( 0.000000000000000000, 1.000000000000000000, 0.000000000000000000 ) ) ;
#46248 = LINE ( 'NONE', #35270, #46879 ) ;
#46247 = DIRECTION ( 'NONE',  ( 1.000000000000000000, 0.000000000000000000, -0.000000000000000000 ) ) ;
#46249 = ORIENTED_EDGE ( 'NONE', *, *, #11006, .F. ) ;
#46251 = ORIENTED_EDGE ( 'NONE', *, *, #12982, .T. ) ;
#46250 = DIRECTION ( 'NONE',  ( -0.7071067811865560104, -0.7071067811865391350, -2.597868168706466792E-16 ) ) ;
#46252 = ORIENTED_EDGE ( 'NONE', *, *, #40844, .T. ) ;
#46253 = SHAPE_DEFINITION_REPRESENTATION ( #33517, #25847 ) ;
#46254 = LINE ( 'NONE', #62503, #6253 ) ;
#46255 = EDGE_CURVE ( 'NONE', #13915, #47971, #57944, .T. ) ;
#46256 = AXIS2_PLACEMENT_3D ( 'NONE', #39117, #2674, #29894 ) ;
#46258 = ORIENTED_EDGE ( 'NONE', *, *, #37009, .T. ) ;
#46257 = LINE ( 'NONE', #8784, #37645 ) ;
#46259 = EDGE_CURVE ( 'NONE', #30300, #17757, #48278, .T. ) ;
#46260 = LINE ( 'NONE', #56518, #4361 ) ;
#46261 = DIRECTION ( 'NONE',  ( 3.540251991789405856E-15, 1.000000000000000000, 0.000000000000000000 ) ) ;
#46262 = ORIENTED_EDGE ( 'NONE', *, *, #67515, .T. ) ;
#46263 = VERTEX_POINT ( 'NONE', #63969 ) ;
#46264 = VECTOR ( 'NONE', #55518, 1000.000000000000000 ) ;
#46265 = DIRECTION ( 'NONE',  ( 0.000000000000000000, 0.000000000000000000, 1.000000000000000000 ) ) ;
#46266 = ORIENTED_EDGE ( 'NONE', *, *, #43131, .T. ) ;
#46267 = AXIS2_PLACEMENT_3D ( 'NONE', #8649, #30920, #3346 ) ;
#46268 = DIRECTION ( 'NONE',  ( 1.000000000000000000, -0.000000000000000000, -0.000000000000000000 ) ) ;
#46269 = DIRECTION ( 'NONE',  ( -1.000000000000000000, 0.000000000000000000, 0.000000000000000000 ) ) ;
#46270 = CARTESIAN_POINT ( 'NONE',  ( -8.566576262117358453, -9.703773737882738004, 54.00000000000000711 ) ) ;
#46271 = ORIENTED_EDGE ( 'NONE', *, *, #11601, .T. ) ;
#46272 = CIRCLE ( 'NONE', #15803, 1.399999999999998579 ) ;
#46273 = B_SPLINE_CURVE_WITH_KNOTS ( 'NONE', 3,
 ( #41376, #51998, #30777, #8492, #25473, #52348 ),
 .UNSPECIFIED., .F., .F.,
 ( 4, 2, 4 ),
 ( 0.0002380763768131538560, 0.7291065797294589146, 1.457975083082104550 ),
 .UNSPECIFIED. ) ;
#46274 = CARTESIAN_POINT ( 'NONE',  ( -8.916576262117258622, 10.03972626211718477, 26.00000000000000711 ) ) ;
#46275 = DIRECTION ( 'NONE',  ( 0.000000000000000000, 1.000000000000000000, 0.000000000000000000 ) ) ;
#46277 = ORIENTED_EDGE ( 'NONE', *, *, #11202, .T. ) ;
#46276 = SURFACE_STYLE_FILL_AREA ( #57242 ) ;
#46279 = ORIENTED_EDGE ( 'NONE', *, *, #23521, .F. ) ;
#46278 = CARTESIAN_POINT ( 'NONE',  ( 30.00000000000000000, -17.50000000000000000, -15.70500000000000007 ) ) ;
#46280 = LINE ( 'NONE', #67519, #33999 ) ;
#46281 = VECTOR ( 'NONE', #16382, 1000.000000000000000 ) ;
#46282 = CARTESIAN_POINT ( 'NONE',  ( -24.00000000000000000, -15.50000000000000000, -19.33772233983200195 ) ) ;
#46283 = FACE_OUTER_BOUND ( 'NONE', #59024, .T. ) ;
#46284 = DIRECTION ( 'NONE',  ( 1.819560449471430698E-15, 1.000000000000000000, 1.836970198721032892E-16 ) ) ;
#46285 = FACE_OUTER_BOUND ( 'NONE', #9979, .T. ) ;
#46286 = VERTEX_POINT ( 'NONE', #37095 ) ;
#46287 = LINE ( 'NONE', #35674, #56053 ) ;
#46288 = CARTESIAN_POINT ( 'NONE',  ( 49.00000000000000000, -0.2000000000089119934, -8.913009219568841313E-12 ) ) ;
#46289 = CARTESIAN_POINT ( 'NONE',  ( -15.50000000000000000, -2.500000000000000000, 23.94337567297399971 ) ) ;
#46290 = EDGE_CURVE ( 'NONE', #62792, #16263, #53357, .T. ) ;
#46292 = ORIENTED_EDGE ( 'NONE', *, *, #40732, .F. ) ;
#46291 = LINE ( 'NONE', #62915, #26600 ) ;
#46293 = DIRECTION ( 'NONE',  ( 1.000000000000000000, 0.000000000000000000, 0.000000000000000000 ) ) ;
#46294 = VECTOR ( 'NONE', #65989, 1000.000000000000000 ) ;
#46295 = CARTESIAN_POINT ( 'NONE',  ( 0.000000000000000000, 9.000000000000001776, 0.000000000000000000 ) ) ;
#46296 = ADVANCED_FACE ( 'NONE', ( #51952 ), #31790, .F. ) ;
#46297 = ORIENTED_EDGE ( 'NONE', *, *, #52966, .F. ) ;
#46298 = VERTEX_POINT ( 'NONE', #30379 ) ;
#46299 = CARTESIAN_POINT ( 'NONE',  ( 28.00000000000000000, -16.28999999999710369, -14.50000000000000000 ) ) ;
#46300 = ADVANCED_FACE ( 'NONE', ( #60363 ), #27513, .F. ) ;
#46301 = CARTESIAN_POINT ( 'NONE',  ( -23.48000000000000043, -17.50000000000000000, 26.00000000000000355 ) ) ;
#46302 = EDGE_CURVE ( 'NONE', #21517, #43460, #67442, .T. ) ;
#46303 = EDGE_LOOP ( 'NONE', ( #51566, #24491, #25454, #52024 ) ) ;
#46304 = DIRECTION ( 'NONE',  ( 1.000000000000000000, -7.808916176531286882E-15, -2.868949260119708725E-30 ) ) ;
#46305 = CARTESIAN_POINT ( 'NONE',  ( 20.90000000000000213, 20.60000000000000142, 13.86939075806900057 ) ) ;
#46306 = EDGE_CURVE ( 'NONE', #58955, #1307, #14397, .T. ) ;
#46307 = EDGE_CURVE ( 'NONE', #29826, #29082, #53935, .T. ) ;
#46308 = LINE ( 'NONE', #39935, #44002 ) ;
#46309 = AXIS2_PLACEMENT_3D ( 'NONE', #43643, #513, #60585 ) ;
#46310 = CARTESIAN_POINT ( 'NONE',  ( 0.000000000000000000, 0.000000000000000000, 0.000000000000000000 ) ) ;
#46311 = ORIENTED_EDGE ( 'NONE', *, *, #60597, .F. ) ;
#46312 = DIRECTION ( 'NONE',  ( 1.836970198721029934E-16, 1.836970198721010706E-16, -1.000000000000000000 ) ) ;
#46313 = VERTEX_POINT ( 'NONE', #38806 ) ;
#46314 = VERTEX_POINT ( 'NONE', #37781 ) ;
#46315 = VERTEX_POINT ( 'NONE', #6630 ) ;
#46316 = AXIS2_PLACEMENT_3D ( 'NONE', #45852, #50469, #2030 ) ;
#46317 = CARTESIAN_POINT ( 'NONE',  ( 7.806483450353379538, -11.12648345035339226, 195.0000000000000284 ) ) ;
#46318 = AXIS2_PLACEMENT_3D ( 'NONE', #64589, #35967, #31016 ) ;
#46319 = DIRECTION ( 'NONE',  ( -0.6414496315691494699, 0.7671651518153064231, 2.818519042764025305E-16 ) ) ;
#46320 = DIRECTION ( 'NONE',  ( 0.000000000000000000, -1.000000000000000000, 0.000000000000000000 ) ) ;
#46321 = ORIENTED_EDGE ( 'NONE', *, *, #43323, .F. ) ;
#46322 = ORIENTED_EDGE ( 'NONE', *, *, #16939, .T. ) ;
#46323 = CARTESIAN_POINT ( 'NONE',  ( 8.580623737882818958, -9.703773737882825046, 54.00000000000000711 ) ) ;
#46324 = EDGE_LOOP ( 'NONE', ( #45731, #43982, #13078, #4170 ) ) ;
#46325 = VECTOR ( 'NONE', #17017, 1000.000000000000114 ) ;
#46326 = EDGE_LOOP ( 'NONE', ( #41557, #11099, #50824, #13991 ) ) ;
#46327 = DIRECTION ( 'NONE',  ( 0.000000000000000000, -0.1249999999999996531, -0.9921567416492215186 ) ) ;
#46328 = FACE_OUTER_BOUND ( 'NONE', #69118, .T. ) ;
#46329 = DIRECTION ( 'NONE',  ( -1.000000000000000000, 0.000000000000000000, 0.000000000000000000 ) ) ;
#46330 = CARTESIAN_POINT ( 'NONE',  ( 9.899999999999998579, -0.1999999999911795112, 8.826273045769999343E-12 ) ) ;
#46331 = ORIENTED_EDGE ( 'NONE', *, *, #45637, .F. ) ;
#46332 = CARTESIAN_POINT ( 'NONE',  ( 7.616533956692213003, -8.406483450353491094, 455.0000000000000568 ) ) ;
#46333 = AXIS2_PLACEMENT_3D ( 'NONE', #42473, #58033, #31877 ) ;
#46334 = AXIS2_PLACEMENT_3D ( 'NONE', #29902, #3390, #30267 ) ;
#46336 = FACE_OUTER_BOUND ( 'NONE', #12747, .T. ) ;
#46335 = DIRECTION ( 'NONE',  ( 9.912705577010336396E-15, 1.000000000000000000, 0.000000000000000000 ) ) ;
#46337 = ORIENTED_EDGE ( 'NONE', *, *, #57339, .F. ) ;
#46339 = ORIENTED_EDGE ( 'NONE', *, *, #24602, .F. ) ;
#46338 = CYLINDRICAL_SURFACE ( 'NONE', #34173, 0.4000000000000617506 ) ;
#46340 = VERTEX_POINT ( 'NONE', #17235 ) ;
#46341 = ORIENTED_EDGE ( 'NONE', *, *, #10395, .T. ) ;
#46342 = FACE_OUTER_BOUND ( 'NONE', #51748, .T. ) ;
#46343 = ADVANCED_FACE ( 'NONE', ( #22216 ), #38140, .F. ) ;
#46344 = CARTESIAN_POINT ( 'NONE',  ( 6.836383711243005479, -4.149127210878743810, 54.00000000000000711 ) ) ;
#46345 = TOROIDAL_SURFACE ( 'NONE', #5741, 0.06000000000000080963, 0.7500000000000000000 ) ;
#46346 = ORIENTED_EDGE ( 'NONE', *, *, #46390, .F. ) ;
#46347 = VERTEX_POINT ( 'NONE', #21513 ) ;
#46348 = EDGE_CURVE ( 'NONE', #35460, #35302, #1001, .T. ) ;
#46349 = CARTESIAN_POINT ( 'NONE',  ( 30.00000000000000000, -5.200000000000001066, -26.59999999999999787 ) ) ;
#46350 = CARTESIAN_POINT ( 'NONE',  ( 6.006483450353379716, -6.006483450353490738, 455.0000000000000568 ) ) ;
#46351 = ORIENTED_EDGE ( 'NONE', *, *, #26931, .T. ) ;
#46352 = ORIENTED_EDGE ( 'NONE', *, *, #37248, .T. ) ;
#46353 = DIRECTION ( 'NONE',  ( 0.000000000000000000, 0.000000000000000000, 1.000000000000000000 ) ) ;
#46354 = AXIS2_PLACEMENT_3D ( 'NONE', #21941, #58740, #36830 ) ;
#46355 = CARTESIAN_POINT ( 'NONE',  ( 7.450000000000006395, 7.250000000000000888, -25.00000000000000000 ) ) ;
#46356 = CIRCLE ( 'NONE', #27143, 0.2000000000000005107 ) ;
#46357 = VERTEX_POINT ( 'NONE', #1333 ) ;
#46358 = FACE_OUTER_BOUND ( 'NONE', #60774, .T. ) ;
#46359 = CARTESIAN_POINT ( 'NONE',  ( 55.00000000000000000, 16.96999999999999886, -21.00000000000000000 ) ) ;
#46361 = ORIENTED_EDGE ( 'NONE', *, *, #32741, .T. ) ;
#46360 = LINE ( 'NONE', #52377, #1249 ) ;
#46362 = VERTEX_POINT ( 'NONE', #22556 ) ;
#46363 = VECTOR ( 'NONE', #37360, 1000.000000000000000 ) ;
#46364 = CARTESIAN_POINT ( 'NONE',  ( -2.355476262117320640, -9.562023737882825003, 26.00000000000000711 ) ) ;
#46365 = LINE ( 'NONE', #64635, #16603 ) ;
#46366 = CARTESIAN_POINT ( 'NONE',  ( -9.690000000000001279, -8.750000000000000000, -7.000000000000000000 ) ) ;
#46367 = LINE ( 'NONE', #41061, #27872 ) ;
#46368 = CARTESIAN_POINT ( 'NONE',  ( -10.91351654964670992, -2.706483450353338593, 455.0000000000000568 ) ) ;
#46369 = VECTOR ( 'NONE', #52875, 1000.000000000000000 ) ;
#46370 = CARTESIAN_POINT ( 'NONE',  ( 15.50000000000000000, 0.000000000000000000, 26.50000000000000000 ) ) ;
#46371 = DIRECTION ( 'NONE',  ( 0.4999999999989361843, 0.000000000000000000, 0.8660254037850529940 ) ) ;
#46372 = ORIENTED_EDGE ( 'NONE', *, *, #2533, .T. ) ;
#46373 = CARTESIAN_POINT ( 'NONE',  ( 30.00000000000000000, -17.50000000000000000, 26.64999999999999858 ) ) ;
#46374 = VECTOR ( 'NONE', #17104, 1000.000000000000000 ) ;
#46376 = ORIENTED_EDGE ( 'NONE', *, *, #26940, .T. ) ;
#46375 = DIRECTION ( 'NONE',  ( 0.000000000000000000, -3.673940397442059868E-16, 1.000000000000000000 ) ) ;
#46377 = EDGE_CURVE ( 'NONE', #2319, #35777, #20000, .T. ) ;
#46378 = PLANE ( 'NONE',  #22008 ) ;
#46379 = PLANE ( 'NONE',  #69651 ) ;
#46380 = DIRECTION ( 'NONE',  ( -1.000000000000000000, 0.000000000000000000, 0.000000000000000000 ) ) ;
#46381 = AXIS2_PLACEMENT_3D ( 'NONE', #63617, #15175, #5269 ) ;
#46382 = CARTESIAN_POINT ( 'NONE',  ( 105.8309041053263257, 3.657408540445008960, 10.00000000000000000 ) ) ;
#46383 = ORIENTED_EDGE ( 'NONE', *, *, #2195, .T. ) ;
#46384 = DIRECTION ( 'NONE',  ( 0.000000000000000000, -1.000000000000000000, -3.673940397442059868E-16 ) ) ;
#46385 = DIRECTION ( 'NONE',  ( -1.000000000000000000, 0.000000000000000000, 0.000000000000000000 ) ) ;
#46386 = EDGE_CURVE ( 'NONE', #40313, #34713, #68559, .T. ) ;
#46387 = ORIENTED_EDGE ( 'NONE', *, *, #48964, .F. ) ;
#46388 = CARTESIAN_POINT ( 'NONE',  ( 8.000000000000000000, 8.000000000000001776, -1.000000000000000000 ) ) ;
#46389 = EDGE_CURVE ( 'NONE', #63351, #17105, #49437, .T. ) ;
#46390 = EDGE_CURVE ( 'NONE', #10200, #37820, #10906, .T. ) ;
#46391 = LINE ( 'NONE', #53125, #30795 ) ;
#46392 = EDGE_CURVE ( 'NONE', #34424, #57233, #1970, .T. ) ;
#46393 = ORIENTED_EDGE ( 'NONE', *, *, #54332, .T. ) ;
#46394 = CIRCLE ( 'NONE', #57706, 2.000000000000001776 ) ;
#46395 = DIRECTION ( 'NONE',  ( 8.673617379884013384E-15, 1.000000000000000000, 0.000000000000000000 ) ) ;
#46396 = ORIENTED_EDGE ( 'NONE', *, *, #4750, .F. ) ;
#46397 = VERTEX_POINT ( 'NONE', #21857 ) ;
#46398 = FACE_OUTER_BOUND ( 'NONE', #20680, .T. ) ;
#46399 = CARTESIAN_POINT ( 'NONE',  ( 275.5000000000000000, -42.50000000000000000, 26.50000000000000000 ) ) ;
#46400 = DIRECTION ( 'NONE',  ( 0.000000000000000000, -0.1249999999999996531, -0.9921567416492215186 ) ) ;
#46401 = LINE ( 'NONE', #45002, #1555 ) ;
#46402 = CARTESIAN_POINT ( 'NONE',  ( 41.09999999999999432, 20.60000000000000142, -13.86939075806900057 ) ) ;
#46403 = ORIENTED_EDGE ( 'NONE', *, *, #15282, .F. ) ;
#46404 = VERTEX_POINT ( 'NONE', #22893 ) ;
#46405 = AXIS2_PLACEMENT_3D ( 'NONE', #50011, #28439, #67336 ) ;
#46407 = ORIENTED_EDGE ( 'NONE', *, *, #5292, .T. ) ;
#46406 = CARTESIAN_POINT ( 'NONE',  ( 5.257023737882819070, -5.257023737882815517, 26.00000000000000711 ) ) ;
#46408 = ORIENTED_EDGE ( 'NONE', *, *, #29063, .F. ) ;
#46409 = PRODUCT_DEFINITION_SHAPE ( 'NONE', 'NONE',  #11064 ) ;
#46410 = AXIS2_PLACEMENT_3D ( 'NONE', #32980, #49253, #11074 ) ;
#46411 = CARTESIAN_POINT ( 'NONE',  ( 8.250000000000005329, -8.249999999999998224, -26.00000000000001066 ) ) ;
#46412 = CARTESIAN_POINT ( 'NONE',  ( -24.00000000000000000, -15.50000000000000000, -19.33772233983200195 ) ) ;
#46413 = CARTESIAN_POINT ( 'NONE',  ( 6.364920264886851697, 3.663616288756991413, 54.00000000000000711 ) ) ;
#46414 = FACE_BOUND ( 'NONE', #51015, .T. ) ;
#46415 = VECTOR ( 'NONE', #19432, 1000.000000000000114 ) ;
#46416 = CARTESIAN_POINT ( 'NONE',  ( 17.00000000000000000, -15.50000000000000000, 14.50000000000000000 ) ) ;
#46417 = ORIENTED_EDGE ( 'NONE', *, *, #42449, .T. ) ;
#46418 = ORIENTED_EDGE ( 'NONE', *, *, #23715, .F. ) ;
#46419 = ORIENTED_EDGE ( 'NONE', *, *, #60240, .T. ) ;
#46420 = AXIS2_PLACEMENT_3D ( 'NONE', #39699, #67630, #66918 ) ;
#46421 = CIRCLE ( 'NONE', #29591, 0.1999999999999987899 ) ;
#46422 = EDGE_LOOP ( 'NONE', ( #48963, #54180, #19965, #49878 ) ) ;
#46423 = PLANE ( 'NONE',  #12946 ) ;
#46424 = LINE ( 'NONE', #19551, #14063 ) ;
#46425 = VECTOR ( 'NONE', #35799, 1000.000000000000000 ) ;
#46426 = CARTESIAN_POINT ( 'NONE',  ( -5.993516549646776603, -6.006483450353426790, 455.0000000000000568 ) ) ;
#46427 = VECTOR ( 'NONE', #67150, 1000.000000000000000 ) ;
#46428 = ORIENTED_EDGE ( 'NONE', *, *, #13001, .F. ) ;
#46429 = ORIENTED_EDGE ( 'NONE', *, *, #51274, .T. ) ;
#46430 = ORIENTED_EDGE ( 'NONE', *, *, #5144, .F. ) ;
#46431 = ADVANCED_FACE ( 'NONE', ( #32127 ), #644, .F. ) ;
#46432 = ADVANCED_FACE ( 'NONE', ( #298 ), #43417, .T. ) ;
#46433 = EDGE_CURVE ( 'NONE', #23129, #55364, #43778, .T. ) ;
#46435 = CYLINDRICAL_SURFACE ( 'NONE', #50825, 4.000000000000000000 ) ;
#46434 = AXIS2_PLACEMENT_3D ( 'NONE', #59183, #142, #48576 ) ;
#46436 = ORIENTED_EDGE ( 'NONE', *, *, #6506, .F. ) ;
#46437 = VERTEX_POINT ( 'NONE', #33157 ) ;
#46438 = CARTESIAN_POINT ( 'NONE',  ( -7.250000000000000888, 8.250000000000001776, -26.00000000000001066 ) ) ;
#46439 = ADVANCED_FACE ( 'NONE', ( #6289 ), #27863, .T. ) ;
#46440 = ORIENTED_EDGE ( 'NONE', *, *, #13277, .T. ) ;
#46441 = ORIENTED_EDGE ( 'NONE', *, *, #47844, .F. ) ;
#46442 = LINE ( 'NONE', #62700, #55324 ) ;
#46444 = ORIENTED_EDGE ( 'NONE', *, *, #37147, .F. ) ;
#46443 = LINE ( 'NONE', #3315, #25489 ) ;
#46445 = ORIENTED_EDGE ( 'NONE', *, *, #14012, .T. ) ;
#46446 = DIRECTION ( 'NONE',  ( 0.000000000000000000, 0.000000000000000000, 1.000000000000000000 ) ) ;
#46447 = CARTESIAN_POINT ( 'NONE',  ( 15.00000000000000000, -42.50000000000000000, 27.00000000000000000 ) ) ;
#46448 = AXIS2_PLACEMENT_3D ( 'NONE', #68462, #20015, #15761 ) ;
#46449 = CARTESIAN_POINT ( 'NONE',  ( -8.750000000000003553, 7.750000000000001776, 5.000000000000000000 ) ) ;
#46451 = VERTEX_POINT ( 'NONE', #2708 ) ;
#46450 = DIRECTION ( 'NONE',  ( 1.000000000000000000, -0.000000000000000000, -0.000000000000000000 ) ) ;
#46452 = ORIENTED_EDGE ( 'NONE', *, *, #21922, .F. ) ;
#46453 = CARTESIAN_POINT ( 'NONE',  ( 6.501044194225438666, 2.617976262117192032, 26.00000000000000711 ) ) ;
#46454 = DIRECTION ( 'NONE',  ( -0.000000000000000000, -0.000000000000000000, -1.000000000000000000 ) ) ;
#46455 = DIRECTION ( 'NONE',  ( -0.000000000000000000, -0.000000000000000000, -1.000000000000000000 ) ) ;
#46456 = CARTESIAN_POINT ( 'NONE',  ( -4.393516549646667713, 11.77351654964658856, 195.0000000000000284 ) ) ;
#46457 = CIRCLE ( 'NONE', #29494, 4.000000000000000888 ) ;
#46458 = VERTEX_POINT ( 'NONE', #24288 ) ;
#46459 = DIRECTION ( 'NONE',  ( 1.000000000000000000, 0.000000000000000000, 0.000000000000000000 ) ) ;
#46460 = FACE_OUTER_BOUND ( 'NONE', #18769, .T. ) ;
#46461 = AXIS2_PLACEMENT_3D ( 'NONE', #42809, #43153, #53433 ) ;
#46462 = FACE_OUTER_BOUND ( 'NONE', #62235, .T. ) ;
#46463 = ORIENTED_EDGE ( 'NONE', *, *, #11730, .F. ) ;
#46464 = DIRECTION ( 'NONE',  ( -0.7071067811865451302, 0.7071067811865500152, 2.597868168706484541E-16 ) ) ;
#46465 = CARTESIAN_POINT ( 'NONE',  ( 40.90000000000000568, -0.2000000000089119934, -8.913009219568841313E-12 ) ) ;
#46466 = CARTESIAN_POINT ( 'NONE',  ( -17.00000000000000000, -17.50000000000000000, 19.33772233983200195 ) ) ;
#46467 = AXIS2_PLACEMENT_3D ( 'NONE', #28663, #23704, #18749 ) ;
#46468 = AXIS2_PLACEMENT_3D ( 'NONE', #54081, #15204, #21886 ) ;
#46469 = VERTEX_POINT ( 'NONE', #51152 ) ;
#46470 = FACE_OUTER_BOUND ( 'NONE', #21021, .T. ) ;
#46471 = CARTESIAN_POINT ( 'NONE',  ( -11.77351654964679106, -7.606483450353366038, 455.0000000000000568 ) ) ;
#46472 = ADVANCED_FACE ( 'NONE', ( #1662 ), #2024, .T. ) ;
#46473 = ADVANCED_FACE ( 'NONE', ( #61766 ), #61050, .F. ) ;
#46474 = DIRECTION ( 'NONE',  ( 0.000000000000000000, 0.000000000000000000, 1.000000000000000000 ) ) ;
#46475 = ORIENTED_EDGE ( 'NONE', *, *, #33309, .T. ) ;
#46476 = CARTESIAN_POINT ( 'NONE',  ( -3.142976262117267883, -4.046023737882828542, 54.00000000000000711 ) ) ;
#46477 = LINE ( 'NONE', #4063, #61425 ) ;
#46478 = ADVANCED_FACE ( 'NONE', ( #67435 ), #18981, .T. ) ;
#46479 = LINE ( 'NONE', #35880, #65814 ) ;
#46480 = CARTESIAN_POINT ( 'NONE',  ( 8.406483450353379183, -4.396432944014562416, 195.0000000000000284 ) ) ;
#46481 = CARTESIAN_POINT ( 'NONE',  ( 0.9555237378828128625, 9.915476262117220330, 26.00000000000000711 ) ) ;
#46482 = ORIENTED_EDGE ( 'NONE', *, *, #52166, .F. ) ;
#46483 = DIRECTION ( 'NONE',  ( 0.000000000000000000, 0.000000000000000000, 1.000000000000000000 ) ) ;
#46484 = DIRECTION ( 'NONE',  ( 1.000000000000000000, 0.000000000000000000, 0.000000000000000000 ) ) ;
#46485 = ADVANCED_FACE ( 'NONE', ( #7309 ), #60720, .T. ) ;
#46486 = DIRECTION ( 'NONE',  ( -0.5773502691896201799, -0.5773502691896285066, -0.5773502691896285066 ) ) ;
#46487 = DIRECTION ( 'NONE',  ( 0.000000000000000000, 0.5017180897718492849, 0.8650311892618014475 ) ) ;
#46488 = EDGE_CURVE ( 'NONE', #10769, #31506, #34717, .T. ) ;
#46489 = DIRECTION ( 'NONE',  ( 0.000000000000000000, 0.000000000000000000, -1.000000000000000000 ) ) ;
#46490 = ORIENTED_EDGE ( 'NONE', *, *, #27397, .F. ) ;
#46492 = ORIENTED_EDGE ( 'NONE', *, *, #20559, .T. ) ;
#46491 = DIRECTION ( 'NONE',  ( 0.000000000000000000, 0.000000000000000000, 1.000000000000000000 ) ) ;
#46493 = ADVANCED_FACE ( 'NONE', ( #55765 ), #18266, .F. ) ;
#46494 = CARTESIAN_POINT ( 'NONE',  ( 0.5000000000000000000, -42.00000000000000000, -27.00000000000000000 ) ) ;
#46495 = DIRECTION ( 'NONE',  ( 0.000000000000000000, 0.000000000000000000, 1.000000000000000000 ) ) ;
#46496 = CARTESIAN_POINT ( 'NONE',  ( 7.532023737882817649, -3.848229544836346605, 54.00000000000000711 ) ) ;
#46497 = VERTEX_POINT ( 'NONE', #28536 ) ;
#46498 = CARTESIAN_POINT ( 'NONE',  ( -4.383466043307969962, -8.606483450353444198, 455.0000000000000568 ) ) ;
#46499 = ORIENTED_EDGE ( 'NONE', *, *, #45673, .F. ) ;
#46500 = ORIENTED_EDGE ( 'NONE', *, *, #16797, .F. ) ;
#46501 = ORIENTED_EDGE ( 'NONE', *, *, #39732, .F. ) ;
#46502 = CARTESIAN_POINT ( 'NONE',  ( 7.250000000000005329, -7.249999999999998224, -14.50000000000000000 ) ) ;
#46503 = CIRCLE ( 'NONE', #30720, 4.000000000000000888 ) ;
#46504 = DIRECTION ( 'NONE',  ( -1.185108578570163560E-14, -1.000000000000000000, -1.836970198721014650E-16 ) ) ;
#46505 = FACE_OUTER_BOUND ( 'NONE', #28590, .T. ) ;
#46506 = LINE ( 'NONE', #18584, #61870 ) ;
#46507 = ORIENTED_EDGE ( 'NONE', *, *, #45316, .F. ) ;
#46508 = VERTEX_POINT ( 'NONE', #35221 ) ;
#46509 = FACE_OUTER_BOUND ( 'NONE', #24216, .T. ) ;
#46510 = DIRECTION ( 'NONE',  ( -1.000000000000000000, 0.000000000000000000, 0.000000000000000000 ) ) ;
#46511 = ORIENTED_EDGE ( 'NONE', *, *, #64152, .T. ) ;
#46512 = VERTEX_POINT ( 'NONE', #34528 ) ;
#46513 = AXIS2_PLACEMENT_3D ( 'NONE', #46498, #67720, #45095 ) ;
#46514 = AXIS2_PLACEMENT_3D ( 'NONE', #67008, #34827, #51100 ) ;
#46515 = EDGE_CURVE ( 'NONE', #26452, #19555, #4269, .T. ) ;
#46516 = ORIENTED_EDGE ( 'NONE', *, *, #27545, .F. ) ;
#46517 = EDGE_LOOP ( 'NONE', ( #23348, #40930, #33466, #11483, #44726, #26911, #42613, #28358 ) ) ;
#46518 = CARTESIAN_POINT ( 'NONE',  ( 8.211283450353400681, 5.993516549646574099, 455.0000000000000568 ) ) ;
#46519 = UNCERTAINTY_MEASURE_WITH_UNIT (LENGTH_MEASURE( 1.000000000000000082E-05 ), #57798, 'distance_accuracy_value', 'NONE');
#46521 = ORIENTED_EDGE ( 'NONE', *, *, #69316, .F. ) ;
#46520 = CARTESIAN_POINT ( 'NONE',  ( -8.821682069070829968, -8.144523737882765957, 54.00000000000000711 ) ) ;
#46522 = CIRCLE ( 'NONE', #50904, 0.2000000000000005107 ) ;
#46523 = CYLINDRICAL_SURFACE ( 'NONE', #7402, 0.4999999999979499732 ) ;
#46524 = PLANE ( 'NONE',  #49832 ) ;
#46525 = EDGE_LOOP ( 'NONE', ( #8112, #59050, #69052, #52268 ) ) ;
#46526 = ORIENTED_EDGE ( 'NONE', *, *, #67466, .T. ) ;
#46527 = AXIS2_PLACEMENT_3D ( 'NONE', #27189, #64324, #5282 ) ;
#46528 = EDGE_CURVE ( 'NONE', #32475, #31391, #39266, .T. ) ;
#46529 = DIRECTION ( 'NONE',  ( 0.000000000000000000, 0.000000000000000000, 1.000000000000000000 ) ) ;
#46530 = CARTESIAN_POINT ( 'NONE',  ( 30.00000000000000000, -12.00000000000000000, 10.52786404500095863 ) ) ;
#46531 = EDGE_CURVE ( 'NONE', #30152, #29737, #23234, .T. ) ;
#46532 = CARTESIAN_POINT ( 'NONE',  ( 8.250000000000005329, 8.250000000000001776, -26.00000000000001066 ) ) ;
#46533 = PLANE ( 'NONE',  #40296 ) ;
#46534 = LINE ( 'NONE', #68109, #17794 ) ;
#46536 = ORIENTED_EDGE ( 'NONE', *, *, #48950, .T. ) ;
#46535 = CARTESIAN_POINT ( 'NONE',  ( -5.655420232009359616, -8.406483450353428921, 455.0000000000000568 ) ) ;
#46537 = ORIENTED_EDGE ( 'NONE', *, *, #56486, .T. ) ;
#46538 = LINE ( 'NONE', #2365, #35480 ) ;
#46539 = CARTESIAN_POINT ( 'NONE',  ( -11.75000000000000000, -5.000000000000000000, -26.25000000000000000 ) ) ;
#46540 = CARTESIAN_POINT ( 'NONE',  ( -6.661338147750939243E-15, 20.50000000000000000, -17.79289321881346808 ) ) ;
#46541 = LINE ( 'NONE', #52571, #51701 ) ;
#46542 = VECTOR ( 'NONE', #3010, 1000.000000000000000 ) ;
#46543 = EDGE_CURVE ( 'NONE', #30313, #33185, #23579, .T. ) ;
#46544 = CARTESIAN_POINT ( 'NONE',  ( 6.836383711243005479, -4.149127210878734040, 26.00000000000000711 ) ) ;
#46545 = ORIENTED_EDGE ( 'NONE', *, *, #12911, .F. ) ;
#46546 = PLANE ( 'NONE',  #65215 ) ;
#46547 = DIRECTION ( 'NONE',  ( -8.951101527228104953E-17, 1.000000000000000000, 0.000000000000000000 ) ) ;
#46548 = AXIS2_PLACEMENT_3D ( 'NONE', #23232, #66715, #55763 ) ;
#46549 = FACE_OUTER_BOUND ( 'NONE', #13227, .T. ) ;
#46550 = DIRECTION ( 'NONE',  ( 0.000000000000000000, 1.000000000000000000, 0.000000000000000000 ) ) ;
#46551 = EDGE_CURVE ( 'NONE', #37385, #6182, #19326, .T. ) ;
#46552 = DIRECTION ( 'NONE',  ( -1.000000000000000000, 0.000000000000000000, 0.000000000000000000 ) ) ;
#46553 = CARTESIAN_POINT ( 'NONE',  ( -7.798499376344067535, 4.727349090213368576, 455.0000000000000568 ) ) ;
#46554 = DIRECTION ( 'NONE',  ( -0.5000000000000004441, 0.8660254037844383745, 3.181725716174720005E-16 ) ) ;
#46555 = EDGE_LOOP ( 'NONE', ( #11241, #36986, #37864, #64424 ) ) ;
#46556 = CARTESIAN_POINT ( 'NONE',  ( 24.00000000000000000, -17.00000000000000000, -15.70499999999969809 ) ) ;
#46557 = CARTESIAN_POINT ( 'NONE',  ( -1.677516549646676625, 10.73351654964656987, 195.0000000000000284 ) ) ;
#46558 = ORIENTED_EDGE ( 'NONE', *, *, #23177, .T. ) ;
#46559 = LINE ( 'NONE', #9445, #6373 ) ;
#46560 = AXIS2_PLACEMENT_3D ( 'NONE', #43295, #59568, #59218 ) ;
#46561 = DIRECTION ( 'NONE',  ( -1.836970198721029934E-16, 1.836970198721036590E-16, -1.000000000000000000 ) ) ;
#46562 = CARTESIAN_POINT ( 'NONE',  ( 7.250000000000005329, 8.250000000000001776, -26.00000000000001066 ) ) ;
#46563 = SURFACE_STYLE_USAGE ( .BOTH. , #24307 ) ;
#46564 = EDGE_CURVE ( 'NONE', #23831, #5664, #39491, .T. ) ;
#46565 = CARTESIAN_POINT ( 'NONE',  ( -4.188533722949369320, -4.740315990920150213, 195.0000000000000284 ) ) ;
#46566 = ORIENTED_EDGE ( 'NONE', *, *, #66489, .T. ) ;
#46567 = ADVANCED_FACE ( 'NONE', ( #29223 ), #50798, .T. ) ;
#46568 = CARTESIAN_POINT ( 'NONE',  ( 6.665817930929297752, -7.357023737882824044, 54.00000000000000711 ) ) ;
#46569 = AXIS2_PLACEMENT_3D ( 'NONE', #4440, #63472, #19621 ) ;
#46570 = ORIENTED_EDGE ( 'NONE', *, *, #57864, .F. ) ;
#46571 = DIRECTION ( 'NONE',  ( 0.000000000000000000, 0.000000000000000000, 1.000000000000000000 ) ) ;
#46572 = LINE ( 'NONE', #63195, #54857 ) ;
#46573 = ORIENTED_EDGE ( 'NONE', *, *, #45281, .T. ) ;
#46574 = CARTESIAN_POINT ( 'NONE',  ( -11.00000000000000000, -5.200000000000001066, 60.00000000000000000 ) ) ;
#46575 = CIRCLE ( 'NONE', #42096, 4.000000000000000888 ) ;
#46576 = AXIS2_PLACEMENT_3D ( 'NONE', #7157, #55958, #51345 ) ;
#46577 = ADVANCED_FACE ( 'NONE', ( #45488 ), #13324, .T. ) ;
#46578 = EDGE_LOOP ( 'NONE', ( #58064, #47495, #37470, #47461 ) ) ;
#46579 = CARTESIAN_POINT ( 'NONE',  ( -10.91351654964670637, 9.293516549646604119, 195.0000000000000284 ) ) ;
#46580 = ORIENTED_EDGE ( 'NONE', *, *, #64059, .F. ) ;
#46581 = ORIENTED_EDGE ( 'NONE', *, *, #29756, .T. ) ;
#46582 = PLANE ( 'NONE',  #38512 ) ;
#46583 = ORIENTED_EDGE ( 'NONE', *, *, #10665, .T. ) ;
#46584 = ORIENTED_EDGE ( 'NONE', *, *, #29181, .T. ) ;
#46585 = DIRECTION ( 'NONE',  ( 0.000000000000000000, 1.000000000000000000, 0.000000000000000000 ) ) ;
#46586 = DIRECTION ( 'NONE',  ( -1.000000000000000000, 0.000000000000000000, 0.000000000000000000 ) ) ;
#46587 = FACE_OUTER_BOUND ( 'NONE', #54386, .T. ) ;
#46588 = AXIS2_PLACEMENT_3D ( 'NONE', #67930, #30095, #46704 ) ;
#46589 = ORIENTED_EDGE ( 'NONE', *, *, #67049, .F. ) ;
#46590 = CARTESIAN_POINT ( 'NONE',  ( 7.265214908726123078, -5.393625297350022052, 455.0000000000000568 ) ) ;
#46592 = DIRECTION ( 'NONE',  ( -1.836970198721029934E-16, 1.836970198721036344E-16, -1.000000000000000000 ) ) ;
#46591 = CARTESIAN_POINT ( 'NONE',  ( 4.720772854004780861, 4.141586236041042923, 54.00000000000000711 ) ) ;
#46593 = ORIENTED_EDGE ( 'NONE', *, *, #27808, .T. ) ;
#46595 = ORIENTED_EDGE ( 'NONE', *, *, #8605, .T. ) ;
#46594 = DIRECTION ( 'NONE',  ( 0.000000000000000000, 0.000000000000000000, -1.000000000000000000 ) ) ;
#46596 = VECTOR ( 'NONE', #6906, 1000.000000000000000 ) ;
#46597 = EDGE_LOOP ( 'NONE', ( #16620, #2323, #38348, #59675 ) ) ;
#46598 = EDGE_CURVE ( 'NONE', #66948, #3798, #67766, .T. ) ;
#46599 = DIRECTION ( 'NONE',  ( 1.000000000000000000, 0.000000000000000000, 0.000000000000000000 ) ) ;
#46600 = CARTESIAN_POINT ( 'NONE',  ( -11.50000000000000000, -12.00000000000000000, 11.03137303340310282 ) ) ;
#46602 = ORIENTED_EDGE ( 'NONE', *, *, #694, .T. ) ;
#46601 = CARTESIAN_POINT ( 'NONE',  ( 40.90000000000000568, 21.00000000000000000, -16.96999999999999886 ) ) ;
#46603 = EDGE_CURVE ( 'NONE', #45572, #26595, #57855, .T. ) ;
#46604 = DIRECTION ( 'NONE',  ( 1.000000000000000000, 0.000000000000000000, 0.000000000000000000 ) ) ;
#46605 = CARTESIAN_POINT ( 'NONE',  ( -7.813516549646839948, -12.00648345035340903, 455.0000000000000568 ) ) ;
#46606 = ORIENTED_EDGE ( 'NONE', *, *, #38296, .F. ) ;
#46607 = VERTEX_POINT ( 'NONE', #30642 ) ;
#46608 = EDGE_CURVE ( 'NONE', #23311, #45889, #58214, .T. ) ;
#46609 = EDGE_CURVE ( 'NONE', #6695, #13669, #68479, .T. ) ;
#46610 = CARTESIAN_POINT ( 'NONE',  ( 0.000000000000000000, 0.000000000000000000, 0.000000000000000000 ) ) ;
#46611 = ORIENTED_EDGE ( 'NONE', *, *, #43684, .F. ) ;
#46612 = FACE_OUTER_BOUND ( 'NONE', #5584, .T. ) ;
#46613 = CARTESIAN_POINT ( 'NONE',  ( 12.00648345035338060, -7.826483450353395988, 195.0000000000000284 ) ) ;
#46614 = EDGE_CURVE ( 'NONE', #41478, #65577, #57158, .T. ) ;
#46615 = CARTESIAN_POINT ( 'NONE',  ( -14.25000000000000000, -2.500000000000000000, 23.22168783648699986 ) ) ;
#46616 = ORIENTED_EDGE ( 'NONE', *, *, #2810, .F. ) ;
#46617 = CIRCLE ( 'NONE', #64710, 0.1749999999999989342 ) ;
#46618 = CARTESIAN_POINT ( 'NONE',  ( -3.650476262117331228, -10.50702373788281641, 26.00000000000000000 ) ) ;
#46619 = DIRECTION ( 'NONE',  ( 1.000000000000000000, 0.000000000000000000, 0.000000000000000000 ) ) ;
#46620 = EDGE_CURVE ( 'NONE', #18569, #60315, #57506, .T. ) ;
#46622 = EDGE_LOOP ( 'NONE', ( #40398, #36783, #34588, #26082 ) ) ;
#46621 = DIRECTION ( 'NONE',  ( 1.836970198721029934E-16, 1.836970198721010706E-16, -1.000000000000000000 ) ) ;
#46624 = VERTEX_POINT ( 'NONE', #3766 ) ;
#46623 = CARTESIAN_POINT ( 'NONE',  ( 5.257023737882819070, -5.257023737882815517, 26.00000000000000711 ) ) ;
#46625 = EDGE_CURVE ( 'NONE', #14276, #55844, #25707, .T. ) ;
#46627 = CARTESIAN_POINT ( 'NONE',  ( 8.689999999999999503, 9.750000000000001776, -7.000000000000000000 ) ) ;
#46626 = AXIS2_PLACEMENT_3D ( 'NONE', #64580, #37710, #27094 ) ;
#46628 = PRESENTATION_LAYER_ASSIGNMENT (  '', '', ( #22908 ) ) ;
#46629 = CARTESIAN_POINT ( 'NONE',  ( -4.242044687070550602, 8.452095193409279617, 455.0000000000000568 ) ) ;
#46630 = EDGE_CURVE ( 'NONE', #7067, #56499, #41598, .T. ) ;
#46631 = CARTESIAN_POINT ( 'NONE',  ( 7.450000000000006395, 7.250000000000000888, -25.50000000000000355 ) ) ;
#46632 = EDGE_CURVE ( 'NONE', #5665, #36973, #9424, .T. ) ;
#46633 = EDGE_CURVE ( 'NONE', #1993, #11369, #14732, .T. ) ;
#46634 = FACE_OUTER_BOUND ( 'NONE', #18229, .T. ) ;
#46635 = AXIS2_PLACEMENT_3D ( 'NONE', #27779, #53972, #49362 ) ;
#46636 = DIRECTION ( 'NONE',  ( 0.000000000000000000, 0.7096009616570518874, 0.7046037717862339012 ) ) ;
#46637 = ORIENTED_EDGE ( 'NONE', *, *, #36591, .T. ) ;
#46638 = DIRECTION ( 'NONE',  ( 0.000000000000000000, 1.000000000000000000, 0.000000000000000000 ) ) ;
#46639 = CARTESIAN_POINT ( 'NONE',  ( -11.00000000000000000, -16.64230188589299786, 14.64519951917100116 ) ) ;
#46640 = EDGE_CURVE ( 'NONE', #51018, #1191, #6533, .T. ) ;
#46641 = DIRECTION ( 'NONE',  ( -1.000000000000000000, 0.000000000000000000, 0.000000000000000000 ) ) ;
#46643 = ORIENTED_EDGE ( 'NONE', *, *, #1996, .T. ) ;
#46642 = CARTESIAN_POINT ( 'NONE',  ( -23.48000000000000043, -15.50000000000000000, -26.00000000000000355 ) ) ;
#46644 = CARTESIAN_POINT ( 'NONE',  ( -7.450000000000001954, 7.250000000000000000, -25.50000000000000355 ) ) ;
#46645 = CIRCLE ( 'NONE', #375, 3.499999999999849454 ) ;
#46646 = EDGE_CURVE ( 'NONE', #42454, #32370, #46541, .T. ) ;
#46647 = LINE ( 'NONE', #8106, #34101 ) ;
#46648 = EDGE_CURVE ( 'NONE', #22317, #67902, #36295, .T. ) ;
#46649 = ORIENTED_EDGE ( 'NONE', *, *, #26296, .T. ) ;
#46650 = DIRECTION ( 'NONE',  ( 0.000000000000000000, -0.7071067811865474617, 0.7071067811865474617 ) ) ;
#46651 = DIRECTION ( 'NONE',  ( 0.000000000000000000, -2.123301534585676023E-12, 1.000000000000000000 ) ) ;
#46652 = VERTEX_POINT ( 'NONE', #63529 ) ;
#46653 = CARTESIAN_POINT ( 'NONE',  ( 30.00000000000000000, -14.33999999999999986, 14.50000000000000000 ) ) ;
#46654 = FACE_OUTER_BOUND ( 'NONE', #36006, .T. ) ;
#46655 = CIRCLE ( 'NONE', #12764, 2.458500000000000796 ) ;
#46656 = ADVANCED_FACE ( 'NONE', ( #36644 ), #47262, .F. ) ;
#46657 = DIRECTION ( 'NONE',  ( -1.000000000000000000, 0.000000000000000000, 0.000000000000000000 ) ) ;
#46658 = ADVANCED_FACE ( 'NONE', ( #31369 ), #63873, .T. ) ;
#46659 = DIRECTION ( 'NONE',  ( 0.000000000000000000, -0.9938079899998859545, 0.1111111111112941946 ) ) ;
#46660 = ORIENTED_EDGE ( 'NONE', *, *, #62092, .F. ) ;
#46661 = LINE ( 'NONE', #68233, #43908 ) ;
#46662 = ORIENTED_EDGE ( 'NONE', *, *, #62706, .F. ) ;
#46663 = ORIENTED_EDGE ( 'NONE', *, *, #31439, .T. ) ;
#46664 = ORIENTED_EDGE ( 'NONE', *, *, #7987, .T. ) ;
#46665 = CIRCLE ( 'NONE', #59094, 0.5000000000000000000 ) ;
#46666 = CARTESIAN_POINT ( 'NONE',  ( 11.78648345035335865, 7.593516549646607494, 195.0000000000000284 ) ) ;
#46667 = LINE ( 'NONE', #25822, #61499 ) ;
#46668 = CARTESIAN_POINT ( 'NONE',  ( 39.00000000000000000, -16.96999999999999886, 21.00000000000000000 ) ) ;
#46669 = EDGE_LOOP ( 'NONE', ( #65156, #30721, #51805, #31924 ) ) ;
#46670 = ORIENTED_EDGE ( 'NONE', *, *, #33124, .F. ) ;
#46671 = CYLINDRICAL_SURFACE ( 'NONE', #61142, 1.000000000000000000 ) ;
#46672 = VERTEX_POINT ( 'NONE', #4482 ) ;
#46673 = ORIENTED_EDGE ( 'NONE', *, *, #7771, .F. ) ;
#46674 = DIRECTION ( 'NONE',  ( -1.000000000000000000, 0.000000000000000000, 0.000000000000000000 ) ) ;
#46675 = LINE ( 'NONE', #30424, #52774 ) ;
#46676 = CIRCLE ( 'NONE', #29760, 0.1999999999999987899 ) ;
#46677 = AXIS2_PLACEMENT_3D ( 'NONE', #17198, #38770, #1292 ) ;
#46678 = CARTESIAN_POINT ( 'NONE',  ( -9.690000000000001279, 9.750000000000000000, -4.250000000000000000 ) ) ;
#46679 = CARTESIAN_POINT ( 'NONE',  ( 30.00000000000000000, -12.00000000000000000, -10.20500000000000007 ) ) ;
#46680 = ORIENTED_EDGE ( 'NONE', *, *, #13674, .T. ) ;
#46681 = CIRCLE ( 'NONE', #43257, 0.4999999999979768961 ) ;
#46682 = DIRECTION ( 'NONE',  ( -1.836970198721029934E-16, 1.836970198721036344E-16, -1.000000000000000000 ) ) ;
#46684 = PLANE ( 'NONE',  #52549 ) ;
#46683 = DIRECTION ( 'NONE',  ( 1.000000000000000000, -3.016910393003147986E-15, 0.000000000000000000 ) ) ;
#46685 = CIRCLE ( 'NONE', #34245, 0.2000000000000005107 ) ;
#46687 = ORIENTED_EDGE ( 'NONE', *, *, #54420, .T. ) ;
#46686 = CIRCLE ( 'NONE', #61351, 24.99999999998784972 ) ;
#46689 = VERTEX_POINT ( 'NONE', #14020 ) ;
#46688 = DIRECTION ( 'NONE',  ( -0.000000000000000000, 3.673940397442059868E-16, -1.000000000000000000 ) ) ;
#46690 = ORIENTED_EDGE ( 'NONE', *, *, #67848, .F. ) ;
#46691 = EDGE_LOOP ( 'NONE', ( #25689, #68014, #6855, #34941 ) ) ;
#46692 = AXIS2_PLACEMENT_3D ( 'NONE', #6450, #31934, #455 ) ;
#46693 = DIRECTION ( 'NONE',  ( -1.000000000000000000, 0.000000000000000000, 0.000000000000000000 ) ) ;
#46694 = EDGE_CURVE ( 'NONE', #56088, #56996, #51864, .T. ) ;
#46695 = DIRECTION ( 'NONE',  ( 1.000000000000000000, -3.491481338843133355E-15, -1.836970198721036344E-16 ) ) ;
#46696 = VERTEX_POINT ( 'NONE', #68118 ) ;
#46697 = ORIENTED_EDGE ( 'NONE', *, *, #64279, .T. ) ;
#46698 = ADVANCED_FACE ( 'NONE', ( #19666 ), #35580, .F. ) ;
#46699 = DIRECTION ( 'NONE',  ( -1.000000000000000000, 0.000000000000000000, 0.000000000000000000 ) ) ;
#46700 = EDGE_CURVE ( 'NONE', #25895, #31596, #26879, .T. ) ;
#46701 = DIRECTION ( 'NONE',  ( 0.000000000000000000, 0.000000000000000000, -1.000000000000000000 ) ) ;
#46702 = EDGE_LOOP ( 'NONE', ( #56220, #43484, #68453, #16364 ) ) ;
#46703 = ORIENTED_EDGE ( 'NONE', *, *, #852, .F. ) ;
#46704 = DIRECTION ( 'NONE',  ( 1.000000000000000000, 0.000000000000000000, 0.000000000000000000 ) ) ;
#46705 = ADVANCED_FACE ( 'NONE', ( #15778 ), #10468, .F. ) ;
#46706 = DIRECTION ( 'NONE',  ( 0.000000000000000000, 0.000000000000000000, -1.000000000000000000 ) ) ;
#46707 = ORIENTED_EDGE ( 'NONE', *, *, #55719, .T. ) ;
#46708 = DIRECTION ( 'NONE',  ( 1.000000000000000000, -3.016910393003147986E-15, 0.000000000000000000 ) ) ;
#46709 = LINE ( 'NONE', #30805, #41874 ) ;
#46711 = ORIENTED_EDGE ( 'NONE', *, *, #42787, .F. ) ;
#46710 = CARTESIAN_POINT ( 'NONE',  ( 6.501044194225490180, -3.157023737882825198, 54.00000000000000711 ) ) ;
#46712 = ORIENTED_EDGE ( 'NONE', *, *, #33623, .F. ) ;
#46713 = DIRECTION ( 'NONE',  ( 0.000000000000000000, 0.000000000000000000, -1.000000000000000000 ) ) ;
#46714 = DIRECTION ( 'NONE',  ( -1.836970198721029934E-16, 1.836970198721036590E-16, -1.000000000000000000 ) ) ;
#46715 = CARTESIAN_POINT ( 'NONE',  ( 39.00000000000000000, 14.08845687959340331, 21.00000000000000000 ) ) ;
#46716 = DIRECTION ( 'NONE',  ( -1.000000000000000000, 0.000000000000000000, 0.000000000000000000 ) ) ;
#46717 = ADVANCED_FACE ( 'NONE', ( #64917 ), #5523, .F. ) ;
#46718 = CARTESIAN_POINT ( 'NONE',  ( 8.250000000000005329, 0.000000000000000000, -21.00000000000000000 ) ) ;
#46719 = APPLICATION_CONTEXT ( 'automotive_design' ) ;
#46720 = DIRECTION ( 'NONE',  ( 1.000000000000000000, -0.000000000000000000, -0.000000000000000000 ) ) ;
#46721 = VERTEX_POINT ( 'NONE', #59946 ) ;
#46722 = DIRECTION ( 'NONE',  ( 1.000000000000000000, -0.000000000000000000, 0.000000000000000000 ) ) ;
#46724 = ORIENTED_EDGE ( 'NONE', *, *, #28354, .T. ) ;
#46723 = CARTESIAN_POINT ( 'NONE',  ( 11.19000000000000128, -12.00000000000000000, 0.000000000000000000 ) ) ;
#46725 = CARTESIAN_POINT ( 'NONE',  ( 31.89999999999999858, 20.60000000000000142, 2.585923194002694273E-15 ) ) ;
#46726 = AXIS2_PLACEMENT_3D ( 'NONE', #31807, #44123, #10571 ) ;
#46727 = VECTOR ( 'NONE', #34764, 1000.000000000000000 ) ;
#46728 = CARTESIAN_POINT ( 'NONE',  ( -9.942044687070568543, 9.234937905883914055, 455.0000000000000568 ) ) ;
#46729 = DIRECTION ( 'NONE',  ( -0.000000000000000000, -0.000000000000000000, 1.000000000000000000 ) ) ;
#46730 = AXIS2_PLACEMENT_3D ( 'NONE', #14816, #31077, #59938 ) ;
#46731 = ORIENTED_EDGE ( 'NONE', *, *, #60922, .F. ) ;
#46732 = FACE_OUTER_BOUND ( 'NONE', #33480, .T. ) ;
#46733 = CARTESIAN_POINT ( 'NONE',  ( -7.798499376344109280, -4.740315990920159095, 455.0000000000000568 ) ) ;
#46734 = ORIENTED_EDGE ( 'NONE', *, *, #22062, .F. ) ;
#46735 = CARTESIAN_POINT ( 'NONE',  ( -7.250000000000000888, -8.249999999999998224, -26.00000000000001066 ) ) ;
#46736 = VECTOR ( 'NONE', #61975, 1000.000000000000000 ) ;
#46737 = AXIS2_PLACEMENT_3D ( 'NONE', #56950, #4294, #47403 ) ;
#46738 = EDGE_CURVE ( 'NONE', #2257, #51399, #38724, .T. ) ;
#46739 = ADVANCED_FACE ( 'NONE', ( #27080 ), #48653, .T. ) ;
#46740 = CARTESIAN_POINT ( 'NONE',  ( 275.0000000000000000, -31.99999999999889866, -7.899999999997660893 ) ) ;
#46741 = ORIENTED_EDGE ( 'NONE', *, *, #28073, .F. ) ;
#46742 = CARTESIAN_POINT ( 'NONE',  ( 3.664523737882778853, -10.50702373788281285, 54.00000000000000711 ) ) ;
#46743 = ORIENTED_EDGE ( 'NONE', *, *, #10050, .T. ) ;
#46744 = EDGE_CURVE ( 'NONE', #58038, #50249, #68612, .T. ) ;
#46745 = ORIENTED_EDGE ( 'NONE', *, *, #14074, .F. ) ;
#46746 = AXIS2_PLACEMENT_3D ( 'NONE', #22356, #17038, #38608 ) ;
#46747 = CARTESIAN_POINT ( 'NONE',  ( 9.900000000000000355, -18.00000000000000355, -21.00000000000000000 ) ) ;
#46748 = CARTESIAN_POINT ( 'NONE',  ( 7.250000000000004441, 7.450000000000001954, -16.00000000000000000 ) ) ;
#46749 = CARTESIAN_POINT ( 'NONE',  ( 30.00000000000000000, -9.487228132326899654, -12.50000000000000000 ) ) ;
#46750 = CYLINDRICAL_SURFACE ( 'NONE', #56917, 24.99999999998789946 ) ;
#46751 = LINE ( 'NONE', #20930, #32853 ) ;
#46752 = ORIENTED_EDGE ( 'NONE', *, *, #3874, .F. ) ;
#46753 = ORIENTED_EDGE ( 'NONE', *, *, #45417, .F. ) ;
#46755 = EDGE_LOOP ( 'NONE', ( #5680, #46786, #52489, #10191, #60165, #48020, #58072 ) ) ;
#46754 = FACE_OUTER_BOUND ( 'NONE', #21601, .T. ) ;
#46756 = VERTEX_POINT ( 'NONE', #59615 ) ;
#46757 = CARTESIAN_POINT ( 'NONE',  ( 2.906483450353369413, 10.08346604330780671, 195.0000000000000284 ) ) ;
#46758 = DIRECTION ( 'NONE',  ( -1.000000000000000000, 0.000000000000000000, 0.000000000000000000 ) ) ;
#46759 = CARTESIAN_POINT ( 'NONE',  ( 7.250000000000005329, -7.249999999999998224, -19.50000000000000000 ) ) ;
#46760 = CARTESIAN_POINT ( 'NONE',  ( 4.186483450353337687, -11.78648345035337996, 195.0000000000000284 ) ) ;
#46761 = VECTOR ( 'NONE', #47538, 1000.000000000000000 ) ;
#46762 = LINE ( 'NONE', #52080, #9653 ) ;
#46763 = LINE ( 'NONE', #17372, #5022 ) ;
#46764 = EDGE_LOOP ( 'NONE', ( #5839, #27276, #32709, #15206 ) ) ;
#46765 = VERTEX_POINT ( 'NONE', #32398 ) ;
#46766 = ORIENTED_EDGE ( 'NONE', *, *, #61218, .F. ) ;
#46767 = EDGE_LOOP ( 'NONE', ( #50563, #19188, #30129, #50048, #55892, #51642 ) ) ;
#46768 = CARTESIAN_POINT ( 'NONE',  ( 49.00000000000000000, -0.1999999999911795112, 8.826273045769999343E-12 ) ) ;
#46769 = DIRECTION ( 'NONE',  ( 1.836970198721029934E-16, 1.836970198721010706E-16, -1.000000000000000000 ) ) ;
#46770 = ADVANCED_FACE ( 'NONE', ( #42991 ), #60286, .T. ) ;
#46771 = VECTOR ( 'NONE', #64584, 1000.000000000000000 ) ;
#46773 = PLANE ( 'NONE',  #7149 ) ;
#46772 = AXIS2_PLACEMENT_3D ( 'NONE', #16711, #10695, #16350 ) ;
#46774 = ORIENTED_EDGE ( 'NONE', *, *, #68093, .F. ) ;
#46775 = ORIENTED_EDGE ( 'NONE', *, *, #47117, .T. ) ;
#46776 = ORIENTED_EDGE ( 'NONE', *, *, #43207, .T. ) ;
#46777 = EDGE_CURVE ( 'NONE', #38349, #65427, #43334, .T. ) ;
#46778 = DIRECTION ( 'NONE',  ( 1.000000000000000000, 0.000000000000000000, -0.000000000000000000 ) ) ;
#46779 = ORIENTED_EDGE ( 'NONE', *, *, #51347, .T. ) ;
#46780 = VECTOR ( 'NONE', #61227, 1000.000000000000000 ) ;
#46781 = VERTEX_POINT ( 'NONE', #54656 ) ;
#46782 = ADVANCED_FACE ( 'NONE', ( #6211 ), #64571, .F. ) ;
#46783 = DIRECTION ( 'NONE',  ( 0.6414496315691592399, 0.7671651518152985405, 2.309356642088728176E-17 ) ) ;
#46784 = EDGE_CURVE ( 'NONE', #62351, #4816, #26740, .T. ) ;
#46785 = ORIENTED_EDGE ( 'NONE', *, *, #29694, .T. ) ;
#46786 = ORIENTED_EDGE ( 'NONE', *, *, #57345, .T. ) ;
#46787 = DIRECTION ( 'NONE',  ( 0.000000000000000000, -0.7071067811865076047, -0.7071067811865875408 ) ) ;
#46788 = EDGE_CURVE ( 'NONE', #32262, #49212, #10816, .T. ) ;
#46789 = ADVANCED_FACE ( 'NONE', ( #11159 ), #58917, .F. ) ;
#46791 = EDGE_LOOP ( 'NONE', ( #19348, #22184, #25326, #34201 ) ) ;
#46790 = CARTESIAN_POINT ( 'NONE',  ( -29.25000000000000000, -5.200000000000001066, 60.00000000000000000 ) ) ;
#46792 = VERTEX_POINT ( 'NONE', #33078 ) ;
#46793 = CARTESIAN_POINT ( 'NONE',  ( 10.92648345035331658, 2.893516549646575786, 195.0000000000000284 ) ) ;
#46794 = FACE_BOUND ( 'NONE', #3719, .T. ) ;
#46795 = EDGE_CURVE ( 'NONE', #52522, #49901, #22129, .T. ) ;
#46796 = CARTESIAN_POINT ( 'NONE',  ( 30.00000000000000000, -11.50000000000000000, 15.00000000000000000 ) ) ;
#46798 = VERTEX_POINT ( 'NONE', #43696 ) ;
#46797 = CARTESIAN_POINT ( 'NONE',  ( 4.456444791733522252E-16, 7.450000000000002842, -10.00000000000000000 ) ) ;
#46799 = VECTOR ( 'NONE', #31141, 1000.000000000000000 ) ;
#46800 = VERTEX_POINT ( 'NONE', #38390 ) ;
#46801 = CARTESIAN_POINT ( 'NONE',  ( 14.66434062215688883, -0.3156604612129069731, 21.53909249377453250 ) ) ;
#46802 = CARTESIAN_POINT ( 'NONE',  ( 8.250000000000005329, -8.249999999999998224, -26.00000000000001066 ) ) ;
#46803 = DIRECTION ( 'NONE',  ( 0.000000000000000000, 0.000000000000000000, -1.000000000000000000 ) ) ;
#46804 = CARTESIAN_POINT ( 'NONE',  ( -7.250000000000001776, -7.249999999999998224, -15.00000000000000000 ) ) ;
#46805 = EDGE_LOOP ( 'NONE', ( #53695, #33811, #10272, #20066 ) ) ;
#46806 = PLANE ( 'NONE',  #67624 ) ;
#46807 = CARTESIAN_POINT ( 'NONE',  ( 6.364920264886889001, 6.822336235477383326, 54.00000000000000711 ) ) ;
#46808 = CARTESIAN_POINT ( 'NONE',  ( 11.34648345035338046, -1.090483450353491035, 455.0000000000000568 ) ) ;
#46809 = ORIENTED_EDGE ( 'NONE', *, *, #19765, .T. ) ;
#46810 = VECTOR ( 'NONE', #35003, 1000.000000000000000 ) ;
#46811 = DIRECTION ( 'NONE',  ( 1.000000000000000000, 0.000000000000000000, 0.000000000000000000 ) ) ;
#46812 = CARTESIAN_POINT ( 'NONE',  ( 7.811466277050736373, -7.272650909786728235, 455.0000000000000568 ) ) ;
#46813 = LINE ( 'NONE', #35864, #56229 ) ;
#46814 = CIRCLE ( 'NONE', #50192, 0.5000000000001392220 ) ;
#46815 = ORIENTED_EDGE ( 'NONE', *, *, #49645, .T. ) ;
#46816 = DIRECTION ( 'NONE',  ( 3.596772705736698833E-15, 1.000000000000000000, 0.000000000000000000 ) ) ;
#46817 = CARTESIAN_POINT ( 'NONE',  ( 30.00000000000000000, -5.599999999999999645, 27.00000000000000000 ) ) ;
#46818 = EDGE_CURVE ( 'NONE', #46841, #64891, #55129, .T. ) ;
#46819 = VECTOR ( 'NONE', #11675, 1000.000000000000000 ) ;
#46820 = CIRCLE ( 'NONE', #53662, 1.399999999999999245 ) ;
#46821 = DIRECTION ( 'NONE',  ( -1.000000000000000000, 0.000000000000000000, 0.000000000000000000 ) ) ;
#46822 = ORIENTED_EDGE ( 'NONE', *, *, #16363, .F. ) ;
#46823 = DIRECTION ( 'NONE',  ( 0.000000000000000000, 0.000000000000000000, -1.000000000000000000 ) ) ;
#46824 = LINE ( 'NONE', #68406, #41106 ) ;
#46825 = PLANE ( 'NONE',  #19580 ) ;
#46826 = EDGE_CURVE ( 'NONE', #45033, #20832, #22484, .T. ) ;
#46827 = ADVANCED_FACE ( 'NONE', ( #65605 ), #69866, .F. ) ;
#46828 = FACE_OUTER_BOUND ( 'NONE', #11656, .T. ) ;
#46829 = DIRECTION ( 'NONE',  ( -1.000000000000000000, 0.000000000000000000, 0.000000000000000000 ) ) ;
#46830 = AXIS2_PLACEMENT_3D ( 'NONE', #61428, #40226, #28572 ) ;
#46831 = EDGE_LOOP ( 'NONE', ( #6309, #43122, #63324, #6166 ) ) ;
#46832 = FACE_OUTER_BOUND ( 'NONE', #57463, .T. ) ;
#46833 = CARTESIAN_POINT ( 'NONE',  ( 7.250000000000005329, -7.449999999999998401, -21.50000000000000000 ) ) ;
#46834 = DIRECTION ( 'NONE',  ( 1.000000000000000000, 0.000000000000000000, 0.000000000000000000 ) ) ;
#46835 = EDGE_CURVE ( 'NONE', #16863, #11814, #65934, .T. ) ;
#46836 = AXIS2_PLACEMENT_3D ( 'NONE', #29981, #51558, #35989 ) ;
#46837 = DIRECTION ( 'NONE',  ( -0.000000000000000000, 3.673940397442059868E-16, -1.000000000000000000 ) ) ;
#46838 = DIRECTION ( 'NONE',  ( -0.7671651518152985405, 0.6414496315691592399, 2.587583378555131749E-16 ) ) ;
#46839 = EDGE_LOOP ( 'NONE', ( #39030, #10102, #1108, #18833 ) ) ;
#46841 = VERTEX_POINT ( 'NONE', #29156 ) ;
#46840 = DIRECTION ( 'NONE',  ( 0.000000000000000000, 0.000000000000000000, -1.000000000000000000 ) ) ;
#46842 = CARTESIAN_POINT ( 'NONE',  ( -22.14589803375000088, -15.50000000000000000, 21.50000000000000000 ) ) ;
#46843 = CYLINDRICAL_SURFACE ( 'NONE', #41360, 1.000000000000000000 ) ;
#46844 = VECTOR ( 'NONE', #46529, 1000.000000000000000 ) ;
#46845 = CARTESIAN_POINT ( 'NONE',  ( 0.9555237378827876604, -9.404523737882790613, 54.00000000000000711 ) ) ;
#46846 = EDGE_LOOP ( 'NONE', ( #27485, #31617, #17640, #35079 ) ) ;
#46847 = AXIS2_PLACEMENT_3D ( 'NONE', #2199, #24472, #1497 ) ;
#46848 = FACE_OUTER_BOUND ( 'NONE', #6610, .T. ) ;
#46849 = DIRECTION ( 'NONE',  ( -0.000000000000000000, -0.000000000000000000, -1.000000000000000000 ) ) ;
#46850 = VERTEX_POINT ( 'NONE', #50024 ) ;
#46851 = VERTEX_POINT ( 'NONE', #40102 ) ;
#46852 = ORIENTED_EDGE ( 'NONE', *, *, #11138, .F. ) ;
#46853 = CARTESIAN_POINT ( 'NONE',  ( 12.90000000000000213, -21.00000000000001421, -13.86939075806900945 ) ) ;
#46854 = CARTESIAN_POINT ( 'NONE',  ( -6.835476262117260227, 10.49297626211718359, 26.00000000000000711 ) ) ;
#46855 = VECTOR ( 'NONE', #52929, 1000.000000000000114 ) ;
#46856 = DIRECTION ( 'NONE',  ( 0.000000000000000000, 0.000000000000000000, 1.000000000000000000 ) ) ;
#46857 = DIRECTION ( 'NONE',  ( -1.000000000000000000, 3.491481338843133355E-15, 1.836970198721036344E-16 ) ) ;
#46858 = VERTEX_POINT ( 'NONE', #23853 ) ;
#46859 = ORIENTED_EDGE ( 'NONE', *, *, #26053, .T. ) ;
#46860 = DIRECTION ( 'NONE',  ( 0.000000000000000000, 0.7046037717862339012, 0.7096009616570518874 ) ) ;
#46861 = LINE ( 'NONE', #20005, #30492 ) ;
#46862 = ORIENTED_EDGE ( 'NONE', *, *, #4386, .T. ) ;
#46863 = VERTEX_POINT ( 'NONE', #66637 ) ;
#46864 = EDGE_LOOP ( 'NONE', ( #69937, #28174, #35082, #19781, #878, #42001, #65459, #67450 ) ) ;
#46865 = ORIENTED_EDGE ( 'NONE', *, *, #55265, .F. ) ;
#46866 = LINE ( 'NONE', #62075, #59836 ) ;
#46867 = EDGE_CURVE ( 'NONE', #41582, #13987, #2290, .T. ) ;
#46869 = ORIENTED_EDGE ( 'NONE', *, *, #62848, .T. ) ;
#46868 = CARTESIAN_POINT ( 'NONE',  ( 2.005523737882813240, 8.598420958951633608, 54.00000000000000711 ) ) ;
#46870 = DIRECTION ( 'NONE',  ( 0.000000000000000000, -1.000000000000000000, 0.000000000000000000 ) ) ;
#46871 = AXIS2_PLACEMENT_3D ( 'NONE', #54992, #5149, #26719 ) ;
#46872 = AXIS2_PLACEMENT_3D ( 'NONE', #49861, #55176, #45234 ) ;
#46873 = VECTOR ( 'NONE', #51753, 1000.000000000000000 ) ;
#46874 = CARTESIAN_POINT ( 'NONE',  ( 39.90000000000000568, -0.2000000000089119934, -8.913009219568841313E-12 ) ) ;
#46875 = EDGE_CURVE ( 'NONE', #6389, #15026, #14495, .T. ) ;
#46876 = CIRCLE ( 'NONE', #59303, 0.5999999999999998668 ) ;
#46877 = ORIENTED_EDGE ( 'NONE', *, *, #41480, .T. ) ;
#46878 = VERTEX_POINT ( 'NONE', #12536 ) ;
#46879 = VECTOR ( 'NONE', #2419, 1000.000000000000000 ) ;
#46880 =( GEOMETRIC_REPRESENTATION_CONTEXT ( 3 ) GLOBAL_UNCERTAINTY_ASSIGNED_CONTEXT ( ( #26717 ) ) GLOBAL_UNIT_ASSIGNED_CONTEXT ( ( #40769, #13191, #40421 ) ) REPRESENTATION_CONTEXT ( 'NONE', 'WORKASPACE' ) );
#46881 = DIRECTION ( 'NONE',  ( 1.000000000000000000, -0.000000000000000000, 0.000000000000000000 ) ) ;
#46882 = AXIS2_PLACEMENT_3D ( 'NONE', #54538, #6093, #59139 ) ;
#46883 = DIRECTION ( 'NONE',  ( -0.7071067811865474617, 0.7071067811865474617, 0.000000000000000000 ) ) ;
#46885 = EDGE_LOOP ( 'NONE', ( #43851, #2442, #18804, #1133 ) ) ;
#46884 = EDGE_CURVE ( 'NONE', #39630, #14703, #44712, .T. ) ;
#46886 = CIRCLE ( 'NONE', #2874, 3.299999999999473577 ) ;
#46887 = CARTESIAN_POINT ( 'NONE',  ( 10.09643294401454661, -2.706483450353491804, 455.0000000000000568 ) ) ;
#46888 = DIRECTION ( 'NONE',  ( 1.000000000000000000, -7.665540703601096574E-15, -2.816273965919649962E-30 ) ) ;
#46889 = SURFACE_SIDE_STYLE ('',( #45842 ) ) ;
#46890 = ORIENTED_EDGE ( 'NONE', *, *, #17849, .T. ) ;
#46891 = STYLED_ITEM ( 'NONE', ( #29320 ), #43848 ) ;
#46892 = DIRECTION ( 'NONE',  ( 0.000000000000000000, 0.6857142857142869419, -0.7278708115918273158 ) ) ;
#46893 = LINE ( 'NONE', #67432, #68550 ) ;
#46894 = LINE ( 'NONE', #41597, #18376 ) ;
#46895 = CARTESIAN_POINT ( 'NONE',  ( 3.848229544836329730, 7.342976262117204556, 54.00000000000000711 ) ) ;
#46896 = LINE ( 'NONE', #46544, #62469 ) ;
#46897 = VERTEX_POINT ( 'NONE', #1255 ) ;
#46898 = CARTESIAN_POINT ( 'NONE',  ( -7.450000000000001954, 0.000000000000000000, -15.50000000000000000 ) ) ;
#46899 = DIRECTION ( 'NONE',  ( 0.000000000000000000, 0.000000000000000000, -1.000000000000000000 ) ) ;
#46900 = DIRECTION ( 'NONE',  ( 1.000000000000000000, -0.000000000000000000, 0.000000000000000000 ) ) ;
#46901 = DIRECTION ( 'NONE',  ( -1.000000000000000000, 0.000000000000000000, 0.000000000000000000 ) ) ;
#46902 = CARTESIAN_POINT ( 'NONE',  ( 4.186483450353376767, 11.99351654964663716, 195.0000000000000284 ) ) ;
#46903 = CARTESIAN_POINT ( 'NONE',  ( -7.342976262117273833, -4.961189459950004377, 54.00000000000000711 ) ) ;
#46904 = CARTESIAN_POINT ( 'NONE',  ( -25.50000000000000355, 0.000000000000000000, -22.50000000000000000 ) ) ;
#46905 = CARTESIAN_POINT ( 'NONE',  ( 13.90000000000000213, -21.00000000000001421, -13.86939075806900945 ) ) ;
#46906 = ORIENTED_EDGE ( 'NONE', *, *, #21981, .F. ) ;
#46907 = CARTESIAN_POINT ( 'NONE',  ( -11.00000000000000000, -14.04000000000000092, 17.04524521594300523 ) ) ;
#46908 = CARTESIAN_POINT ( 'NONE',  ( 20.90000000000000213, 13.66939075806899240, 20.79999999999999361 ) ) ;
#46909 = VECTOR ( 'NONE', #27891, 1000.000000000000000 ) ;
#46910 = EDGE_LOOP ( 'NONE', ( #6842, #5095 ) ) ;
#46911 = DIRECTION ( 'NONE',  ( 0.000000000000000000, 1.000000000000000000, 0.000000000000000000 ) ) ;
#46912 = CARTESIAN_POINT ( 'NONE',  ( 11.50000000000000000, -11.50000000000000000, -19.00000000000000000 ) ) ;
#46913 = EDGE_CURVE ( 'NONE', #58012, #41307, #1944, .T. ) ;
#46914 = DIRECTION ( 'NONE',  ( -0.000000000000000000, 3.673940397442059868E-16, -1.000000000000000000 ) ) ;
#46915 = AXIS2_PLACEMENT_3D ( 'NONE', #34895, #40910, #29953 ) ;
#46916 = CARTESIAN_POINT ( 'NONE',  ( -6.822336235477489019, -6.364920264886855250, 54.00000000000000711 ) ) ;
#46917 = LINE ( 'NONE', #20058, #56513 ) ;
#46918 = EDGE_LOOP ( 'NONE', ( #29141, #14773, #3493, #47560, #41505 ) ) ;
#46919 = VECTOR ( 'NONE', #13996, 1000.000000000000000 ) ;
#46920 = VECTOR ( 'NONE', #13422, 1000.000000000000114 ) ;
#46921 = AXIS2_PLACEMENT_3D ( 'NONE', #6451, #43578, #54550 ) ;
#46922 = ORIENTED_EDGE ( 'NONE', *, *, #28816, .T. ) ;
#46923 = LINE ( 'NONE', #26418, #14621 ) ;
#46924 = CYLINDRICAL_SURFACE ( 'NONE', #11919, 4.500000000000189182 ) ;
#46925 = ORIENTED_EDGE ( 'NONE', *, *, #25254, .T. ) ;
#46926 = CARTESIAN_POINT ( 'NONE',  ( 15.00000000000000000, -42.00000000000000000, -26.50000000000000000 ) ) ;
#46927 = VECTOR ( 'NONE', #37769, 1000.000000000000000 ) ;
#46928 = AXIS2_PLACEMENT_3D ( 'NONE', #49720, #49393, #26783 ) ;
#46929 = VECTOR ( 'NONE', #29027, 1000.000000000000000 ) ;
#46930 = EDGE_CURVE ( 'NONE', #18594, #36419, #39319, .T. ) ;
#46931 = CARTESIAN_POINT ( 'NONE',  ( 4.456444791733522252E-16, 7.450000000000002842, -22.50000000000000000 ) ) ;
#46932 = ORIENTED_EDGE ( 'NONE', *, *, #1527, .F. ) ;
#46933 = AXIS2_PLACEMENT_3D ( 'NONE', #52635, #42709, #4199 ) ;
#46934 = ADVANCED_FACE ( 'NONE', ( #56037 ), #39414, .F. ) ;
#46935 = DIRECTION ( 'NONE',  ( 0.000000000000000000, 1.000000000000000000, 0.000000000000000000 ) ) ;
#46936 = ORIENTED_EDGE ( 'NONE', *, *, #5858, .T. ) ;
#46937 = EDGE_LOOP ( 'NONE', ( #66508, #23799, #68517, #13813 ) ) ;
#46938 = DIRECTION ( 'NONE',  ( 0.000000000000000000, -0.7071067811865480168, 0.7071067811865470176 ) ) ;
#46939 = ORIENTED_EDGE ( 'NONE', *, *, #13728, .F. ) ;
#46940 = ORIENTED_EDGE ( 'NONE', *, *, #25579, .F. ) ;
#46941 = CYLINDRICAL_SURFACE ( 'NONE', #47427, 24.99999999998784972 ) ;
#46942 = CARTESIAN_POINT ( 'NONE',  ( 7.450000000000006395, 7.250000000000000888, -16.00000000000000000 ) ) ;
#46943 = AXIS2_PLACEMENT_3D ( 'NONE', #668, #22238, #11260 ) ;
#46944 = DIRECTION ( 'NONE',  ( 1.000000000000000000, -1.047444401652939849E-14, 0.000000000000000000 ) ) ;
#46945 = EDGE_LOOP ( 'NONE', ( #5836, #10932 ) ) ;
#46946 = VECTOR ( 'NONE', #28208, 1000.000000000000000 ) ;
#46947 = LINE ( 'NONE', #37059, #25553 ) ;
#46949 = DIRECTION ( 'NONE',  ( -1.047444401652940007E-14, -1.000000000000000000, -1.836970198721029934E-16 ) ) ;
#46948 = CARTESIAN_POINT ( 'NONE',  ( 11.78648345035337819, -7.826483450353395988, 195.0000000000000284 ) ) ;
#46950 = ORIENTED_EDGE ( 'NONE', *, *, #18526, .F. ) ;
#46952 = VERTEX_POINT ( 'NONE', #7587 ) ;
#46951 = DIRECTION ( 'NONE',  ( -0.7071067811865480168, 0.000000000000000000, -0.7071067811865470176 ) ) ;
#46953 = VERTEX_POINT ( 'NONE', #2633 ) ;
#46954 = APPLICATION_PROTOCOL_DEFINITION ( 'draft international standard', 'automotive_design', 1998, #54903 ) ;
#46955 = CARTESIAN_POINT ( 'NONE',  ( 28.00000000000000000, -15.50000000000000000, 14.50000000000000000 ) ) ;
#46957 = VERTEX_POINT ( 'NONE', #24207 ) ;
#46956 = DIRECTION ( 'NONE',  ( 0.000000000000000000, 1.000000000000000000, 0.000000000000000000 ) ) ;
#46958 = ADVANCED_FACE ( 'NONE', ( #8280 ), #66983, .F. ) ;
#46959 = CARTESIAN_POINT ( 'NONE',  ( -29.50000000000000355, -11.70000000000000284, 11.00000000000000000 ) ) ;
#46960 = DIRECTION ( 'NONE',  ( 0.000000000000000000, 1.000000000000000000, -0.000000000000000000 ) ) ;
#46961 = EDGE_CURVE ( 'NONE', #67142, #64098, #61320, .T. ) ;
#46962 = VERTEX_POINT ( 'NONE', #17505 ) ;
#46963 = EDGE_CURVE ( 'NONE', #7638, #14513, #38185, .T. ) ;
#46964 = VERTEX_POINT ( 'NONE', #18543 ) ;
#46965 = CARTESIAN_POINT ( 'NONE',  ( -9.293516549646710700, 10.91351654964659801, 195.0000000000000284 ) ) ;
#46966 = EDGE_CURVE ( 'NONE', #21056, #12243, #23508, .T. ) ;
#46967 = AXIS2_PLACEMENT_3D ( 'NONE', #57455, #10079, #25285 ) ;
#46968 = EDGE_LOOP ( 'NONE', ( #45462, #13080, #3131, #13290, #44017, #22532, #65255 ) ) ;
#46969 = EDGE_CURVE ( 'NONE', #14942, #21656, #56380, .T. ) ;
#46970 = CARTESIAN_POINT ( 'NONE',  ( -15.08565937784311295, -0.3156604612129216836, -23.70415600323552852 ) ) ;
#46971 = DIRECTION ( 'NONE',  ( -0.7071067811865441310, 0.7071067811865510144, 0.000000000000000000 ) ) ;
#46972 = VECTOR ( 'NONE', #5471, 1000.000000000000000 ) ;
#46973 = EDGE_CURVE ( 'NONE', #1040, #60826, #69824, .T. ) ;
#46974 = CYLINDRICAL_SURFACE ( 'NONE', #33980, 0.1749999999999993783 ) ;
#46975 = ORIENTED_EDGE ( 'NONE', *, *, #61737, .F. ) ;
#46976 = EDGE_CURVE ( 'NONE', #45256, #10779, #60642, .T. ) ;
#46977 = VECTOR ( 'NONE', #50621, 1000.000000000000000 ) ;
#46978 = VECTOR ( 'NONE', #20734, 1000.000000000000000 ) ;
#46979 = VECTOR ( 'NONE', #10279, 1000.000000000000000 ) ;
#46980 = DIRECTION ( 'NONE',  ( -1.836970198721029934E-16, -1.836970198721010706E-16, 1.000000000000000000 ) ) ;
#46981 = FACE_OUTER_BOUND ( 'NONE', #38602, .T. ) ;
#46983 = VERTEX_POINT ( 'NONE', #56730 ) ;
#46982 = CARTESIAN_POINT ( 'NONE',  ( -7.259684009079963474, -4.201500623656036382, 455.0000000000000568 ) ) ;
#46985 = VERTEX_POINT ( 'NONE', #12193 ) ;
#46984 = FACE_OUTER_BOUND ( 'NONE', #3415, .T. ) ;
#46986 = CARTESIAN_POINT ( 'NONE',  ( 30.00000000000000000, -5.200000000000001066, -9.400000000000000355 ) ) ;
#46987 = AXIS2_PLACEMENT_3D ( 'NONE', #68465, #41938, #4472 ) ;
#46988 = VECTOR ( 'NONE', #30782, 1000.000000000000000 ) ;
#46989 = CIRCLE ( 'NONE', #30075, 0.1999999999999987899 ) ;
#46990 = DIRECTION ( 'NONE',  ( 0.6414496315691617934, -0.7671651518152962090, -2.818519042763987834E-16 ) ) ;
#46991 = CARTESIAN_POINT ( 'NONE',  ( 15.50000000000000000, -1.037157890325000054, -22.50000000000000000 ) ) ;
#46992 = DIRECTION ( 'NONE',  ( -1.836970198721029934E-16, 1.836970198721036344E-16, -1.000000000000000000 ) ) ;
#46993 = CARTESIAN_POINT ( 'NONE',  ( -13.00000000000000178, -17.50000000000000000, -20.05051025721700242 ) ) ;
#46994 = ORIENTED_EDGE ( 'NONE', *, *, #1401, .T. ) ;
#46995 = CARTESIAN_POINT ( 'NONE',  ( -11.07551654964683330, -11.48848345035333907, 455.0000000000000568 ) ) ;
#46996 = FACE_OUTER_BOUND ( 'NONE', #40928, .T. ) ;
#46997 = CARTESIAN_POINT ( 'NONE',  ( 27.90000000000000213, 0.000000000000000000, 2.458500000000000796 ) ) ;
#46999 = ORIENTED_EDGE ( 'NONE', *, *, #29294, .T. ) ;
#46998 = FACE_OUTER_BOUND ( 'NONE', #19756, .T. ) ;
#47000 = AXIS2_PLACEMENT_3D ( 'NONE', #23258, #28219, #33861 ) ;
#47001 = CARTESIAN_POINT ( 'NONE',  ( 0.000000000000000000, 0.000000000000000000, -22.50000000000000000 ) ) ;
#47002 = EDGE_CURVE ( 'NONE', #36489, #32081, #33764, .T. ) ;
#47003 = DIRECTION ( 'NONE',  ( 0.8660254037844485886, 0.000000000000000000, -0.4999999999999827360 ) ) ;
#47004 = CARTESIAN_POINT ( 'NONE',  ( 11.50000000000000000, -12.00000000000000000, -10.69999999999999929 ) ) ;
#47005 = VERTEX_POINT ( 'NONE', #4409 ) ;
#47006 = FACE_OUTER_BOUND ( 'NONE', #36984, .T. ) ;
#47007 = CARTESIAN_POINT ( 'NONE',  ( 8.750000000000000000, -7.348062532928000934, 5.000000000000000000 ) ) ;
#47008 = ORIENTED_EDGE ( 'NONE', *, *, #25118, .T. ) ;
#47009 = DIRECTION ( 'NONE',  ( 0.000000000000000000, 0.000000000000000000, 1.000000000000000000 ) ) ;
#47010 = ADVANCED_FACE ( 'NONE', ( #25972 ), #63090, .F. ) ;
#47011 = DIRECTION ( 'NONE',  ( 0.000000000000000000, 1.000000000000000000, 0.000000000000000000 ) ) ;
#47012 = CARTESIAN_POINT ( 'NONE',  ( -25.50000000000000355, -17.50000000000000000, -22.50000000000000000 ) ) ;
#47013 = LINE ( 'NONE', #69645, #32708 ) ;
#47014 = DIRECTION ( 'NONE',  ( 1.261617073437657735E-14, 1.000000000000000000, 3.673940397442059868E-16 ) ) ;
#47015 = ORIENTED_EDGE ( 'NONE', *, *, #41350, .F. ) ;
#47016 = PLANE ( 'NONE',  #31668 ) ;
#47017 = ORIENTED_EDGE ( 'NONE', *, *, #11954, .T. ) ;
#47018 = CARTESIAN_POINT ( 'NONE',  ( 20.90000000000000213, -14.06939075806902117, -20.80000000000000426 ) ) ;
#47019 = VERTEX_POINT ( 'NONE', #20302 ) ;
#47020 = AXIS2_PLACEMENT_3D ( 'NONE', #50987, #39335, #45671 ) ;
#47021 = VERTEX_POINT ( 'NONE', #31286 ) ;
#47022 = DIRECTION ( 'NONE',  ( 0.3479852726768751237, 0.000000000000000000, 0.9375000000000004441 ) ) ;
#47023 = AXIS2_PLACEMENT_3D ( 'NONE', #514, #65225, #34048 ) ;
#47024 = DIRECTION ( 'NONE',  ( 0.000000000000000000, 0.000000000000000000, -1.000000000000000000 ) ) ;
#47025 = VECTOR ( 'NONE', #36032, 999.9999999999998863 ) ;
#47026 = AXIS2_PLACEMENT_3D ( 'NONE', #51679, #67935, #36453 ) ;
#47027 = EDGE_CURVE ( 'NONE', #21803, #63045, #26925, .T. ) ;
#47028 = DIRECTION ( 'NONE',  ( 0.000000000000000000, 0.000000000000000000, -1.000000000000000000 ) ) ;
#47029 = VERTEX_POINT ( 'NONE', #42215 ) ;
#47030 = ORIENTED_EDGE ( 'NONE', *, *, #4892, .F. ) ;
#47031 = CARTESIAN_POINT ( 'NONE',  ( -25.50000000000000355, -15.50000000000000000, -24.50000000000000000 ) ) ;
#47032 = VERTEX_POINT ( 'NONE', #46466 ) ;
#47033 = VERTEX_POINT ( 'NONE', #57079 ) ;
#47034 = VECTOR ( 'NONE', #59519, 1000.000000000000000 ) ;
#47035 = VECTOR ( 'NONE', #19774, 1000.000000000000000 ) ;
#47036 = AXIS2_PLACEMENT_3D ( 'NONE', #722, #48806, #37160 ) ;
#47037 = LINE ( 'NONE', #53057, #68836 ) ;
#47038 = CARTESIAN_POINT ( 'NONE',  ( 11.48848345035337282, 11.07551654964657395, 195.0000000000000284 ) ) ;
#47039 = FACE_OUTER_BOUND ( 'NONE', #15194, .T. ) ;
#47040 = EDGE_CURVE ( 'NONE', #47719, #8412, #61882, .T. ) ;
#47041 = ORIENTED_EDGE ( 'NONE', *, *, #69316, .T. ) ;
#47042 = EDGE_CURVE ( 'NONE', #20832, #28438, #41520, .T. ) ;
#47043 = FACE_OUTER_BOUND ( 'NONE', #24095, .T. ) ;
#47044 = AXIS2_PLACEMENT_3D ( 'NONE', #28845, #50430, #45816 ) ;
#47046 = CARTESIAN_POINT ( 'NONE',  ( 10.20488345035340849, 11.07551654964657928, 195.0000000000000284 ) ) ;
#47045 = CARTESIAN_POINT ( 'NONE',  ( 4.720772854004775532, 4.141586236041047364, 26.00000000000000711 ) ) ;
#47047 = ORIENTED_EDGE ( 'NONE', *, *, #27093, .T. ) ;
#47050 = EDGE_CURVE ( 'NONE', #22451, #50321, #48369, .T. ) ;
#47049 = ORIENTED_EDGE ( 'NONE', *, *, #66413, .T. ) ;
#47048 = CARTESIAN_POINT ( 'NONE',  ( 9.900000000000000355, 21.00000000000000000, -18.00000000000000355 ) ) ;
#47051 = ORIENTED_EDGE ( 'NONE', *, *, #12642, .T. ) ;
#47052 = EDGE_CURVE ( 'NONE', #41205, #62492, #62730, .T. ) ;
#47053 = EDGE_CURVE ( 'NONE', #6044, #64879, #24564, .T. ) ;
#47054 = AXIS2_PLACEMENT_3D ( 'NONE', #7039, #23651, #39561 ) ;
#47055 = DIRECTION ( 'NONE',  ( -1.836970198721029934E-16, 1.836970198721036590E-16, -1.000000000000000000 ) ) ;
#47056 = ADVANCED_FACE ( 'NONE', ( #19249 ), #25262, .F. ) ;
#47057 = CIRCLE ( 'NONE', #23374, 6.000000000000005329 ) ;
#47058 = DIRECTION ( 'NONE',  ( 0.000000000000000000, 0.000000000000000000, -1.000000000000000000 ) ) ;
#47059 = ADVANCED_FACE ( 'NONE', ( #8642 ), #36561, .F. ) ;
#47060 = ORIENTED_EDGE ( 'NONE', *, *, #2012, .T. ) ;
#47061 = ORIENTED_EDGE ( 'NONE', *, *, #2287, .F. ) ;
#47062 = DIRECTION ( 'NONE',  ( -9.912705577010336396E-15, -1.000000000000000000, 0.000000000000000000 ) ) ;
#47063 = DIRECTION ( 'NONE',  ( -1.000000000000000000, 0.000000000000000000, 0.000000000000000000 ) ) ;
#47064 = ORIENTED_EDGE ( 'NONE', *, *, #40719, .F. ) ;
#47065 = VERTEX_POINT ( 'NONE', #46123 ) ;
#47066 = CARTESIAN_POINT ( 'NONE',  ( 25.50000000000000355, -5.200000000000001066, -20.49999999999999645 ) ) ;
#47067 = EDGE_CURVE ( 'NONE', #23915, #22764, #40818, .T. ) ;
#47068 = FACE_OUTER_BOUND ( 'NONE', #42190, .T. ) ;
#47069 = ORIENTED_EDGE ( 'NONE', *, *, #5649, .F. ) ;
#47070 = EDGE_CURVE ( 'NONE', #190, #23182, #46813, .T. ) ;
#47071 = DIRECTION ( 'NONE',  ( 0.000000000000000000, 0.000000000000000000, 1.000000000000000000 ) ) ;
#47072 = PLANE ( 'NONE',  #40707 ) ;
#47073 = AXIS2_PLACEMENT_3D ( 'NONE', #2121, #45237, #44543 ) ;
#47075 = VERTEX_POINT ( 'NONE', #10054 ) ;
#47074 = CARTESIAN_POINT ( 'NONE',  ( -7.593516549646711411, 11.77351654964660277, 455.0000000000000568 ) ) ;
#47076 = ORIENTED_EDGE ( 'NONE', *, *, #53075, .F. ) ;
#47077 = PLANE ( 'NONE',  #10180 ) ;
#47078 = VECTOR ( 'NONE', #35213, 1000.000000000000000 ) ;
#47079 = DIRECTION ( 'NONE',  ( 0.000000000000000000, 0.000000000000000000, -1.000000000000000000 ) ) ;
#47080 = ADVANCED_FACE ( 'NONE', ( #63795 ), #47525, .T. ) ;
#47081 = CARTESIAN_POINT ( 'NONE',  ( 9.690000000000001279, -9.690000000000001279, 0.000000000000000000 ) ) ;
#47082 = CARTESIAN_POINT ( 'NONE',  ( 11.12648345035337982, -4.206483450353396769, 195.0000000000000284 ) ) ;
#47083 = CARTESIAN_POINT ( 'NONE',  ( -7.450000000000001954, 7.250000000000000000, -21.50000000000000000 ) ) ;
#47084 = CIRCLE ( 'NONE', #10996, 2.250000000000001776 ) ;
#47085 = VECTOR ( 'NONE', #29303, 1000.000000000000000 ) ;
#47086 = DIRECTION ( 'NONE',  ( 0.000000000000000000, -0.5017180897718492849, 0.8650311892618014475 ) ) ;
#47087 = ORIENTED_EDGE ( 'NONE', *, *, #46976, .T. ) ;
#47088 = LINE ( 'NONE', #68660, #13457 ) ;
#47090 = ORIENTED_EDGE ( 'NONE', *, *, #28525, .T. ) ;
#47089 = DIRECTION ( 'NONE',  ( 9.912705577010336396E-15, 1.000000000000000000, 0.000000000000000000 ) ) ;
#47092 = CARTESIAN_POINT ( 'NONE',  ( -14.25000000000000000, -2.500000000000000000, -23.22168783648699986 ) ) ;
#47091 = VECTOR ( 'NONE', #5586, 1000.000000000000000 ) ;
#47093 = CARTESIAN_POINT ( 'NONE',  ( 36.90000000000000568, -0.1999999999911795112, 8.826273045769999343E-12 ) ) ;
#47094 = FACE_OUTER_BOUND ( 'NONE', #29134, .T. ) ;
#47095 = CARTESIAN_POINT ( 'NONE',  ( 30.00000000000000000, -17.35230188589299871, -15.35019951917099945 ) ) ;
#47096 = CIRCLE ( 'NONE', #23364, 0.8100000000000017186 ) ;
#47097 = VECTOR ( 'NONE', #55810, 1000.000000000000114 ) ;
#47098 = ORIENTED_EDGE ( 'NONE', *, *, #23119, .T. ) ;
#47099 = LINE ( 'NONE', #25179, #37664 ) ;
#47100 = CARTESIAN_POINT ( 'NONE',  ( 41.09999999999999432, 13.66939075806899950, 20.80000000000000426 ) ) ;
#47101 = VERTEX_POINT ( 'NONE', #58131 ) ;
#47102 = EDGE_CURVE ( 'NONE', #49409, #43101, #69092, .T. ) ;
#47103 = DIRECTION ( 'NONE',  ( 1.000000000000000000, -0.000000000000000000, 0.000000000000000000 ) ) ;
#47104 = CARTESIAN_POINT ( 'NONE',  ( 7.250000000000005329, -8.249999999999998224, -17.00000000000000000 ) ) ;
#47105 = EDGE_CURVE ( 'NONE', #11772, #56785, #50579, .T. ) ;
#47106 = B_SPLINE_CURVE_WITH_KNOTS ( 'NONE', 3,
 ( #14696, #46164, #51475, #19294, #41569, #36609 ),
 .UNSPECIFIED., .F., .F.,
 ( 4, 2, 4 ),
 ( 0.0002380763768132232450, 0.7291065797294586925, 1.457975083082104106 ),
 .UNSPECIFIED. ) ;
#47107 = VECTOR ( 'NONE', #62907, 999.9999999999998863 ) ;
#47108 = DIRECTION ( 'NONE',  ( -1.000000000000000000, 0.000000000000000000, 0.000000000000000000 ) ) ;
#47109 = EDGE_LOOP ( 'NONE', ( #49846, #49264, #44245, #27530, #20557, #46673, #19669, #20718, #50888, #54019, #17832, #33015, #45258, #63356, #42545, #58011, #65676, #57593, #34382, #15897, #2736, #23575, #63932, #54574, #29554, #37750, #65401, #36703, #23826, #48866, #5514, #44077, #32376, #4445, #44641, #33833, #589, #21057, #48919, #63844, #59208, #44413, #51452, #55660, #20464, #10207, #24254, #37295, #17951, #15981, #39348, #37785, #49517, #46932, #54519, #20002, #52066, #26242, #38601, #45493, #12164, #38700, #21424, #48976, #50915, #64461, #21918, #37519, #29559, #451, #20238, #4054, #30281, #50054, #39197, #58756, #22541, #22586, #336, #59956, #31512, #54268, #1118, #57634, #56004, #5903, #36330, #29906, #57296, #9057, #20412, #1615, #10252, #30740, #54798, #32882, #23862, #40646, #55177, #63642, #67584, #68184, #55723, #31060, #58016, #44358, #24172, #10254, #38292, #30695, #52681, #67030, #64975, #52126, #2903, #42692, #2928, #13216, #36159, #50173, #57457, #16244, #10352, #5323, #15067, #65022, #13122, #49578, #49573, #4380, #55397, #36180, #51814, #35377, #30078, #57218, #23333, #57182, #29781, #57536, #50604, #16735, #65653, #24640, #38220, #21171, #28072, #46113, #2105, #21211, #28409, #21835, #33668, #46940, #16555, #30588, #33647, #7421, #50913, #21455, #60275, #17378, #65742, #1019, #64274, #58223, #23821, #37188, #52983, #13378, #42812, #7100, #25760, #13753, #57214, #4586, #38371, #45342, #1329, #26554, #45516, #44858, #22067, #11293, #66354, #34509, #52373, #24210, #6123, #19546, #7736, #46311, #17527, #13499, #59494, #59028, #41669, #66859, #67254, #31679, #18883, #38360, #59206, #56574, #5021, #33986, #60947, #41097, #31730, #12414, #45881, #69288, #37908, #25710 ) ) ;
#47110 = CARTESIAN_POINT ( 'NONE',  ( -7.250000000000000000, -7.449999999999998401, -7.000000000000000000 ) ) ;
#47111 = ORIENTED_EDGE ( 'NONE', *, *, #14962, .T. ) ;
#47112 = EDGE_CURVE ( 'NONE', #40446, #997, #64183, .T. ) ;
#47113 = ORIENTED_EDGE ( 'NONE', *, *, #30391, .F. ) ;
#47114 = DIRECTION ( 'NONE',  ( -1.000000000000000000, 0.000000000000000000, 0.000000000000000000 ) ) ;
#47115 = FACE_OUTER_BOUND ( 'NONE', #1400, .T. ) ;
#47116 = LINE ( 'NONE', #27209, #22099 ) ;
#47117 = EDGE_CURVE ( 'NONE', #13055, #6004, #5796, .T. ) ;
#47118 = CARTESIAN_POINT ( 'NONE',  ( 49.00000000000000000, -0.1999999999911795112, 8.826273045769999343E-12 ) ) ;
#47119 = ADVANCED_FACE ( 'NONE', ( #54237 ), #21704, .F. ) ;
#47120 = DIRECTION ( 'NONE',  ( -1.000000000000000000, 0.000000000000000000, 0.000000000000000000 ) ) ;
#47121 = VERTEX_POINT ( 'NONE', #58841 ) ;
#47122 = ORIENTED_EDGE ( 'NONE', *, *, #19091, .T. ) ;
#47124 = VERTEX_POINT ( 'NONE', #38317 ) ;
#47123 = LINE ( 'NONE', #57014, #5818 ) ;
#47125 = ORIENTED_EDGE ( 'NONE', *, *, #38577, .F. ) ;
#47126 = CARTESIAN_POINT ( 'NONE',  ( 25.50000000000000355, -17.50000000000000000, -22.50000000000000000 ) ) ;
#47127 = DIRECTION ( 'NONE',  ( -1.000000000000000000, 0.000000000000000000, 0.000000000000000000 ) ) ;
#47128 = CARTESIAN_POINT ( 'NONE',  ( -7.250000000000000888, 7.250000000000001776, -16.50000000000000000 ) ) ;
#47129 = VECTOR ( 'NONE', #52678, 1000.000000000000000 ) ;
#47130 = EDGE_CURVE ( 'NONE', #47065, #58190, #64843, .T. ) ;
#47131 = LINE ( 'NONE', #59130, #37866 ) ;
#47133 = DIRECTION ( 'NONE',  ( 0.000000000000000000, 0.000000000000000000, -1.000000000000000000 ) ) ;
#47132 = CARTESIAN_POINT ( 'NONE',  ( 15.00000000000000000, -21.00000000000000000, 4.000000000000000000 ) ) ;
#47134 = ORIENTED_EDGE ( 'NONE', *, *, #66736, .F. ) ;
#47135 = ORIENTED_EDGE ( 'NONE', *, *, #11516, .T. ) ;
#47136 = ORIENTED_EDGE ( 'NONE', *, *, #67128, .F. ) ;
#47137 = EDGE_CURVE ( 'NONE', #46196, #51028, #43260, .T. ) ;
#47138 = EDGE_CURVE ( 'NONE', #17638, #43882, #4747, .T. ) ;
#47139 = AXIS2_PLACEMENT_3D ( 'NONE', #10463, #5172, #37689 ) ;
#47140 = ORIENTED_EDGE ( 'NONE', *, *, #21431, .T. ) ;
#47141 = CYLINDRICAL_SURFACE ( 'NONE', #620, 3.499999999999850342 ) ;
#47142 = CARTESIAN_POINT ( 'NONE',  ( -8.689999999999999503, -9.750000000000001776, -7.000000000000000000 ) ) ;
#47143 = EDGE_CURVE ( 'NONE', #55385, #64507, #26309, .T. ) ;
#47144 =( NAMED_UNIT ( * ) SI_UNIT ( $, .STERADIAN. ) SOLID_ANGLE_UNIT ( ) );
#47145 = VECTOR ( 'NONE', #59547, 1000.000000000000000 ) ;
#47146 = VECTOR ( 'NONE', #54645, 1000.000000000000000 ) ;
#47147 = DIRECTION ( 'NONE',  ( 0.000000000000000000, 0.000000000000000000, 1.000000000000000000 ) ) ;
#47148 = ORIENTED_EDGE ( 'NONE', *, *, #20268, .F. ) ;
#47149 = ORIENTED_EDGE ( 'NONE', *, *, #63819, .F. ) ;
#47150 = VERTEX_POINT ( 'NONE', #6134 ) ;
#47151 = CARTESIAN_POINT ( 'NONE',  ( 0.000000000000000000, -8.249999999999998224, -10.00000000000000000 ) ) ;
#47152 = VECTOR ( 'NONE', #7226, 1000.000000000000000 ) ;
#47153 = AXIS2_PLACEMENT_3D ( 'NONE', #46242, #8770, #67819 ) ;
#47154 = ORIENTED_EDGE ( 'NONE', *, *, #37659, .F. ) ;
#47155 = VERTEX_POINT ( 'NONE', #11426 ) ;
#47156 = DIRECTION ( 'NONE',  ( -1.000000000000000000, 0.000000000000000000, 0.000000000000000000 ) ) ;
#47157 = ORIENTED_EDGE ( 'NONE', *, *, #17736, .T. ) ;
#47158 = EDGE_LOOP ( 'NONE', ( #45980, #32227, #55888, #32628 ) ) ;
#47159 = CARTESIAN_POINT ( 'NONE',  ( -8.452095193409434160, -4.255011587777239868, 455.0000000000000568 ) ) ;
#47160 = EDGE_CURVE ( 'NONE', #40034, #67224, #22048, .T. ) ;
#47162 = VERTEX_POINT ( 'NONE', #65198 ) ;
#47161 = CARTESIAN_POINT ( 'NONE',  ( -10.19191654964686933, -11.48848345035334795, 455.0000000000000568 ) ) ;
#47163 = ORIENTED_EDGE ( 'NONE', *, *, #3839, .F. ) ;
#47164 = ADVANCED_FACE ( 'NONE', ( #47869 ), #37975, .F. ) ;
#47165 = VECTOR ( 'NONE', #7664, 1000.000000000000000 ) ;
#47166 = LINE ( 'NONE', #3673, #43120 ) ;
#47167 = DIRECTION ( 'NONE',  ( -3.903627567395476653E-15, -1.000000000000000000, -1.836970198721029194E-16 ) ) ;
#47169 = VERTEX_POINT ( 'NONE', #59537 ) ;
#47168 = LINE ( 'NONE', #68734, #792 ) ;
#47170 = VERTEX_POINT ( 'NONE', #10397 ) ;
#47171 = DIRECTION ( 'NONE',  ( 0.000000000000000000, 0.000000000000000000, -1.000000000000000000 ) ) ;
#47172 = DIRECTION ( 'NONE',  ( -1.000000000000000000, 1.794541526872559352E-16, 0.000000000000000000 ) ) ;
#47173 = LINE ( 'NONE', #20287, #4148 ) ;
#47174 = CARTESIAN_POINT ( 'NONE',  ( 34.89999999999999858, -14.06939075806900163, -20.80000000000000426 ) ) ;
#47175 = EDGE_LOOP ( 'NONE', ( #4625, #47051, #51029, #37258 ) ) ;
#47176 = LINE ( 'NONE', #24199, #11147 ) ;
#47177 = CARTESIAN_POINT ( 'NONE',  ( -7.259684009079930611, 4.188533722949235205, 455.0000000000000568 ) ) ;
#47178 = FACE_OUTER_BOUND ( 'NONE', #54101, .T. ) ;
#47179 = VECTOR ( 'NONE', #60566, 1000.000000000000000 ) ;
#47180 = ORIENTED_EDGE ( 'NONE', *, *, #45240, .F. ) ;
#47181 = CARTESIAN_POINT ( 'NONE',  ( -28.00000000000000000, -17.50000000000000000, -20.05051025721700242 ) ) ;
#47182 = CARTESIAN_POINT ( 'NONE',  ( 7.357023737882817827, -5.552858015815587578, 54.00000000000000711 ) ) ;
#47183 = CARTESIAN_POINT ( 'NONE',  ( 9.106483450353380249, -10.92648345035348711, 455.0000000000000568 ) ) ;
#47184 = VERTEX_POINT ( 'NONE', #22403 ) ;
#47185 = AXIS2_PLACEMENT_3D ( 'NONE', #6276, #65339, #43064 ) ;
#47186 = CARTESIAN_POINT ( 'NONE',  ( 41.09999999999999432, -0.2000000000089119934, -8.913009219568841313E-12 ) ) ;
#47187 = DIRECTION ( 'NONE',  ( 0.000000000000000000, -1.000000000000000000, -1.838806884531994514E-12 ) ) ;
#47188 = CIRCLE ( 'NONE', #18912, 4.000000000000000888 ) ;
#47189 = ADVANCED_FACE ( 'NONE', ( #16051 ), #59184, .T. ) ;
#47190 = CIRCLE ( 'NONE', #62982, 1.000000000000000000 ) ;
#47191 = CYLINDRICAL_SURFACE ( 'NONE', #8974, 1.000000000000000000 ) ;
#47192 = ORIENTED_EDGE ( 'NONE', *, *, #2679, .T. ) ;
#47193 = DIRECTION ( 'NONE',  ( 0.000000000000000000, 0.000000000000000000, 1.000000000000000000 ) ) ;
#47195 = CARTESIAN_POINT ( 'NONE',  ( 9.912023737882801555, 6.642976262117184838, 54.00000000000000711 ) ) ;
#47194 = VECTOR ( 'NONE', #32901, 1000.000000000000000 ) ;
#47196 = CARTESIAN_POINT ( 'NONE',  ( 4.622483450353380263, -3.606483450353395792, 195.0000000000000284 ) ) ;
#47197 = EDGE_CURVE ( 'NONE', #65847, #24983, #60759, .T. ) ;
#47198 = CARTESIAN_POINT ( 'NONE',  ( -11.99351654964671354, 7.813516549646603693, 455.0000000000000568 ) ) ;
#47199 =( GEOMETRIC_REPRESENTATION_CONTEXT ( 3 ) GLOBAL_UNCERTAINTY_ASSIGNED_CONTEXT ( ( #26025 ) ) GLOBAL_UNIT_ASSIGNED_CONTEXT ( ( #19999, #36253, #27396 ) ) REPRESENTATION_CONTEXT ( 'NONE', 'WORKASPACE' ) );
#47200 = CARTESIAN_POINT ( 'NONE',  ( 275.0000000000000000, -25.60000000000000142, 17.60000000000000142 ) ) ;
#47201 = ORIENTED_EDGE ( 'NONE', *, *, #51981, .T. ) ;
#47202 = CARTESIAN_POINT ( 'NONE',  ( -9.689726262117330791, -10.05377373788272699, 54.00000000000000711 ) ) ;
#47203 = CARTESIAN_POINT ( 'NONE',  ( 21.90000000000000213, 0.000000000000000000, 1.508455196501571824E-15 ) ) ;
#47204 = EDGE_CURVE ( 'NONE', #65422, #47230, #48928, .T. ) ;
#47205 = ADVANCED_FACE ( 'NONE', ( #486 ), #48233, .T. ) ;
#47206 = CARTESIAN_POINT ( 'NONE',  ( 29.50000000000000355, -11.50000000000000000, -15.00000000000000000 ) ) ;
#47207 = LINE ( 'NONE', #10418, #60301 ) ;
#47208 = ADVANCED_FACE ( 'NONE', ( #27696 ), #43951, .F. ) ;
#47209 = CARTESIAN_POINT ( 'NONE',  ( 4.149127210878726935, -3.677663764522637546, 26.00000000000000711 ) ) ;
#47210 = EDGE_CURVE ( 'NONE', #22923, #54282, #17084, .T. ) ;
#47211 = ORIENTED_EDGE ( 'NONE', *, *, #5210, .T. ) ;
#47213 = ORIENTED_EDGE ( 'NONE', *, *, #22093, .F. ) ;
#47212 = DIRECTION ( 'NONE',  ( 1.000000000000000000, 0.000000000000000000, 0.000000000000000000 ) ) ;
#47214 = VECTOR ( 'NONE', #45065, 1000.000000000000000 ) ;
#47215 = EDGE_CURVE ( 'NONE', #7152, #11562, #24684, .T. ) ;
#47216 = LINE ( 'NONE', #32000, #53105 ) ;
#47217 = DIRECTION ( 'NONE',  ( -0.000000000000000000, -0.000000000000000000, 1.000000000000000000 ) ) ;
#47218 = CARTESIAN_POINT ( 'NONE',  ( 39.00000000000000000, 21.00000000000000000, -13.98999642601811999 ) ) ;
#47219 = ORIENTED_EDGE ( 'NONE', *, *, #54401, .T. ) ;
#47220 = DIRECTION ( 'NONE',  ( 0.000000000000000000, 0.000000000000000000, -1.000000000000000000 ) ) ;
#47221 = DIRECTION ( 'NONE',  ( -0.000000000000000000, 3.673940397442059868E-16, -1.000000000000000000 ) ) ;
#47222 = ORIENTED_EDGE ( 'NONE', *, *, #28965, .T. ) ;
#47223 = VERTEX_POINT ( 'NONE', #42915 ) ;
#47224 = EDGE_LOOP ( 'NONE', ( #44597, #43468, #34069, #67722, #2207, #64628, #15276, #22285 ) ) ;
#47225 = DIRECTION ( 'NONE',  ( 0.000000000000000000, -3.673940397442059868E-16, 1.000000000000000000 ) ) ;
#47226 = LINE ( 'NONE', #46854, #5004 ) ;
#47227 = DIRECTION ( 'NONE',  ( -0.000000000000000000, 1.000000000000000000, -0.000000000000000000 ) ) ;
#47228 = CYLINDRICAL_SURFACE ( 'NONE', #69814, 1.000000000000000000 ) ;
#47229 = EDGE_LOOP ( 'NONE', ( #1064, #13711, #42101, #19792, #6764, #49489, #64174, #39106 ) ) ;
#47230 = VERTEX_POINT ( 'NONE', #45676 ) ;
#47231 = DIRECTION ( 'NONE',  ( 0.000000000000000000, 0.000000000000000000, 1.000000000000000000 ) ) ;
#47232 = DIRECTION ( 'NONE',  ( 0.4999999999999827360, 0.000000000000000000, 0.8660254037844485886 ) ) ;
#47233 = ORIENTED_EDGE ( 'NONE', *, *, #49443, .T. ) ;
#47234 = ORIENTED_EDGE ( 'NONE', *, *, #22531, .F. ) ;
#47235 = ORIENTED_EDGE ( 'NONE', *, *, #41065, .F. ) ;
#47236 = ORIENTED_EDGE ( 'NONE', *, *, #67389, .T. ) ;
#47237 = CARTESIAN_POINT ( 'NONE',  ( 8.406483450353379183, -6.344579767990935260, 455.0000000000000568 ) ) ;
#47238 = UNCERTAINTY_MEASURE_WITH_UNIT (LENGTH_MEASURE( 1.000000000000000082E-05 ), #41232, 'distance_accuracy_value', 'NONE');
#47240 = ORIENTED_EDGE ( 'NONE', *, *, #60072, .T. ) ;
#47239 = CARTESIAN_POINT ( 'NONE',  ( -8.393516549646744096, -7.616533956692189022, 195.0000000000000284 ) ) ;
#47241 = CIRCLE ( 'NONE', #23502, 4.000000000000000000 ) ;
#47242 = FACE_OUTER_BOUND ( 'NONE', #20743, .T. ) ;
#47243 = EDGE_CURVE ( 'NONE', #16302, #7103, #42759, .T. ) ;
#47244 = CARTESIAN_POINT ( 'NONE',  ( 9.189999999999999503, 9.750000000000000000, -5.000000000000000000 ) ) ;
#47245 = CARTESIAN_POINT ( 'NONE',  ( 38.90000000000000568, 3.010794155703768650E-16, -2.458500000000000796 ) ) ;
#47246 = EDGE_LOOP ( 'NONE', ( #68820, #50091, #26054, #49495, #426, #37163, #29702, #62787 ) ) ;
#47247 = ADVANCED_FACE ( 'NONE', ( #33685 ), #39363, .T. ) ;
#47248 = ORIENTED_EDGE ( 'NONE', *, *, #9205, .F. ) ;
#47249 = VECTOR ( 'NONE', #13386, 1000.000000000000000 ) ;
#47250 = ADVANCED_FACE ( 'NONE', ( #55264 ), #44288, .T. ) ;
#47251 = EDGE_CURVE ( 'NONE', #64694, #67710, #18111, .T. ) ;
#47252 = DIRECTION ( 'NONE',  ( 1.836970198721029934E-16, 1.836970198721010706E-16, -1.000000000000000000 ) ) ;
#47253 = FACE_OUTER_BOUND ( 'NONE', #3769, .T. ) ;
#47254 = ORIENTED_EDGE ( 'NONE', *, *, #34405, .F. ) ;
#47255 = CARTESIAN_POINT ( 'NONE',  ( 7.450000000000004619, -1.336933437520057563E-15, -14.50000000000000000 ) ) ;
#47256 = CARTESIAN_POINT ( 'NONE',  ( 176.0064834503533575, -29.83962462487173894, 0.000000000000000000 ) ) ;
#47257 = CARTESIAN_POINT ( 'NONE',  ( 29.50000000000000355, -11.70000000000000284, 11.00000000000000000 ) ) ;
#47258 = ORIENTED_EDGE ( 'NONE', *, *, #42173, .F. ) ;
#47259 = CARTESIAN_POINT ( 'NONE',  ( 7.250000000000005329, 7.250000000000000888, -24.50000000000000000 ) ) ;
#47260 = DIRECTION ( 'NONE',  ( 0.000000000000000000, 1.000000000000000000, 0.000000000000000000 ) ) ;
#47261 = CARTESIAN_POINT ( 'NONE',  ( 0.000000000000000000, 0.000000000000000000, -29.90000000000000924 ) ) ;
#47262 = PLANE ( 'NONE',  #33618 ) ;
#47263 = CARTESIAN_POINT ( 'NONE',  ( 11.00000000000000000, -13.79999999999979998, 17.30000000000000071 ) ) ;
#47264 = ORIENTED_EDGE ( 'NONE', *, *, #9372, .F. ) ;
#47265 = CARTESIAN_POINT ( 'NONE',  ( -8.130476262117259267, 9.547976262117177981, 54.00000000000000711 ) ) ;
#47266 = CARTESIAN_POINT ( 'NONE',  ( 73.77321854994620765, 47.95351654967443977, 25.00000000000000000 ) ) ;
#47267 = DIRECTION ( 'NONE',  ( -1.000000000000000000, 1.610765207321970913E-14, 1.836970198721059516E-16 ) ) ;
#47268 = EDGE_CURVE ( 'NONE', #65337, #47349, #49943, .T. ) ;
#47269 = CARTESIAN_POINT ( 'NONE',  ( -7.450000000000001954, 0.000000000000000000, -7.500000000000000000 ) ) ;
#47270 = CARTESIAN_POINT ( 'NONE',  ( 10.31452373788279964, 6.642976262117187503, 26.00000000000000711 ) ) ;
#47271 = FACE_OUTER_BOUND ( 'NONE', #3625, .T. ) ;
#47272 = CYLINDRICAL_SURFACE ( 'NONE', #52205, 1.000000000000000000 ) ;
#47273 = ORIENTED_EDGE ( 'NONE', *, *, #14059, .F. ) ;
#47274 = CARTESIAN_POINT ( 'NONE',  ( 15.08565937784311117, -0.3156604612129225162, 23.70415600323552852 ) ) ;
#47275 = CARTESIAN_POINT ( 'NONE',  ( -7.342976262117277386, -5.552858015815541393, 26.00000000000000711 ) ) ;
#47276 = LINE ( 'NONE', #15104, #52677 ) ;
#47277 = CARTESIAN_POINT ( 'NONE',  ( -10.49297626211725110, -3.664523737882711352, 54.00000000000000711 ) ) ;
#47278 = CARTESIAN_POINT ( 'NONE',  ( -4.706725378239216440, 6.344366288193329595, 54.00000000000000711 ) ) ;
#47279 = DIRECTION ( 'NONE',  ( 1.000000000000000000, 0.000000000000000000, 0.000000000000000000 ) ) ;
#47280 = EDGE_CURVE ( 'NONE', #16692, #9544, #65333, .T. ) ;
#47281 = DIRECTION ( 'NONE',  ( 0.000000000000000000, 0.000000000000000000, 1.000000000000000000 ) ) ;
#47282 = EDGE_CURVE ( 'NONE', #15112, #56088, #66466, .T. ) ;
#47283 = ORIENTED_EDGE ( 'NONE', *, *, #67053, .F. ) ;
#47284 = VECTOR ( 'NONE', #31024, 1000.000000000000000 ) ;
#47285 = VERTEX_POINT ( 'NONE', #65863 ) ;
#47286 = EDGE_CURVE ( 'NONE', #32555, #63705, #50292, .T. ) ;
#47287 = DIRECTION ( 'NONE',  ( -1.836970198721029934E-16, 1.836970198721036590E-16, -1.000000000000000000 ) ) ;
#47288 = DIRECTION ( 'NONE',  ( 0.000000000000000000, 1.000000000000000000, 0.000000000000000000 ) ) ;
#47289 = ORIENTED_EDGE ( 'NONE', *, *, #14695, .F. ) ;
#47290 = LINE ( 'NONE', #62477, #44991 ) ;
#47291 = VECTOR ( 'NONE', #68561, 1000.000000000000000 ) ;
#47292 = DIRECTION ( 'NONE',  ( 0.000000000000000000, 0.000000000000000000, -1.000000000000000000 ) ) ;
#47293 = ORIENTED_EDGE ( 'NONE', *, *, #69567, .T. ) ;
#47294 = DIRECTION ( 'NONE',  ( 0.000000000000000000, 1.000000000000000000, 0.000000000000000000 ) ) ;
#47295 = VERTEX_POINT ( 'NONE', #34359 ) ;
#47296 = ORIENTED_EDGE ( 'NONE', *, *, #57472, .F. ) ;
#47297 = PLANE ( 'NONE',  #62216 ) ;
#47298 = ORIENTED_EDGE ( 'NONE', *, *, #2810, .T. ) ;
#47299 = VECTOR ( 'NONE', #27092, 1000.000000000000000 ) ;
#47300 = CARTESIAN_POINT ( 'NONE',  ( 6.849523737882817542, -10.50702373788282529, 54.00000000000000711 ) ) ;
#47301 = CARTESIAN_POINT ( 'NONE',  ( 7.250000000000005329, 7.250000000000000888, -22.00000000000000000 ) ) ;
#47302 = DIRECTION ( 'NONE',  ( -0.000000000000000000, 3.673940397442059868E-16, -1.000000000000000000 ) ) ;
#47303 = ORIENTED_EDGE ( 'NONE', *, *, #17026, .T. ) ;
#47304 = DIRECTION ( 'NONE',  ( -3.491481338843132961E-15, -1.000000000000000000, 0.000000000000000000 ) ) ;
#47306 = CARTESIAN_POINT ( 'NONE',  ( -1.853252480934882929, -9.417013320880883498, 455.0000000000000568 ) ) ;
#47305 = CARTESIAN_POINT ( 'NONE',  ( 78.77321854994620765, 47.95351654967443977, 20.00000000000000000 ) ) ;
#47307 = ORIENTED_EDGE ( 'NONE', *, *, #69856, .T. ) ;
#47308 = ORIENTED_EDGE ( 'NONE', *, *, #10460, .T. ) ;
#47309 = ORIENTED_EDGE ( 'NONE', *, *, #11395, .T. ) ;
#47311 = ORIENTED_EDGE ( 'NONE', *, *, #27594, .T. ) ;
#47310 = APPLICATION_PROTOCOL_DEFINITION ( 'draft international standard', 'automotive_design', 1998, #35891 ) ;
#47312 = LINE ( 'NONE', #48366, #64963 ) ;
#47314 = ORIENTED_EDGE ( 'NONE', *, *, #26728, .F. ) ;
#47313 = DIRECTION ( 'NONE',  ( 1.000000000000000000, -0.000000000000000000, -0.000000000000000000 ) ) ;
#47315 = PLANE ( 'NONE',  #33369 ) ;
#47316 = LINE ( 'NONE', #26455, #22683 ) ;
#47317 = EDGE_LOOP ( 'NONE', ( #11112, #31880, #30970, #44332 ) ) ;
#47318 = VERTEX_POINT ( 'NONE', #18817 ) ;
#47319 = EDGE_CURVE ( 'NONE', #2487, #61865, #34723, .T. ) ;
#47320 = ADVANCED_FACE ( 'NONE', ( #60562 ), #44986, .T. ) ;
#47321 = EDGE_CURVE ( 'NONE', #4210, #36995, #28074, .T. ) ;
#47322 = DIRECTION ( 'NONE',  ( 0.000000000000000000, 0.000000000000000000, -1.000000000000000000 ) ) ;
#47323 = ORIENTED_EDGE ( 'NONE', *, *, #32352, .T. ) ;
#47324 = EDGE_CURVE ( 'NONE', #47809, #10522, #55175, .T. ) ;
#47325 = AXIS2_PLACEMENT_3D ( 'NONE', #67731, #44751, #56765 ) ;
#47326 = DIRECTION ( 'NONE',  ( 1.836970198721029934E-16, -1.836970198721036344E-16, 1.000000000000000000 ) ) ;
#47327 = DIRECTION ( 'NONE',  ( -0.000000000000000000, -0.000000000000000000, -1.000000000000000000 ) ) ;
#47328 = CARTESIAN_POINT ( 'NONE',  ( -17.24945551514599984, -17.50000000000000000, -25.53140320652400064 ) ) ;
#47329 = VERTEX_POINT ( 'NONE', #28046 ) ;
#47330 = AXIS2_PLACEMENT_3D ( 'NONE', #44573, #1450, #23021 ) ;
#47331 = DIRECTION ( 'NONE',  ( 4.745709458399858621E-16, 1.000000000000000000, 1.836970198721035604E-16 ) ) ;
#47333 = ORIENTED_EDGE ( 'NONE', *, *, #54030, .T. ) ;
#47332 = DIRECTION ( 'NONE',  ( -0.000000000000000000, -0.000000000000000000, -1.000000000000000000 ) ) ;
#47335 = ORIENTED_EDGE ( 'NONE', *, *, #7685, .T. ) ;
#47334 = PLANE ( 'NONE',  #11699 ) ;
#47336 = LINE ( 'NONE', #63255, #39950 ) ;
#47337 = AXIS2_PLACEMENT_3D ( 'NONE', #25964, #54228, #27353 ) ;
#47338 = CARTESIAN_POINT ( 'NONE',  ( 30.00000000000000000, -12.00000000000000000, 11.03137303340310282 ) ) ;
#47339 = LINE ( 'NONE', #4569, #62955 ) ;
#47340 = PLANE ( 'NONE',  #21566 ) ;
#47341 = CIRCLE ( 'NONE', #56367, 0.1999999999999987899 ) ;
#47342 = FACE_OUTER_BOUND ( 'NONE', #62565, .T. ) ;
#47343 = ORIENTED_EDGE ( 'NONE', *, *, #15756, .F. ) ;
#47344 = CARTESIAN_POINT ( 'NONE',  ( 9.703773737882817940, 10.03972626211715280, 54.00000000000000711 ) ) ;
#47345 = DIRECTION ( 'NONE',  ( 1.000000000000000000, 0.000000000000000000, 0.000000000000000000 ) ) ;
#47346 = PRESENTATION_STYLE_ASSIGNMENT (( #52673 ) ) ;
#47347 = VECTOR ( 'NONE', #64850, 1000.000000000000000 ) ;
#47349 = VERTEX_POINT ( 'NONE', #23774 ) ;
#47348 = CARTESIAN_POINT ( 'NONE',  ( 8.250000000000005329, -7.249999999999998224, -7.500000000000000000 ) ) ;
#47350 = DIRECTION ( 'NONE',  ( 0.000000000000000000, 0.000000000000000000, -1.000000000000000000 ) ) ;
#47351 = LINE ( 'NONE', #48053, #17206 ) ;
#47352 = CIRCLE ( 'NONE', #54134, 1.224999999999999423 ) ;
#47353 = LINE ( 'NONE', #15188, #4055 ) ;
#47354 = ORIENTED_EDGE ( 'NONE', *, *, #38493, .T. ) ;
#47355 = CARTESIAN_POINT ( 'NONE',  ( 15.50000000000000000, -0.4000000000005274892, -19.20000000000052864 ) ) ;
#47356 = CARTESIAN_POINT ( 'NONE',  ( -7.450000000000001954, -7.249999999999998224, -25.50000000000000355 ) ) ;
#47357 = ORIENTED_EDGE ( 'NONE', *, *, #26527, .F. ) ;
#47358 = CARTESIAN_POINT ( 'NONE',  ( -11.47551654964683010, -11.08848345035333338, 455.0000000000000568 ) ) ;
#47359 = CARTESIAN_POINT ( 'NONE',  ( -30.00000000000000000, -5.599999999999999645, -9.000000000000001776 ) ) ;
#47360 = CARTESIAN_POINT ( 'NONE',  ( 9.912023737882815766, -3.857023737882825820, 54.00000000000000711 ) ) ;
#47361 = LINE ( 'NONE', #42757, #24878 ) ;
#47362 = EDGE_CURVE ( 'NONE', #46672, #45646, #39338, .T. ) ;
#47363 = LINE ( 'NONE', #29690, #29713 ) ;
#47364 = EDGE_LOOP ( 'NONE', ( #28772, #1251, #41804, #13361, #47926, #57278, #58891, #17441, #35980, #36145, #61278, #48282 ) ) ;
#47365 = EDGE_CURVE ( 'NONE', #16188, #26187, #61232, .T. ) ;
#47366 = ORIENTED_EDGE ( 'NONE', *, *, #50409, .F. ) ;
#47367 = FACE_OUTER_BOUND ( 'NONE', #33664, .T. ) ;
#47368 = ORIENTED_EDGE ( 'NONE', *, *, #59332, .T. ) ;
#47369 = ADVANCED_FACE ( 'NONE', ( #34022 ), #61582, .T. ) ;
#47370 = ORIENTED_EDGE ( 'NONE', *, *, #13817, .F. ) ;
#47371 = CARTESIAN_POINT ( 'NONE',  ( 7.250000000000005329, 7.250000000000000888, -8.000000000000000000 ) ) ;
#47372 = EDGE_CURVE ( 'NONE', #34850, #14942, #4374, .T. ) ;
#47373 = DIRECTION ( 'NONE',  ( -0.000000000000000000, 0.000000000000000000, -1.000000000000000000 ) ) ;
#47374 = CARTESIAN_POINT ( 'NONE',  ( 8.900000000000005684, -0.1999999999911430404, -8.864436962241481021E-12 ) ) ;
#47375 = ORIENTED_EDGE ( 'NONE', *, *, #8840, .F. ) ;
#47376 = EDGE_CURVE ( 'NONE', #6322, #14837, #49607, .T. ) ;
#47377 = ORIENTED_EDGE ( 'NONE', *, *, #60866, .T. ) ;
#47378 = DIRECTION ( 'NONE',  ( 1.000000000000000000, 0.000000000000000000, 0.000000000000000000 ) ) ;
#47379 = VECTOR ( 'NONE', #47287, 1000.000000000000000 ) ;
#47381 = ORIENTED_EDGE ( 'NONE', *, *, #55725, .F. ) ;
#47380 = EDGE_CURVE ( 'NONE', #7833, #57470, #30335, .T. ) ;
#47382 = CIRCLE ( 'NONE', #23637, 4.000000000000000888 ) ;
#47383 = ORIENTED_EDGE ( 'NONE', *, *, #66898, .F. ) ;
#47384 = CARTESIAN_POINT ( 'NONE',  ( 9.690000000000001279, 8.750000000000000000, -5.000000000000000000 ) ) ;
#47385 = LINE ( 'NONE', #31489, #48265 ) ;
#47386 = LINE ( 'NONE', #42079, #25343 ) ;
#47387 = VERTEX_POINT ( 'NONE', #63982 ) ;
#47388 = AXIS2_PLACEMENT_3D ( 'NONE', #392, #47425, #9967 ) ;
#47389 = DIRECTION ( 'NONE',  ( -1.000000000000000000, 0.000000000000000000, 0.000000000000000000 ) ) ;
#47391 = DIRECTION ( 'NONE',  ( 0.000000000000000000, -1.000000000000000000, 0.000000000000000000 ) ) ;
#47390 = CARTESIAN_POINT ( 'NONE',  ( -11.77351654964674310, -7.606483450353318965, 195.0000000000000284 ) ) ;
#47392 = ORIENTED_EDGE ( 'NONE', *, *, #36771, .T. ) ;
#47394 = ORIENTED_EDGE ( 'NONE', *, *, #11574, .T. ) ;
#47393 = DIRECTION ( 'NONE',  ( -1.000000000000000000, 2.602085213965213008E-15, 0.000000000000000000 ) ) ;
#47395 = ORIENTED_EDGE ( 'NONE', *, *, #15123, .T. ) ;
#47396 = VECTOR ( 'NONE', #55532, 1000.000000000000000 ) ;
#47397 = DIRECTION ( 'NONE',  ( -5.981805089575196197E-17, -1.000000000000000000, 0.000000000000000000 ) ) ;
#47398 = AXIS2_PLACEMENT_3D ( 'NONE', #6816, #55277, #55614 ) ;
#47399 = DIRECTION ( 'NONE',  ( 1.000000000000000000, 0.000000000000000000, 0.000000000000000000 ) ) ;
#47400 = ORIENTED_EDGE ( 'NONE', *, *, #19402, .F. ) ;
#47401 = ORIENTED_EDGE ( 'NONE', *, *, #35671, .F. ) ;
#47402 = AXIS2_PLACEMENT_3D ( 'NONE', #40595, #62495, #35269 ) ;
#47403 = DIRECTION ( 'NONE',  ( 1.000000000000000000, 0.000000000000000000, 0.000000000000000000 ) ) ;
#47404 = DIRECTION ( 'NONE',  ( -2.312964634635740689E-15, 1.000000000000000000, 0.000000000000000000 ) ) ;
#47405 = ORIENTED_EDGE ( 'NONE', *, *, #31290, .F. ) ;
#47406 = EDGE_LOOP ( 'NONE', ( #3583, #34050, #5125, #46049 ) ) ;
#47407 = DIRECTION ( 'NONE',  ( 1.836970198721029934E-16, -1.836970198721036344E-16, 1.000000000000000000 ) ) ;
#47408 = DIRECTION ( 'NONE',  ( -1.000000000000000000, 0.000000000000000000, 0.000000000000000000 ) ) ;
#47409 = ORIENTED_EDGE ( 'NONE', *, *, #66618, .T. ) ;
#47410 = DIRECTION ( 'NONE',  ( -1.000000000000000000, 0.000000000000000000, 0.000000000000000000 ) ) ;
#47411 = CIRCLE ( 'NONE', #11269, 4.000000000000000888 ) ;
#47412 = CARTESIAN_POINT ( 'NONE',  ( -2.355476262117234931, 8.821682069070680754, 54.00000000000000711 ) ) ;
#47413 = ORIENTED_EDGE ( 'NONE', *, *, #47975, .F. ) ;
#47415 = VERTEX_POINT ( 'NONE', #56647 ) ;
#47414 = DIRECTION ( 'NONE',  ( 0.000000000000000000, 0.000000000000000000, -1.000000000000000000 ) ) ;
#47416 = LINE ( 'NONE', #32570, #7646 ) ;
#47417 = EDGE_CURVE ( 'NONE', #66328, #10926, #19026, .T. ) ;
#47418 = DIRECTION ( 'NONE',  ( -1.000000000000000000, 0.000000000000000000, 0.000000000000000000 ) ) ;
#47419 = DIRECTION ( 'NONE',  ( 0.000000000000000000, -1.000000000000000000, 0.000000000000000000 ) ) ;
#47420 = DIRECTION ( 'NONE',  ( 1.836970198721029934E-16, 1.836970198721010706E-16, -1.000000000000000000 ) ) ;
#47421 = LINE ( 'NONE', #5700, #10209 ) ;
#47422 = EDGE_CURVE ( 'NONE', #2415, #13815, #12244, .T. ) ;
#47423 = CARTESIAN_POINT ( 'NONE',  ( -11.00000000000000000, -9.200000000000120082, 17.30000000000000071 ) ) ;
#47424 = ORIENTED_EDGE ( 'NONE', *, *, #41007, .T. ) ;
#47425 = DIRECTION ( 'NONE',  ( 0.000000000000000000, 1.000000000000000000, 0.000000000000000000 ) ) ;
#47426 = CIRCLE ( 'NONE', #13553, 0.5999999999999998668 ) ;
#47427 = AXIS2_PLACEMENT_3D ( 'NONE', #68522, #26089, #20079 ) ;
#47429 = ORIENTED_EDGE ( 'NONE', *, *, #25209, .F. ) ;
#47428 = CARTESIAN_POINT ( 'NONE',  ( 3.848229544836323512, -7.357023737882811609, 54.00000000000000711 ) ) ;
#47430 = DIRECTION ( 'NONE',  ( -1.000000000000000000, 0.000000000000000000, 0.000000000000000000 ) ) ;
#47431 = VECTOR ( 'NONE', #16141, 1000.000000000000000 ) ;
#47432 = CARTESIAN_POINT ( 'NONE',  ( 55.00000000000000000, -21.00000000000000000, 16.96999999999999886 ) ) ;
#47433 = DIRECTION ( 'NONE',  ( 1.000000000000000000, 0.000000000000000000, 0.000000000000000000 ) ) ;
#47434 = EDGE_CURVE ( 'NONE', #42236, #30238, #37108, .T. ) ;
#47435 = CARTESIAN_POINT ( 'NONE',  ( 14.25000000000000000, -0.2038245569916330158, -21.77831216351300014 ) ) ;
#47436 = CIRCLE ( 'NONE', #18042, 0.1999999999999987899 ) ;
#47437 = ORIENTED_EDGE ( 'NONE', *, *, #24940, .F. ) ;
#47438 = DIRECTION ( 'NONE',  ( 1.000000000000000000, -0.000000000000000000, 0.000000000000000000 ) ) ;
#47439 = FACE_OUTER_BOUND ( 'NONE', #10963, .T. ) ;
#47440 = EDGE_CURVE ( 'NONE', #59557, #7845, #15547, .T. ) ;
#47441 = ORIENTED_EDGE ( 'NONE', *, *, #57738, .T. ) ;
#47442 = VECTOR ( 'NONE', #35600, 1000.000000000000000 ) ;
#47443 = DIRECTION ( 'NONE',  ( 0.000000000000000000, 0.000000000000000000, 1.000000000000000000 ) ) ;
#47444 = LINE ( 'NONE', #9981, #955 ) ;
#47445 = CIRCLE ( 'NONE', #42907, 1.000000000000000000 ) ;
#47446 = DIRECTION ( 'NONE',  ( -0.000000000000000000, 3.673940397442059868E-16, -1.000000000000000000 ) ) ;
#47447 = ORIENTED_EDGE ( 'NONE', *, *, #13703, .T. ) ;
#47448 = ADVANCED_FACE ( 'NONE', ( #3255 ), #64323, .T. ) ;
#47449 = DIRECTION ( 'NONE',  ( -0.5773502691896257311, -0.5773502691896257311, 0.5773502691896257311 ) ) ;
#47450 = ORIENTED_EDGE ( 'NONE', *, *, #44784, .T. ) ;
#47451 = ORIENTED_EDGE ( 'NONE', *, *, #37499, .T. ) ;
#47452 = CARTESIAN_POINT ( 'NONE',  ( -9.897976262117291313, -6.657023737882756365, 54.00000000000000711 ) ) ;
#47453 = VECTOR ( 'NONE', #55594, 1000.000000000000000 ) ;
#47454 = CARTESIAN_POINT ( 'NONE',  ( 275.0000000000000000, -32.44999999999905071, 13.20000000000091944 ) ) ;
#47455 = CIRCLE ( 'NONE', #16972, 0.1999999999999987899 ) ;
#47456 = DIRECTION ( 'NONE',  ( 0.000000000000000000, 0.9760787414516765015, 0.2174173187354474512 ) ) ;
#47457 = DIRECTION ( 'NONE',  ( 1.000000000000000000, 0.000000000000000000, 0.000000000000000000 ) ) ;
#47458 = CARTESIAN_POINT ( 'NONE',  ( 1.480523737882794233, -8.612468434717218457, 54.00000000000000711 ) ) ;
#47459 = VERTEX_POINT ( 'NONE', #24825 ) ;
#47460 = EDGE_CURVE ( 'NONE', #33281, #31845, #23560, .T. ) ;
#47461 = ORIENTED_EDGE ( 'NONE', *, *, #67756, .F. ) ;
#47463 = EDGE_LOOP ( 'NONE', ( #2420, #34794, #43803, #706 ) ) ;
#47462 = DIRECTION ( 'NONE',  ( 0.000000000000000000, -1.000000000000000000, 0.000000000000000000 ) ) ;
#47465 = ORIENTED_EDGE ( 'NONE', *, *, #24123, .T. ) ;
#47464 = EDGE_CURVE ( 'NONE', #45716, #7560, #8196, .T. ) ;
#47466 = DIRECTION ( 'NONE',  ( 0.000000000000000000, 0.000000000000000000, -1.000000000000000000 ) ) ;
#47467 = DIRECTION ( 'NONE',  ( -1.000000000000000000, 0.000000000000000000, 0.000000000000000000 ) ) ;
#47468 = VECTOR ( 'NONE', #29999, 1000.000000000000000 ) ;
#47469 = CARTESIAN_POINT ( 'NONE',  ( -10.30047626211725742, 6.642976262117184838, 54.00000000000000711 ) ) ;
#47470 = FACE_OUTER_BOUND ( 'NONE', #44148, .T. ) ;
#47472 = CARTESIAN_POINT ( 'NONE',  ( 75.42576880091934299, 10.00000000000000000, 330.9830310981789694 ) ) ;
#47471 = CARTESIAN_POINT ( 'NONE',  ( -8.250000000000001776, -7.249999999999998224, -15.50000000000000000 ) ) ;
#47473 = ORIENTED_EDGE ( 'NONE', *, *, #51436, .T. ) ;
#47474 = EDGE_CURVE ( 'NONE', #61998, #2382, #14210, .T. ) ;
#47475 = ORIENTED_EDGE ( 'NONE', *, *, #12685, .T. ) ;
#47476 = EDGE_LOOP ( 'NONE', ( #35416, #6098, #38541, #14645 ) ) ;
#47477 = CIRCLE ( 'NONE', #30513, 2.458500000000000796 ) ;
#47478 = LINE ( 'NONE', #10012, #62684 ) ;
#47479 = DIRECTION ( 'NONE',  ( -0.7071067811865527908, -0.7071067811865422437, 0.000000000000000000 ) ) ;
#47480 = VECTOR ( 'NONE', #65756, 1000.000000000000000 ) ;
#47481 = CARTESIAN_POINT ( 'NONE',  ( 85.07737089618316872, 8.033516549646932958, 318.7837994620735458 ) ) ;
#47482 = LINE ( 'NONE', #58803, #2664 ) ;
#47483 = AXIS2_PLACEMENT_3D ( 'NONE', #8659, #24227, #68059 ) ;
#47484 = VERTEX_POINT ( 'NONE', #47702 ) ;
#47485 = VERTEX_POINT ( 'NONE', #67962 ) ;
#47486 = VERTEX_POINT ( 'NONE', #19165 ) ;
#47487 = CIRCLE ( 'NONE', #6835, 24.99999999998784972 ) ;
#47488 = FACE_OUTER_BOUND ( 'NONE', #30435, .T. ) ;
#47489 = VERTEX_POINT ( 'NONE', #26147 ) ;
#47490 = VERTEX_POINT ( 'NONE', #20824 ) ;
#47491 = CARTESIAN_POINT ( 'NONE',  ( 7.000000000000000000, -30.80000000000000071, 8.900000000000000355 ) ) ;
#47492 = EDGE_LOOP ( 'NONE', ( #36279, #33233, #22083, #40423 ) ) ;
#47493 = CIRCLE ( 'NONE', #3483, 0.1999999999999987899 ) ;
#47494 = EDGE_CURVE ( 'NONE', #24019, #3194, #63096, .T. ) ;
#47495 = ORIENTED_EDGE ( 'NONE', *, *, #29111, .T. ) ;
#47496 = DIRECTION ( 'NONE',  ( 0.000000000000000000, 0.000000000000000000, 1.000000000000000000 ) ) ;
#47497 = CIRCLE ( 'NONE', #12437, 24.99999999998789946 ) ;
#47499 = ORIENTED_EDGE ( 'NONE', *, *, #44228, .T. ) ;
#47498 = DIRECTION ( 'NONE',  ( 0.000000000000000000, 0.000000000000000000, 1.000000000000000000 ) ) ;
#47500 = ORIENTED_EDGE ( 'NONE', *, *, #45016, .F. ) ;
#47501 = EDGE_CURVE ( 'NONE', #53417, #27421, #10224, .T. ) ;
#47502 = CARTESIAN_POINT ( 'NONE',  ( -10.19191654964671301, 11.47551654964660450, 455.0000000000000568 ) ) ;
#47503 = DIRECTION ( 'NONE',  ( 1.000000000000000000, -3.903627567395476653E-15, 0.000000000000000000 ) ) ;
#47504 = ADVANCED_FACE ( 'NONE', ( #10567 ), #5281, .F. ) ;
#47506 = ORIENTED_EDGE ( 'NONE', *, *, #633, .F. ) ;
#47505 = CARTESIAN_POINT ( 'NONE',  ( 7.000000000000000000, -21.00000000000000000, -7.800000000000000711 ) ) ;
#47507 = VERTEX_POINT ( 'NONE', #9888 ) ;
#47508 = VECTOR ( 'NONE', #28977, 1000.000000000000000 ) ;
#47509 = DIRECTION ( 'NONE',  ( 0.000000000000000000, 0.000000000000000000, 1.000000000000000000 ) ) ;
#47510 = VECTOR ( 'NONE', #2259, 1000.000000000000000 ) ;
#47511 = ADVANCED_FACE ( 'NONE', ( #26486 ), #21526, .F. ) ;
#47512 = LINE ( 'NONE', #52842, #15990 ) ;
#47513 = FACE_OUTER_BOUND ( 'NONE', #57578, .T. ) ;
#47514 = DIRECTION ( 'NONE',  ( 0.000000000000000000, 1.000000000000000000, 0.000000000000000000 ) ) ;
#47515 = EDGE_CURVE ( 'NONE', #47649, #43371, #21189, .T. ) ;
#47516 = VERTEX_POINT ( 'NONE', #53025 ) ;
#47517 = CARTESIAN_POINT ( 'NONE',  ( -8.593516549646711411, 4.383466043307770121, 455.0000000000000568 ) ) ;
#47518 = CARTESIAN_POINT ( 'NONE',  ( 49.00000000000000000, 13.66939075806899950, 20.80000000000000426 ) ) ;
#47519 = CARTESIAN_POINT ( 'NONE',  ( -8.227189898828745740, 1.620245201994245487, 26.00000000000000711 ) ) ;
#47520 = AXIS2_PLACEMENT_3D ( 'NONE', #60343, #1315, #65669 ) ;
#47521 = EDGE_CURVE ( 'NONE', #29373, #58489, #69967, .T. ) ;
#47522 = CARTESIAN_POINT ( 'NONE',  ( 7.000000000000000000, -26.06128899128900045, -10.14003097807800025 ) ) ;
#47523 = ADVANCED_FACE ( 'NONE', ( #40736 ), #62292, .F. ) ;
#47524 = CARTESIAN_POINT ( 'NONE',  ( 12.90000000000000213, 20.60000000000000142, -13.86939075806900057 ) ) ;
#47525 = PLANE ( 'NONE',  #3190 ) ;
#47526 = EDGE_CURVE ( 'NONE', #28620, #19158, #16579, .T. ) ;
#47527 = EDGE_CURVE ( 'NONE', #34438, #44371, #2118, .T. ) ;
#47528 = EDGE_CURVE ( 'NONE', #9916, #35535, #66027, .T. ) ;
#47529 = EDGE_LOOP ( 'NONE', ( #43090, #60147, #63838, #65108, #15489, #40954, #13280, #14311, #46351, #56495, #13367, #63362, #61913, #40843, #59758 ) ) ;
#47530 = SURFACE_SIDE_STYLE ('',( #59189 ) ) ;
#47531 = CIRCLE ( 'NONE', #17047, 1.399999999999998579 ) ;
#47532 = DIRECTION ( 'NONE',  ( 0.5000000000000111022, 0.8660254037844322683, 2.509347957447867451E-16 ) ) ;
#47533 = EDGE_CURVE ( 'NONE', #16044, #69842, #38234, .T. ) ;
#47534 = AXIS2_PLACEMENT_3D ( 'NONE', #58392, #59072, #53091 ) ;
#47535 = CARTESIAN_POINT ( 'NONE',  ( 38.90000000000000568, 20.60000000000000142, -13.86939075806900057 ) ) ;
#47536 = ORIENTED_EDGE ( 'NONE', *, *, #32860, .F. ) ;
#47537 = CARTESIAN_POINT ( 'NONE',  ( 17.00000000000000000, -15.50000000000000000, 14.50000000000000000 ) ) ;
#47538 = DIRECTION ( 'NONE',  ( 0.000000000000000000, 0.000000000000000000, -1.000000000000000000 ) ) ;
#47539 = DIRECTION ( 'NONE',  ( 1.000000000000000000, 0.000000000000000000, -0.000000000000000000 ) ) ;
#47540 = AXIS2_PLACEMENT_3D ( 'NONE', #44911, #28638, #66474 ) ;
#47541 = DIRECTION ( 'NONE',  ( -1.000000000000000000, 0.000000000000000000, 0.000000000000000000 ) ) ;
#47542 = LINE ( 'NONE', #4764, #55685 ) ;
#47543 = ORIENTED_EDGE ( 'NONE', *, *, #10968, .F. ) ;
#47544 = DIRECTION ( 'NONE',  ( 1.000000000000000000, 0.000000000000000000, 0.000000000000000000 ) ) ;
#47545 = LINE ( 'NONE', #63107, #31749 ) ;
#47546 = LINE ( 'NONE', #64177, #37960 ) ;
#47547 = CIRCLE ( 'NONE', #31759, 0.1999999999999996503 ) ;
#47548 = CIRCLE ( 'NONE', #67882, 0.3499999999999996447 ) ;
#47549 = CARTESIAN_POINT ( 'NONE',  ( 283.0000000000000568, -23.50007830495750127, -12.28007262201345995 ) ) ;
#47550 = CARTESIAN_POINT ( 'NONE',  ( 10.00000000000000000, 21.00000000000000000, -18.00000000000000355 ) ) ;
#47551 = EDGE_CURVE ( 'NONE', #48678, #35336, #17246, .T. ) ;
#47552 = ORIENTED_EDGE ( 'NONE', *, *, #26139, .F. ) ;
#47554 = ORIENTED_EDGE ( 'NONE', *, *, #203, .F. ) ;
#47553 = DIRECTION ( 'NONE',  ( 1.000000000000000000, -0.000000000000000000, 0.000000000000000000 ) ) ;
#47555 = VECTOR ( 'NONE', #49966, 1000.000000000000000 ) ;
#47556 = ADVANCED_FACE ( 'NONE', ( #22231 ), #33171, .T. ) ;
#47557 = DIRECTION ( 'NONE',  ( 0.000000000000000000, -3.673940397442059868E-16, 1.000000000000000000 ) ) ;
#47558 = CARTESIAN_POINT ( 'NONE',  ( -6.835476262117260227, 10.30047626211718104, 54.00000000000000711 ) ) ;
#47559 = CARTESIAN_POINT ( 'NONE',  ( 46.39999999999999858, 33.00000000000000000, 0.7500000000000000000 ) ) ;
#47560 = ORIENTED_EDGE ( 'NONE', *, *, #40134, .T. ) ;
#47561 = CARTESIAN_POINT ( 'NONE',  ( 176.0064834503533575, -29.01119750012555087, 5.000000000000000000 ) ) ;
#47562 = LINE ( 'NONE', #25293, #29598 ) ;
#47563 = ORIENTED_EDGE ( 'NONE', *, *, #23293, .F. ) ;
#47564 = VERTEX_POINT ( 'NONE', #65016 ) ;
#47565 = ORIENTED_EDGE ( 'NONE', *, *, #28406, .T. ) ;
#47566 = DIRECTION ( 'NONE',  ( 1.000000000000000000, 0.000000000000000000, 0.000000000000000000 ) ) ;
#47567 = CARTESIAN_POINT ( 'NONE',  ( -8.250000000000001776, 7.250000000000000888, -20.50000000000000000 ) ) ;
#47568 = CARTESIAN_POINT ( 'NONE',  ( 283.0000000000000568, -40.30000000000000426, -12.20000000000000107 ) ) ;
#47569 = EDGE_CURVE ( 'NONE', #64136, #45523, #16773, .T. ) ;
#47570 = ORIENTED_EDGE ( 'NONE', *, *, #63074, .F. ) ;
#47571 = ORIENTED_EDGE ( 'NONE', *, *, #16194, .F. ) ;
#47572 = CARTESIAN_POINT ( 'NONE',  ( 275.0000000000001137, -41.99999999999996447, -26.49999999999994316 ) ) ;
#47573 = ORIENTED_EDGE ( 'NONE', *, *, #30122, .F. ) ;
#47574 = ORIENTED_EDGE ( 'NONE', *, *, #18884, .F. ) ;
#47575 = VERTEX_POINT ( 'NONE', #48750 ) ;
#47576 = ORIENTED_EDGE ( 'NONE', *, *, #9643, .T. ) ;
#47577 = PLANE ( 'NONE',  #68872 ) ;
#47578 = VECTOR ( 'NONE', #16739, 1000.000000000000000 ) ;
#47580 = ORIENTED_EDGE ( 'NONE', *, *, #55502, .F. ) ;
#47579 = DIRECTION ( 'NONE',  ( 1.000000000000000000, 2.135044278125301343E-15, 0.000000000000000000 ) ) ;
#47581 = EDGE_CURVE ( 'NONE', #27421, #23856, #65362, .T. ) ;
#47582 = DIRECTION ( 'NONE',  ( 0.000000000000000000, -0.1875000000000000000, -0.9822646028438569710 ) ) ;
#47583 = VECTOR ( 'NONE', #19488, 1000.000000000000114 ) ;
#47584 = DIRECTION ( 'NONE',  ( 0.000000000000000000, 1.000000000000000000, 0.000000000000000000 ) ) ;
#47585 = CARTESIAN_POINT ( 'NONE',  ( 30.00000000000000000, -11.50000000000000000, -15.00000000000000000 ) ) ;
#47586 = VERTEX_POINT ( 'NONE', #16916 ) ;
#47587 = EDGE_CURVE ( 'NONE', #13563, #55579, #54125, .T. ) ;
#47588 = EDGE_LOOP ( 'NONE', ( #30436, #35959, #27567, #19118 ) ) ;
#47589 = EDGE_CURVE ( 'NONE', #49352, #21570, #6977, .T. ) ;
#47590 = CIRCLE ( 'NONE', #19359, 0.8099999999999999423 ) ;
#47591 = AXIS2_PLACEMENT_3D ( 'NONE', #65643, #65311, #23542 ) ;
#47592 = FACE_OUTER_BOUND ( 'NONE', #11873, .T. ) ;
#47593 = EDGE_CURVE ( 'NONE', #25334, #43217, #22903, .T. ) ;
#47594 = PLANE ( 'NONE',  #64311 ) ;
#47595 = VERTEX_POINT ( 'NONE', #59702 ) ;
#47596 = VECTOR ( 'NONE', #15991, 1000.000000000000000 ) ;
#47597 = DIRECTION ( 'NONE',  ( 1.000000000000000000, 0.000000000000000000, 0.000000000000000000 ) ) ;
#47598 = CARTESIAN_POINT ( 'NONE',  ( -25.49999999999869971, -15.50000000000000000, 22.50000000000000000 ) ) ;
#47599 = DIRECTION ( 'NONE',  ( -1.000000000000000000, 0.000000000000000000, 0.000000000000000000 ) ) ;
#47600 = ORIENTED_EDGE ( 'NONE', *, *, #32900, .F. ) ;
#47601 = DIRECTION ( 'NONE',  ( -0.000000000000000000, 3.673940397442059868E-16, -1.000000000000000000 ) ) ;
#47602 = PLANE ( 'NONE',  #33554 ) ;
#47603 = AXIS2_PLACEMENT_3D ( 'NONE', #5093, #27007, #16050 ) ;
#47604 = DIRECTION ( 'NONE',  ( 0.8660254037844510311, 0.4999999999999785727, 0.000000000000000000 ) ) ;
#47605 = DIRECTION ( 'NONE',  ( 7.751221965937476285E-17, 1.000000000000000000, -0.000000000000000000 ) ) ;
#47606 = EDGE_CURVE ( 'NONE', #67667, #34368, #28544, .T. ) ;
#47607 = CARTESIAN_POINT ( 'NONE',  ( 4.747751991980625696, -6.619341603356844850, 195.0000000000000284 ) ) ;
#47608 = ORIENTED_EDGE ( 'NONE', *, *, #69417, .F. ) ;
#47609 = DIRECTION ( 'NONE',  ( 0.000000000000000000, 0.000000000000000000, 1.000000000000000000 ) ) ;
#47610 = DIRECTION ( 'NONE',  ( 0.7071067811865475727, 0.000000000000000000, 0.7071067811865475727 ) ) ;
#47611 = CARTESIAN_POINT ( 'NONE',  ( 23.90000000000000213, 20.60000000000000142, 13.86939075806899702 ) ) ;
#47612 = CARTESIAN_POINT ( 'NONE',  ( 283.0000000000000568, -38.15000000000000568, 14.50000000000000000 ) ) ;
#47613 = VECTOR ( 'NONE', #61292, 1000.000000000000000 ) ;
#47614 = ORIENTED_EDGE ( 'NONE', *, *, #10480, .F. ) ;
#47615 = CARTESIAN_POINT ( 'NONE',  ( -9.897976262117293089, -6.832023737882757075, 54.00000000000000711 ) ) ;
#47616 = CARTESIAN_POINT ( 'NONE',  ( 2.369523737882811787, 9.547976262117209956, 26.00000000000000711 ) ) ;
#47617 = CARTESIAN_POINT ( 'NONE',  ( 0.000000000000000000, -7.449999999999998401, -12.00000000000000000 ) ) ;
#47618 = DIRECTION ( 'NONE',  ( -1.000000000000000000, 0.000000000000000000, 0.000000000000000000 ) ) ;
#47619 = VERTEX_POINT ( 'NONE', #16218 ) ;
#47620 = DIRECTION ( 'NONE',  ( -1.000000000000000000, 3.491481338843133355E-15, 1.836970198721036344E-16 ) ) ;
#47621 = DIRECTION ( 'NONE',  ( -0.6414496315691537998, 0.7671651518153029814, 0.000000000000000000 ) ) ;
#47622 = DIRECTION ( 'NONE',  ( 0.7671651518153105309, 0.6414496315691445849, 0.000000000000000000 ) ) ;
#47623 = LINE ( 'NONE', #30664, #32144 ) ;
#47624 = DIRECTION ( 'NONE',  ( -0.000000000000000000, 3.673940397442059868E-16, -1.000000000000000000 ) ) ;
#47625 = DIRECTION ( 'NONE',  ( 0.7671651518153105309, -0.6414496315691445849, -0.000000000000000000 ) ) ;
#47626 = VECTOR ( 'NONE', #46714, 1000.000000000000000 ) ;
#47627 = EDGE_CURVE ( 'NONE', #29534, #31249, #44455, .T. ) ;
#47628 = ORIENTED_EDGE ( 'NONE', *, *, #55077, .F. ) ;
#47629 = EDGE_CURVE ( 'NONE', #42154, #39526, #57486, .T. ) ;
#47630 = VECTOR ( 'NONE', #25514, 1000.000000000000000 ) ;
#47631 = ORIENTED_EDGE ( 'NONE', *, *, #31168, .T. ) ;
#47632 = DIRECTION ( 'NONE',  ( 0.000000000000000000, 0.000000000000000000, 1.000000000000000000 ) ) ;
#47633 = DIRECTION ( 'NONE',  ( -1.000000000000000000, 0.000000000000000000, 0.000000000000000000 ) ) ;
#47634 = ORIENTED_EDGE ( 'NONE', *, *, #7850, .F. ) ;
#47635 = EDGE_CURVE ( 'NONE', #22923, #29997, #64655, .T. ) ;
#47636 = DIRECTION ( 'NONE',  ( -1.000000000000000000, 0.000000000000000000, 0.000000000000000000 ) ) ;
#47637 = CARTESIAN_POINT ( 'NONE',  ( 41.09999999999999432, -0.2000000000089119934, 8.909539772616881237E-12 ) ) ;
#47638 = ORIENTED_EDGE ( 'NONE', *, *, #28010, .T. ) ;
#47639 = CIRCLE ( 'NONE', #48809, 0.1749999999999993783 ) ;
#47640 = CLOSED_SHELL ( 'NONE', ( #17859, #57149, #33231, #4282, #34885, #33761, #20855, #36560, #18101, #17726, #48222, #63603, #52285, #33565, #54005, #49348, #13591, #11472, #4168, #31026, #50055 ) ) ;
#47641 = CARTESIAN_POINT ( 'NONE',  ( 15.00000000000000000, -21.00000000000000000, -8.000000000000000000 ) ) ;
#47642 = ORIENTED_EDGE ( 'NONE', *, *, #12386, .T. ) ;
#47643 = ORIENTED_EDGE ( 'NONE', *, *, #13240, .F. ) ;
#47644 = DIRECTION ( 'NONE',  ( -1.000000000000000000, 0.000000000000000000, 0.000000000000000000 ) ) ;
#47645 = EDGE_LOOP ( 'NONE', ( #32153, #46776, #3309, #62578, #44598, #49719, #42417, #44546 ) ) ;
#47646 = FACE_OUTER_BOUND ( 'NONE', #39126, .T. ) ;
#47647 = CARTESIAN_POINT ( 'NONE',  ( 39.90000000000000568, -21.00000000000000000, -16.96999999999999886 ) ) ;
#47648 = CARTESIAN_POINT ( 'NONE',  ( -4.734785091273957747, 6.606374702650051667, 455.0000000000000568 ) ) ;
#47649 = VERTEX_POINT ( 'NONE', #10919 ) ;
#47650 = CARTESIAN_POINT ( 'NONE',  ( 283.0000000000000568, -25.00000000000000000, 17.50000000000000000 ) ) ;
#47651 = AXIS2_PLACEMENT_3D ( 'NONE', #66809, #56218, #50206 ) ;
#47653 = CARTESIAN_POINT ( 'NONE',  ( 11.08848345035334404, -9.804883450353528929, 455.0000000000000568 ) ) ;
#47652 = CARTESIAN_POINT ( 'NONE',  ( 27.90000000000000213, -21.00000000000000000, 13.86939075806900057 ) ) ;
#47654 = ORIENTED_EDGE ( 'NONE', *, *, #11575, .T. ) ;
#47655 = ORIENTED_EDGE ( 'NONE', *, *, #12831, .T. ) ;
#47656 = EDGE_LOOP ( 'NONE', ( #19103, #53646, #35975, #59729 ) ) ;
#47658 = ORIENTED_EDGE ( 'NONE', *, *, #3051, .F. ) ;
#47657 = CONTEXT_DEPENDENT_SHAPE_REPRESENTATION ( #18737, #60034 ) ;
#47659 =( REPRESENTATION_RELATIONSHIP ('NONE','NONE', #33057, #33595 ) REPRESENTATION_RELATIONSHIP_WITH_TRANSFORMATION ( #26446 )SHAPE_REPRESENTATION_RELATIONSHIP( ) );
#47660 = DIRECTION ( 'NONE',  ( 0.000000000000000000, 0.000000000000000000, -1.000000000000000000 ) ) ;
#47662 = ORIENTED_EDGE ( 'NONE', *, *, #33805, .T. ) ;
#47661 = DIRECTION ( 'NONE',  ( 0.000000000000000000, 0.000000000000000000, -1.000000000000000000 ) ) ;
#47663 = ADVANCED_FACE ( 'NONE', ( #54407 ), #54062, .T. ) ;
#47664 = DIRECTION ( 'NONE',  ( 0.000000000000000000, 0.000000000000000000, -1.000000000000000000 ) ) ;
#47665 = DIRECTION ( 'NONE',  ( -0.000000000000000000, -1.000000000000000000, 0.000000000000000000 ) ) ;
#47666 = VERTEX_POINT ( 'NONE', #21870 ) ;
#47667 = ORIENTED_EDGE ( 'NONE', *, *, #30029, .T. ) ;
#47668 = CARTESIAN_POINT ( 'NONE',  ( 11.12648345035337982, -7.806483450353490561, 455.0000000000000568 ) ) ;
#47669 = ADVANCED_FACE ( 'NONE', ( #43427, #27524 ), #2035, .T. ) ;
#47670 = VECTOR ( 'NONE', #663, 1000.000000000000000 ) ;
#47671 = EDGE_CURVE ( 'NONE', #28065, #18663, #51161, .T. ) ;
#47672 = ORIENTED_EDGE ( 'NONE', *, *, #46084, .T. ) ;
#47673 = CARTESIAN_POINT ( 'NONE',  ( 6.657023737882815873, 10.30047626211719880, 26.00000000000000711 ) ) ;
#47674 = DIRECTION ( 'NONE',  ( 0.000000000000000000, 0.000000000000000000, 1.000000000000000000 ) ) ;
#47675 = EDGE_CURVE ( 'NONE', #57047, #48724, #29248, .T. ) ;
#47676 = LINE ( 'NONE', #63950, #12477 ) ;
#47677 = EDGE_CURVE ( 'NONE', #10200, #50705, #56811, .T. ) ;
#47678 = VECTOR ( 'NONE', #8441, 1000.000000000000000 ) ;
#47679 = ORIENTED_EDGE ( 'NONE', *, *, #56385, .T. ) ;
#47680 = ADVANCED_FACE ( 'NONE', ( #45860 ), #4414, .T. ) ;
#47681 = DIRECTION ( 'NONE',  ( -0.000000000000000000, -0.000000000000000000, -1.000000000000000000 ) ) ;
#47682 = CARTESIAN_POINT ( 'NONE',  ( 7.000000000000000000, -32.00000000000000000, -8.400000000000000355 ) ) ;
#47684 = VERTEX_POINT ( 'NONE', #29234 ) ;
#47683 = SURFACE_SIDE_STYLE ('',( #10204 ) ) ;
#47686 = ORIENTED_EDGE ( 'NONE', *, *, #64880, .F. ) ;
#47685 = CARTESIAN_POINT ( 'NONE',  ( 39.90000000000000568, 0.000000000000000000, 3.447897592003593022E-15 ) ) ;
#47687 = VECTOR ( 'NONE', #33645, 1000.000000000000000 ) ;
#47688 = FACE_OUTER_BOUND ( 'NONE', #17211, .T. ) ;
#47689 = CARTESIAN_POINT ( 'NONE',  ( 11.78648345035337819, -7.606483450353398013, 195.0000000000000284 ) ) ;
#47690 = DIRECTION ( 'NONE',  ( -1.000000000000000000, 0.000000000000000000, 0.000000000000000000 ) ) ;
#47691 = CIRCLE ( 'NONE', #64644, 0.9999999999999991118 ) ;
#47692 = CARTESIAN_POINT ( 'NONE',  ( 7.408280051175172076, -3.724485858128701032, 54.00000000000000711 ) ) ;
#47693 = DIRECTION ( 'NONE',  ( -1.000000000000000000, 3.491481338843133355E-15, 1.836970198721036344E-16 ) ) ;
#47694 = ORIENTED_EDGE ( 'NONE', *, *, #58690, .T. ) ;
#47695 = CYLINDRICAL_SURFACE ( 'NONE', #42587, 4.500000000000188294 ) ;
#47696 = DIRECTION ( 'NONE',  ( 0.000000000000000000, 0.000000000000000000, 1.000000000000000000 ) ) ;
#47697 = DIRECTION ( 'NONE',  ( -1.000000000000000000, 0.000000000000000000, 0.000000000000000000 ) ) ;
#47699 = ORIENTED_EDGE ( 'NONE', *, *, #57556, .F. ) ;
#47698 = DIRECTION ( 'NONE',  ( 0.6414496315691565753, 0.7671651518153006499, 2.818519042764004597E-16 ) ) ;
#47700 = DIRECTION ( 'NONE',  ( 1.000000000000000000, 0.000000000000000000, 0.000000000000000000 ) ) ;
#47701 = AXIS2_PLACEMENT_3D ( 'NONE', #14412, #51540, #24667 ) ;
#47702 = CARTESIAN_POINT ( 'NONE',  ( 0.000000000000000000, 17.79289321881345032, -20.50000000000000000 ) ) ;
#47703 = LINE ( 'NONE', #68925, #43157 ) ;
#47704 = CIRCLE ( 'NONE', #65764, 0.1999999999999987899 ) ;
#47705 = CARTESIAN_POINT ( 'NONE',  ( -11.00000000000000000, -11.50000000000100009, -19.50000000000103739 ) ) ;
#47706 = ORIENTED_EDGE ( 'NONE', *, *, #27157, .F. ) ;
#47707 = LINE ( 'NONE', #69276, #58041 ) ;
#47708 = DIRECTION ( 'NONE',  ( -0.000000000000000000, -1.000000000000000000, -0.000000000000000000 ) ) ;
#47709 = EDGE_LOOP ( 'NONE', ( #35117, #13305, #47536, #61089 ) ) ;
#47710 = DIRECTION ( 'NONE',  ( 0.000000000000000000, 0.000000000000000000, -1.000000000000000000 ) ) ;
#47711 = CARTESIAN_POINT ( 'NONE',  ( 16.89999999999999858, -21.00000000000001421, -13.86939075806900945 ) ) ;
#47712 = DIRECTION ( 'NONE',  ( 0.000000000000000000, -0.1111111111108836896, -0.9938079899999319178 ) ) ;
#47713 = CARTESIAN_POINT ( 'NONE',  ( 283.0000000000000568, -25.60000000000000142, 17.35424868893542438 ) ) ;
#47714 = CARTESIAN_POINT ( 'NONE',  ( 73.77321854994620765, 47.95351654967443977, 25.00000000000000000 ) ) ;
#47715 = ORIENTED_EDGE ( 'NONE', *, *, #26365, .F. ) ;
#47716 = ORIENTED_EDGE ( 'NONE', *, *, #11189, .T. ) ;
#47717 = CARTESIAN_POINT ( 'NONE',  ( -11.00000000000000000, -17.50000000000000000, -15.70500000000000007 ) ) ;
#47718 = VERTEX_POINT ( 'NONE', #24652 ) ;
#47719 = VERTEX_POINT ( 'NONE', #39502 ) ;
#47720 = EDGE_CURVE ( 'NONE', #22255, #67830, #8368, .T. ) ;
#47721 = DIRECTION ( 'NONE',  ( 0.000000000000000000, 1.000000000000000000, 0.000000000000000000 ) ) ;
#47722 = ADVANCED_FACE ( 'NONE', ( #66724, #23248, #17936, #67444, #45501 ), #50808, .F. ) ;
#47723 = VECTOR ( 'NONE', #7605, 1000.000000000000000 ) ;
#47724 = EDGE_CURVE ( 'NONE', #16791, #13851, #56324, .T. ) ;
#47725 = CARTESIAN_POINT ( 'NONE',  ( -7.750000000000001776, 7.750000000000001776, -5.000000000000000000 ) ) ;
#47726 = DIRECTION ( 'NONE',  ( 0.000000000000000000, 1.000000000000000000, 0.000000000000000000 ) ) ;
#47727 = ORIENTED_EDGE ( 'NONE', *, *, #41543, .T. ) ;
#47728 = VERTEX_POINT ( 'NONE', #19334 ) ;
#47729 = DIRECTION ( 'NONE',  ( 1.000000000000000000, 0.000000000000000000, 0.000000000000000000 ) ) ;
#47730 = ORIENTED_EDGE ( 'NONE', *, *, #67999, .T. ) ;
#47731 = EDGE_LOOP ( 'NONE', ( #53246, #48937, #21400, #57715 ) ) ;
#47732 = LINE ( 'NONE', #20861, #69939 ) ;
#47733 = CARTESIAN_POINT ( 'NONE',  ( -30.00000000000000000, -11.10796162543699950, -9.102987789146602893 ) ) ;
#47734 = DIRECTION ( 'NONE',  ( -0.000000000000000000, 3.673940397442059868E-16, -1.000000000000000000 ) ) ;
#47735 = EDGE_LOOP ( 'NONE', ( #19980, #58273, #38799, #30113 ) ) ;
#47736 = VECTOR ( 'NONE', #21572, 1000.000000000000000 ) ;
#47737 = LINE ( 'NONE', #31493, #34501 ) ;
#47739 = CARTESIAN_POINT ( 'NONE',  ( -5.993516549646776603, -6.006483450353426790, 455.0000000000000568 ) ) ;
#47738 = DIRECTION ( 'NONE',  ( 0.000000000000000000, 0.000000000000000000, -1.000000000000000000 ) ) ;
#47740 = ORIENTED_EDGE ( 'NONE', *, *, #45016, .T. ) ;
#47742 = ORIENTED_EDGE ( 'NONE', *, *, #6484, .F. ) ;
#47741 = CARTESIAN_POINT ( 'NONE',  ( 8.250000000000005329, 7.250000000000000888, -14.50000000000000000 ) ) ;
#47743 = EDGE_LOOP ( 'NONE', ( #60873, #19095, #43227, #64887 ) ) ;
#47744 = CARTESIAN_POINT ( 'NONE',  ( -9.093516549646711411, 11.11351654964659730, 455.0000000000000568 ) ) ;
#47745 = CARTESIAN_POINT ( 'NONE',  ( 7.357023737882806280, 6.651770455163672935, 54.00000000000000711 ) ) ;
#47746 = AXIS2_PLACEMENT_3D ( 'NONE', #24935, #57456, #51458 ) ;
#47747 = EDGE_LOOP ( 'NONE', ( #31820, #6668, #64984, #69964, #55075, #54350, #3372, #6749 ) ) ;
#47748 = AXIS2_PLACEMENT_3D ( 'NONE', #60297, #17517, #5880 ) ;
#47750 = CARTESIAN_POINT ( 'NONE',  ( -5.538810540050064901, -7.357023737882800951, 54.00000000000000711 ) ) ;
#47749 = VECTOR ( 'NONE', #30665, 1000.000000000000000 ) ;
#47751 = CARTESIAN_POINT ( 'NONE',  ( -8.249999999999996447, -7.848062532927998269, 0.000000000000000000 ) ) ;
#47752 = VERTEX_POINT ( 'NONE', #2379 ) ;
#47753 = EDGE_LOOP ( 'NONE', ( #3834, #31287, #50123, #42770 ) ) ;
#47754 = LINE ( 'NONE', #15603, #18361 ) ;
#47755 = VECTOR ( 'NONE', #11577, 1000.000000000000000 ) ;
#47756 = CARTESIAN_POINT ( 'NONE',  ( 0.000000000000000000, 0.000000000000000000, -29.90000000000000924 ) ) ;
#47757 = EDGE_CURVE ( 'NONE', #66251, #58795, #7674, .T. ) ;
#47758 = ORIENTED_EDGE ( 'NONE', *, *, #36659, .T. ) ;
#47759 = EDGE_CURVE ( 'NONE', #68548, #37548, #34540, .T. ) ;
#47760 = VECTOR ( 'NONE', #29387, 1000.000000000000000 ) ;
#47761 = EDGE_CURVE ( 'NONE', #64729, #30577, #51874, .T. ) ;
#47762 = CARTESIAN_POINT ( 'NONE',  ( -11.99351654964671354, 4.173516549646604901, 195.0000000000000284 ) ) ;
#47763 = CARTESIAN_POINT ( 'NONE',  ( 17.00000000000000000, -16.28999999999710369, 15.00000000000794920 ) ) ;
#47764 = EDGE_CURVE ( 'NONE', #57794, #62883, #29589, .T. ) ;
#47765 = ORIENTED_EDGE ( 'NONE', *, *, #38895, .F. ) ;
#47767 = VERTEX_POINT ( 'NONE', #40549 ) ;
#47766 = PLANE ( 'NONE',  #67319 ) ;
#47768 = DIRECTION ( 'NONE',  ( 0.000000000000000000, 0.000000000000000000, -1.000000000000000000 ) ) ;
#47769 = LINE ( 'NONE', #27263, #44229 ) ;
#47770 = AXIS2_PLACEMENT_3D ( 'NONE', #867, #11778, #17096 ) ;
#47771 = CARTESIAN_POINT ( 'NONE',  ( 7.250000000000005329, -8.249999999999998224, -26.00000000000001066 ) ) ;
#47772 = DIRECTION ( 'NONE',  ( 0.000000000000000000, 0.000000000000000000, 1.000000000000000000 ) ) ;
#47773 = FACE_OUTER_BOUND ( 'NONE', #52501, .T. ) ;
#47774 = LINE ( 'NONE', #37186, #15720 ) ;
#47775 = CIRCLE ( 'NONE', #44368, 0.1999999999999996503 ) ;
#47776 = ORIENTED_EDGE ( 'NONE', *, *, #20413, .T. ) ;
#47777 = DIRECTION ( 'NONE',  ( 0.000000000000000000, 0.000000000000000000, -1.000000000000000000 ) ) ;
#47778 = EDGE_CURVE ( 'NONE', #51438, #68065, #44808, .T. ) ;
#47780 = VERTEX_POINT ( 'NONE', #34187 ) ;
#47779 = CARTESIAN_POINT ( 'NONE',  ( -7.955476262117311848, -8.835729544836290472, 26.00000000000000000 ) ) ;
#47781 = CARTESIAN_POINT ( 'NONE',  ( -24.00000000000000000, -17.50000000000000000, -15.70500000000000007 ) ) ;
#47782 = PLANE ( 'NONE',  #1891 ) ;
#47783 = CIRCLE ( 'NONE', #10536, 0.4999999999945534124 ) ;
#47784 = DIRECTION ( 'NONE',  ( 1.000000000000000000, 0.000000000000000000, 0.000000000000000000 ) ) ;
#47785 = ORIENTED_EDGE ( 'NONE', *, *, #27267, .F. ) ;
#47786 = CARTESIAN_POINT ( 'NONE',  ( 30.00000000000000000, -11.70000000000012008, -10.70000000000011831 ) ) ;
#47787 = CARTESIAN_POINT ( 'NONE',  ( -6.350872789121327244, 3.663616288756986084, 54.00000000000000711 ) ) ;
#47788 = ORIENTED_EDGE ( 'NONE', *, *, #16153, .F. ) ;
#47789 = DIRECTION ( 'NONE',  ( -0.000000000000000000, -0.000000000000000000, 1.000000000000000000 ) ) ;
#47790 = DIRECTION ( 'NONE',  ( -1.047444401652940007E-14, -1.000000000000000000, -1.836970198721029934E-16 ) ) ;
#47791 = DIRECTION ( 'NONE',  ( 0.000000000000000000, -1.000000000000000000, 0.000000000000000000 ) ) ;
#47792 = AXIS2_PLACEMENT_3D ( 'NONE', #63744, #10346, #16699 ) ;
#47793 = EDGE_LOOP ( 'NONE', ( #65227, #18788, #19037, #40931 ) ) ;
#47794 = FACE_OUTER_BOUND ( 'NONE', #5130, .T. ) ;
#47795 = VERTEX_POINT ( 'NONE', #57174 ) ;
#47796 = ORIENTED_EDGE ( 'NONE', *, *, #50576, .T. ) ;
#47797 = AXIS2_PLACEMENT_3D ( 'NONE', #23691, #18739, #65795 ) ;
#47798 = DIRECTION ( 'NONE',  ( 0.000000000000000000, 1.000000000000000000, -0.000000000000000000 ) ) ;
#47799 = LINE ( 'NONE', #24841, #57964 ) ;
#47800 = AXIS2_PLACEMENT_3D ( 'NONE', #44252, #7108, #806 ) ;
#47801 = ADVANCED_FACE ( 'NONE', ( #13333 ), #56467, .T. ) ;
#47802 = DIRECTION ( 'NONE',  ( 0.000000000000000000, 0.000000000000000000, 1.000000000000000000 ) ) ;
#47803 = MECHANICAL_DESIGN_GEOMETRIC_PRESENTATION_REPRESENTATION (  '', ( #54585 ), #66971 ) ;
#47804 = VECTOR ( 'NONE', #25344, 1000.000000000000000 ) ;
#47805 = CARTESIAN_POINT ( 'NONE',  ( 7.450000000000004619, -1.336933437520057563E-15, -25.50000000000000355 ) ) ;
#47806 = VERTEX_POINT ( 'NONE', #7318 ) ;
#47807 = ORIENTED_EDGE ( 'NONE', *, *, #63507, .F. ) ;
#47809 = VERTEX_POINT ( 'NONE', #28890 ) ;
#47808 = CARTESIAN_POINT ( 'NONE',  ( 0.7669999999999959073, 0.000000000000000000, 0.000000000000000000 ) ) ;
#47810 = ORIENTED_EDGE ( 'NONE', *, *, #27642, .F. ) ;
#47811 = CARTESIAN_POINT ( 'NONE',  ( 26.90000000000000213, 20.60000000000000142, 13.86939075806900057 ) ) ;
#47812 = CARTESIAN_POINT ( 'NONE',  ( -7.250000000000000888, 8.250000000000001776, -19.00000000000000000 ) ) ;
#47813 = CARTESIAN_POINT ( 'NONE',  ( -11.18999999999999950, 12.00000000000000178, -4.250000000000000000 ) ) ;
#47814 = CARTESIAN_POINT ( 'NONE',  ( 49.00000000000000000, -21.00000000000000000, 13.86939075806900057 ) ) ;
#47815 = EDGE_CURVE ( 'NONE', #2345, #14406, #19074, .T. ) ;
#47817 = CARTESIAN_POINT ( 'NONE',  ( -1.677516549646816291, -9.841277389592811176, 455.0000000000000568 ) ) ;
#47816 = DIRECTION ( 'NONE',  ( 0.000000000000000000, 0.000000000000000000, -1.000000000000000000 ) ) ;
#47818 = VERTEX_POINT ( 'NONE', #35955 ) ;
#47819 = VECTOR ( 'NONE', #2737, 1000.000000000000000 ) ;
#47820 = VERTEX_POINT ( 'NONE', #32053 ) ;
#47821 = VERTEX_POINT ( 'NONE', #52581 ) ;
#47822 = EDGE_LOOP ( 'NONE', ( #2120, #36441, #23181, #21458 ) ) ;
#47823 = EDGE_CURVE ( 'NONE', #29536, #51293, #21096, .T. ) ;
#47824 = LINE ( 'NONE', #37234, #43508 ) ;
#47825 = CARTESIAN_POINT ( 'NONE',  ( 11.12648345035337982, -7.806483450353490561, 455.0000000000000568 ) ) ;
#47826 = DIRECTION ( 'NONE',  ( -0.4999999999999832356, 0.000000000000000000, 0.8660254037844483666 ) ) ;
#47827 = ORIENTED_EDGE ( 'NONE', *, *, #45311, .F. ) ;
#47828 = ORIENTED_EDGE ( 'NONE', *, *, #56547, .T. ) ;
#47829 = ORIENTED_EDGE ( 'NONE', *, *, #31079, .F. ) ;
#47830 = VECTOR ( 'NONE', #68761, 1000.000000000000000 ) ;
#47831 = CARTESIAN_POINT ( 'NONE',  ( 11.00000000000000000, -16.64230188589299786, 14.64519951917100116 ) ) ;
#47832 = VERTEX_POINT ( 'NONE', #41961 ) ;
#47833 = DIRECTION ( 'NONE',  ( 1.000000000000000000, -5.981805089575196197E-17, 0.000000000000000000 ) ) ;
#47834 = ORIENTED_EDGE ( 'NONE', *, *, #44484, .T. ) ;
#47835 = ORIENTED_EDGE ( 'NONE', *, *, #45448, .T. ) ;
#47836 = CARTESIAN_POINT ( 'NONE',  ( 7.000000000000000000, -42.00000000000000000, -15.00000000000000000 ) ) ;
#47838 = ORIENTED_EDGE ( 'NONE', *, *, #47944, .F. ) ;
#47837 = DIRECTION ( 'NONE',  ( 0.000000000000000000, 1.000000000000000000, -0.000000000000000000 ) ) ;
#47839 = ORIENTED_EDGE ( 'NONE', *, *, #12949, .T. ) ;
#47840 = EDGE_CURVE ( 'NONE', #7061, #38093, #15451, .T. ) ;
#47841 = AXIS2_PLACEMENT_3D ( 'NONE', #44910, #2816, #50211 ) ;
#47843 = FACE_OUTER_BOUND ( 'NONE', #58245, .T. ) ;
#47842 = AXIS2_PLACEMENT_3D ( 'NONE', #65976, #21818, #43377 ) ;
#47844 = EDGE_CURVE ( 'NONE', #68196, #15146, #13420, .T. ) ;
#47845 = DIRECTION ( 'NONE',  ( 0.000000000000000000, 0.000000000000000000, -1.000000000000000000 ) ) ;
#47846 = EDGE_CURVE ( 'NONE', #3117, #1599, #15787, .T. ) ;
#47848 = ORIENTED_EDGE ( 'NONE', *, *, #20104, .T. ) ;
#47847 = DIRECTION ( 'NONE',  ( 1.000000000000000000, -5.981805089575194965E-17, 0.000000000000000000 ) ) ;
#47849 = VERTEX_POINT ( 'NONE', #53289 ) ;
#47850 = DIRECTION ( 'NONE',  ( -0.000000000000000000, 3.673940397442059868E-16, -1.000000000000000000 ) ) ;
#47851 = DIRECTION ( 'NONE',  ( 0.7671651518153065341, 0.6414496315691495809, -0.000000000000000000 ) ) ;
#47852 = COLOUR_RGB ( '', 0.66274510, 0.83137255, 0.94901961) ;
#47853 = AXIS2_PLACEMENT_3D ( 'NONE', #2791, #45936, #52291 ) ;
#47854 = EDGE_CURVE ( 'NONE', #47684, #58217, #29204, .T. ) ;
#47855 = DIRECTION ( 'NONE',  ( 1.000000000000000000, 0.000000000000000000, 0.000000000000000000 ) ) ;
#47856 = CARTESIAN_POINT ( 'NONE',  ( 37.90000000000000568, -0.1999999999911430404, -8.864436962241481021E-12 ) ) ;
#47857 = CARTESIAN_POINT ( 'NONE',  ( -8.393516549646712122, 5.655420232009161552, 195.0000000000000284 ) ) ;
#47858 = AXIS2_PLACEMENT_3D ( 'NONE', #53009, #9874, #41677 ) ;
#47859 = AXIS2_PLACEMENT_3D ( 'NONE', #35094, #56675, #35443 ) ;
#47860 = AXIS2_PLACEMENT_3D ( 'NONE', #46004, #1822, #17386 ) ;
#47861 = ADVANCED_FACE ( 'NONE', ( #37028 ), #10482, .T. ) ;
#47862 = ORIENTED_EDGE ( 'NONE', *, *, #25767, .T. ) ;
#47863 = FACE_BOUND ( 'NONE', #50283, .T. ) ;
#47864 = EDGE_CURVE ( 'NONE', #30586, #56148, #3432, .T. ) ;
#47865 = ORIENTED_EDGE ( 'NONE', *, *, #1793, .T. ) ;
#47866 = CARTESIAN_POINT ( 'NONE',  ( 9.703773737882814387, 8.916576262117184015, 54.00000000000000711 ) ) ;
#47867 = DIRECTION ( 'NONE',  ( 0.000000000000000000, -0.9938079899998859545, 0.1111111111112941946 ) ) ;
#47868 = CARTESIAN_POINT ( 'NONE',  ( -6.835476262117327728, -10.31452373788278187, 26.00000000000000000 ) ) ;
#47869 = FACE_OUTER_BOUND ( 'NONE', #24789, .T. ) ;
#47870 = ORIENTED_EDGE ( 'NONE', *, *, #65703, .F. ) ;
#47871 = CARTESIAN_POINT ( 'NONE',  ( 30.00000000000000000, -14.04000000000000092, 17.04524521594300523 ) ) ;
#47872 = DIRECTION ( 'NONE',  ( -1.000000000000000000, 0.000000000000000000, 0.000000000000000000 ) ) ;
#47873 = CARTESIAN_POINT ( 'NONE',  ( 4.201500623655991085, 7.259684009079854228, 195.0000000000000284 ) ) ;
#47874 = ORIENTED_EDGE ( 'NONE', *, *, #6556, .T. ) ;
#47875 = DIRECTION ( 'NONE',  ( 0.000000000000000000, 1.000000000000000000, 0.000000000000000000 ) ) ;
#47876 = EDGE_CURVE ( 'NONE', #52264, #19534, #60857, .T. ) ;
#47877 = LINE ( 'NONE', #58144, #6099 ) ;
#47878 = CARTESIAN_POINT ( 'NONE',  ( -15.50000000000000000, -0.4000000000000000222, -22.50000000000000000 ) ) ;
#47879 = AXIS2_PLACEMENT_3D ( 'NONE', #48586, #65538, #6495 ) ;
#47880 = DIRECTION ( 'NONE',  ( 9.912705577010386883E-15, 1.000000000000000000, 0.000000000000000000 ) ) ;
#47881 = DIRECTION ( 'NONE',  ( -1.000000000000000000, 0.000000000000000000, 0.000000000000000000 ) ) ;
#47882 = ORIENTED_EDGE ( 'NONE', *, *, #38044, .F. ) ;
#47883 = CARTESIAN_POINT ( 'NONE',  ( 283.0000000000000568, -37.61196062927500350, -8.008708659369300875 ) ) ;
#47884 = DIRECTION ( 'NONE',  ( -0.000000000000000000, -0.000000000000000000, -1.000000000000000000 ) ) ;
#47885 = AXIS2_PLACEMENT_3D ( 'NONE', #63995, #24746, #35688 ) ;
#47886 = DIRECTION ( 'NONE',  ( 0.000000000000000000, 0.000000000000000000, 1.000000000000000000 ) ) ;
#47887 = EDGE_CURVE ( 'NONE', #16165, #65332, #36303, .T. ) ;
#47888 = CARTESIAN_POINT ( 'NONE',  ( 9.689999999999999503, -9.750000000000001776, -5.000000000000000000 ) ) ;
#47889 = DIRECTION ( 'NONE',  ( 0.000000000000000000, 0.000000000000000000, -1.000000000000000000 ) ) ;
#47890 = ORIENTED_EDGE ( 'NONE', *, *, #18363, .T. ) ;
#47892 = ORIENTED_EDGE ( 'NONE', *, *, #34098, .F. ) ;
#47891 = CARTESIAN_POINT ( 'NONE',  ( 8.250000000000005329, 7.250000000000000888, -26.00000000000001066 ) ) ;
#47893 = EDGE_CURVE ( 'NONE', #65641, #49539, #68130, .T. ) ;
#47894 = VECTOR ( 'NONE', #47479, 1000.000000000000000 ) ;
#47895 = CARTESIAN_POINT ( 'NONE',  ( -7.450000000000001954, 7.250000000000000000, -11.50000000000000000 ) ) ;
#47896 = CARTESIAN_POINT ( 'NONE',  ( 3.664523737882815269, 10.49297626211721024, 26.00000000000000711 ) ) ;
#47897 = DIRECTION ( 'NONE',  ( 0.000000000000000000, 0.000000000000000000, -1.000000000000000000 ) ) ;
#47898 = VERTEX_POINT ( 'NONE', #19674 ) ;
#47899 = DIRECTION ( 'NONE',  ( 0.000000000000000000, 0.000000000000000000, 1.000000000000000000 ) ) ;
#47900 = VECTOR ( 'NONE', #16256, 1000.000000000000114 ) ;
#47901 = CIRCLE ( 'NONE', #26459, 1.000000000000000000 ) ;
#47902 = DIRECTION ( 'NONE',  ( 0.000000000000000000, -1.000000000000000000, 0.000000000000000000 ) ) ;
#47903 = AXIS2_PLACEMENT_3D ( 'NONE', #53890, #10048, #59177 ) ;
#47904 = ORIENTED_EDGE ( 'NONE', *, *, #1493, .T. ) ;
#47905 = ORIENTED_EDGE ( 'NONE', *, *, #20104, .F. ) ;
#47907 = VERTEX_POINT ( 'NONE', #30652 ) ;
#47906 = AXIS2_PLACEMENT_3D ( 'NONE', #12654, #55474, #23283 ) ;
#47908 = ADVANCED_FACE ( 'NONE', ( #41249 ), #68491, .T. ) ;
#47909 = CARTESIAN_POINT ( 'NONE',  ( 9.249999999999998224, 8.250000000000001776, -5.000000000000000000 ) ) ;
#47910 = CARTESIAN_POINT ( 'NONE',  ( 7.250000000000005329, -7.249999999999998224, -8.500000000000000000 ) ) ;
#47911 = FACE_OUTER_BOUND ( 'NONE', #48456, .T. ) ;
#47912 = AXIS2_PLACEMENT_3D ( 'NONE', #50460, #57154, #41236 ) ;
#47913 = VECTOR ( 'NONE', #60021, 1000.000000000000114 ) ;
#47914 = ORIENTED_EDGE ( 'NONE', *, *, #40714, .F. ) ;
#47915 = EDGE_CURVE ( 'NONE', #34995, #19545, #68839, .T. ) ;
#47916 = ORIENTED_EDGE ( 'NONE', *, *, #5135, .T. ) ;
#47918 = EDGE_CURVE ( 'NONE', #9024, #17119, #5565, .T. ) ;
#47917 = AXIS2_PLACEMENT_3D ( 'NONE', #2845, #18398, #1807 ) ;
#47919 = LINE ( 'NONE', #26708, #14699 ) ;
#47920 = VERTEX_POINT ( 'NONE', #31002 ) ;
#47921 = EDGE_CURVE ( 'NONE', #10775, #32155, #42304, .T. ) ;
#47922 = ORIENTED_EDGE ( 'NONE', *, *, #54856, .T. ) ;
#47923 = EDGE_CURVE ( 'NONE', #56561, #54968, #14588, .T. ) ;
#47924 = EDGE_CURVE ( 'NONE', #45591, #18488, #10138, .T. ) ;
#47925 = ORIENTED_EDGE ( 'NONE', *, *, #22563, .T. ) ;
#47926 = ORIENTED_EDGE ( 'NONE', *, *, #60917, .F. ) ;
#47927 = LINE ( 'NONE', #11136, #37283 ) ;
#47928 = UNCERTAINTY_MEASURE_WITH_UNIT (LENGTH_MEASURE( 1.000000000000000082E-05 ), #55997, 'distance_accuracy_value', 'NONE');
#47930 = VERTEX_POINT ( 'NONE', #58224 ) ;
#47929 = DIRECTION ( 'NONE',  ( -0.000000000000000000, 3.673940397442059868E-16, -1.000000000000000000 ) ) ;
#47931 = EDGE_CURVE ( 'NONE', #50433, #26084, #11203, .T. ) ;
#47932 = CARTESIAN_POINT ( 'NONE',  ( -30.00000000000000000, -5.599999999999379696, 26.60000000000059828 ) ) ;
#47933 = CARTESIAN_POINT ( 'NONE',  ( 181.4833316329832940, 0.000000000000000000, 276.7801873289890295 ) ) ;
#47934 = EDGE_CURVE ( 'NONE', #18569, #68953, #5531, .T. ) ;
#47935 = LINE ( 'NONE', #31348, #24523 ) ;
#47936 = EDGE_LOOP ( 'NONE', ( #66581, #28692, #25321, #38904, #692, #7359, #21034, #58667, #33975, #24298, #38101, #65387, #19560, #69056, #23849 ) ) ;
#47937 = VECTOR ( 'NONE', #19102, 1000.000000000000000 ) ;
#47938 = ORIENTED_EDGE ( 'NONE', *, *, #26047, .T. ) ;
#47939 = EDGE_CURVE ( 'NONE', #4220, #43137, #68757, .T. ) ;
#47940 = VECTOR ( 'NONE', #9331, 1000.000000000000000 ) ;
#47941 = EDGE_CURVE ( 'NONE', #11904, #46878, #16134, .T. ) ;
#47942 = CARTESIAN_POINT ( 'NONE',  ( 30.00000000000000000, -8.959999999999999076, 17.04524521594300523 ) ) ;
#47943 = ORIENTED_EDGE ( 'NONE', *, *, #52519, .T. ) ;
#47944 = EDGE_CURVE ( 'NONE', #23638, #24719, #60296, .T. ) ;
#47945 = AXIS2_PLACEMENT_3D ( 'NONE', #63181, #62461, #42311 ) ;
#47946 = VECTOR ( 'NONE', #34679, 1000.000000000000114 ) ;
#47947 = CARTESIAN_POINT ( 'NONE',  ( 48.50000000000000000, 0.7500000000000000000, -3.418698582794335028 ) ) ;
#47948 = CARTESIAN_POINT ( 'NONE',  ( 7.272650909786598561, -7.811466277050860718, 455.0000000000000568 ) ) ;
#47949 = EDGE_LOOP ( 'NONE', ( #22626, #4532, #46774, #53656, #49488, #4551, #51930, #30453 ) ) ;
#47950 = CARTESIAN_POINT ( 'NONE',  ( 7.000000000000000000, -23.65000000000000568, -12.40000000000000213 ) ) ;
#47951 = DIRECTION ( 'NONE',  ( -0.000000000000000000, -0.000000000000000000, -1.000000000000000000 ) ) ;
#47952 = AXIS2_PLACEMENT_3D ( 'NONE', #45975, #61518, #23367 ) ;
#47954 = AXIS2_PLACEMENT_3D ( 'NONE', #46426, #24867, #25222 ) ;
#47953 = LINE ( 'NONE', #64570, #55644 ) ;
#47955 = DIRECTION ( 'NONE',  ( -1.836970198721029934E-16, 1.836970198721036344E-16, -1.000000000000000000 ) ) ;
#47956 = EDGE_CURVE ( 'NONE', #52439, #69628, #65614, .T. ) ;
#47957 = AXIS2_PLACEMENT_3D ( 'NONE', #36338, #4180, #25748 ) ;
#47958 = DIRECTION ( 'NONE',  ( -1.000000000000000000, 1.214636490590110272E-14, -1.836970198721007747E-16 ) ) ;
#47959 = ORIENTED_EDGE ( 'NONE', *, *, #50073, .T. ) ;
#47960 = LINE ( 'NONE', #16827, #42632 ) ;
#47961 = CARTESIAN_POINT ( 'NONE',  ( -10.91351654964670992, -2.706483450353338593, 455.0000000000000568 ) ) ;
#47962 = LINE ( 'NONE', #21090, #9614 ) ;
#47963 = CARTESIAN_POINT ( 'NONE',  ( 283.0000000000000568, -23.70411739045900390, -12.50000000000000000 ) ) ;
#47964 = AXIS2_PLACEMENT_3D ( 'NONE', #67073, #39499, #61403 ) ;
#47965 = ORIENTED_EDGE ( 'NONE', *, *, #50305, .F. ) ;
#47966 = DIRECTION ( 'NONE',  ( 0.000000000000000000, 0.000000000000000000, 1.000000000000000000 ) ) ;
#47967 = DIRECTION ( 'NONE',  ( 1.000000000000000000, -0.000000000000000000, 0.000000000000000000 ) ) ;
#47968 = AXIS2_PLACEMENT_3D ( 'NONE', #39289, #62243, #39624 ) ;
#47969 = CARTESIAN_POINT ( 'NONE',  ( -25.50000000000000355, 0.000000000000000000, -20.24999999999999645 ) ) ;
#47970 = DIRECTION ( 'NONE',  ( 0.000000000000000000, 1.000000000000000000, 0.000000000000000000 ) ) ;
#47971 = VERTEX_POINT ( 'NONE', #6578 ) ;
#47972 = DIRECTION ( 'NONE',  ( 0.000000000000000000, 0.000000000000000000, -1.000000000000000000 ) ) ;
#47973 = CARTESIAN_POINT ( 'NONE',  ( 15.50000000000000000, -1.037157890325000054, -18.50000000000000000 ) ) ;
#47974 = CARTESIAN_POINT ( 'NONE',  ( 30.00000000000000000, -11.50000000000100009, 15.00000000000084910 ) ) ;
#47975 = EDGE_CURVE ( 'NONE', #16799, #27858, #18001, .T. ) ;
#47976 = DIRECTION ( 'NONE',  ( 0.000000000000000000, 0.000000000000000000, -1.000000000000000000 ) ) ;
#47977 = FILL_AREA_STYLE ('',( #26413 ) ) ;
#47978 = LINE ( 'NONE', #36672, #13566 ) ;
#47979 = EDGE_LOOP ( 'NONE', ( #11382, #4028, #48324, #32274 ) ) ;
#47980 = EDGE_CURVE ( 'NONE', #22897, #29653, #59819, .T. ) ;
#47981 = ORIENTED_EDGE ( 'NONE', *, *, #8343, .T. ) ;
#47982 = CYLINDRICAL_SURFACE ( 'NONE', #16894, 24.99999999998784972 ) ;
#47983 = DIRECTION ( 'NONE',  ( -1.000000000000000000, 1.260948829465470062E-14, -1.836970198721007008E-16 ) ) ;
#47984 = ORIENTED_EDGE ( 'NONE', *, *, #289, .F. ) ;
#47985 = ADVANCED_FACE ( 'NONE', ( #59957 ), #17516, .F. ) ;
#47986 = DIRECTION ( 'NONE',  ( 1.000000000000000000, -0.000000000000000000, -0.000000000000000000 ) ) ;
#47987 = DIRECTION ( 'NONE',  ( 0.000000000000000000, 0.000000000000000000, 1.000000000000000000 ) ) ;
#47988 = ADVANCED_FACE ( 'NONE', ( #11167 ), #27439, .F. ) ;
#47989 = VECTOR ( 'NONE', #19609, 1000.000000000000000 ) ;
#47990 = ORIENTED_EDGE ( 'NONE', *, *, #47243, .T. ) ;
#47991 = DIRECTION ( 'NONE',  ( 0.000000000000000000, -1.000000000000000000, 0.000000000000000000 ) ) ;
#47992 = ORIENTED_EDGE ( 'NONE', *, *, #55882, .T. ) ;
#47993 = EDGE_CURVE ( 'NONE', #54514, #705, #27786, .T. ) ;
#47994 = ORIENTED_EDGE ( 'NONE', *, *, #30306, .F. ) ;
#47995 = DIRECTION ( 'NONE',  ( -1.000000000000000000, 0.000000000000000000, -0.000000000000000000 ) ) ;
#47996 = VERTEX_POINT ( 'NONE', #37709 ) ;
#47997 = CYLINDRICAL_SURFACE ( 'NONE', #50050, 24.99999999998784972 ) ;
#47998 = DIRECTION ( 'NONE',  ( -1.000000000000000000, 5.626525616968433120E-15, 0.000000000000000000 ) ) ;
#47999 = LINE ( 'NONE', #9473, #33607 ) ;
#48000 = AXIS2_PLACEMENT_3D ( 'NONE', #27571, #56179, #33566 ) ;
#48001 = DIRECTION ( 'NONE',  ( 0.000000000000000000, 0.000000000000000000, -1.000000000000000000 ) ) ;
#48002 = ORIENTED_EDGE ( 'NONE', *, *, #66898, .T. ) ;
#48003 = ORIENTED_EDGE ( 'NONE', *, *, #40978, .T. ) ;
#48004 = CARTESIAN_POINT ( 'NONE',  ( 283.0000000000000568, -29.94999999999999929, 14.50000000000000000 ) ) ;
#48006 = CARTESIAN_POINT ( 'NONE',  ( 29.25000000000000000, -5.200000000000001066, -26.25000000000000000 ) ) ;
#48005 = DIRECTION ( 'NONE',  ( 0.7071067811865500152, 0.7071067811865451302, -4.683861624749757595E-31 ) ) ;
#48007 = VECTOR ( 'NONE', #48360, 1000.000000000000000 ) ;
#48008 = AXIS2_PLACEMENT_3D ( 'NONE', #26004, #25658, #47220 ) ;
#48009 = ORIENTED_EDGE ( 'NONE', *, *, #38828, .T. ) ;
#48010 = ORIENTED_EDGE ( 'NONE', *, *, #3969, .T. ) ;
#48011 = EDGE_CURVE ( 'NONE', #33817, #50086, #33089, .T. ) ;
#48012 = ORIENTED_EDGE ( 'NONE', *, *, #25920, .F. ) ;
#48013 = VECTOR ( 'NONE', #12832, 1000.000000000000000 ) ;
#48014 = CARTESIAN_POINT ( 'NONE',  ( 7.250000000000005329, -7.449999999999998401, -21.00000000000000000 ) ) ;
#48016 = EDGE_LOOP ( 'NONE', ( #37511, #55557, #33612, #48060 ) ) ;
#48015 = CARTESIAN_POINT ( 'NONE',  ( -7.250000000000001776, -7.249999999999998224, -10.00000000000000000 ) ) ;
#48017 = CARTESIAN_POINT ( 'NONE',  ( -3.663616288757090445, -4.149127210878730487, 54.00000000000000711 ) ) ;
#48018 = MECHANICAL_DESIGN_GEOMETRIC_PRESENTATION_REPRESENTATION (  '', ( #38970 ), #5069 ) ;
#48019 = CARTESIAN_POINT ( 'NONE',  ( 7.000000000000000000, -20.40000000000000213, -17.60000000000000142 ) ) ;
#48020 = ORIENTED_EDGE ( 'NONE', *, *, #17572, .F. ) ;
#48021 = ORIENTED_EDGE ( 'NONE', *, *, #203, .T. ) ;
#48022 = CIRCLE ( 'NONE', #17518, 2.000000000000001776 ) ;
#48023 = FACE_OUTER_BOUND ( 'NONE', #59274, .T. ) ;
#48024 = VERTEX_POINT ( 'NONE', #571 ) ;
#48025 = CARTESIAN_POINT ( 'NONE',  ( 11.75000000000000000, -5.000000000000000000, 21.10805890929250239 ) ) ;
#48026 = CARTESIAN_POINT ( 'NONE',  ( -5.993516549646799696, -8.211283450353425550, 455.0000000000000568 ) ) ;
#48027 = DIRECTION ( 'NONE',  ( -1.000000000000000000, 0.000000000000000000, 0.000000000000000000 ) ) ;
#48028 = EDGE_CURVE ( 'NONE', #29479, #6534, #30441, .T. ) ;
#48029 = ORIENTED_EDGE ( 'NONE', *, *, #16372, .T. ) ;
#48030 = ADVANCED_FACE ( 'NONE', ( #11506 ), #53979, .F. ) ;
#48031 = CARTESIAN_POINT ( 'NONE',  ( 30.00000000000000000, -16.28999999999710369, 15.00000000000794920 ) ) ;
#48032 = CARTESIAN_POINT ( 'NONE',  ( -11.99351654964674374, -4.186483450353318148, 455.0000000000000568 ) ) ;
#48033 = ORIENTED_EDGE ( 'NONE', *, *, #54318, .T. ) ;
#48034 = VERTEX_POINT ( 'NONE', #939 ) ;
#48035 = DIRECTION ( 'NONE',  ( 0.000000000000000000, 0.000000000000000000, -1.000000000000000000 ) ) ;
#48036 = DIRECTION ( 'NONE',  ( -1.000000000000000000, 0.000000000000000000, 0.000000000000000000 ) ) ;
#48037 = VECTOR ( 'NONE', #29965, 1000.000000000000000 ) ;
#48038 = CARTESIAN_POINT ( 'NONE',  ( 8.249999999999996447, -7.848062532927998269, 5.000000000000000000 ) ) ;
#48039 = FACE_OUTER_BOUND ( 'NONE', #40771, .T. ) ;
#48040 = AXIS2_PLACEMENT_3D ( 'NONE', #66397, #66732, #49098 ) ;
#48041 = CARTESIAN_POINT ( 'NONE',  ( 6.665817930929297752, -7.532023737882814096, 26.00000000000000000 ) ) ;
#48042 = VERTEX_POINT ( 'NONE', #17168 ) ;
#48043 = DIRECTION ( 'NONE',  ( -1.836970198721029934E-16, 1.836970198721036344E-16, -1.000000000000000000 ) ) ;
#48044 = CARTESIAN_POINT ( 'NONE',  ( -3.650476262117333892, -10.31452373788281740, 54.00000000000000711 ) ) ;
#48045 = DIRECTION ( 'NONE',  ( 0.000000000000000000, 0.000000000000000000, 1.000000000000000000 ) ) ;
#48047 = ORIENTED_EDGE ( 'NONE', *, *, #63553, .T. ) ;
#48046 = FACE_OUTER_BOUND ( 'NONE', #32198, .T. ) ;
#48048 = AXIS2_PLACEMENT_3D ( 'NONE', #59928, #48629, #5845 ) ;
#48049 = CIRCLE ( 'NONE', #58192, 0.5999999999999989786 ) ;
#48050 = AXIS2_PLACEMENT_3D ( 'NONE', #11551, #33130, #29824 ) ;
#48051 = PRESENTATION_STYLE_ASSIGNMENT (( #49446 ) ) ;
#48052 = DIRECTION ( 'NONE',  ( 0.000000000000000000, 1.000000000000000000, 0.000000000000000000 ) ) ;
#48053 = CARTESIAN_POINT ( 'NONE',  ( -1.677516549646683730, 9.828310488885911411, 455.0000000000000568 ) ) ;
#48054 = VECTOR ( 'NONE', #31029, 1000.000000000000000 ) ;
#48055 = VECTOR ( 'NONE', #52886, 1000.000000000000000 ) ;
#48056 = PLANE ( 'NONE',  #1704 ) ;
#48057 = ORIENTED_EDGE ( 'NONE', *, *, #41602, .F. ) ;
#48058 = LINE ( 'NONE', #52682, #16251 ) ;
#48059 = FACE_OUTER_BOUND ( 'NONE', #50443, .T. ) ;
#48060 = ORIENTED_EDGE ( 'NONE', *, *, #4273, .T. ) ;
#48061 = LINE ( 'NONE', #64330, #52618 ) ;
#48062 = CARTESIAN_POINT ( 'NONE',  ( 9.106483450353380249, -10.92648345035348711, 455.0000000000000568 ) ) ;
#48063 = CIRCLE ( 'NONE', #40162, 0.06000000000000102474 ) ;
#48064 = DIRECTION ( 'NONE',  ( 0.000000000000000000, 0.000000000000000000, 1.000000000000000000 ) ) ;
#48065 = CARTESIAN_POINT ( 'NONE',  ( -3.834182069070763976, 7.517976262117170627, 54.00000000000000711 ) ) ;
#48066 = EDGE_CURVE ( 'NONE', #7845, #26371, #54181, .T. ) ;
#48067 = CARTESIAN_POINT ( 'NONE',  ( -25.50000000000000355, -5.200000000000001066, -22.50000000000000000 ) ) ;
#48068 =( GEOMETRIC_REPRESENTATION_CONTEXT ( 3 ) GLOBAL_UNCERTAINTY_ASSIGNED_CONTEXT ( ( #59235 ) ) GLOBAL_UNIT_ASSIGNED_CONTEXT ( ( #1868, #1512, #12458 ) ) REPRESENTATION_CONTEXT ( 'NONE', 'WORKASPACE' ) );
#48069 = ORIENTED_EDGE ( 'NONE', *, *, #15062, .F. ) ;
#48070 = VERTEX_POINT ( 'NONE', #53630 ) ;
#48071 = CARTESIAN_POINT ( 'NONE',  ( 4.396432944014577515, 8.593516549646585290, 455.0000000000000568 ) ) ;
#48072 = VERTEX_POINT ( 'NONE', #55025 ) ;
#48073 = ORIENTED_EDGE ( 'NONE', *, *, #47915, .F. ) ;
#48074 = AXIS2_PLACEMENT_3D ( 'NONE', #36843, #57689, #9259 ) ;
#48075 = EDGE_CURVE ( 'NONE', #27294, #21746, #49698, .T. ) ;
#48076 = DIRECTION ( 'NONE',  ( 0.000000000000000000, 1.000000000000000000, 0.000000000000000000 ) ) ;
#48077 = ADVANCED_FACE ( 'NONE', ( #43000, #64579 ), #10825, .F. ) ;
#48078 = ADVANCED_FACE ( 'NONE', ( #28808 ), #62033, .F. ) ;
#48079 = DIRECTION ( 'NONE',  ( 1.000000000000000000, -8.728482790395504563E-15, -3.206792553201184024E-30 ) ) ;
#48080 = CARTESIAN_POINT ( 'NONE',  ( -6.606374702650259501, -7.265214908726163046, 455.0000000000000568 ) ) ;
#48081 = ORIENTED_EDGE ( 'NONE', *, *, #34281, .F. ) ;
#48082 = EDGE_CURVE ( 'NONE', #23904, #55686, #34811, .T. ) ;
#48083 = ORIENTED_EDGE ( 'NONE', *, *, #35375, .T. ) ;
#48084 = EDGE_CURVE ( 'NONE', #11897, #39293, #7599, .T. ) ;
#48085 = DIRECTION ( 'NONE',  ( 0.6785983445458448893, -0.2810846377148217834, 0.6785983445458485530 ) ) ;
#48086 = ORIENTED_EDGE ( 'NONE', *, *, #44744, .F. ) ;
#48087 = EDGE_LOOP ( 'NONE', ( #60644, #59161, #38136, #69766 ) ) ;
#48088 = CARTESIAN_POINT ( 'NONE',  ( 14.66434062215688883, -0.3156604612129108589, -23.46090750622545684 ) ) ;
#48089 = DIRECTION ( 'NONE',  ( 0.000000000000000000, -0.7057491738665943037, -0.7084617869628675457 ) ) ;
#48090 = DIRECTION ( 'NONE',  ( 0.000000000000000000, 0.000000000000000000, 1.000000000000000000 ) ) ;
#48091 = EDGE_CURVE ( 'NONE', #17044, #40228, #13604, .T. ) ;
#48092 = AXIS2_PLACEMENT_3D ( 'NONE', #48644, #50019, #27425 ) ;
#48093 = ORIENTED_EDGE ( 'NONE', *, *, #1534, .T. ) ;
#48094 = CARTESIAN_POINT ( 'NONE',  ( 7.450000000000003730, -7.249999999999997335, -9.000000000000001776 ) ) ;
#48096 = CARTESIAN_POINT ( 'NONE',  ( -15.50000000000000000, -15.50000000000000000, -25.99999999999985079 ) ) ;
#48095 = DIRECTION ( 'NONE',  ( -8.903847840905249551E-15, -1.000000000000000000, -1.836970198721027222E-16 ) ) ;
#48097 = EDGE_LOOP ( 'NONE', ( #19430, #12403, #29897, #62247, #19047, #3649, #47441, #60327 ) ) ;
#48099 = ORIENTED_EDGE ( 'NONE', *, *, #17074, .T. ) ;
#48098 = CARTESIAN_POINT ( 'NONE',  ( 170.5922698879802226, -35.25383818724483831, 0.000000000000000000 ) ) ;
#48100 = AXIS2_PLACEMENT_3D ( 'NONE', #24238, #55712, #18571 ) ;
#48101 = VERTEX_POINT ( 'NONE', #40826 ) ;
#48102 = AXIS2_PLACEMENT_3D ( 'NONE', #32062, #53638, #5540 ) ;
#48103 = DIRECTION ( 'NONE',  ( 1.836970198721029934E-16, 1.836970198721010706E-16, -1.000000000000000000 ) ) ;
#48104 = AXIS2_PLACEMENT_3D ( 'NONE', #51397, #57049, #47498 ) ;
#48105 = VECTOR ( 'NONE', #27437, 1000.000000000000000 ) ;
#48106 = DIRECTION ( 'NONE',  ( -1.000000000000000000, 0.000000000000000000, 0.000000000000000000 ) ) ;
#48107 = VERTEX_POINT ( 'NONE', #46129 ) ;
#48108 = AXIS2_PLACEMENT_3D ( 'NONE', #69161, #26034, #20715 ) ;
#48109 = VECTOR ( 'NONE', #39450, 1000.000000000000000 ) ;
#48110 = AXIS2_PLACEMENT_3D ( 'NONE', #8143, #24425, #45989 ) ;
#48111 = DIRECTION ( 'NONE',  ( 0.000000000000000000, 0.000000000000000000, 1.000000000000000000 ) ) ;
#48112 = CARTESIAN_POINT ( 'NONE',  ( 15.00000000000000000, -23.65000000000000568, 12.40000000000000213 ) ) ;
#48113 = ORIENTED_EDGE ( 'NONE', *, *, #52727, .T. ) ;
#48114 = ORIENTED_EDGE ( 'NONE', *, *, #42666, .T. ) ;
#48115 = LINE ( 'NONE', #58387, #10461 ) ;
#48117 = VECTOR ( 'NONE', #39809, 1000.000000000000000 ) ;
#48116 = CARTESIAN_POINT ( 'NONE',  ( 9.900000000000000355, -18.00000000000000355, -21.00000000000000000 ) ) ;
#48118 = CARTESIAN_POINT ( 'NONE',  ( 0.5000000000000000000, -21.00000000000000000, 18.00000000000000355 ) ) ;
#48119 = ORIENTED_EDGE ( 'NONE', *, *, #9695, .F. ) ;
#48120 = ADVANCED_FACE ( 'NONE', ( #2641 ), #45073, .T. ) ;
#48121 = ADVANCED_FACE ( 'NONE', ( #67696, #1593 ), #62379, .F. ) ;
#48122 = LINE ( 'NONE', #10626, #18802 ) ;
#48123 = CARTESIAN_POINT ( 'NONE',  ( 6.657023737882818537, -10.31452373788282095, 54.00000000000000711 ) ) ;
#48126 = VERTEX_POINT ( 'NONE', #60986 ) ;
#48125 = EDGE_CURVE ( 'NONE', #66609, #48603, #45422, .T. ) ;
#48124 = LINE ( 'NONE', #38, #13747 ) ;
#48127 = VECTOR ( 'NONE', #4231, 1000.000000000000000 ) ;
#48129 = VERTEX_POINT ( 'NONE', #33775 ) ;
#48128 = FACE_OUTER_BOUND ( 'NONE', #60693, .T. ) ;
#48130 = EDGE_CURVE ( 'NONE', #33635, #55576, #25917, .T. ) ;
#48131 = FACE_OUTER_BOUND ( 'NONE', #19365, .T. ) ;
#48132 = CARTESIAN_POINT ( 'NONE',  ( 280.0000000000000000, -25.50000000000000355, -20.00000000000000000 ) ) ;
#48133 = CARTESIAN_POINT ( 'NONE',  ( 7.000000000000000000, -25.60000000000000142, 15.10000000000000142 ) ) ;
#48134 = CARTESIAN_POINT ( 'NONE',  ( 5.552858015815581361, -7.357023737882824044, 54.00000000000000711 ) ) ;
#48135 = ADVANCED_FACE ( 'NONE', ( #29516 ), #12545, .T. ) ;
#48136 = CARTESIAN_POINT ( 'NONE',  ( 37.90000000000000568, -0.000000000000000000, -20.80000000000000071 ) ) ;
#48137 = DIRECTION ( 'NONE',  ( -1.836970198721029934E-16, 1.836970198721036590E-16, -1.000000000000000000 ) ) ;
#48138 = ORIENTED_EDGE ( 'NONE', *, *, #24756, .T. ) ;
#48139 = DIRECTION ( 'NONE',  ( -1.000000000000000000, 0.000000000000000000, 0.000000000000000000 ) ) ;
#48141 = ORIENTED_EDGE ( 'NONE', *, *, #4058, .F. ) ;
#48140 = DIRECTION ( 'NONE',  ( 1.000000000000000000, -0.000000000000000000, -0.000000000000000000 ) ) ;
#48142 = LINE ( 'NONE', #69717, #32199 ) ;
#48143 = CARTESIAN_POINT ( 'NONE',  ( -8.250000000000001776, -7.249999999999998224, -26.00000000000001066 ) ) ;
#48144 = VECTOR ( 'NONE', #27693, 1000.000000000000000 ) ;
#48145 = LINE ( 'NONE', #53455, #57790 ) ;
#48146 = CIRCLE ( 'NONE', #26646, 0.5000000000000000000 ) ;
#48147 = EDGE_LOOP ( 'NONE', ( #47047, #39459, #65155, #38861 ) ) ;
#48148 = CARTESIAN_POINT ( 'NONE',  ( 41.09999999999999432, -0.1999999999911430404, -8.864436962241481021E-12 ) ) ;
#48149 = PLANE ( 'NONE',  #1209 ) ;
#48150 = EDGE_LOOP ( 'NONE', ( #5277, #62519, #1287, #2690, #18147, #10797, #3464, #44540 ) ) ;
#48151 = FACE_OUTER_BOUND ( 'NONE', #22393, .T. ) ;
#48152 = FILL_AREA_STYLE_COLOUR ( '', #21242 ) ;
#48153 = VECTOR ( 'NONE', #27683, 1000.000000000000000 ) ;
#48154 = CIRCLE ( 'NONE', #34596, 0.4999999999991842636 ) ;
#48155 = EDGE_CURVE ( 'NONE', #27113, #2487, #56043, .T. ) ;
#48156 = AXIS2_PLACEMENT_3D ( 'NONE', #9941, #31510, #42796 ) ;
#48157 = VERTEX_POINT ( 'NONE', #29163 ) ;
#48158 = CARTESIAN_POINT ( 'NONE',  ( -4.173516549646666185, 11.99351654964658920, 195.0000000000000284 ) ) ;
#48159 = VERTEX_POINT ( 'NONE', #50728 ) ;
#48160 = ORIENTED_EDGE ( 'NONE', *, *, #24748, .T. ) ;
#48161 = DIRECTION ( 'NONE',  ( 1.836970198721029934E-16, 1.836970198721010706E-16, -1.000000000000000000 ) ) ;
#48163 = CARTESIAN_POINT ( 'NONE',  ( 275.0000000000000000, -20.40000000000000213, 12.40000000000000213 ) ) ;
#48162 = CIRCLE ( 'NONE', #11986, 1.224999999999998757 ) ;
#48164 = VECTOR ( 'NONE', #36886, 1000.000000000000000 ) ;
#48165 = CIRCLE ( 'NONE', #10850, 0.3499999999999996447 ) ;
#48166 = VECTOR ( 'NONE', #29298, 1000.000000000000000 ) ;
#48167 = DIRECTION ( 'NONE',  ( 1.000000000000000000, 0.000000000000000000, -0.000000000000000000 ) ) ;
#48168 = DIRECTION ( 'NONE',  ( -0.000000000000000000, -0.000000000000000000, 1.000000000000000000 ) ) ;
#48169 = ORIENTED_EDGE ( 'NONE', *, *, #24672, .T. ) ;
#48170 = ORIENTED_EDGE ( 'NONE', *, *, #11062, .T. ) ;
#48171 = ADVANCED_FACE ( 'NONE', ( #2300 ), #8286, .T. ) ;
#48173 = VERTEX_POINT ( 'NONE', #23863 ) ;
#48172 = FACE_OUTER_BOUND ( 'NONE', #16221, .T. ) ;
#48174 = ORIENTED_EDGE ( 'NONE', *, *, #21777, .F. ) ;
#48175 = VECTOR ( 'NONE', #47847, 1000.000000000000000 ) ;
#48176 = DIRECTION ( 'NONE',  ( -1.836970198721029934E-16, 1.836970198721036590E-16, -1.000000000000000000 ) ) ;
#48177 = CARTESIAN_POINT ( 'NONE',  ( 8.093267424590464998, -8.711985858128699078, 54.00000000000000711 ) ) ;
#48178 = EDGE_CURVE ( 'NONE', #32858, #43292, #39455, .T. ) ;
#48179 = LINE ( 'NONE', #42859, #20686 ) ;
#48180 = FACE_OUTER_BOUND ( 'NONE', #32180, .T. ) ;
#48182 = CYLINDRICAL_SURFACE ( 'NONE', #5213, 1.000000000000000000 ) ;
#48181 = LINE ( 'NONE', #47132, #10671 ) ;
#48183 = EDGE_LOOP ( 'NONE', ( #53168, #28373, #50687, #3277 ) ) ;
#48184 = ORIENTED_EDGE ( 'NONE', *, *, #25749, .F. ) ;
#48185 = ORIENTED_EDGE ( 'NONE', *, *, #31040, .T. ) ;
#48186 = EDGE_LOOP ( 'NONE', ( #4523, #69580, #36271, #63832, #46077 ) ) ;
#48187 = LINE ( 'NONE', #14262, #60401 ) ;
#48188 = FACE_OUTER_BOUND ( 'NONE', #7544, .T. ) ;
#48189 =( LENGTH_UNIT ( ) NAMED_UNIT ( * ) SI_UNIT ( .MILLI., .METRE. ) );
#48190 = ADVANCED_FACE ( 'NONE', ( #51081 ), #61685, .F. ) ;
#48191 = DIRECTION ( 'NONE',  ( 0.000000000000000000, 0.7071067811865496822, 0.7071067811865454633 ) ) ;
#48192 = ORIENTED_EDGE ( 'NONE', *, *, #34732, .T. ) ;
#48193 = ORIENTED_EDGE ( 'NONE', *, *, #36935, .F. ) ;
#48194 = VECTOR ( 'NONE', #58, 1000.000000000000000 ) ;
#48195 = ORIENTED_EDGE ( 'NONE', *, *, #21305, .F. ) ;
#48196 = CARTESIAN_POINT ( 'NONE',  ( -8.393516549646768965, -5.668387132715940524, 455.0000000000000568 ) ) ;
#48197 = ORIENTED_EDGE ( 'NONE', *, *, #4359, .T. ) ;
#48198 = CARTESIAN_POINT ( 'NONE',  ( -7.250000000000000888, 8.250000000000001776, -26.00000000000001066 ) ) ;
#48199 = AXIS2_PLACEMENT_3D ( 'NONE', #19620, #4081, #15030 ) ;
#48200 = CARTESIAN_POINT ( 'NONE',  ( 6.657023737882818537, -10.31452373788282095, 54.00000000000000711 ) ) ;
#48201 = ORIENTED_EDGE ( 'NONE', *, *, #10469, .F. ) ;
#48202 = ORIENTED_EDGE ( 'NONE', *, *, #15496, .T. ) ;
#48203 = VECTOR ( 'NONE', #67525, 1000.000000000000000 ) ;
#48205 = CARTESIAN_POINT ( 'NONE',  ( -7.250000000000000888, 8.250000000000001776, -26.00000000000001066 ) ) ;
#48204 = CIRCLE ( 'NONE', #17700, 3.499999999999849454 ) ;
#48206 = CARTESIAN_POINT ( 'NONE',  ( -16.75000000000000000, -0.2038245569916330158, -23.22168783648699986 ) ) ;
#48207 = ORIENTED_EDGE ( 'NONE', *, *, #38404, .T. ) ;
#48208 = AXIS2_PLACEMENT_3D ( 'NONE', #12549, #22495, #1267 ) ;
#48209 = VECTOR ( 'NONE', #6016, 1000.000000000000000 ) ;
#48210 =( GEOMETRIC_REPRESENTATION_CONTEXT ( 3 ) GLOBAL_UNCERTAINTY_ASSIGNED_CONTEXT ( ( #21755 ) ) GLOBAL_UNIT_ASSIGNED_CONTEXT ( ( #23818, #45371, #12499 ) ) REPRESENTATION_CONTEXT ( 'NONE', 'WORKASPACE' ) );
#48211 = CARTESIAN_POINT ( 'NONE',  ( -4.393516549646788505, -11.78648345035339418, 195.0000000000000284 ) ) ;
#48214 = ORIENTED_EDGE ( 'NONE', *, *, #6233, .T. ) ;
#48213 = ADVANCED_FACE ( 'NONE', ( #40473 ), #6901, .F. ) ;
#48212 = CARTESIAN_POINT ( 'NONE',  ( 11.00000000000000000, -15.46862696659690073, -14.50000000000000000 ) ) ;
#48215 = VERTEX_POINT ( 'NONE', #8651 ) ;
#48216 = CARTESIAN_POINT ( 'NONE',  ( 7.969523737882818537, -9.562023737882819674, 54.00000000000000711 ) ) ;
#48217 = VECTOR ( 'NONE', #36110, 1000.000000000000000 ) ;
#48218 = CARTESIAN_POINT ( 'NONE',  ( 0.000000000000000000, 8.250000000000001776, -14.00000000000000000 ) ) ;
#48219 = VECTOR ( 'NONE', #1987, 1000.000000000000000 ) ;
#48220 = CARTESIAN_POINT ( 'NONE',  ( -6.817976262117325881, -9.737023737882786634, 54.00000000000000711 ) ) ;
#48221 = CARTESIAN_POINT ( 'NONE',  ( 8.406483450353405829, 7.603567055985406498, 455.0000000000000568 ) ) ;
#48222 = ADVANCED_FACE ( 'NONE', ( #14317 ), #8994, .T. ) ;
#48223 = LINE ( 'NONE', #69433, #56469 ) ;
#48224 = VECTOR ( 'NONE', #11229, 1000.000000000000000 ) ;
#48225 = ORIENTED_EDGE ( 'NONE', *, *, #11548, .F. ) ;
#48226 = DIRECTION ( 'NONE',  ( -1.000000000000000000, 0.000000000000000000, 0.000000000000000000 ) ) ;
#48227 = VERTEX_POINT ( 'NONE', #68405 ) ;
#48228 = VECTOR ( 'NONE', #57680, 1000.000000000000000 ) ;
#48229 = DIRECTION ( 'NONE',  ( 0.000000000000000000, -0.7278708115916149302, -0.6857142857145122061 ) ) ;
#48230 = FACE_OUTER_BOUND ( 'NONE', #18128, .T. ) ;
#48231 = CARTESIAN_POINT ( 'NONE',  ( 146.5599459900709860, 5.000000000000000000, 320.8239988703753056 ) ) ;
#48232 = CARTESIAN_POINT ( 'NONE',  ( -6.331612867284244217, -8.406483450353421816, 455.0000000000000568 ) ) ;
#48233 = PLANE ( 'NONE',  #33712 ) ;
#48234 = ORIENTED_EDGE ( 'NONE', *, *, #44959, .F. ) ;
#48235 = EDGE_CURVE ( 'NONE', #54092, #5641, #35878, .T. ) ;
#48236 = DIRECTION ( 'NONE',  ( 0.000000000000000000, 0.000000000000000000, -1.000000000000000000 ) ) ;
#48237 = FACE_BOUND ( 'NONE', #51329, .T. ) ;
#48238 = VERTEX_POINT ( 'NONE', #36944 ) ;
#48239 = DIRECTION ( 'NONE',  ( 0.000000000000000000, -1.000000000000000000, 0.000000000000000000 ) ) ;
#48240 = DIRECTION ( 'NONE',  ( -0.000000000000000000, -0.000000000000000000, -1.000000000000000000 ) ) ;
#48241 = EDGE_LOOP ( 'NONE', ( #4989, #65926, #50953, #29264 ) ) ;
#48242 = DIRECTION ( 'NONE',  ( 0.000000000000000000, 0.000000000000000000, -1.000000000000000000 ) ) ;
#48243 = LINE ( 'NONE', #48589, #26327 ) ;
#48244 = ORIENTED_EDGE ( 'NONE', *, *, #16553, .F. ) ;
#48245 = CARTESIAN_POINT ( 'NONE',  ( -30.00000000000000000, -16.64230188589299786, -14.64519951917100116 ) ) ;
#48246 = DIRECTION ( 'NONE',  ( 0.000000000000000000, 0.000000000000000000, -1.000000000000000000 ) ) ;
#48247 = CIRCLE ( 'NONE', #17748, 3.500000000000003109 ) ;
#48248 = VECTOR ( 'NONE', #20114, 1000.000000000000000 ) ;
#48249 = B_SPLINE_CURVE_WITH_KNOTS ( 'NONE', 3,
 ( #54610, #16775, #38681, #21025, #15733, #37999 ),
 .UNSPECIFIED., .F., .F.,
 ( 4, 2, 4 ),
 ( 0.0002380763768132926339, 0.7291065797294586925, 1.457975083082104106 ),
 .UNSPECIFIED. ) ;
#48250 = LINE ( 'NONE', #33371, #20436 ) ;
#48251 = ORIENTED_EDGE ( 'NONE', *, *, #23747, .T. ) ;
#48253 = ORIENTED_EDGE ( 'NONE', *, *, #61950, .T. ) ;
#48252 = CARTESIAN_POINT ( 'NONE',  ( -5.538810540050059572, -7.357023737882796510, 26.00000000000000711 ) ) ;
#48254 = EDGE_CURVE ( 'NONE', #17912, #43298, #41877, .T. ) ;
#48255 = VECTOR ( 'NONE', #63807, 1000.000000000000000 ) ;
#48256 = AXIS2_PLACEMENT_3D ( 'NONE', #6547, #44345, #49342 ) ;
#48257 = DIRECTION ( 'NONE',  ( -1.000000000000000000, 0.000000000000000000, 0.000000000000000000 ) ) ;
#48258 = AXIS2_PLACEMENT_3D ( 'NONE', #55142, #6686, #61455 ) ;
#48259 = EDGE_CURVE ( 'NONE', #38194, #52237, #66564, .T. ) ;
#48260 = PLANE ( 'NONE',  #35702 ) ;
#48261 = DIRECTION ( 'NONE',  ( 0.000000000000000000, 0.000000000000000000, -1.000000000000000000 ) ) ;
#48262 = ORIENTED_EDGE ( 'NONE', *, *, #21341, .T. ) ;
#48263 = EDGE_CURVE ( 'NONE', #39654, #50592, #51792, .T. ) ;
#48264 = AXIS2_PLACEMENT_3D ( 'NONE', #21078, #25702, #42989 ) ;
#48266 = PLANE ( 'NONE',  #48008 ) ;
#48265 = VECTOR ( 'NONE', #16617, 1000.000000000000000 ) ;
#48267 = CARTESIAN_POINT ( 'NONE',  ( 10.00000000000000000, 18.00000000000000355, 21.00000000000000000 ) ) ;
#48268 = ADVANCED_FACE ( 'NONE', ( #25630 ), #57787, .F. ) ;
#48269 = VERTEX_POINT ( 'NONE', #57089 ) ;
#48270 = EDGE_LOOP ( 'NONE', ( #53449, #26243, #4354, #16197 ) ) ;
#48271 = ADVANCED_FACE ( 'NONE', ( #41531 ), #52862, .F. ) ;
#48272 = ORIENTED_EDGE ( 'NONE', *, *, #47105, .F. ) ;
#48273 = ADVANCED_FACE ( 'NONE', ( #15011 ), #3701, .T. ) ;
#48274 = CARTESIAN_POINT ( 'NONE',  ( 7.250000000000005329, -7.249999999999998224, -26.00000000000001066 ) ) ;
#48275 = ADVANCED_FACE ( 'NONE', ( #19958 ), #36568, .F. ) ;
#48276 = DIRECTION ( 'NONE',  ( -1.000000000000000000, -2.135044278125301343E-15, -7.844025423732065664E-31 ) ) ;
#48277 = CARTESIAN_POINT ( 'NONE',  ( -11.00000000000000000, -17.14999999999999858, -27.00000000000000000 ) ) ;
#48278 = CIRCLE ( 'NONE', #21168, 0.5000000000000000000 ) ;
#48279 = EDGE_LOOP ( 'NONE', ( #62395, #38261 ) ) ;
#48280 = VERTEX_POINT ( 'NONE', #52495 ) ;
#48281 = CARTESIAN_POINT ( 'NONE',  ( 0.5000000000000000000, -21.00000000000000000, -18.00000000000000355 ) ) ;
#48282 = ORIENTED_EDGE ( 'NONE', *, *, #67400, .F. ) ;
#48283 = EDGE_LOOP ( 'NONE', ( #5576, #29101, #18014, #66231 ) ) ;
#48284 = ORIENTED_EDGE ( 'NONE', *, *, #58933, .F. ) ;
#48285 = VERTEX_POINT ( 'NONE', #62739 ) ;
#48286 = CARTESIAN_POINT ( 'NONE',  ( 30.00000000000000000, -11.85423089348099879, 9.852125413066602277 ) ) ;
#48288 = ORIENTED_EDGE ( 'NONE', *, *, #69873, .F. ) ;
#48287 = LINE ( 'NONE', #64551, #55907 ) ;
#48289 = CARTESIAN_POINT ( 'NONE',  ( 7.250000000000005329, 7.250000000000000888, -20.50000000000000000 ) ) ;
#48290 = LINE ( 'NONE', #53257, #64541 ) ;
#48291 = CARTESIAN_POINT ( 'NONE',  ( 5.257023737882819070, -5.257023737882825287, 54.00000000000000711 ) ) ;
#48292 = PRESENTATION_LAYER_ASSIGNMENT (  '', '', ( #49448 ) ) ;
#48293 = ORIENTED_EDGE ( 'NONE', *, *, #22070, .T. ) ;
#48294 = CARTESIAN_POINT ( 'NONE',  ( 8.835729544836331328, 8.130476262117188213, 54.00000000000000711 ) ) ;
#48295 = AXIS2_PLACEMENT_3D ( 'NONE', #9861, #14807, #52998 ) ;
#48296 = AXIS2_PLACEMENT_3D ( 'NONE', #28529, #50099, #1653 ) ;
#48297 = DIRECTION ( 'NONE',  ( 1.836970198721029934E-16, -1.836970198721036344E-16, 1.000000000000000000 ) ) ;
#48298 = VERTEX_POINT ( 'NONE', #4062 ) ;
#48299 = DIRECTION ( 'NONE',  ( -1.034072152899300747E-14, -1.000000000000000000, 0.000000000000000000 ) ) ;
#48300 = VECTOR ( 'NONE', #47798, 1000.000000000000000 ) ;
#48301 = VECTOR ( 'NONE', #4725, 1000.000000000000000 ) ;
#48302 = DIRECTION ( 'NONE',  ( 1.000000000000000000, 0.000000000000000000, 0.000000000000000000 ) ) ;
#48303 = CARTESIAN_POINT ( 'NONE',  ( -7.250000000000001776, -7.249999999999998224, -26.00000000000001066 ) ) ;
#48304 = VERTEX_POINT ( 'NONE', #68760 ) ;
#48305 = CARTESIAN_POINT ( 'NONE',  ( 7.250000000000005329, -8.249999999999998224, -26.00000000000001066 ) ) ;
#48306 = VECTOR ( 'NONE', #60891, 1000.000000000000000 ) ;
#48307 = AXIS2_PLACEMENT_3D ( 'NONE', #37395, #58262, #31406 ) ;
#48308 = EDGE_CURVE ( 'NONE', #4905, #10643, #20312, .T. ) ;
#48309 = CARTESIAN_POINT ( 'NONE',  ( 29.50000000000000355, -11.50000000000100009, 19.50000000000103739 ) ) ;
#48310 = DIRECTION ( 'NONE',  ( -0.000000000000000000, -0.000000000000000000, -1.000000000000000000 ) ) ;
#48311 = EDGE_CURVE ( 'NONE', #27939, #56472, #25980, .T. ) ;
#48312 = CARTESIAN_POINT ( 'NONE',  ( 7.250000000000005329, -7.249999999999998224, -18.50000000000000000 ) ) ;
#48313 = DIRECTION ( 'NONE',  ( 0.000000000000000000, 0.000000000000000000, -1.000000000000000000 ) ) ;
#48314 = CARTESIAN_POINT ( 'NONE',  ( -7.593516549646711411, 11.31351654964660014, 455.0000000000000568 ) ) ;
#48315 = LINE ( 'NONE', #31712, #17467 ) ;
#48316 = CARTESIAN_POINT ( 'NONE',  ( 0.000000000000000000, 8.250000000000001776, -11.00000000000000000 ) ) ;
#48317 = VECTOR ( 'NONE', #26390, 1000.000000000000000 ) ;
#48318 = ORIENTED_EDGE ( 'NONE', *, *, #53281, .F. ) ;
#48319 = CARTESIAN_POINT ( 'NONE',  ( 39.90000000000000568, -0.2000000000089119934, 8.909539772616881237E-12 ) ) ;
#48320 = EDGE_CURVE ( 'NONE', #43217, #32555, #68854, .T. ) ;
#48321 = CARTESIAN_POINT ( 'NONE',  ( -4.242044687070550602, 8.452095193409279617, 195.0000000000000284 ) ) ;
#48322 = DIRECTION ( 'NONE',  ( 0.7071067811865422437, -0.7071067811865529018, 0.000000000000000000 ) ) ;
#48323 = CARTESIAN_POINT ( 'NONE',  ( -25.50000000000000355, 0.000000000000000000, -20.87899999999999778 ) ) ;
#48324 = ORIENTED_EDGE ( 'NONE', *, *, #32425, .T. ) ;
#48325 = LINE ( 'NONE', #27792, #27606 ) ;
#48326 = LINE ( 'NONE', #14751, #53111 ) ;
#48327 = ADVANCED_FACE ( 'NONE', ( #24916 ), #35505, .F. ) ;
#48328 = LINE ( 'NONE', #37717, #1737 ) ;
#48329 = DIRECTION ( 'NONE',  ( 0.000000000000000000, 0.6857142857146703019, -0.7278708115914659382 ) ) ;
#48330 = FACE_OUTER_BOUND ( 'NONE', #67829, .T. ) ;
#48331 = DIRECTION ( 'NONE',  ( -1.000000000000000000, 0.000000000000000000, 0.000000000000000000 ) ) ;
#48332 = VERTEX_POINT ( 'NONE', #68052 ) ;
#48333 = VERTEX_POINT ( 'NONE', #69450 ) ;
#48334 = CARTESIAN_POINT ( 'NONE',  ( 49.00000000000000000, -0.2000000000089119934, -8.913009219568841313E-12 ) ) ;
#48335 = EDGE_CURVE ( 'NONE', #43945, #4916, #3335, .T. ) ;
#48336 = DIRECTION ( 'NONE',  ( 0.000000000000000000, 0.000000000000000000, -1.000000000000000000 ) ) ;
#48337 = STYLED_ITEM ( 'NONE', ( #58056 ), #21303 ) ;
#48338 = VERTEX_POINT ( 'NONE', #22059 ) ;
#48339 = DIRECTION ( 'NONE',  ( -9.050731179009442381E-15, -1.000000000000000000, 0.000000000000000000 ) ) ;
#48340 = DIRECTION ( 'NONE',  ( -1.000000000000000000, 0.000000000000000000, 0.000000000000000000 ) ) ;
#48341 = ORIENTED_EDGE ( 'NONE', *, *, #2710, .T. ) ;
#48342 = DIRECTION ( 'NONE',  ( -1.000000000000000000, 0.000000000000000000, 0.000000000000000000 ) ) ;
#48343 = ORIENTED_EDGE ( 'NONE', *, *, #45271, .T. ) ;
#48344 = ORIENTED_EDGE ( 'NONE', *, *, #55883, .T. ) ;
#48346 = EDGE_CURVE ( 'NONE', #67047, #60224, #53547, .T. ) ;
#48345 = CARTESIAN_POINT ( 'NONE',  ( 8.835729544836288696, 2.355476262117161657, 54.00000000000000711 ) ) ;
#48347 = ORIENTED_EDGE ( 'NONE', *, *, #15452, .T. ) ;
#48348 = CARTESIAN_POINT ( 'NONE',  ( -11.99351654964669756, -4.186483450353271074, 195.0000000000000284 ) ) ;
#48349 = EDGE_CURVE ( 'NONE', #49918, #17310, #19125, .T. ) ;
#48350 = VECTOR ( 'NONE', #31825, 1000.000000000000000 ) ;
#48351 = CARTESIAN_POINT ( 'NONE',  ( 7.250000000000005329, -7.449999999999998401, -11.50000000000000000 ) ) ;
#48353 =( BOUNDED_CURVE ( )  B_SPLINE_CURVE ( 3, ( #30235, #19263, #7603, #7944 ),
 .UNSPECIFIED., .F., .F. ) 
 B_SPLINE_CURVE_WITH_KNOTS ( ( 4, 4 ),
 ( 3.864326901403221104, 4.037257447447658798 ),
 .UNSPECIFIED. ) 
 CURVE ( )  GEOMETRIC_REPRESENTATION_ITEM ( )  RATIONAL_B_SPLINE_CURVE ( ( 1.000000000000000000, 0.9975094710839678136, 0.9975094710839678136, 1.000000000000000000 ) ) 
 REPRESENTATION_ITEM ( '' )  );
#48352 = DIRECTION ( 'NONE',  ( 1.000000000000000000, 0.000000000000000000, 0.000000000000000000 ) ) ;
#48354 = ORIENTED_EDGE ( 'NONE', *, *, #63498, .T. ) ;
#48355 = ORIENTED_EDGE ( 'NONE', *, *, #6254, .T. ) ;
#48356 = CARTESIAN_POINT ( 'NONE',  ( 7.000000000000000000, -32.45000000000000995, -15.00000000000000000 ) ) ;
#48357 = VECTOR ( 'NONE', #17295, 1000.000000000000000 ) ;
#48358 = AXIS2_PLACEMENT_3D ( 'NONE', #58885, #32012, #31670 ) ;
#48360 = DIRECTION ( 'NONE',  ( -1.836970198721029934E-16, 1.836970198721036344E-16, -1.000000000000000000 ) ) ;
#48359 = CARTESIAN_POINT ( 'NONE',  ( -11.18071654964676753, -11.19368345035331203, 195.0000000000000284 ) ) ;
#48361 = ORIENTED_EDGE ( 'NONE', *, *, #27491, .T. ) ;
#48362 = EDGE_CURVE ( 'NONE', #8384, #19992, #5803, .T. ) ;
#48363 = VERTEX_POINT ( 'NONE', #64504 ) ;
#48365 = ORIENTED_EDGE ( 'NONE', *, *, #28665, .T. ) ;
#48364 = CONTEXT_DEPENDENT_SHAPE_REPRESENTATION ( #22378, #32379 ) ;
#48366 = CARTESIAN_POINT ( 'NONE',  ( -28.00000000000000000, -17.35230188589299871, -15.35019951917099945 ) ) ;
#48368 = ORIENTED_EDGE ( 'NONE', *, *, #64770, .T. ) ;
#48367 = DIRECTION ( 'NONE',  ( 1.000000000000000000, -8.540177112501197482E-15, 0.000000000000000000 ) ) ;
#48369 = CIRCLE ( 'NONE', #11113, 24.99999999998784972 ) ;
#48370 = DIRECTION ( 'NONE',  ( 0.000000000000000000, 0.000000000000000000, -1.000000000000000000 ) ) ;
#48371 = CARTESIAN_POINT ( 'NONE',  ( 11.75000000000000000, -5.000000000000000000, -23.89194109070750471 ) ) ;
#48372 = ORIENTED_EDGE ( 'NONE', *, *, #28113, .F. ) ;
#48373 = ORIENTED_EDGE ( 'NONE', *, *, #4546, .F. ) ;
#48374 = DIRECTION ( 'NONE',  ( 1.000000000000000000, 0.000000000000000000, 0.000000000000000000 ) ) ;
#48375 = ORIENTED_EDGE ( 'NONE', *, *, #32693, .T. ) ;
#48376 = ADVANCED_FACE ( 'NONE', ( #65537 ), #58849, .F. ) ;
#48377 = CARTESIAN_POINT ( 'NONE',  ( -14.45313394609757118, -0.2715358723599894386, -23.33896727494798284 ) ) ;
#48378 = DIRECTION ( 'NONE',  ( -0.8660254037844363761, 0.5000000000000038858, -0.000000000000000000 ) ) ;
#48379 = ORIENTED_EDGE ( 'NONE', *, *, #2853, .T. ) ;
#48380 = EDGE_CURVE ( 'NONE', #39081, #16092, #45105, .T. ) ;
#48381 = CARTESIAN_POINT ( 'NONE',  ( 2.906483450353349429, -10.09643294401463365, 455.0000000000000568 ) ) ;
#48382 = CARTESIAN_POINT ( 'NONE',  ( -13.00000000000000178, -15.50000000000000000, 14.50000000000000000 ) ) ;
#48384 = ORIENTED_EDGE ( 'NONE', *, *, #3178, .T. ) ;
#48383 = CARTESIAN_POINT ( 'NONE',  ( 39.90000000000000568, -21.00000000000000000, 13.86939075806900057 ) ) ;
#48385 = ORIENTED_EDGE ( 'NONE', *, *, #69730, .F. ) ;
#48386 = EDGE_CURVE ( 'NONE', #14923, #49745, #32324, .T. ) ;
#48387 = LINE ( 'NONE', #26132, #33159 ) ;
#48388 = PLANE ( 'NONE',  #61222 ) ;
#48389 = EDGE_CURVE ( 'NONE', #16263, #52016, #22520, .T. ) ;
#48390 = DIRECTION ( 'NONE',  ( 0.000000000000000000, 0.000000000000000000, -1.000000000000000000 ) ) ;
#48391 = CARTESIAN_POINT ( 'NONE',  ( 13.00000000000000178, -15.50000000000000000, 20.05051025721700242 ) ) ;
#48392 = ADVANCED_FACE ( 'NONE', ( #37284 ), #49289, .F. ) ;
#48393 = CARTESIAN_POINT ( 'NONE',  ( -11.00000000000000000, -11.85423089348099879, 9.852125413066602277 ) ) ;
#48394 = EDGE_LOOP ( 'NONE', ( #1463, #42427, #27736, #45590 ) ) ;
#48395 = DIRECTION ( 'NONE',  ( 0.000000000000000000, 0.000000000000000000, 1.000000000000000000 ) ) ;
#48396 = CARTESIAN_POINT ( 'NONE',  ( 11.32648345035337734, -4.206483450353492692, 455.0000000000000568 ) ) ;
#48397 = DIRECTION ( 'NONE',  ( -0.8660254037844375974, 0.5000000000000019984, 1.836970198721037330E-16 ) ) ;
#48398 = AXIS2_PLACEMENT_3D ( 'NONE', #60748, #28568, #50140 ) ;
#48400 = ORIENTED_EDGE ( 'NONE', *, *, #11302, .F. ) ;
#48399 = FACE_OUTER_BOUND ( 'NONE', #67168, .T. ) ;
#48401 = DIRECTION ( 'NONE',  ( 0.000000000000000000, -0.7071067811865480168, -0.7071067811865470176 ) ) ;
#48402 = CARTESIAN_POINT ( 'NONE',  ( 0.000000000000000000, -7.449999999999998401, -9.000000000000001776 ) ) ;
#48403 = EDGE_CURVE ( 'NONE', #53316, #19917, #18, .T. ) ;
#48404 = DIRECTION ( 'NONE',  ( -1.000000000000000000, 0.000000000000000000, 0.000000000000000000 ) ) ;
#48405 = EDGE_CURVE ( 'NONE', #27698, #41049, #37634, .T. ) ;
#48406 = CIRCLE ( 'NONE', #31508, 0.5249999999999994671 ) ;
#48407 = CARTESIAN_POINT ( 'NONE',  ( -8.249999999999996447, -7.848062532927998269, 5.000000000000000000 ) ) ;
#48408 = ORIENTED_EDGE ( 'NONE', *, *, #63559, .F. ) ;
#48409 = CARTESIAN_POINT ( 'NONE',  ( 283.0000000000000568, -30.80000000000000071, -8.900000000000000355 ) ) ;
#48410 = CARTESIAN_POINT ( 'NONE',  ( -8.000000000000000000, -6.879816696376141572, -1.000000000000000000 ) ) ;
#48411 = VERTEX_POINT ( 'NONE', #53900 ) ;
#48412 = DIRECTION ( 'NONE',  ( 1.836970198721029934E-16, 1.836970198721010706E-16, -1.000000000000000000 ) ) ;
#48413 = ADVANCED_FACE ( 'NONE', ( #27019 ), #38666, .T. ) ;
#48414 = EDGE_CURVE ( 'NONE', #705, #57915, #10406, .T. ) ;
#48415 = CARTESIAN_POINT ( 'NONE',  ( 4.046023737882819660, -3.157023737882826087, 54.00000000000000711 ) ) ;
#48416 = CARTESIAN_POINT ( 'NONE',  ( 31.89999999999999858, 13.66939075806899240, 20.79999999999999361 ) ) ;
#48417 = DIRECTION ( 'NONE',  ( 0.000000000000000000, 1.000000000000000000, 0.000000000000000000 ) ) ;
#48418 = ADVANCED_FACE ( 'NONE', ( #10745 ), #21712, .T. ) ;
#48419 = VECTOR ( 'NONE', #17424, 1000.000000000000000 ) ;
#48420 = PLANE ( 'NONE',  #63667 ) ;
#48421 = ORIENTED_EDGE ( 'NONE', *, *, #51806, .F. ) ;
#48422 = ORIENTED_EDGE ( 'NONE', *, *, #11138, .T. ) ;
#48423 = DIRECTION ( 'NONE',  ( 1.000000000000000000, 0.000000000000000000, 0.000000000000000000 ) ) ;
#48424 = EDGE_LOOP ( 'NONE', ( #12083, #6396, #17218, #13794, #45454, #51610, #61187, #54545, #61945, #12486, #58810 ) ) ;
#48425 = ORIENTED_EDGE ( 'NONE', *, *, #34410, .F. ) ;
#48426 = DIRECTION ( 'NONE',  ( -0.000000000000000000, -0.000000000000000000, -1.000000000000000000 ) ) ;
#48427 = CARTESIAN_POINT ( 'NONE',  ( 3.677663764522620227, 4.135079735113113664, 54.00000000000000711 ) ) ;
#48428 = LINE ( 'NONE', #59034, #31023 ) ;
#48429 = EDGE_LOOP ( 'NONE', ( #13799, #16310, #49092, #57108 ) ) ;
#48430 = ORIENTED_EDGE ( 'NONE', *, *, #38115, .F. ) ;
#48432 = ADVANCED_FACE ( 'NONE', ( #21363 ), #11435, .F. ) ;
#48431 = DIRECTION ( 'NONE',  ( 1.836970198721029934E-16, 1.836970198721010706E-16, -1.000000000000000000 ) ) ;
#48433 = ORIENTED_EDGE ( 'NONE', *, *, #60813, .F. ) ;
#48434 = ORIENTED_EDGE ( 'NONE', *, *, #50444, .F. ) ;
#48435 = EDGE_CURVE ( 'NONE', #54028, #12647, #32666, .T. ) ;
#48436 = CARTESIAN_POINT ( 'NONE',  ( -7.250000000000001776, -7.249999999999998224, -8.000000000000000000 ) ) ;
#48437 = CARTESIAN_POINT ( 'NONE',  ( 5.668387132715968058, 8.393516549646582448, 455.0000000000000568 ) ) ;
#48438 = DIRECTION ( 'NONE',  ( 0.000000000000000000, -1.000000000000000000, 0.000000000000000000 ) ) ;
#48439 = ORIENTED_EDGE ( 'NONE', *, *, #50681, .F. ) ;
#48440 = DIRECTION ( 'NONE',  ( 0.000000000000000000, 1.000000000000000000, 0.000000000000000000 ) ) ;
#48442 = CARTESIAN_POINT ( 'NONE',  ( 4.149127210878736705, 3.663616288757004291, 26.00000000000000711 ) ) ;
#48441 = CARTESIAN_POINT ( 'NONE',  ( 41.09999999999999432, -21.00000000000000000, -13.86939075806900057 ) ) ;
#48443 = VERTEX_POINT ( 'NONE', #48935 ) ;
#48444 = ORIENTED_EDGE ( 'NONE', *, *, #23078, .T. ) ;
#48446 = ORIENTED_EDGE ( 'NONE', *, *, #8588, .F. ) ;
#48445 = LINE ( 'NONE', #54790, #30825 ) ;
#48447 = ORIENTED_EDGE ( 'NONE', *, *, #1530, .F. ) ;
#48448 = AXIS2_PLACEMENT_3D ( 'NONE', #37319, #32699, #10774 ) ;
#48449 = CARTESIAN_POINT ( 'NONE',  ( 0.000000000000000000, -8.249999999999998224, -21.00000000000000000 ) ) ;
#48450 = AXIS2_PLACEMENT_3D ( 'NONE', #61894, #13098, #67195 ) ;
#48451 = CARTESIAN_POINT ( 'NONE',  ( -6.344366288193416636, -4.720772854004745334, 26.00000000000000711 ) ) ;
#48452 = ORIENTED_EDGE ( 'NONE', *, *, #46744, .F. ) ;
#48453 = AXIS2_PLACEMENT_3D ( 'NONE', #7137, #38647, #55253 ) ;
#48454 = DIRECTION ( 'NONE',  ( 0.8660254037844435926, 0.4999999999999913958, 2.509347957447859069E-16 ) ) ;
#48455 = FACE_OUTER_BOUND ( 'NONE', #56975, .T. ) ;
#48456 = EDGE_LOOP ( 'NONE', ( #11984, #55639, #17696, #1541 ) ) ;
#48457 = ORIENTED_EDGE ( 'NONE', *, *, #2507, .T. ) ;
#48458 = VECTOR ( 'NONE', #32595, 1000.000000000000000 ) ;
#48459 = CARTESIAN_POINT ( 'NONE',  ( 28.00000000000000000, -15.50000000000000000, 20.05051025721700242 ) ) ;
#48460 = PLANE ( 'NONE',  #57185 ) ;
#48461 = DIRECTION ( 'NONE',  ( 0.000000000000000000, 0.000000000000000000, -1.000000000000000000 ) ) ;
#48462 = ORIENTED_EDGE ( 'NONE', *, *, #59332, .F. ) ;
#48464 = AXIS2_PLACEMENT_3D ( 'NONE', #8344, #7993, #40173 ) ;
#48463 = VECTOR ( 'NONE', #57866, 1000.000000000000000 ) ;
#48465 = EDGE_CURVE ( 'NONE', #7047, #7104, #68903, .T. ) ;
#48466 = CARTESIAN_POINT ( 'NONE',  ( -8.916576262117258622, 10.03972626211718477, 26.00000000000000711 ) ) ;
#48467 = CARTESIAN_POINT ( 'NONE',  ( -7.250000000000000888, 7.450000000000003730, -9.500000000000001776 ) ) ;
#48469 = ORIENTED_EDGE ( 'NONE', *, *, #9942, .T. ) ;
#48468 = CARTESIAN_POINT ( 'NONE',  ( 0.000000000000000000, 0.000000000000000000, -29.90000000000000924 ) ) ;
#48471 = EDGE_LOOP ( 'NONE', ( #33558, #41840, #41096, #9159 ) ) ;
#48470 = DIRECTION ( 'NONE',  ( 0.000000000000000000, 0.000000000000000000, -1.000000000000000000 ) ) ;
#48472 = EDGE_CURVE ( 'NONE', #69700, #15393, #66228, .T. ) ;
#48473 = LINE ( 'NONE', #4646, #22642 ) ;
#48474 = AXIS2_PLACEMENT_3D ( 'NONE', #67603, #40005, #29753 ) ;
#48475 = DIRECTION ( 'NONE',  ( 0.000000000000000000, 0.7071067811865474617, -0.7071067811865474617 ) ) ;
#48476 = EDGE_CURVE ( 'NONE', #27121, #7467, #58718, .T. ) ;
#48477 = DIRECTION ( 'NONE',  ( 0.000000000000000000, 1.000000000000000000, 0.000000000000000000 ) ) ;
#48478 = EDGE_CURVE ( 'NONE', #4626, #11704, #34953, .T. ) ;
#48479 = DIRECTION ( 'NONE',  ( 1.000000000000000000, -0.000000000000000000, 0.000000000000000000 ) ) ;
#48480 = LINE ( 'NONE', #37526, #52003 ) ;
#48481 = EDGE_CURVE ( 'NONE', #33646, #64293, #39347, .T. ) ;
#48482 = EDGE_CURVE ( 'NONE', #67437, #3267, #3383, .T. ) ;
#48483 = FACE_OUTER_BOUND ( 'NONE', #6135, .T. ) ;
#48484 = ORIENTED_EDGE ( 'NONE', *, *, #31491, .T. ) ;
#48485 = CARTESIAN_POINT ( 'NONE',  ( 9.804883450353379715, -10.20488345035352928, 455.0000000000000568 ) ) ;
#48487 = VERTEX_POINT ( 'NONE', #17430 ) ;
#48486 = CARTESIAN_POINT ( 'NONE',  ( -8.250000000000001776, 0.000000000000000000, -14.00000000000000000 ) ) ;
#48489 = ORIENTED_EDGE ( 'NONE', *, *, #10872, .F. ) ;
#48488 = CARTESIAN_POINT ( 'NONE',  ( -5.655420232009250370, 8.393516549646600211, 455.0000000000000568 ) ) ;
#48490 = CARTESIAN_POINT ( 'NONE',  ( 39.00000000000000000, -0.2000000000000000111, 0.000000000000000000 ) ) ;
#48491 = DIRECTION ( 'NONE',  ( -0.000000000000000000, -0.000000000000000000, -1.000000000000000000 ) ) ;
#48492 = EDGE_LOOP ( 'NONE', ( #8243, #62685, #37810, #5496 ) ) ;
#48493 = CARTESIAN_POINT ( 'NONE',  ( 30.00000000000000000, -8.959999999999999076, -12.95475478405700009 ) ) ;
#48494 = CARTESIAN_POINT ( 'NONE',  ( -25.49999999999869971, -15.50000000000000000, 22.50000000000000000 ) ) ;
#48495 = ORIENTED_EDGE ( 'NONE', *, *, #60380, .T. ) ;
#48496 = AXIS2_PLACEMENT_3D ( 'NONE', #762, #22331, #11684 ) ;
#48497 = FACE_OUTER_BOUND ( 'NONE', #67034, .T. ) ;
#48498 = LINE ( 'NONE', #28302, #56351 ) ;
#48499 = LINE ( 'NONE', #11019, #13332 ) ;
#48500 = VECTOR ( 'NONE', #47632, 1000.000000000000000 ) ;
#48501 = CIRCLE ( 'NONE', #17987, 0.2000000000000005107 ) ;
#48502 = VERTEX_POINT ( 'NONE', #60906 ) ;
#48503 = DIRECTION ( 'NONE',  ( 0.000000000000000000, 0.000000000000000000, 1.000000000000000000 ) ) ;
#48504 = ORIENTED_EDGE ( 'NONE', *, *, #17534, .F. ) ;
#48505 = VERTEX_POINT ( 'NONE', #34367 ) ;
#48506 = VECTOR ( 'NONE', #37874, 1000.000000000000000 ) ;
#48507 = FACE_BOUND ( 'NONE', #59909, .T. ) ;
#48508 = CARTESIAN_POINT ( 'NONE',  ( 15.50000000000000000, -0.4000000000005274892, 19.20000000000052864 ) ) ;
#48509 = AXIS2_PLACEMENT_3D ( 'NONE', #36216, #63098, #53209 ) ;
#48510 = CARTESIAN_POINT ( 'NONE',  ( 30.00000000000000000, -11.70000000000012008, 10.70000000000011831 ) ) ;
#48511 = CARTESIAN_POINT ( 'NONE',  ( 24.00000000000000000, -16.64230188589299786, 14.64519951917100116 ) ) ;
#48512 = VERTEX_POINT ( 'NONE', #2915 ) ;
#48513 = VERTEX_POINT ( 'NONE', #45335 ) ;
#48515 = ORIENTED_EDGE ( 'NONE', *, *, #5633, .F. ) ;
#48514 = DIRECTION ( 'NONE',  ( -0.000000000000000000, -0.000000000000000000, -1.000000000000000000 ) ) ;
#48516 = VERTEX_POINT ( 'NONE', #23783 ) ;
#48517 = EDGE_CURVE ( 'NONE', #56963, #28943, #20343, .T. ) ;
#48518 = DIRECTION ( 'NONE',  ( -1.000000000000000000, 0.000000000000000000, 0.000000000000000000 ) ) ;
#48519 = DIRECTION ( 'NONE',  ( -1.000000000000000000, 0.000000000000000000, 0.000000000000000000 ) ) ;
#48520 = DIRECTION ( 'NONE',  ( 1.047444401652940007E-14, 1.000000000000000000, 1.836970198721029934E-16 ) ) ;
#48521 = EDGE_CURVE ( 'NONE', #67310, #32707, #12464, .T. ) ;
#48522 = CARTESIAN_POINT ( 'NONE',  ( -7.342976262117259623, 6.651770455163663165, 54.00000000000000711 ) ) ;
#48523 = AXIS2_PLACEMENT_3D ( 'NONE', #28112, #34429, #66628 ) ;
#48525 = CYLINDRICAL_SURFACE ( 'NONE', #9755, 0.1999999999999987899 ) ;
#48524 = LINE ( 'NONE', #59826, #30960 ) ;
#48526 = EDGE_LOOP ( 'NONE', ( #68007, #20208, #14436, #33223 ) ) ;
#48528 = ORIENTED_EDGE ( 'NONE', *, *, #28420, .T. ) ;
#48527 = CARTESIAN_POINT ( 'NONE',  ( -7.813516549646711162, 11.99351654964660341, 455.0000000000000568 ) ) ;
#48529 = ORIENTED_EDGE ( 'NONE', *, *, #16331, .T. ) ;
#48530 = ORIENTED_EDGE ( 'NONE', *, *, #36911, .T. ) ;
#48531 = LINE ( 'NONE', #32961, #12996 ) ;
#48532 = CARTESIAN_POINT ( 'NONE',  ( 8.835729544836338434, -7.969523737882825642, 54.00000000000000711 ) ) ;
#48533 = SHAPE_REPRESENTATION_RELATIONSHIP ( 'NONE' , 'NONE' ,  #33595, #19156 ) ;
#48534 = LINE ( 'NONE', #36893, #11642 ) ;
#48535 = VECTOR ( 'NONE', #68629, 1000.000000000000000 ) ;
#48536 = ORIENTED_EDGE ( 'NONE', *, *, #32836, .F. ) ;
#48537 = ORIENTED_EDGE ( 'NONE', *, *, #50020, .T. ) ;
#48538 = ORIENTED_EDGE ( 'NONE', *, *, #37157, .T. ) ;
#48539 = CARTESIAN_POINT ( 'NONE',  ( 4.720772854004775532, -4.155633711806681063, 54.00000000000000711 ) ) ;
#48540 = DIRECTION ( 'NONE',  ( 0.000000000000000000, 0.000000000000000000, 1.000000000000000000 ) ) ;
#48541 = LINE ( 'NONE', #21675, #30012 ) ;
#48542 = VERTEX_POINT ( 'NONE', #35076 ) ;
#48543 = VERTEX_POINT ( 'NONE', #61957 ) ;
#48544 = DIRECTION ( 'NONE',  ( 0.000000000000000000, 0.000000000000000000, -1.000000000000000000 ) ) ;
#48545 = DIRECTION ( 'NONE',  ( -1.000000000000000000, 0.000000000000000000, 0.000000000000000000 ) ) ;
#48546 = AXIS2_PLACEMENT_3D ( 'NONE', #12483, #50324, #18141 ) ;
#48547 = ORIENTED_EDGE ( 'NONE', *, *, #23866, .T. ) ;
#48548 = AXIS2_PLACEMENT_3D ( 'NONE', #35623, #12652, #45891 ) ;
#48549 = EDGE_CURVE ( 'NONE', #7124, #18304, #28386, .T. ) ;
#48550 = AXIS2_PLACEMENT_3D ( 'NONE', #66394, #39175, #12625 ) ;
#48551 = CARTESIAN_POINT ( 'NONE',  ( 283.0000000000000568, -21.00000000000000000, 17.50000000000000000 ) ) ;
#48553 = EDGE_LOOP ( 'NONE', ( #42843, #49600, #59722, #57050 ) ) ;
#48552 = CARTESIAN_POINT ( 'NONE',  ( 25.57999999999999829, 3.010794155703768650E-16, -2.458500000000000796 ) ) ;
#48554 = VERTEX_POINT ( 'NONE', #18828 ) ;
#48555 = VECTOR ( 'NONE', #42040, 1000.000000000000000 ) ;
#48556 = LINE ( 'NONE', #51851, #28117 ) ;
#48557 = CARTESIAN_POINT ( 'NONE',  ( 15.50000000000000000, -2.500000000000000000, 23.94337567297399971 ) ) ;
#48558 = EDGE_CURVE ( 'NONE', #40825, #28070, #28731, .T. ) ;
#48559 = DIRECTION ( 'NONE',  ( 0.000000000000000000, 1.000000000000000000, -0.000000000000000000 ) ) ;
#48560 = EDGE_CURVE ( 'NONE', #6981, #22970, #44994, .T. ) ;
#48561 = EDGE_CURVE ( 'NONE', #20561, #29125, #50307, .T. ) ;
#48562 = DIRECTION ( 'NONE',  ( -0.8660254037844363761, 0.5000000000000038858, -0.000000000000000000 ) ) ;
#48563 = VECTOR ( 'NONE', #35503, 1000.000000000000000 ) ;
#48564 = LINE ( 'NONE', #64830, #23718 ) ;
#48565 = EDGE_CURVE ( 'NONE', #9839, #15117, #55327, .T. ) ;
#48566 = ADVANCED_FACE ( 'NONE', ( #45687 ), #66907, .T. ) ;
#48567 = VECTOR ( 'NONE', #67664, 1000.000000000000000 ) ;
#48568 = ORIENTED_EDGE ( 'NONE', *, *, #54995, .T. ) ;
#48569 = FACE_BOUND ( 'NONE', #267, .T. ) ;
#48570 = AXIS2_PLACEMENT_3D ( 'NONE', #39002, #44639, #33693 ) ;
#48571 = ORIENTED_EDGE ( 'NONE', *, *, #42969, .T. ) ;
#48572 = CARTESIAN_POINT ( 'NONE',  ( 8.250000000000005329, 7.250000000000000888, -24.00000000000000000 ) ) ;
#48573 = CARTESIAN_POINT ( 'NONE',  ( 9.900000000000000355, 0.000000000000000000, 2.154935995002245639E-16 ) ) ;
#48574 = ADVANCED_FACE ( 'NONE', ( #55960, #40023 ), #40395, .T. ) ;
#48575 = CARTESIAN_POINT ( 'NONE',  ( -8.250000000000001776, 7.250000000000000888, -17.50000000000000000 ) ) ;
#48576 = DIRECTION ( 'NONE',  ( 9.912705577010386883E-15, 1.000000000000000000, 0.000000000000000000 ) ) ;
#48577 = VECTOR ( 'NONE', #1167, 1000.000000000000000 ) ;
#48578 = AXIS2_PLACEMENT_3D ( 'NONE', #61732, #46166, #7975 ) ;
#48579 = DIRECTION ( 'NONE',  ( 1.034072152899299800E-14, 1.000000000000000000, 0.000000000000000000 ) ) ;
#48580 = ORIENTED_EDGE ( 'NONE', *, *, #22713, .T. ) ;
#48581 = DIRECTION ( 'NONE',  ( 1.000000000000000000, 0.000000000000000000, 0.000000000000000000 ) ) ;
#48582 = FACE_OUTER_BOUND ( 'NONE', #44106, .T. ) ;
#48583 = ORIENTED_EDGE ( 'NONE', *, *, #47521, .T. ) ;
#48584 = CIRCLE ( 'NONE', #24855, 0.1750000000000002387 ) ;
#48585 = CARTESIAN_POINT ( 'NONE',  ( 11.50000000000000000, -11.50000000000100009, 15.00000000000084910 ) ) ;
#48586 = CARTESIAN_POINT ( 'NONE',  ( 283.0000000000000568, -38.65000000000095781, 13.20000000000094253 ) ) ;
#48587 = VERTEX_POINT ( 'NONE', #61595 ) ;
#48588 = FACE_OUTER_BOUND ( 'NONE', #16224, .T. ) ;
#48589 = CARTESIAN_POINT ( 'NONE',  ( -7.250000000000000888, 7.450000000000003730, -14.50000000000000000 ) ) ;
#48590 = VERTEX_POINT ( 'NONE', #29088 ) ;
#48591 = LINE ( 'NONE', #160, #32191 ) ;
#48592 = CARTESIAN_POINT ( 'NONE',  ( 25.50000000000000355, -5.578999999999999737, 24.12099999999999511 ) ) ;
#48593 = CARTESIAN_POINT ( 'NONE',  ( -23.48000000000000043, -15.50000000000000000, 26.00000000000000355 ) ) ;
#48594 = CARTESIAN_POINT ( 'NONE',  ( 6.006483450353401921, 5.993516549646582092, 455.0000000000000568 ) ) ;
#48595 = VERTEX_POINT ( 'NONE', #8206 ) ;
#48596 = AXIS2_PLACEMENT_3D ( 'NONE', #33996, #33663, #40355 ) ;
#48598 = VERTEX_POINT ( 'NONE', #50651 ) ;
#48597 = PLANE ( 'NONE',  #5771 ) ;
#48599 = VECTOR ( 'NONE', #29170, 1000.000000000000000 ) ;
#48600 = DIRECTION ( 'NONE',  ( 1.000000000000000000, -1.356437060717831815E-15, -1.836970198721032646E-16 ) ) ;
#48601 = DIRECTION ( 'NONE',  ( -0.4999999999999785727, 0.8660254037844510311, 3.181725716174766844E-16 ) ) ;
#48602 = LINE ( 'NONE', #16081, #12684 ) ;
#48603 = VERTEX_POINT ( 'NONE', #67272 ) ;
#48604 = EDGE_CURVE ( 'NONE', #9143, #67986, #47445, .T. ) ;
#48605 = AXIS2_PLACEMENT_3D ( 'NONE', #55352, #12196, #11501 ) ;
#48606 = EDGE_CURVE ( 'NONE', #45353, #65774, #63371, .T. ) ;
#48607 = EDGE_CURVE ( 'NONE', #49327, #40754, #16913, .T. ) ;
#48608 =( NAMED_UNIT ( * ) PLANE_ANGLE_UNIT ( ) SI_UNIT ( $, .RADIAN. ) );
#48609 = DIRECTION ( 'NONE',  ( 0.000000000000000000, 1.000000000000000000, 0.000000000000000000 ) ) ;
#48610 = ORIENTED_EDGE ( 'NONE', *, *, #8979, .F. ) ;
#48611 = EDGE_LOOP ( 'NONE', ( #50833, #38181, #16942, #26172, #21678, #20821, #51080, #58539 ) ) ;
#48612 = ADVANCED_FACE ( 'NONE', ( #63727 ), #19520, .F. ) ;
#48613 = VECTOR ( 'NONE', #11264, 1000.000000000000000 ) ;
#48614 = ORIENTED_EDGE ( 'NONE', *, *, #49144, .F. ) ;
#48615 = VECTOR ( 'NONE', #36533, 1000.000000000000000 ) ;
#48616 = CARTESIAN_POINT ( 'NONE',  ( -4.173516549646839380, -12.00648345035344811, 455.0000000000000568 ) ) ;
#48617 = DIRECTION ( 'NONE',  ( 0.000000000000000000, 0.000000000000000000, -1.000000000000000000 ) ) ;
#48618 = ORIENTED_EDGE ( 'NONE', *, *, #33765, .T. ) ;
#48619 = ORIENTED_EDGE ( 'NONE', *, *, #45746, .T. ) ;
#48621 = FACE_OUTER_BOUND ( 'NONE', #18263, .T. ) ;
#48620 = AXIS2_PLACEMENT_3D ( 'NONE', #60459, #33253, #743 ) ;
#48622 = VECTOR ( 'NONE', #61280, 1000.000000000000000 ) ;
#48623 = ORIENTED_EDGE ( 'NONE', *, *, #28891, .T. ) ;
#48624 = VERTEX_POINT ( 'NONE', #20576 ) ;
#48625 = EDGE_LOOP ( 'NONE', ( #30817, #3974, #56191, #55455 ) ) ;
#48626 = VERTEX_POINT ( 'NONE', #35426 ) ;
#48627 = DIRECTION ( 'NONE',  ( 0.000000000000000000, 0.000000000000000000, -1.000000000000000000 ) ) ;
#48628 = UNCERTAINTY_MEASURE_WITH_UNIT (LENGTH_MEASURE( 1.000000000000000082E-05 ), #184, 'distance_accuracy_value', 'NONE');
#48630 = ORIENTED_EDGE ( 'NONE', *, *, #44942, .T. ) ;
#48629 = DIRECTION ( 'NONE',  ( 0.000000000000000000, 0.000000000000000000, -1.000000000000000000 ) ) ;
#48631 = LINE ( 'NONE', #540, #17607 ) ;
#48632 = DIRECTION ( 'NONE',  ( -0.7071067811865470176, 0.7071067811865480168, 0.000000000000000000 ) ) ;
#48633 = CIRCLE ( 'NONE', #67801, 0.5999999999999989786 ) ;
#48634 = CARTESIAN_POINT ( 'NONE',  ( -22.14589803375000088, -15.50000000000000000, 21.50000000000000000 ) ) ;
#48635 = EDGE_LOOP ( 'NONE', ( #69512, #61858, #69251, #52615 ) ) ;
#48636 = CARTESIAN_POINT ( 'NONE',  ( 4.456444791733522252E-16, 7.450000000000002842, -11.50000000000000000 ) ) ;
#48637 = VECTOR ( 'NONE', #15614, 1000.000000000000000 ) ;
#48638 = LINE ( 'NONE', #209, #58659 ) ;
#48639 = AXIS2_PLACEMENT_3D ( 'NONE', #1931, #23497, #44696 ) ;
#48640 = VERTEX_POINT ( 'NONE', #47110 ) ;
#48641 = CARTESIAN_POINT ( 'NONE',  ( -11.75000000000000000, -5.200000000000001066, -11.75000000000000000 ) ) ;
#48642 = EDGE_CURVE ( 'NONE', #11897, #30360, #12392, .T. ) ;
#48643 = AXIS2_PLACEMENT_3D ( 'NONE', #68287, #67590, #45650 ) ;
#48644 = CARTESIAN_POINT ( 'NONE',  ( 3.682023737882785586, -9.912023737882808661, 54.00000000000000711 ) ) ;
#48645 = DIRECTION ( 'NONE',  ( 0.7671651518153105309, 0.6414496315691445849, 2.356647714346206145E-16 ) ) ;
#48646 = EDGE_CURVE ( 'NONE', #56856, #5501, #35788, .T. ) ;
#48647 = EDGE_CURVE ( 'NONE', #52778, #27455, #19874, .T. ) ;
#48648 = ORIENTED_EDGE ( 'NONE', *, *, #51593, .F. ) ;
#48650 = FACE_OUTER_BOUND ( 'NONE', #33544, .T. ) ;
#48649 = VECTOR ( 'NONE', #60816, 1000.000000000000000 ) ;
#48651 = PLANE ( 'NONE',  #13849 ) ;
#48652 = ADVANCED_FACE ( 'NONE', ( #8911 ), #52058, .T. ) ;
#48653 = CYLINDRICAL_SURFACE ( 'NONE', #2013, 4.000000000000000000 ) ;
#48654 = PRODUCT_RELATED_PRODUCT_CATEGORY ( 'part', '', ( #44806 ) ) ;
#48655 = VECTOR ( 'NONE', #31993, 1000.000000000000000 ) ;
#48656 = AXIS2_PLACEMENT_3D ( 'NONE', #1708, #17278, #38842 ) ;
#48657 = DIRECTION ( 'NONE',  ( -0.000000000000000000, 3.673940397442059868E-16, -1.000000000000000000 ) ) ;
#48658 = EDGE_CURVE ( 'NONE', #12490, #69842, #24836, .T. ) ;
#48659 = FACE_BOUND ( 'NONE', #6234, .T. ) ;
#48660 = PLANE ( 'NONE',  #36172 ) ;
#48662 = EDGE_CURVE ( 'NONE', #44153, #41828, #68318, .T. ) ;
#48661 = DIRECTION ( 'NONE',  ( -0.000000000000000000, 0.000000000000000000, 1.000000000000000000 ) ) ;
#48663 = VECTOR ( 'NONE', #58529, 1000.000000000000000 ) ;
#48664 = DIRECTION ( 'NONE',  ( 0.000000000000000000, 1.000000000000000000, 0.000000000000000000 ) ) ;
#48665 = EDGE_LOOP ( 'NONE', ( #13734, #2668, #42253, #45527 ) ) ;
#48666 = DIRECTION ( 'NONE',  ( -0.000000000000000000, 0.000000000000000000, 1.000000000000000000 ) ) ;
#48667 = DIRECTION ( 'NONE',  ( 0.000000000000000000, 0.000000000000000000, -1.000000000000000000 ) ) ;
#48668 = AXIS2_PLACEMENT_3D ( 'NONE', #43779, #1663, #23236 ) ;
#48669 = DIRECTION ( 'NONE',  ( -1.000000000000000000, 0.000000000000000000, 0.000000000000000000 ) ) ;
#48670 = EDGE_LOOP ( 'NONE', ( #30465, #746, #18066, #25007 ) ) ;
#48671 = CARTESIAN_POINT ( 'NONE',  ( -2.693516549646772340, -10.09643294401458036, 195.0000000000000284 ) ) ;
#48672 = DIRECTION ( 'NONE',  ( 9.912705577010336396E-15, 1.000000000000000000, 0.000000000000000000 ) ) ;
#48673 = DIRECTION ( 'NONE',  ( 1.836970198721029934E-16, 1.836970198721010706E-16, -1.000000000000000000 ) ) ;
#48674 = DIRECTION ( 'NONE',  ( 0.000000000000000000, 0.000000000000000000, 1.000000000000000000 ) ) ;
#48675 = FACE_BOUND ( 'NONE', #21062, .T. ) ;
#48676 = DIRECTION ( 'NONE',  ( 1.000000000000000000, -3.016910393003147986E-15, 0.000000000000000000 ) ) ;
#48677 = ORIENTED_EDGE ( 'NONE', *, *, #28920, .T. ) ;
#48678 = VERTEX_POINT ( 'NONE', #9628 ) ;
#48679 = CARTESIAN_POINT ( 'NONE',  ( 11.00000000000000000, -11.50000000000100009, -15.00000000000084910 ) ) ;
#48680 = VECTOR ( 'NONE', #53682, 1000.000000000000000 ) ;
#48681 = DIRECTION ( 'NONE',  ( 1.836970198721029934E-16, 1.836970198721010706E-16, -1.000000000000000000 ) ) ;
#48682 = VERTEX_POINT ( 'NONE', #56997 ) ;
#48683 = DIRECTION ( 'NONE',  ( -0.000000000000000000, -0.000000000000000000, -1.000000000000000000 ) ) ;
#48684 = CARTESIAN_POINT ( 'NONE',  ( -8.130476262117259267, 9.547976262117177981, 54.00000000000000711 ) ) ;
#48685 = VERTEX_POINT ( 'NONE', #31553 ) ;
#48686 = EDGE_CURVE ( 'NONE', #5255, #12276, #41087, .T. ) ;
#48687 = CYLINDRICAL_SURFACE ( 'NONE', #36811, 3.499999999999038547 ) ;
#48688 = EDGE_LOOP ( 'NONE', ( #63426, #46003, #23028, #42188 ) ) ;
#48689 = ORIENTED_EDGE ( 'NONE', *, *, #35353, .T. ) ;
#48690 = FACE_OUTER_BOUND ( 'NONE', #68329, .T. ) ;
#48691 = VECTOR ( 'NONE', #42558, 1000.000000000000000 ) ;
#48692 = VERTEX_POINT ( 'NONE', #62303 ) ;
#48693 = PLANE ( 'NONE',  #47842 ) ;
#48694 = CYLINDRICAL_SURFACE ( 'NONE', #50788, 3.499999999999038547 ) ;
#48695 = DIRECTION ( 'NONE',  ( 1.000000000000000000, -7.457533623526253657E-15, 1.836970198721016375E-16 ) ) ;
#48696 = CIRCLE ( 'NONE', #39633, 0.2000000000000005107 ) ;
#48697 = ORIENTED_EDGE ( 'NONE', *, *, #9660, .F. ) ;
#48698 = ORIENTED_EDGE ( 'NONE', *, *, #69046, .F. ) ;
#48699 = VECTOR ( 'NONE', #12972, 999.9999999999998863 ) ;
#48700 = CARTESIAN_POINT ( 'NONE',  ( 11.00000000000000000, -14.04000000000000092, -14.80000000000000071 ) ) ;
#48702 = DIRECTION ( 'NONE',  ( 0.000000000000000000, 1.000000000000000000, 0.000000000000000000 ) ) ;
#48701 = CARTESIAN_POINT ( 'NONE',  ( 8.250000000000005329, -7.249999999999998224, -26.00000000000001066 ) ) ;
#48703 = EDGE_CURVE ( 'NONE', #3786, #7925, #46272, .T. ) ;
#48704 = ORIENTED_EDGE ( 'NONE', *, *, #22139, .T. ) ;
#48705 = EDGE_LOOP ( 'NONE', ( #24712, #68681, #15286, #15297, #59000, #9009 ) ) ;
#48706 = CIRCLE ( 'NONE', #45294, 1.000000000000000000 ) ;
#48707 = AXIS2_PLACEMENT_3D ( 'NONE', #34136, #61012, #12917 ) ;
#48708 = VERTEX_POINT ( 'NONE', #46050 ) ;
#48709 = EDGE_CURVE ( 'NONE', #5314, #51178, #5671, .T. ) ;
#48710 = DIRECTION ( 'NONE',  ( -0.000000000000000000, 1.000000000000000000, -0.000000000000000000 ) ) ;
#48712 = ORIENTED_EDGE ( 'NONE', *, *, #44868, .F. ) ;
#48711 = CARTESIAN_POINT ( 'NONE',  ( 30.00000000000000000, -17.50000000000000000, -15.70500000000000007 ) ) ;
#48713 = AXIS2_PLACEMENT_3D ( 'NONE', #4353, #47462, #25913 ) ;
#48714 = CARTESIAN_POINT ( 'NONE',  ( 24.00000000000000000, -17.50000000000000000, 15.70500000000000007 ) ) ;
#48715 = LINE ( 'NONE', #9489, #31734 ) ;
#48716 = VERTEX_POINT ( 'NONE', #41446 ) ;
#48717 = ORIENTED_EDGE ( 'NONE', *, *, #10042, .T. ) ;
#48718 = AXIS2_PLACEMENT_3D ( 'NONE', #38315, #59871, #11425 ) ;
#48719 = FACE_BOUND ( 'NONE', #12871, .T. ) ;
#48720 = EDGE_CURVE ( 'NONE', #51749, #4323, #52785, .T. ) ;
#48721 = VERTEX_POINT ( 'NONE', #3973 ) ;
#48722 = CARTESIAN_POINT ( 'NONE',  ( -11.47551654964667733, 10.19191654964664018, 455.0000000000000568 ) ) ;
#48723 = CARTESIAN_POINT ( 'NONE',  ( 4.740315990920129785, -4.201500623656146516, 455.0000000000000568 ) ) ;
#48724 = VERTEX_POINT ( 'NONE', #14933 ) ;
#48725 = PLANE ( 'NONE',  #31303 ) ;
#48726 = CARTESIAN_POINT ( 'NONE',  ( 26.90000000000000213, 20.60000000000000142, -13.86939075806900057 ) ) ;
#48727 = CIRCLE ( 'NONE', #13683, 2.000000000000001776 ) ;
#48728 = EDGE_CURVE ( 'NONE', #24032, #11040, #14690, .T. ) ;
#48730 = ORIENTED_EDGE ( 'NONE', *, *, #23613, .T. ) ;
#48729 = DIRECTION ( 'NONE',  ( -1.836970198721029934E-16, 1.836970198721036590E-16, -1.000000000000000000 ) ) ;
#48731 = ORIENTED_EDGE ( 'NONE', *, *, #20427, .F. ) ;
#48732 = DIRECTION ( 'NONE',  ( 0.000000000000000000, 1.000000000000000000, 3.673940397442059868E-16 ) ) ;
#48733 = CARTESIAN_POINT ( 'NONE',  ( 7.428221114744945730, 2.993516549646613623, 195.0000000000000284 ) ) ;
#48734 = EDGE_CURVE ( 'NONE', #68045, #59557, #62064, .T. ) ;
#48735 = CARTESIAN_POINT ( 'NONE',  ( -11.50000000000000000, -11.50000000000000000, 15.00000000000000000 ) ) ;
#48736 = CARTESIAN_POINT ( 'NONE',  ( 7.000000000000000000, -42.50000000000000000, 14.50000000000000000 ) ) ;
#48737 = CARTESIAN_POINT ( 'NONE',  ( 35.89999999999999858, 20.60000000000000142, 3.016910393003143647E-15 ) ) ;
#48738 = ADVANCED_FACE ( 'NONE', ( #53127 ), #24492, .T. ) ;
#48739 = EDGE_LOOP ( 'NONE', ( #57200, #50704, #57759, #39346 ) ) ;
#48740 = CARTESIAN_POINT ( 'NONE',  ( -5.538810540050023157, 7.342976262117183239, 54.00000000000000711 ) ) ;
#48741 = DIRECTION ( 'NONE',  ( 1.000000000000000000, -1.185108578570163244E-14, 0.000000000000000000 ) ) ;
#48742 = VECTOR ( 'NONE', #15951, 1000.000000000000000 ) ;
#48744 = EDGE_CURVE ( 'NONE', #56308, #68972, #60139, .T. ) ;
#48743 = DIRECTION ( 'NONE',  ( 1.836970198721029934E-16, 1.836970198721010706E-16, -1.000000000000000000 ) ) ;
#48746 = ORIENTED_EDGE ( 'NONE', *, *, #24114, .T. ) ;
#48745 = DIRECTION ( 'NONE',  ( 0.000000000000000000, 0.000000000000000000, 1.000000000000000000 ) ) ;
#48747 = PRODUCT_DEFINITION_SHAPE ( 'NONE', 'NONE',  #69982 ) ;
#48748 = VECTOR ( 'NONE', #54129, 1000.000000000000114 ) ;
#48749 = FACE_OUTER_BOUND ( 'NONE', #65235, .T. ) ;
#48750 = CARTESIAN_POINT ( 'NONE',  ( 13.90000000000000213, -14.06939075806900874, 20.80000000000001137 ) ) ;
#48751 = CARTESIAN_POINT ( 'NONE',  ( 7.450000000000004619, -1.336933437520057563E-15, -19.50000000000000000 ) ) ;
#48752 = LINE ( 'NONE', #33521, #45528 ) ;
#48753 = EDGE_LOOP ( 'NONE', ( #22783, #43514, #43520, #19948 ) ) ;
#48754 = DIRECTION ( 'NONE',  ( -1.000000000000000000, 0.000000000000000000, 0.000000000000000000 ) ) ;
#48755 = LINE ( 'NONE', #10230, #67874 ) ;
#48756 = ORIENTED_EDGE ( 'NONE', *, *, #37321, .T. ) ;
#48757 = DIRECTION ( 'NONE',  ( 0.000000000000000000, -1.000000000000000000, 0.000000000000000000 ) ) ;
#48758 = CONICAL_SURFACE ( 'NONE', #10399, 7.799999999999999822, 1.047197551196693555 ) ;
#48759 = CLOSED_SHELL ( 'NONE', ( #33227, #16147, #59851, #65940, #19887, #22992, #14593, #20203, #15856, #61783, #65616, #62991, #24764, #19043, #50779, #12915, #41118, #66565, #7191, #26518, #12436, #30422, #18836, #63429, #27886, #28978, #64914, #7071, #67139, #56375, #40270, #22777, #17107, #34628, #66700, #34085, #9334, #20297, #16401, #30678, #63462, #65263, #69478, #60435, #22620, #22409, #37569, #20754, #32639, #59815, #45138, #45060, #2824, #40578, #43509, #26850, #44179, #63236, #9434, #12931, #51698, #13983, #8297, #62035, #66906, #39396, #3460, #69224, #15559, #31015, #6375, #60466, #10966, #55008, #14202, #48273, #33683, #8935, #43066, #9930, #35288, #53331, #44066, #62280, #39618, #26695, #42327, #38149, #31644, #3657, #12330, #31573, #40889, #21300, #35124, #22463, #53609, #24040, #19833, #32537, #15364, #34773, #15789, #28096, #56161, #29855, #22989, #62755, #15069, #57415, #60583, #41282, #55677, #1645, #33199, #51639, #32977, #67443, #60979, #46782, #39476, #29309, #41996, #56905, #37088, #460, #4699, #55714, #51547, #41048, #65578, #55461, #54768, #53150, #58846, #5477, #20977, #59897, #19645, #60974, #35840, #25931, #61723, #12592, #34861, #21436, #50542, #914, #949, #44799, #49128, #33704, #61492, #49614, #65015, #4284, #23404, #62826, #23314, #49401, #7665, #55735, #53284, #37784, #23481, #3658, #53203, #68119, #8219, #37077, #58475, #34992, #31501, #37587, #40429, #4030, #61301, #8139, #41513, #19884, #68752, #28868, #29813, #29768, #4434, #41600, #57160, #46485, #42464, #41101, #68223 ) ) ;
#48760 = CARTESIAN_POINT ( 'NONE',  ( -6.331612867284244217, -8.406483450353421816, 455.0000000000000568 ) ) ;
#48761 = LINE ( 'NONE', #38826, #41112 ) ;
#48762 = LINE ( 'NONE', #322, #59862 ) ;
#48763 = CARTESIAN_POINT ( 'NONE',  ( 4.456444791733522252E-16, 7.450000000000002842, -19.00000000000000000 ) ) ;
#48764 = EDGE_LOOP ( 'NONE', ( #50727, #55469, #33304, #6646 ) ) ;
#48765 = VERTEX_POINT ( 'NONE', #26944 ) ;
#48766 = LINE ( 'NONE', #327, #19360 ) ;
#48767 = ORIENTED_EDGE ( 'NONE', *, *, #3528, .F. ) ;
#48768 = FACE_OUTER_BOUND ( 'NONE', #36092, .T. ) ;
#48769 = ADVANCED_FACE ( 'NONE', ( #16684 ), #411, .T. ) ;
#48770 = ORIENTED_EDGE ( 'NONE', *, *, #25397, .F. ) ;
#48771 = CARTESIAN_POINT ( 'NONE',  ( -15.50000000000000000, 0.000000000000000000, -22.50000000000000000 ) ) ;
#48772 = CIRCLE ( 'NONE', #53326, 0.1999999999999996503 ) ;
#48773 = EDGE_CURVE ( 'NONE', #20589, #57392, #37206, .T. ) ;
#48774 = DIRECTION ( 'NONE',  ( 1.836970198721029934E-16, 1.836970198721010706E-16, -1.000000000000000000 ) ) ;
#48775 = DIRECTION ( 'NONE',  ( 0.000000000000000000, 0.2142857142857142738, 0.9767710236555245951 ) ) ;
#48776 = VERTEX_POINT ( 'NONE', #10668 ) ;
#48777 = ORIENTED_EDGE ( 'NONE', *, *, #8127, .T. ) ;
#48778 = PLANE ( 'NONE',  #42993 ) ;
#48779 = ORIENTED_EDGE ( 'NONE', *, *, #14246, .T. ) ;
#48780 = EDGE_CURVE ( 'NONE', #67915, #63729, #27623, .T. ) ;
#48781 = EDGE_LOOP ( 'NONE', ( #61877, #40038, #24125, #2244 ) ) ;
#48782 = PRODUCT_DEFINITION_CONTEXT ( 'detailed design', #54903, 'design' ) ;
#48783 = PLANE ( 'NONE',  #58699 ) ;
#48784 = CARTESIAN_POINT ( 'NONE',  ( 7.250000000000005329, -7.449999999999998401, -10.00000000000000000 ) ) ;
#48785 = LINE ( 'NONE', #6338, #8359 ) ;
#48786 = VECTOR ( 'NONE', #40799, 1000.000000000000000 ) ;
#48787 = ORIENTED_EDGE ( 'NONE', *, *, #66524, .F. ) ;
#48788 = EDGE_CURVE ( 'NONE', #36931, #56714, #42842, .T. ) ;
#48789 = DIRECTION ( 'NONE',  ( -1.836970198721029934E-16, 1.836970198721036344E-16, -1.000000000000000000 ) ) ;
#48791 = CARTESIAN_POINT ( 'NONE',  ( 10.90000000000000036, 20.60000000000000142, -13.86939075806900057 ) ) ;
#48790 = LINE ( 'NONE', #48441, #53632 ) ;
#48792 = ORIENTED_EDGE ( 'NONE', *, *, #23397, .F. ) ;
#48793 = ORIENTED_EDGE ( 'NONE', *, *, #49726, .F. ) ;
#48794 = ADVANCED_FACE ( 'NONE', ( #11022 ), #32235, .F. ) ;
#48796 = ORIENTED_EDGE ( 'NONE', *, *, #41645, .F. ) ;
#48795 = DIRECTION ( 'NONE',  ( -1.000000000000000000, 0.000000000000000000, 0.000000000000000000 ) ) ;
#48797 = VECTOR ( 'NONE', #28214, 1000.000000000000000 ) ;
#48798 = ORIENTED_EDGE ( 'NONE', *, *, #35071, .F. ) ;
#48799 = EDGE_CURVE ( 'NONE', #22437, #10280, #15857, .T. ) ;
#48800 = CARTESIAN_POINT ( 'NONE',  ( 7.281754163448140638, 8.000000000000001776, 0.000000000000000000 ) ) ;
#48801 = VECTOR ( 'NONE', #23664, 1000.000000000000000 ) ;
#48802 = EDGE_LOOP ( 'NONE', ( #18383, #69144, #41010, #785 ) ) ;
#48803 = ADVANCED_FACE ( 'NONE', ( #4675 ), #58769, .T. ) ;
#48804 = ORIENTED_EDGE ( 'NONE', *, *, #26189, .T. ) ;
#48805 = ADVANCED_FACE ( 'NONE', ( #47794 ), #11359, .T. ) ;
#48806 = DIRECTION ( 'NONE',  ( -0.000000000000000000, -0.000000000000000000, -1.000000000000000000 ) ) ;
#48807 = PLANE ( 'NONE',  #61657 ) ;
#48808 = EDGE_CURVE ( 'NONE', #57192, #28510, #32930, .T. ) ;
#48810 = ADVANCED_FACE ( 'NONE', ( #773 ), #16321, .F. ) ;
#48809 = AXIS2_PLACEMENT_3D ( 'NONE', #58879, #26691, #31661 ) ;
#48811 = EDGE_CURVE ( 'NONE', #18896, #2326, #4559, .T. ) ;
#48812 = ORIENTED_EDGE ( 'NONE', *, *, #65655, .T. ) ;
#48813 = CARTESIAN_POINT ( 'NONE',  ( -25.50000000000000355, -15.50000000000000000, -22.50000000000000000 ) ) ;
#48814 = DIRECTION ( 'NONE',  ( 1.836970198721029934E-16, 1.836970198721010706E-16, -1.000000000000000000 ) ) ;
#48815 = DIRECTION ( 'NONE',  ( 0.000000000000000000, 0.000000000000000000, -1.000000000000000000 ) ) ;
#48816 = ORIENTED_EDGE ( 'NONE', *, *, #2901, .F. ) ;
#48817 = AXIS2_PLACEMENT_3D ( 'NONE', #33542, #39196, #23970 ) ;
#48818 = EDGE_CURVE ( 'NONE', #68319, #18594, #22339, .T. ) ;
#48819 = AXIS2_PLACEMENT_3D ( 'NONE', #10239, #36772, #58342 ) ;
#48820 = DIRECTION ( 'NONE',  ( 8.540177112501197482E-15, 1.000000000000000000, -0.000000000000000000 ) ) ;
#48821 = EDGE_CURVE ( 'NONE', #51395, #50609, #43880, .T. ) ;
#48822 = CARTESIAN_POINT ( 'NONE',  ( 7.000000000000000000, -32.95000000000000284, 13.19999999999999929 ) ) ;
#48824 = ORIENTED_EDGE ( 'NONE', *, *, #56860, .F. ) ;
#48823 = CARTESIAN_POINT ( 'NONE',  ( 29.25000000000000000, -5.000000000000000000, -11.75000000000000000 ) ) ;
#48826 = VERTEX_POINT ( 'NONE', #64760 ) ;
#48825 = CARTESIAN_POINT ( 'NONE',  ( 146.5599459900709860, 0.000000000000000000, 328.5239988703752942 ) ) ;
#48827 = EDGE_CURVE ( 'NONE', #49071, #2772, #37899, .T. ) ;
#48829 = LINE ( 'NONE', #31178, #57668 ) ;
#48828 = AXIS2_PLACEMENT_3D ( 'NONE', #31804, #37109, #10568 ) ;
#48830 = DIRECTION ( 'NONE',  ( -1.000000000000000000, 0.000000000000000000, 0.000000000000000000 ) ) ;
#48831 = DIRECTION ( 'NONE',  ( 0.4999999999999974465, -0.8660254037844401509, -2.509347957447879284E-16 ) ) ;
#48832 = CARTESIAN_POINT ( 'NONE',  ( 29.50000000000000355, -12.00000000000000000, -11.03137303340310282 ) ) ;
#48833 = CARTESIAN_POINT ( 'NONE',  ( 30.00000000000000000, -12.00000000000000000, 10.52786404500095863 ) ) ;
#48834 = DIRECTION ( 'NONE',  ( 0.000000000000000000, 0.000000000000000000, -1.000000000000000000 ) ) ;
#48835 = EDGE_CURVE ( 'NONE', #62567, #53126, #65460, .T. ) ;
#48836 = VERTEX_POINT ( 'NONE', #43531 ) ;
#48837 = LINE ( 'NONE', #64404, #48506 ) ;
#48840 = ORIENTED_EDGE ( 'NONE', *, *, #9540, .T. ) ;
#48839 = ADVANCED_FACE ( 'NONE', ( #38590 ), #50914, .T. ) ;
#48838 = CARTESIAN_POINT ( 'NONE',  ( -11.77351654964679284, -7.826483450353365789, 455.0000000000000568 ) ) ;
#48842 = ORIENTED_EDGE ( 'NONE', *, *, #58859, .T. ) ;
#48841 = CARTESIAN_POINT ( 'NONE',  ( 27.00000000000000000, 3.010794155703768650E-16, 2.458500000000000796 ) ) ;
#48843 = DIRECTION ( 'NONE',  ( 0.000000000000000000, -0.1249999999999996531, -0.9921567416492215186 ) ) ;
#48844 = PLANE ( 'NONE',  #29564 ) ;
#48845 = ORIENTED_EDGE ( 'NONE', *, *, #52524, .F. ) ;
#48846 = CYLINDRICAL_SURFACE ( 'NONE', #7141, 1.000000000000000000 ) ;
#48847 = CARTESIAN_POINT ( 'NONE',  ( 15.50000000000000000, -1.037157890325000054, -22.50000000000000000 ) ) ;
#48848 = VECTOR ( 'NONE', #58588, 1000.000000000000000 ) ;
#48849 = ORIENTED_EDGE ( 'NONE', *, *, #28435, .F. ) ;
#48850 = DIRECTION ( 'NONE',  ( -0.7071067811865391350, 0.7071067811865560104, 1.750285133459120294E-30 ) ) ;
#48851 = CYLINDRICAL_SURFACE ( 'NONE', #60880, 1.224999999999998757 ) ;
#48852 = CARTESIAN_POINT ( 'NONE',  ( 7.250000000000005329, -7.249999999999998224, -14.50000000000000000 ) ) ;
#48853 = CIRCLE ( 'NONE', #18326, 2.204799999999999205 ) ;
#48854 = EDGE_LOOP ( 'NONE', ( #3746, #44756, #23735, #13523, #9583, #64612, #5623, #13274, #24257, #69597, #14829, #65199, #31065, #33322 ) ) ;
#48855 = DIRECTION ( 'NONE',  ( 1.920885163218982051E-15, 1.000000000000000000, 1.836970198721033139E-16 ) ) ;
#48856 = ORIENTED_EDGE ( 'NONE', *, *, #58515, .F. ) ;
#48857 = ORIENTED_EDGE ( 'NONE', *, *, #19864, .F. ) ;
#48858 = CIRCLE ( 'NONE', #9327, 1.000000000000000000 ) ;
#48859 = DIRECTION ( 'NONE',  ( 0.000000000000000000, -1.000000000000000000, 3.819861094142539476E-12 ) ) ;
#48860 = CARTESIAN_POINT ( 'NONE',  ( -24.00000000000000000, -15.50000000000000000, 14.50000000000000000 ) ) ;
#48861 = FACE_OUTER_BOUND ( 'NONE', #52531, .T. ) ;
#48862 = CARTESIAN_POINT ( 'NONE',  ( -8.250000000000001776, 0.000000000000000000, -11.50000000000000000 ) ) ;
#48863 = VERTEX_POINT ( 'NONE', #49880 ) ;
#48864 = ORIENTED_EDGE ( 'NONE', *, *, #43149, .T. ) ;
#48866 = ORIENTED_EDGE ( 'NONE', *, *, #51335, .F. ) ;
#48865 = CARTESIAN_POINT ( 'NONE',  ( -11.11351654964670921, 8.693516549646615132, 455.0000000000000568 ) ) ;
#48867 = ORIENTED_EDGE ( 'NONE', *, *, #22660, .T. ) ;
#48868 = ADVANCED_FACE ( 'NONE', ( #22668 ), #13438, .F. ) ;
#48869 = DIRECTION ( 'NONE',  ( 0.000000000000000000, 3.673940397442059868E-16, -1.000000000000000000 ) ) ;
#48870 = AXIS2_PLACEMENT_3D ( 'NONE', #64524, #17111, #32002 ) ;
#48871 = CARTESIAN_POINT ( 'NONE',  ( 0.000000000000000000, -8.249999999999998224, -19.50000000000000000 ) ) ;
#48872 = CARTESIAN_POINT ( 'NONE',  ( -11.77351654964670935, 7.593516549646604830, 195.0000000000000284 ) ) ;
#48873 = ADVANCED_FACE ( 'NONE', ( #17707 ), #54849, .F. ) ;
#48874 = CIRCLE ( 'NONE', #46626, 0.2000000000000005107 ) ;
#48875 = CYLINDRICAL_SURFACE ( 'NONE', #54877, 3.500000000000003109 ) ;
#48877 = DIRECTION ( 'NONE',  ( 0.000000000000000000, 1.000000000000000000, 0.000000000000000000 ) ) ;
#48876 = DIRECTION ( 'NONE',  ( -0.000000000000000000, -0.000000000000000000, -1.000000000000000000 ) ) ;
#48878 = VECTOR ( 'NONE', #36132, 1000.000000000000000 ) ;
#48879 = EDGE_LOOP ( 'NONE', ( #5920, #42512, #50985, #33125 ) ) ;
#48880 = ADVANCED_FACE ( 'NONE', ( #12373 ), #45255, .F. ) ;
#48882 = EDGE_LOOP ( 'NONE', ( #62077, #59970, #26937, #43250 ) ) ;
#48881 = DIRECTION ( 'NONE',  ( -0.000000000000000000, 1.000000000000000000, -0.000000000000000000 ) ) ;
#48883 = ORIENTED_EDGE ( 'NONE', *, *, #19868, .F. ) ;
#48884 = ORIENTED_EDGE ( 'NONE', *, *, #23743, .F. ) ;
#48885 = LINE ( 'NONE', #20134, #66053 ) ;
#48886 = CIRCLE ( 'NONE', #20648, 0.2000000000000005107 ) ;
#48887 = ADVANCED_FACE ( 'NONE', ( #67178 ), #39269, .F. ) ;
#48888 = DIRECTION ( 'NONE',  ( 0.000000000000000000, 0.000000000000000000, 1.000000000000000000 ) ) ;
#48889 = DIRECTION ( 'NONE',  ( 1.836970198721029934E-16, 1.836970198721010706E-16, -1.000000000000000000 ) ) ;
#48890 = VECTOR ( 'NONE', #52021, 1000.000000000000000 ) ;
#48891 = ORIENTED_EDGE ( 'NONE', *, *, #65946, .T. ) ;
#48892 = EDGE_LOOP ( 'NONE', ( #45530, #95, #13911, #46516 ) ) ;
#48893 = EDGE_LOOP ( 'NONE', ( #7528, #34076, #65580, #7432 ) ) ;
#48894 = FACE_OUTER_BOUND ( 'NONE', #41474, .T. ) ;
#48895 = DIRECTION ( 'NONE',  ( 1.000000000000000000, -5.626525616968433909E-15, -1.836970198721040534E-16 ) ) ;
#48896 = DIRECTION ( 'NONE',  ( 1.000000000000000000, 0.000000000000000000, 0.000000000000000000 ) ) ;
#48897 = TOROIDAL_SURFACE ( 'NONE', #36463, 8.300000000000006040, 1.000000000000000000 ) ;
#48898 = EDGE_LOOP ( 'NONE', ( #7777, #69136, #2959, #63564 ) ) ;
#48899 = ADVANCED_FACE ( 'NONE', ( #12721 ), #49540, .T. ) ;
#48900 = ORIENTED_EDGE ( 'NONE', *, *, #50688, .F. ) ;
#48901 = CARTESIAN_POINT ( 'NONE',  ( 7.450000000000006395, 7.250000000000000888, -19.50000000000000000 ) ) ;
#48902 = AXIS2_PLACEMENT_3D ( 'NONE', #7927, #7586, #20211 ) ;
#48903 = CARTESIAN_POINT ( 'NONE',  ( 15.50000000000000000, -0.4000000000000000222, -19.00000000000000355 ) ) ;
#48904 = ORIENTED_EDGE ( 'NONE', *, *, #64668, .F. ) ;
#48905 = CARTESIAN_POINT ( 'NONE',  ( 1.690483450353418737, 10.73351654964659652, 455.0000000000000568 ) ) ;
#48906 = CIRCLE ( 'NONE', #3762, 4.000000000000000000 ) ;
#48908 = ORIENTED_EDGE ( 'NONE', *, *, #28082, .T. ) ;
#48907 = DIRECTION ( 'NONE',  ( 1.000000000000000000, -0.000000000000000000, 0.000000000000000000 ) ) ;
#48909 = ORIENTED_EDGE ( 'NONE', *, *, #36727, .T. ) ;
#48910 = LINE ( 'NONE', #5077, #22477 ) ;
#48911 = LINE ( 'NONE', #65182, #8614 ) ;
#48912 = CARTESIAN_POINT ( 'NONE',  ( -11.11351654964668612, 8.693516549646636449, 194.9999952000000292 ) ) ;
#48913 = DIRECTION ( 'NONE',  ( 0.000000000000000000, 0.000000000000000000, 1.000000000000000000 ) ) ;
#48914 = CARTESIAN_POINT ( 'NONE',  ( 49.00000000000000000, -21.00000000000000000, 13.86939075806900057 ) ) ;
#48915 = ADVANCED_FACE ( 'NONE', ( #27976 ), #61167, .F. ) ;
#48916 = ORIENTED_EDGE ( 'NONE', *, *, #25349, .T. ) ;
#48917 = LINE ( 'NONE', #64487, #37159 ) ;
#48919 = ORIENTED_EDGE ( 'NONE', *, *, #30083, .F. ) ;
#48918 = EDGE_CURVE ( 'NONE', #34291, #46672, #1022, .T. ) ;
#48920 = DIRECTION ( 'NONE',  ( 0.7071067811865500152, 0.7071067811865451302, -4.683861624749757595E-31 ) ) ;
#48921 = VECTOR ( 'NONE', #60843, 1000.000000000000000 ) ;
#48922 = CARTESIAN_POINT ( 'NONE',  ( -11.00000000000000000, -17.50000000000000000, -15.70500000000000007 ) ) ;
#48923 = EDGE_CURVE ( 'NONE', #8038, #20570, #60825, .T. ) ;
#48924 = LINE ( 'NONE', #16750, #26869 ) ;
#48926 = CARTESIAN_POINT ( 'NONE',  ( 27.00000000000000000, 3.010794155703768650E-16, 2.458500000000000796 ) ) ;
#48925 = AXIS2_PLACEMENT_3D ( 'NONE', #61332, #30233, #51794 ) ;
#48927 = CIRCLE ( 'NONE', #28548, 0.1749999999999989342 ) ;
#48928 = LINE ( 'NONE', #5094, #66420 ) ;
#48929 = VERTEX_POINT ( 'NONE', #65798 ) ;
#48930 = VECTOR ( 'NONE', #46621, 1000.000000000000000 ) ;
#48931 = FACE_OUTER_BOUND ( 'NONE', #13182, .T. ) ;
#48932 = AXIS2_PLACEMENT_3D ( 'NONE', #66717, #61769, #39832 ) ;
#48933 = LINE ( 'NONE', #31289, #66062 ) ;
#48934 = VERTEX_POINT ( 'NONE', #38924 ) ;
#48935 = CARTESIAN_POINT ( 'NONE',  ( 106.4257688009193430, 0.000000000000000000, 334.4830310981789694 ) ) ;
#48936 = LINE ( 'NONE', #32667, #2691 ) ;
#48937 = ORIENTED_EDGE ( 'NONE', *, *, #69912, .F. ) ;
#48938 = CARTESIAN_POINT ( 'NONE',  ( 29.50000000000000355, -11.50000000000000000, 15.00000000000000000 ) ) ;
#48939 = LINE ( 'NONE', #6144, #28570 ) ;
#48940 = ORIENTED_EDGE ( 'NONE', *, *, #45807, .T. ) ;
#48941 = CARTESIAN_POINT ( 'NONE',  ( -10.73351654964671020, 1.677516549646604016, 195.0000000000000284 ) ) ;
#48942 = CIRCLE ( 'NONE', #27479, 0.3000000000005387246 ) ;
#48943 = DIRECTION ( 'NONE',  ( -0.7071067811865550112, -0.7071067811865401342, 0.000000000000000000 ) ) ;
#48944 = DIRECTION ( 'NONE',  ( 1.000000000000000000, 0.000000000000000000, 0.000000000000000000 ) ) ;
#48945 = FACE_OUTER_BOUND ( 'NONE', #62067, .T. ) ;
#48946 = AXIS2_PLACEMENT_3D ( 'NONE', #48711, #16183, #27835 ) ;
#48947 = EDGE_LOOP ( 'NONE', ( #1374, #22360, #62141, #63487 ) ) ;
#48949 = ORIENTED_EDGE ( 'NONE', *, *, #66531, .T. ) ;
#48948 = CARTESIAN_POINT ( 'NONE',  ( -7.342976262117282715, -5.552858015815545834, 54.00000000000000711 ) ) ;
#48950 = EDGE_CURVE ( 'NONE', #51945, #51749, #37167, .T. ) ;
#48951 = CARTESIAN_POINT ( 'NONE',  ( 11.12648345035340647, 7.793516549646564151, 455.0000000000000568 ) ) ;
#48952 = CARTESIAN_POINT ( 'NONE',  ( 283.0000000000000568, -32.00000000000000000, 8.400000000000000355 ) ) ;
#48953 = DIRECTION ( 'NONE',  ( -1.000000000000000000, 0.000000000000000000, 0.000000000000000000 ) ) ;
#48954 = ORIENTED_EDGE ( 'NONE', *, *, #55593, .T. ) ;
#48955 = VECTOR ( 'NONE', #17977, 1000.000000000000000 ) ;
#48956 = EDGE_CURVE ( 'NONE', #3545, #65838, #17348, .T. ) ;
#48957 = FACE_OUTER_BOUND ( 'NONE', #22785, .T. ) ;
#48958 = CARTESIAN_POINT ( 'NONE',  ( 50.83090410532631864, 3.657408540445007628, 2.000000000000000000 ) ) ;
#48959 = EDGE_CURVE ( 'NONE', #6054, #2145, #60853, .T. ) ;
#48960 = ORIENTED_EDGE ( 'NONE', *, *, #27131, .T. ) ;
#48961 = VERTEX_POINT ( 'NONE', #23360 ) ;
#48962 = ADVANCED_FACE ( 'NONE', ( #33621 ), #29341, .T. ) ;
#48963 = ORIENTED_EDGE ( 'NONE', *, *, #20696, .F. ) ;
#48964 = EDGE_CURVE ( 'NONE', #8868, #1245, #39604, .T. ) ;
#48965 = EDGE_CURVE ( 'NONE', #29553, #30907, #6798, .T. ) ;
#48966 = DIRECTION ( 'NONE',  ( -1.000000000000000000, 0.000000000000000000, 0.000000000000000000 ) ) ;
#48967 = DIRECTION ( 'NONE',  ( 0.000000000000000000, 0.000000000000000000, -1.000000000000000000 ) ) ;
#48968 =( NAMED_UNIT ( * ) PLANE_ANGLE_UNIT ( ) SI_UNIT ( $, .RADIAN. ) );
#48969 = VECTOR ( 'NONE', #49398, 1000.000000000000114 ) ;
#48970 = EDGE_CURVE ( 'NONE', #36267, #39887, #51837, .T. ) ;
#48971 = EDGE_LOOP ( 'NONE', ( #55048, #63415, #48113, #41836 ) ) ;
#48972 = ORIENTED_EDGE ( 'NONE', *, *, #5151, .F. ) ;
#48973 = ORIENTED_EDGE ( 'NONE', *, *, #35801, .F. ) ;
#48974 = AXIS2_PLACEMENT_3D ( 'NONE', #34202, #17266, #22921 ) ;
#48975 = CARTESIAN_POINT ( 'NONE',  ( 41.09999999999999432, 20.60000000000000142, 13.86939075806900057 ) ) ;
#48976 = ORIENTED_EDGE ( 'NONE', *, *, #3969, .F. ) ;
#48977 = AXIS2_PLACEMENT_3D ( 'NONE', #62752, #14330, #9004 ) ;
#48978 = CIRCLE ( 'NONE', #26358, 0.5250000000000003553 ) ;
#48979 = ORIENTED_EDGE ( 'NONE', *, *, #66831, .T. ) ;
#48980 = ORIENTED_EDGE ( 'NONE', *, *, #25495, .T. ) ;
#48981 = VERTEX_POINT ( 'NONE', #45970 ) ;
#48982 = CARTESIAN_POINT ( 'NONE',  ( 5.257023737882819070, -5.257023737882815517, 26.00000000000000711 ) ) ;
#48983 = AXIS2_PLACEMENT_3D ( 'NONE', #11374, #32611, #21991 ) ;
#48984 = VECTOR ( 'NONE', #8164, 1000.000000000000000 ) ;
#48986 = ORIENTED_EDGE ( 'NONE', *, *, #68644, .F. ) ;
#48985 = LINE ( 'NONE', #32711, #8505 ) ;
#48987 = DIRECTION ( 'NONE',  ( -1.047444401652940007E-14, -1.000000000000000000, 0.000000000000000000 ) ) ;
#48988 = DIRECTION ( 'NONE',  ( -0.000000000000000000, 0.000000000000000000, 1.000000000000000000 ) ) ;
#48989 = DIRECTION ( 'NONE',  ( 0.000000000000000000, -1.000000000000000000, 0.000000000000000000 ) ) ;
#48990 = ORIENTED_EDGE ( 'NONE', *, *, #53014, .T. ) ;
#48991 = LINE ( 'NONE', #918, #22114 ) ;
#48992 = ORIENTED_EDGE ( 'NONE', *, *, #12728, .T. ) ;
#48993 = DIRECTION ( 'NONE',  ( 1.000000000000000000, -8.728482790395504563E-15, -3.206792553201184024E-30 ) ) ;
#48994 = EDGE_CURVE ( 'NONE', #32184, #67007, #8835, .T. ) ;
#48995 = DIRECTION ( 'NONE',  ( -1.000000000000000000, 0.000000000000000000, 0.000000000000000000 ) ) ;
#48996 = FACE_OUTER_BOUND ( 'NONE', #4798, .T. ) ;
#48997 = LINE ( 'NONE', #69862, #23402 ) ;
#48998 = ORIENTED_EDGE ( 'NONE', *, *, #64840, .T. ) ;
#48999 = EDGE_CURVE ( 'NONE', #17134, #24869, #30407, .T. ) ;
#49000 = CARTESIAN_POINT ( 'NONE',  ( 30.00000000000000000, -10.85999999999999943, -9.000000000000001776 ) ) ;
#49001 = EDGE_CURVE ( 'NONE', #62786, #46075, #62224, .T. ) ;
#49002 = CARTESIAN_POINT ( 'NONE',  ( 9.690000000000001279, -8.750000000000000000, -7.000000000000000000 ) ) ;
#49003 = DIRECTION ( 'NONE',  ( -1.836970198721029934E-16, 1.836970198721036344E-16, -1.000000000000000000 ) ) ;
#49004 = EDGE_CURVE ( 'NONE', #6993, #44864, #56911, .T. ) ;
#49005 = APPLICATION_CONTEXT ( 'automotive_design' ) ;
#49006 = CARTESIAN_POINT ( 'NONE',  ( 29.50000000000000355, -11.50000000000100009, 15.00000000000084910 ) ) ;
#49007 = CARTESIAN_POINT ( 'NONE',  ( 10.31452373788278187, 3.650476262117146042, 54.00000000000000711 ) ) ;
#49008 = DIRECTION ( 'NONE',  ( 0.000000000000000000, -1.000000000000000000, 0.000000000000000000 ) ) ;
#49009 = DIRECTION ( 'NONE',  ( 0.000000000000000000, 0.000000000000000000, -1.000000000000000000 ) ) ;
#49010 = CARTESIAN_POINT ( 'NONE',  ( 9.912023737882798002, 6.642976262117190167, 26.00000000000000711 ) ) ;
#49011 = VECTOR ( 'NONE', #9892, 1000.000000000000000 ) ;
#49012 = AXIS2_PLACEMENT_3D ( 'NONE', #65237, #33041, #10772 ) ;
#49013 = ORIENTED_EDGE ( 'NONE', *, *, #23485, .T. ) ;
#49014 = DIRECTION ( 'NONE',  ( 0.000000000000000000, 1.000000000000000000, 3.673940397442059868E-16 ) ) ;
#49015 = PLANE ( 'NONE',  #53418 ) ;
#49016 = LINE ( 'NONE', #38739, #54976 ) ;
#49017 = LINE ( 'NONE', #17172, #46596 ) ;
#49018 = AXIS2_PLACEMENT_3D ( 'NONE', #60578, #65546, #1198 ) ;
#49019 = ORIENTED_EDGE ( 'NONE', *, *, #15496, .F. ) ;
#49020 = VECTOR ( 'NONE', #1248, 1000.000000000000000 ) ;
#49021 = FACE_OUTER_BOUND ( 'NONE', #28163, .T. ) ;
#49022 = CARTESIAN_POINT ( 'NONE',  ( -30.00000000000000000, -12.00000000000000000, 12.20000000000000107 ) ) ;
#49023 = DIRECTION ( 'NONE',  ( 1.000000000000000000, 2.135044278125299371E-15, 7.844025423732059533E-31 ) ) ;
#49024 = LINE ( 'NONE', #31725, #1631 ) ;
#49025 = AXIS2_PLACEMENT_3D ( 'NONE', #64691, #37828, #32867 ) ;
#49026 = CARTESIAN_POINT ( 'NONE',  ( 30.00000000000000000, -12.00000000000000000, 11.03137303340310282 ) ) ;
#49027 = DIRECTION ( 'NONE',  ( 0.000000000000000000, 0.000000000000000000, 1.000000000000000000 ) ) ;
#49028 = ORIENTED_EDGE ( 'NONE', *, *, #13665, .T. ) ;
#49029 = ORIENTED_EDGE ( 'NONE', *, *, #9894, .F. ) ;
#49030 = CARTESIAN_POINT ( 'NONE',  ( 3.006483450353407250, 7.415254214038215608, 455.0000000000000568 ) ) ;
#49031 = CARTESIAN_POINT ( 'NONE',  ( 7.450000000000004619, -1.336933437520057563E-15, -14.50000000000000000 ) ) ;
#49032 = ORIENTED_EDGE ( 'NONE', *, *, #8896, .F. ) ;
#49033 = AXIS2_PLACEMENT_3D ( 'NONE', #15304, #42519, #31920 ) ;
#49034 = CYLINDRICAL_SURFACE ( 'NONE', #40862, 2.215251240775983899 ) ;
#49035 = EDGE_LOOP ( 'NONE', ( #68019, #2748, #37196, #3807 ) ) ;
#49036 = DIRECTION ( 'NONE',  ( 1.000000000000000000, -0.000000000000000000, 0.000000000000000000 ) ) ;
#49037 = ORIENTED_EDGE ( 'NONE', *, *, #29576, .T. ) ;
#49038 = ORIENTED_EDGE ( 'NONE', *, *, #22491, .F. ) ;
#49039 = CARTESIAN_POINT ( 'NONE',  ( 9.703773737882785966, -10.05377373788281403, 26.00000000000000000 ) ) ;
#49040 = EDGE_CURVE ( 'NONE', #19647, #42529, #34996, .T. ) ;
#49041 = ORIENTED_EDGE ( 'NONE', *, *, #32518, .F. ) ;
#49042 = DIRECTION ( 'NONE',  ( 0.000000000000000000, 0.000000000000000000, -1.000000000000000000 ) ) ;
#49043 = CARTESIAN_POINT ( 'NONE',  ( -11.00000000000000000, -12.00000000000000000, 10.52786404500095863 ) ) ;
#49044 = CARTESIAN_POINT ( 'NONE',  ( 7.250000000000005329, -8.249999999999998224, -10.00000000000000000 ) ) ;
#49045 = ADVANCED_FACE ( 'NONE', ( #25103 ), #47016, .F. ) ;
#49046 = ORIENTED_EDGE ( 'NONE', *, *, #20624, .F. ) ;
#49047 = VECTOR ( 'NONE', #24917, 1000.000000000000000 ) ;
#49048 = ORIENTED_EDGE ( 'NONE', *, *, #16984, .T. ) ;
#49049 = DIRECTION ( 'NONE',  ( -1.836970198721029934E-16, -1.836970198721010706E-16, 1.000000000000000000 ) ) ;
#49050 = CARTESIAN_POINT ( 'NONE',  ( 10.90000000000000036, -0.2000000000089119934, -8.913009219568841313E-12 ) ) ;
#49051 = ORIENTED_EDGE ( 'NONE', *, *, #32419, .T. ) ;
#49052 = AXIS2_PLACEMENT_3D ( 'NONE', #39179, #55447, #67453 ) ;
#49053 = ORIENTED_EDGE ( 'NONE', *, *, #61803, .T. ) ;
#49054 = VERTEX_POINT ( 'NONE', #8472 ) ;
#49055 = LINE ( 'NONE', #38451, #61543 ) ;
#49057 = ORIENTED_EDGE ( 'NONE', *, *, #10519, .F. ) ;
#49056 = DIRECTION ( 'NONE',  ( -1.836970198721029934E-16, 1.836970198721036344E-16, -1.000000000000000000 ) ) ;
#49058 = CARTESIAN_POINT ( 'NONE',  ( -3.710438382363177912, -7.408280051175174741, 54.00000000000000711 ) ) ;
#49059 = CYLINDRICAL_SURFACE ( 'NONE', #15928, 0.5249999999999994671 ) ;
#49060 = EDGE_LOOP ( 'NONE', ( #10371, #61236, #17784, #59328 ) ) ;
#49061 = EDGE_LOOP ( 'NONE', ( #66603, #32720, #4163, #29754 ) ) ;
#49062 = AXIS2_PLACEMENT_3D ( 'NONE', #4348, #47457, #69025 ) ;
#49063 = VECTOR ( 'NONE', #51419, 1000.000000000000000 ) ;
#49064 = ORIENTED_EDGE ( 'NONE', *, *, #21427, .T. ) ;
#49065 = CARTESIAN_POINT ( 'NONE',  ( 15.00000000000000000, -42.00000000000000000, -15.10000000000000142 ) ) ;
#49066 = CARTESIAN_POINT ( 'NONE',  ( -8.697938382363135545, 2.406732575409538111, 54.00000000000000711 ) ) ;
#49067 = ORIENTED_EDGE ( 'NONE', *, *, #57418, .T. ) ;
#49068 = DIRECTION ( 'NONE',  ( -1.836970198721029934E-16, -1.836970198721010706E-16, 1.000000000000000000 ) ) ;
#49069 = PLANE ( 'NONE',  #38059 ) ;
#49071 = VERTEX_POINT ( 'NONE', #13784 ) ;
#49070 = DIRECTION ( 'NONE',  ( 1.000000000000000000, 0.000000000000000000, 0.000000000000000000 ) ) ;
#49072 = EDGE_LOOP ( 'NONE', ( #68149, #6770, #61070, #45828 ) ) ;
#49073 = EDGE_CURVE ( 'NONE', #52982, #5963, #8120, .T. ) ;
#49074 = AXIS2_PLACEMENT_3D ( 'NONE', #27560, #65056, #65736 ) ;
#49075 = DIRECTION ( 'NONE',  ( -1.836970198721029934E-16, 1.836970198721036590E-16, -1.000000000000000000 ) ) ;
#49076 = DIRECTION ( 'NONE',  ( 1.836970198721029934E-16, 1.836970198721010706E-16, -1.000000000000000000 ) ) ;
#49077 = CARTESIAN_POINT ( 'NONE',  ( -8.697938382363135545, 8.079219948824830411, 54.00000000000000711 ) ) ;
#49078 = CARTESIAN_POINT ( 'NONE',  ( -4.135079735113167843, 3.663616288757005623, 54.00000000000000711 ) ) ;
#49079 = EDGE_CURVE ( 'NONE', #52737, #60571, #14498, .T. ) ;
#49080 = CARTESIAN_POINT ( 'NONE',  ( -8.250000000000001776, -7.249999999999998224, -11.50000000000000000 ) ) ;
#49081 = VERTEX_POINT ( 'NONE', #3543 ) ;
#49082 = DIRECTION ( 'NONE',  ( 0.000000000000000000, -1.000000000000000000, 0.000000000000000000 ) ) ;
#49083 = CARTESIAN_POINT ( 'NONE',  ( 9.249999999999998224, -7.848062532927998269, 5.000000000000000000 ) ) ;
#49084 = PLANE ( 'NONE',  #66178 ) ;
#49086 = ORIENTED_EDGE ( 'NONE', *, *, #66004, .F. ) ;
#49085 = DIRECTION ( 'NONE',  ( 0.000000000000000000, -1.000000000000000000, 0.000000000000000000 ) ) ;
#49087 = DIRECTION ( 'NONE',  ( -0.9583148474998867128, 0.000000000000000000, 0.2857142857143631365 ) ) ;
#49088 = AXIS2_PLACEMENT_3D ( 'NONE', #45612, #13792, #2833 ) ;
#49089 = CARTESIAN_POINT ( 'NONE',  ( 152.0064834503532722, -35.83962462487175316, 5.000000000000000000 ) ) ;
#49090 = EDGE_CURVE ( 'NONE', #1707, #65063, #51629, .T. ) ;
#49091 = CARTESIAN_POINT ( 'NONE',  ( 10.74648345035337904, -1.690483450353491124, 455.0000000000000568 ) ) ;
#49092 = ORIENTED_EDGE ( 'NONE', *, *, #13739, .T. ) ;
#49093 = CARTESIAN_POINT ( 'NONE',  ( 7.250000000000005329, -8.249999999999998224, -22.50000000000000000 ) ) ;
#49094 = DIRECTION ( 'NONE',  ( -1.000000000000000000, 0.000000000000000000, 0.000000000000000000 ) ) ;
#49095 = VECTOR ( 'NONE', #64587, 1000.000000000000000 ) ;
#49096 = ORIENTED_EDGE ( 'NONE', *, *, #8801, .T. ) ;
#49097 = DIRECTION ( 'NONE',  ( -1.836970198721029934E-16, 1.836970198721036344E-16, -1.000000000000000000 ) ) ;
#49098 = DIRECTION ( 'NONE',  ( 0.000000000000000000, 1.000000000000000000, 0.000000000000000000 ) ) ;
#49099 = CARTESIAN_POINT ( 'NONE',  ( -7.450000000000001954, -7.249999999999998224, -7.000000000000000000 ) ) ;
#49100 = EDGE_CURVE ( 'NONE', #17018, #18984, #46661, .T. ) ;
#49101 = DIRECTION ( 'NONE',  ( 0.5773502691896230665, 0.5773502691896271743, 0.5773502691896271743 ) ) ;
#49102 = LINE ( 'NONE', #60741, #29346 ) ;
#49103 = DIRECTION ( 'NONE',  ( -0.000000000000000000, -0.000000000000000000, -1.000000000000000000 ) ) ;
#49104 = AXIS2_PLACEMENT_3D ( 'NONE', #42480, #26927, #32916 ) ;
#49105 = AXIS2_PLACEMENT_3D ( 'NONE', #41300, #68176, #34933 ) ;
#49106 = B_SPLINE_CURVE_WITH_KNOTS ( 'NONE', 3,
 ( #9299, #12913, #67387, #67021, #1616, #2324 ),
 .UNSPECIFIED., .F., .F.,
 ( 4, 2, 4 ),
 ( 1.820537833122031213, 2.555393473688635453, 3.290249114255239693 ),
 .UNSPECIFIED. ) ;
#49107 = ORIENTED_EDGE ( 'NONE', *, *, #69362, .F. ) ;
#49108 = DIRECTION ( 'NONE',  ( 0.000000000000000000, 0.000000000000000000, 1.000000000000000000 ) ) ;
#49109 = CARTESIAN_POINT ( 'NONE',  ( 7.250000000000005329, -7.449999999999998401, -21.50000000000000000 ) ) ;
#49110 = ORIENTED_EDGE ( 'NONE', *, *, #52076, .T. ) ;
#49111 = CARTESIAN_POINT ( 'NONE',  ( 5.257023737882819070, -5.257023737882815517, 26.00000000000000711 ) ) ;
#49112 = AXIS2_PLACEMENT_3D ( 'NONE', #37817, #17273, #5983 ) ;
#49113 = LINE ( 'NONE', #33537, #55864 ) ;
#49114 = CIRCLE ( 'NONE', #26511, 1.399999999999998579 ) ;
#49115 = CARTESIAN_POINT ( 'NONE',  ( -9.390476262117260831, 0.9414762621171833823, 54.00000000000000711 ) ) ;
#49116 = EDGE_LOOP ( 'NONE', ( #50857, #58556, #26891, #3586 ) ) ;
#49117 = ORIENTED_EDGE ( 'NONE', *, *, #20670, .T. ) ;
#49118 = CARTESIAN_POINT ( 'NONE',  ( -6.822336235477446387, -4.149127210878696737, 54.00000000000000711 ) ) ;
#49119 = ORIENTED_EDGE ( 'NONE', *, *, #11687, .T. ) ;
#49120 = ORIENTED_EDGE ( 'NONE', *, *, #1072, .F. ) ;
#49121 = EDGE_CURVE ( 'NONE', #61094, #69579, #19782, .T. ) ;
#49122 = DIRECTION ( 'NONE',  ( -0.7071067811865513475, -0.7071067811865435759, 0.000000000000000000 ) ) ;
#49123 = DIRECTION ( 'NONE',  ( 0.000000000000000000, 0.000000000000000000, 1.000000000000000000 ) ) ;
#49124 = AXIS2_PLACEMENT_3D ( 'NONE', #18548, #60651, #50725 ) ;
#49125 = CARTESIAN_POINT ( 'NONE',  ( 9.690000000000001279, -9.750000000000001776, -7.000000000000000000 ) ) ;
#49126 = EDGE_CURVE ( 'NONE', #59026, #59587, #40674, .T. ) ;
#49127 = VECTOR ( 'NONE', #22033, 1000.000000000000000 ) ;
#49128 = ADVANCED_FACE ( 'NONE', ( #9193 ), #52329, .F. ) ;
#49129 = VERTEX_POINT ( 'NONE', #14851 ) ;
#49130 = CIRCLE ( 'NONE', #53685, 24.99999999998784972 ) ;
#49131 = CARTESIAN_POINT ( 'NONE',  ( -29.25000000000000000, -5.200000000000001066, -11.75000000000000000 ) ) ;
#49133 = DIRECTION ( 'NONE',  ( 0.000000000000000000, 1.000000000000000000, 0.000000000000000000 ) ) ;
#49132 = LINE ( 'NONE', #42780, #529 ) ;
#49134 = ORIENTED_EDGE ( 'NONE', *, *, #15677, .T. ) ;
#49135 = ORIENTED_EDGE ( 'NONE', *, *, #31560, .T. ) ;
#49138 = ORIENTED_EDGE ( 'NONE', *, *, #22821, .F. ) ;
#49137 = ADVANCED_FACE ( 'NONE', ( #24399 ), #67545, .F. ) ;
#49136 = CARTESIAN_POINT ( 'NONE',  ( 15.50000000000000000, 0.000000000000000000, -22.50000000000000000 ) ) ;
#49139 = ORIENTED_EDGE ( 'NONE', *, *, #48465, .F. ) ;
#49140 = EDGE_CURVE ( 'NONE', #28197, #68445, #17569, .T. ) ;
#49141 = EDGE_CURVE ( 'NONE', #8140, #47285, #60710, .T. ) ;
#49142 = CARTESIAN_POINT ( 'NONE',  ( -6.817976262117327657, -9.912023737882785568, 54.00000000000000711 ) ) ;
#49143 = CIRCLE ( 'NONE', #63233, 0.5999999999999989786 ) ;
#49144 = EDGE_CURVE ( 'NONE', #31847, #47032, #2695, .T. ) ;
#49145 = CARTESIAN_POINT ( 'NONE',  ( -8.227189898828745740, 1.620245201994245487, 54.00000000000000711 ) ) ;
#49146 = ORIENTED_EDGE ( 'NONE', *, *, #9658, .F. ) ;
#49147 = ORIENTED_EDGE ( 'NONE', *, *, #26980, .F. ) ;
#49148 = CARTESIAN_POINT ( 'NONE',  ( 0.000000000000000000, 0.000000000000000000, -15.00000000000000000 ) ) ;
#49149 = CARTESIAN_POINT ( 'NONE',  ( 29.50000000000000355, -12.00000000000000000, 11.03137303340310282 ) ) ;
#49150 = CIRCLE ( 'NONE', #66034, 0.2000000000000000944 ) ;
#49151 = ORIENTED_EDGE ( 'NONE', *, *, #15280, .T. ) ;
#49152 = DIRECTION ( 'NONE',  ( 0.000000000000000000, 1.000000000000000000, 0.000000000000000000 ) ) ;
#49153 = DIRECTION ( 'NONE',  ( 0.000000000000000000, 1.000000000000000000, 0.000000000000000000 ) ) ;
#49154 = AXIS2_PLACEMENT_3D ( 'NONE', #55107, #55784, #39178 ) ;
#49155 = PLANE ( 'NONE',  #31695 ) ;
#49156 = ORIENTED_EDGE ( 'NONE', *, *, #44484, .F. ) ;
#49157 = VECTOR ( 'NONE', #32459, 1000.000000000000000 ) ;
#49158 = CIRCLE ( 'NONE', #8455, 0.2000000000000005107 ) ;
#49159 = DIRECTION ( 'NONE',  ( -0.4998444328988824181, 0.000000000000000000, 0.8661152018640445593 ) ) ;
#49160 = ADVANCED_FACE ( 'NONE', ( #51142 ), #12254, .F. ) ;
#49161 = DIRECTION ( 'NONE',  ( 1.000000000000000000, 0.000000000000000000, -0.000000000000000000 ) ) ;
#49163 = VERTEX_POINT ( 'NONE', #6957 ) ;
#49162 = DIRECTION ( 'NONE',  ( 0.000000000000000000, -1.000000000000000000, 0.000000000000000000 ) ) ;
#49165 = ORIENTED_EDGE ( 'NONE', *, *, #64880, .T. ) ;
#49164 = PLANE ( 'NONE',  #26742 ) ;
#49166 = CARTESIAN_POINT ( 'NONE',  ( 30.00000000000000000, -12.00000000000000000, -12.20000000000000107 ) ) ;
#49167 = CIRCLE ( 'NONE', #19767, 0.2000000000000005107 ) ;
#49168 = AXIS2_PLACEMENT_3D ( 'NONE', #64528, #4085, #63475 ) ;
#49169 = DIRECTION ( 'NONE',  ( 1.000000000000000000, -0.000000000000000000, -0.000000000000000000 ) ) ;
#49170 = DIRECTION ( 'NONE',  ( 0.000000000000000000, 0.000000000000000000, 1.000000000000000000 ) ) ;
#49171 = CARTESIAN_POINT ( 'NONE',  ( 275.0000000000000000, -39.79999999999954952, -8.900000000000419575 ) ) ;
#49172 = EDGE_CURVE ( 'NONE', #51726, #25149, #55156, .T. ) ;
#49173 = CARTESIAN_POINT ( 'NONE',  ( -8.821682069070780230, 8.130476262117182884, 54.00000000000000711 ) ) ;
#49174 = CARTESIAN_POINT ( 'NONE',  ( 0.000000000000000000, 0.000000000000000000, -30.00000000000001066 ) ) ;
#49175 = ORIENTED_EDGE ( 'NONE', *, *, #3136, .F. ) ;
#49176 = FACE_OUTER_BOUND ( 'NONE', #38345, .T. ) ;
#49178 = VERTEX_POINT ( 'NONE', #67054 ) ;
#49177 = DIRECTION ( 'NONE',  ( -1.000000000000000000, 0.000000000000000000, 0.000000000000000000 ) ) ;
#49180 = ORIENTED_EDGE ( 'NONE', *, *, #64530, .T. ) ;
#49179 = LINE ( 'NONE', #66468, #61493 ) ;
#49181 = AXIS2_PLACEMENT_3D ( 'NONE', #17511, #49367, #935 ) ;
#49182 = CARTESIAN_POINT ( 'NONE',  ( -8.693516549646709279, 11.11351654964659907, 455.0000000000000568 ) ) ;
#49183 = AXIS2_PLACEMENT_3D ( 'NONE', #25878, #46375, #36472 ) ;
#49184 = CARTESIAN_POINT ( 'NONE',  ( -7.250000000000000888, 7.250000000000001776, -10.00000000000000000 ) ) ;
#49185 = ORIENTED_EDGE ( 'NONE', *, *, #38202, .T. ) ;
#49186 = LINE ( 'NONE', #6726, #9432 ) ;
#49187 = DIRECTION ( 'NONE',  ( 0.000000000000000000, 0.000000000000000000, -1.000000000000000000 ) ) ;
#49188 = EDGE_LOOP ( 'NONE', ( #57842, #41661, #19513, #2777 ) ) ;
#49189 = CARTESIAN_POINT ( 'NONE',  ( 7.000000000000000000, -25.50000000000000355, 14.74860679774999994 ) ) ;
#49190 = CARTESIAN_POINT ( 'NONE',  ( -8.250000000000000000, 7.250000000000001776, -7.500000000000000000 ) ) ;
#49191 =( NAMED_UNIT ( * ) PLANE_ANGLE_UNIT ( ) SI_UNIT ( $, .RADIAN. ) );
#49192 = EDGE_CURVE ( 'NONE', #65388, #35918, #21359, .T. ) ;
#49193 = CARTESIAN_POINT ( 'NONE',  ( 9.306483450353415066, 10.08346604330773744, 455.0000000000000568 ) ) ;
#49194 = CARTESIAN_POINT ( 'NONE',  ( 3.006483450353369502, -7.428221114745093168, 455.0000000000000568 ) ) ;
#49195 = ORIENTED_EDGE ( 'NONE', *, *, #52380, .T. ) ;
#49196 = CARTESIAN_POINT ( 'NONE',  ( 30.00000000000000000, -11.50000000000100009, 15.00000000000084910 ) ) ;
#49197 = ORIENTED_EDGE ( 'NONE', *, *, #35938, .F. ) ;
#49198 = EDGE_CURVE ( 'NONE', #64226, #33306, #7996, .T. ) ;
#49199 = ORIENTED_EDGE ( 'NONE', *, *, #66324, .F. ) ;
#49200 = EDGE_CURVE ( 'NONE', #21581, #56475, #39822, .T. ) ;
#49201 = DIRECTION ( 'NONE',  ( -1.000000000000000000, 1.813998472013049822E-14, -1.836970198720996654E-16 ) ) ;
#49202 = DIRECTION ( 'NONE',  ( -1.000000000000000000, 3.491481338843133355E-15, 1.836970198721036344E-16 ) ) ;
#49203 = EDGE_CURVE ( 'NONE', #42601, #48598, #55753, .T. ) ;
#49204 = EDGE_CURVE ( 'NONE', #34259, #41478, #25908, .T. ) ;
#49205 = ADVANCED_FACE ( 'NONE', ( #56791 ), #23571, .F. ) ;
#49206 = CARTESIAN_POINT ( 'NONE',  ( 11.12648345035335851, 7.793516549646610336, 195.0000000000000284 ) ) ;
#49207 = VECTOR ( 'NONE', #60995, 1000.000000000000000 ) ;
#49208 = DIRECTION ( 'NONE',  ( 0.000000000000000000, 0.000000000000000000, 1.000000000000000000 ) ) ;
#49209 = EDGE_LOOP ( 'NONE', ( #23726, #54946, #11948, #33562 ) ) ;
#49210 = ORIENTED_EDGE ( 'NONE', *, *, #5404, .T. ) ;
#49212 = VERTEX_POINT ( 'NONE', #1323 ) ;
#49211 = PLANE ( 'NONE',  #9188 ) ;
#49213 = ADVANCED_FACE ( 'NONE', ( #13312 ), #44429, .T. ) ;
#49214 = ORIENTED_EDGE ( 'NONE', *, *, #56331, .T. ) ;
#49215 = AXIS2_PLACEMENT_3D ( 'NONE', #46100, #25946, #10028 ) ;
#49216 = AXIS2_PLACEMENT_3D ( 'NONE', #15444, #58582, #10136 ) ;
#49217 = AXIS2_PLACEMENT_3D ( 'NONE', #51666, #57664, #63322 ) ;
#49218 = LINE ( 'NONE', #12058, #63128 ) ;
#49219 = CARTESIAN_POINT ( 'NONE',  ( 39.00000000000000000, -16.96999999999999886, -21.00000000000000000 ) ) ;
#49220 = EDGE_CURVE ( 'NONE', #21056, #5435, #13466, .T. ) ;
#49221 = DIRECTION ( 'NONE',  ( 1.836970198721029934E-16, -1.836970198721036344E-16, 1.000000000000000000 ) ) ;
#49222 = EDGE_CURVE ( 'NONE', #8535, #19822, #35211, .T. ) ;
#49223 = DIRECTION ( 'NONE',  ( 0.000000000000000000, 1.000000000000000000, 0.000000000000000000 ) ) ;
#49224 = CIRCLE ( 'NONE', #58250, 0.3499999999999611200 ) ;
#49225 = VECTOR ( 'NONE', #66750, 1000.000000000000000 ) ;
#49226 = AXIS2_PLACEMENT_3D ( 'NONE', #64358, #63668, #42779 ) ;
#49228 = CARTESIAN_POINT ( 'NONE',  ( -4.383466043307859827, 8.393516549646591329, 455.0000000000000568 ) ) ;
#49227 = CARTESIAN_POINT ( 'NONE',  ( 33.89999999999999858, -21.00000000000000000, 13.86939075806900057 ) ) ;
#49229 = VERTEX_POINT ( 'NONE', #56440 ) ;
#49231 = ORIENTED_EDGE ( 'NONE', *, *, #47593, .F. ) ;
#49230 = CARTESIAN_POINT ( 'NONE',  ( 283.0000000000000568, -42.00000000000000000, -15.00000000000000000 ) ) ;
#49232 = ORIENTED_EDGE ( 'NONE', *, *, #61435, .T. ) ;
#49233 = ORIENTED_EDGE ( 'NONE', *, *, #12348, .F. ) ;
#49234 = VECTOR ( 'NONE', #33485, 1000.000000000000000 ) ;
#49235 = DIRECTION ( 'NONE',  ( 0.000000000000000000, -1.000000000000000000, 0.000000000000000000 ) ) ;
#49236 = EDGE_CURVE ( 'NONE', #5474, #7017, #27057, .T. ) ;
#49237 = CARTESIAN_POINT ( 'NONE',  ( 30.00000000000000000, -4.000000000000000000, 26.25000000000000000 ) ) ;
#49238 = ADVANCED_FACE ( 'NONE', ( #29211 ), #24785, .T. ) ;
#49239 = VECTOR ( 'NONE', #64665, 1000.000000000000000 ) ;
#49240 = DIRECTION ( 'NONE',  ( 1.836970198721029934E-16, 1.836970198721010706E-16, -1.000000000000000000 ) ) ;
#49241 = DIRECTION ( 'NONE',  ( 0.000000000000000000, 0.000000000000000000, 1.000000000000000000 ) ) ;
#49242 = ORIENTED_EDGE ( 'NONE', *, *, #61402, .T. ) ;
#49243 = ORIENTED_EDGE ( 'NONE', *, *, #16860, .T. ) ;
#49244 = CARTESIAN_POINT ( 'NONE',  ( 18.89999999999999858, 20.60000000000000142, -13.86939075806900057 ) ) ;
#49245 = CARTESIAN_POINT ( 'NONE',  ( -4.393516549646671265, 11.31351654964658771, 455.0000000000000568 ) ) ;
#49246 = ORIENTED_EDGE ( 'NONE', *, *, #56515, .T. ) ;
#49247 = ORIENTED_EDGE ( 'NONE', *, *, #34594, .T. ) ;
#49248 = DIRECTION ( 'NONE',  ( -1.836970198721029934E-16, -1.836970198721010706E-16, 1.000000000000000000 ) ) ;
#49249 = FACE_OUTER_BOUND ( 'NONE', #57440, .T. ) ;
#49250 = EDGE_LOOP ( 'NONE', ( #23192, #69321, #69095, #62484 ) ) ;
#49251 = CARTESIAN_POINT ( 'NONE',  ( 20.90000000000000213, 13.66939075806899950, 20.80000000000000426 ) ) ;
#49252 = COLOUR_RGB ( '', 0.31764706, 0.68627451, 0.89019608) ;
#49254 = ORIENTED_EDGE ( 'NONE', *, *, #23866, .F. ) ;
#49253 = DIRECTION ( 'NONE',  ( 1.224646799147353207E-16, 1.000000000000000000, -0.000000000000000000 ) ) ;
#49255 = ORIENTED_EDGE ( 'NONE', *, *, #6572, .T. ) ;
#49256 = DIRECTION ( 'NONE',  ( -0.000000000000000000, -0.000000000000000000, -1.000000000000000000 ) ) ;
#49257 = LINE ( 'NONE', #21337, #39101 ) ;
#49258 = AXIS2_PLACEMENT_3D ( 'NONE', #5550, #1280, #64946 ) ;
#49259 = CARTESIAN_POINT ( 'NONE',  ( -4.947141984184481700, 7.342976262117180575, 26.00000000000000711 ) ) ;
#49260 = FACE_OUTER_BOUND ( 'NONE', #21246, .T. ) ;
#49261 = EDGE_CURVE ( 'NONE', #54522, #53050, #23923, .T. ) ;
#49262 = DIRECTION ( 'NONE',  ( 0.000000000000000000, 0.000000000000000000, -1.000000000000000000 ) ) ;
#49263 = AXIS2_PLACEMENT_3D ( 'NONE', #47206, #21720, #28067 ) ;
#49264 = ORIENTED_EDGE ( 'NONE', *, *, #34273, .F. ) ;
#49265 = CARTESIAN_POINT ( 'NONE',  ( -4.135079735113208699, -3.677663764522613121, 54.00000000000000711 ) ) ;
#49266 = EDGE_CURVE ( 'NONE', #25825, #6078, #8346, .T. ) ;
#49268 = ORIENTED_EDGE ( 'NONE', *, *, #60072, .F. ) ;
#49267 = CARTESIAN_POINT ( 'NONE',  ( 7.357023737882817827, -3.848229544836335947, 26.00000000000000711 ) ) ;
#49269 = VECTOR ( 'NONE', #33670, 1000.000000000000000 ) ;
#49270 = AXIS2_PLACEMENT_3D ( 'NONE', #23349, #1098, #60818 ) ;
#49272 = LINE ( 'NONE', #15349, #67119 ) ;
#49271 = AXIS2_PLACEMENT_3D ( 'NONE', #57232, #47322, #41308 ) ;
#49273 = LINE ( 'NONE', #11422, #36896 ) ;
#49275 = EDGE_CURVE ( 'NONE', #11123, #9064, #14005, .T. ) ;
#49274 = CARTESIAN_POINT ( 'NONE',  ( -3.834182069070824816, -7.532023737882819425, 54.00000000000000711 ) ) ;
#49276 = CYLINDRICAL_SURFACE ( 'NONE', #26168, 0.1999999999999987899 ) ;
#49277 = CIRCLE ( 'NONE', #51525, 0.1749999999999998224 ) ;
#49278 = CIRCLE ( 'NONE', #1805, 0.3499999999999996447 ) ;
#49279 = CARTESIAN_POINT ( 'NONE',  ( 8.900000000000002132, 0.000000000000000000, 0.000000000000000000 ) ) ;
#49280 = ADVANCED_FACE ( 'NONE', ( #3756 ), #47594, .T. ) ;
#49281 = ORIENTED_EDGE ( 'NONE', *, *, #3314, .F. ) ;
#49282 = ORIENTED_EDGE ( 'NONE', *, *, #51981, .F. ) ;
#49283 = AXIS2_PLACEMENT_3D ( 'NONE', #18886, #55661, #13574 ) ;
#49284 = FACE_OUTER_BOUND ( 'NONE', #32758, .T. ) ;
#49285 = EDGE_CURVE ( 'NONE', #14752, #5450, #3409, .T. ) ;
#49286 = DIRECTION ( 'NONE',  ( 0.000000000000000000, 0.000000000000000000, 1.000000000000000000 ) ) ;
#49287 = CIRCLE ( 'NONE', #33473, 5.000000000000000000 ) ;
#49288 = EDGE_LOOP ( 'NONE', ( #155, #39213, #61926, #5329 ) ) ;
#49289 = CYLINDRICAL_SURFACE ( 'NONE', #24833, 4.500000000000188294 ) ;
#49290 = CARTESIAN_POINT ( 'NONE',  ( -8.249999999999996447, -7.848062532927998269, -1.000000000000000000 ) ) ;
#49291 = ADVANCED_FACE ( 'NONE', ( #57496 ), #9062, .F. ) ;
#49292 = EDGE_LOOP ( 'NONE', ( #49926, #29247, #55846, #38137 ) ) ;
#49293 = EDGE_CURVE ( 'NONE', #36081, #14970, #23598, .T. ) ;
#49294 = CARTESIAN_POINT ( 'NONE',  ( -4.734785091273957747, 6.606374702650051667, 195.0000000000000284 ) ) ;
#49295 = CYLINDRICAL_SURFACE ( 'NONE', #30811, 1.000000000000001776 ) ;
#49296 = ORIENTED_EDGE ( 'NONE', *, *, #10773, .T. ) ;
#49297 = DIRECTION ( 'NONE',  ( 1.000000000000000000, 0.000000000000000000, 0.000000000000000000 ) ) ;
#49298 = DIRECTION ( 'NONE',  ( 0.8660254037844510311, 0.4999999999999785727, 1.836970198720951294E-16 ) ) ;
#49299 = EDGE_CURVE ( 'NONE', #5817, #25935, #22513, .T. ) ;
#49300 = EDGE_CURVE ( 'NONE', #37343, #28935, #31355, .T. ) ;
#49301 = LINE ( 'NONE', #43971, #6891 ) ;
#49302 = VERTEX_POINT ( 'NONE', #68106 ) ;
#49304 = EDGE_LOOP ( 'NONE', ( #20026, #41315 ) ) ;
#49303 = CARTESIAN_POINT ( 'NONE',  ( 111.9257688011041836, 10.00000000000000000, 281.4830310981151911 ) ) ;
#49305 = EDGE_CURVE ( 'NONE', #17555, #46800, #69162, .T. ) ;
#49306 = CARTESIAN_POINT ( 'NONE',  ( 6.344579767990823349, -8.406483450353491094, 455.0000000000000568 ) ) ;
#49307 = CARTESIAN_POINT ( 'NONE',  ( 4.720772854004775532, -4.155633711806670405, 26.00000000000000711 ) ) ;
#49308 = CARTESIAN_POINT ( 'NONE',  ( -11.00000000000000000, -11.50000000000100009, -15.00000000000084910 ) ) ;
#49309 = ORIENTED_EDGE ( 'NONE', *, *, #36371, .F. ) ;
#49310 = VECTOR ( 'NONE', #2894, 1000.000000000000000 ) ;
#49311 = DIRECTION ( 'NONE',  ( 1.000000000000000000, -3.491481338843132961E-15, -1.836970198721036344E-16 ) ) ;
#49312 = FACE_OUTER_BOUND ( 'NONE', #69679, .T. ) ;
#49313 = CIRCLE ( 'NONE', #33490, 0.5999999999999989786 ) ;
#49314 = VERTEX_POINT ( 'NONE', #68814 ) ;
#49315 = EDGE_LOOP ( 'NONE', ( #9409, #14425 ) ) ;
#49316 = VECTOR ( 'NONE', #53782, 1000.000000000000000 ) ;
#49317 = ORIENTED_EDGE ( 'NONE', *, *, #7941, .T. ) ;
#49318 = LINE ( 'NONE', #49980, #2770 ) ;
#49319 = ADVANCED_FACE ( 'NONE', ( #19655 ), #20371, .F. ) ;
#49320 = CARTESIAN_POINT ( 'NONE',  ( -11.18999999999999950, 11.18999999999999950, 0.000000000000000000 ) ) ;
#49321 = CYLINDRICAL_SURFACE ( 'NONE', #20219, 1.000000000000000000 ) ;
#49322 = EDGE_CURVE ( 'NONE', #26913, #60006, #47341, .T. ) ;
#49323 = CIRCLE ( 'NONE', #66258, 1.000000000000000000 ) ;
#49324 = AXIS2_PLACEMENT_3D ( 'NONE', #36312, #29243, #9094 ) ;
#49325 = VECTOR ( 'NONE', #48454, 1000.000000000000000 ) ;
#49326 = ORIENTED_EDGE ( 'NONE', *, *, #18988, .T. ) ;
#49327 = VERTEX_POINT ( 'NONE', #35939 ) ;
#49328 = ORIENTED_EDGE ( 'NONE', *, *, #69182, .F. ) ;
#49329 = CARTESIAN_POINT ( 'NONE',  ( -8.393516549646792058, -7.616533956692236096, 455.0000000000000568 ) ) ;
#49330 = AXIS2_PLACEMENT_3D ( 'NONE', #52533, #68446, #35544 ) ;
#49331 = ORIENTED_EDGE ( 'NONE', *, *, #69892, .F. ) ;
#49332 = VERTEX_POINT ( 'NONE', #42281 ) ;
#49333 = VERTEX_POINT ( 'NONE', #68466 ) ;
#49334 = ORIENTED_EDGE ( 'NONE', *, *, #27331, .F. ) ;
#49335 = CIRCLE ( 'NONE', #8630, 1.929199999999998916 ) ;
#49336 = FACE_OUTER_BOUND ( 'NONE', #29128, .T. ) ;
#49338 = ORIENTED_EDGE ( 'NONE', *, *, #44266, .F. ) ;
#49337 = CARTESIAN_POINT ( 'NONE',  ( -3.417780618358722933, -7.852485183457003970, 455.0000000000000568 ) ) ;
#49339 = CARTESIAN_POINT ( 'NONE',  ( 7.250000000000005329, -7.249999999999998224, -7.000000000000000000 ) ) ;
#49340 = AXIS2_PLACEMENT_3D ( 'NONE', #19934, #68024, #36916 ) ;
#49341 = PLANE ( 'NONE',  #62239 ) ;
#49342 = DIRECTION ( 'NONE',  ( 0.000000000000000000, 0.000000000000000000, 1.000000000000000000 ) ) ;
#49343 = ORIENTED_EDGE ( 'NONE', *, *, #60643, .F. ) ;
#49344 = CARTESIAN_POINT ( 'NONE',  ( -7.450000000000001954, -7.249999999999998224, -10.50000000000000000 ) ) ;
#49345 = LINE ( 'NONE', #548, #66160 ) ;
#49346 = ORIENTED_EDGE ( 'NONE', *, *, #12640, .F. ) ;
#49347 = DIRECTION ( 'NONE',  ( 1.000000000000000000, 0.000000000000000000, 0.000000000000000000 ) ) ;
#49348 = ADVANCED_FACE ( 'NONE', ( #47253 ), #3068, .F. ) ;
#49349 = LINE ( 'NONE', #44020, #24173 ) ;
#49350 = DIRECTION ( 'NONE',  ( -1.000000000000000000, 0.000000000000000000, 0.000000000000000000 ) ) ;
#49351 = VECTOR ( 'NONE', #24386, 1000.000000000000000 ) ;
#49352 = VERTEX_POINT ( 'NONE', #20025 ) ;
#49354 = EDGE_CURVE ( 'NONE', #29693, #68454, #14580, .T. ) ;
#49353 = LINE ( 'NONE', #55011, #23415 ) ;
#49355 = FACE_OUTER_BOUND ( 'NONE', #13388, .T. ) ;
#49356 = AXIS2_PLACEMENT_3D ( 'NONE', #42720, #64300, #58299 ) ;
#49357 = DIRECTION ( 'NONE',  ( 0.000000000000000000, 1.000000000000000000, 0.000000000000000000 ) ) ;
#49358 = EDGE_CURVE ( 'NONE', #63961, #62878, #57846, .T. ) ;
#49359 = EDGE_CURVE ( 'NONE', #21251, #32793, #30981, .T. ) ;
#49360 = AXIS2_PLACEMENT_3D ( 'NONE', #31794, #20127, #46638 ) ;
#49361 = VECTOR ( 'NONE', #37774, 1000.000000000000000 ) ;
#49362 = DIRECTION ( 'NONE',  ( 0.000000000000000000, -3.673940397442059868E-16, 1.000000000000000000 ) ) ;
#49363 = EDGE_CURVE ( 'NONE', #18151, #41573, #15072, .T. ) ;
#49364 = DIRECTION ( 'NONE',  ( 1.000000000000000000, -8.728482790395504563E-15, -3.206792553201184024E-30 ) ) ;
#49365 = EDGE_CURVE ( 'NONE', #43945, #40050, #10458, .T. ) ;
#49366 = PLANE ( 'NONE',  #45187 ) ;
#49367 = DIRECTION ( 'NONE',  ( -0.000000000000000000, -0.000000000000000000, -1.000000000000000000 ) ) ;
#49368 = CARTESIAN_POINT ( 'NONE',  ( -7.450000000000001954, 0.000000000000000000, -16.00000000000000000 ) ) ;
#49369 = AXIS2_PLACEMENT_3D ( 'NONE', #27710, #65876, #17433 ) ;
#49370 = VECTOR ( 'NONE', #23835, 1000.000000000000000 ) ;
#49371 = AXIS2_PLACEMENT_3D ( 'NONE', #4373, #63049, #69397 ) ;
#49372 = VERTEX_POINT ( 'NONE', #28710 ) ;
#49373 = DIRECTION ( 'NONE',  ( 0.000000000000000000, 1.000000000000000000, 0.000000000000000000 ) ) ;
#49374 = DIRECTION ( 'NONE',  ( -1.000000000000000000, 0.000000000000000000, 0.000000000000000000 ) ) ;
#49375 = AXIS2_PLACEMENT_3D ( 'NONE', #26046, #5176, #10125 ) ;
#49376 = DIRECTION ( 'NONE',  ( 8.339399738404099512E-15, 1.000000000000000000, 1.836970198721025990E-16 ) ) ;
#49377 = AXIS2_PLACEMENT_3D ( 'NONE', #68956, #31838, #53402 ) ;
#49378 = DIRECTION ( 'NONE',  ( 0.000000000000000000, 1.000000000000000000, 0.000000000000000000 ) ) ;
#49379 = ORIENTED_EDGE ( 'NONE', *, *, #36245, .T. ) ;
#49380 = DIRECTION ( 'NONE',  ( 0.000000000000000000, 0.000000000000000000, 1.000000000000000000 ) ) ;
#49381 = LINE ( 'NONE', #11862, #22600 ) ;
#49382 = LINE ( 'NONE', #49706, #7383 ) ;
#49383 = AXIS2_PLACEMENT_3D ( 'NONE', #4212, #57930, #21500 ) ;
#49384 = CARTESIAN_POINT ( 'NONE',  ( 7.250000000000005329, 7.250000000000000888, -22.50000000000000000 ) ) ;
#49385 = DIRECTION ( 'NONE',  ( -1.000000000000000000, 0.000000000000000000, 0.000000000000000000 ) ) ;
#49386 = ORIENTED_EDGE ( 'NONE', *, *, #55993, .T. ) ;
#49387 = ORIENTED_EDGE ( 'NONE', *, *, #36563, .F. ) ;
#49388 = DIRECTION ( 'NONE',  ( 0.000000000000000000, -0.7071067811865475727, -0.7071067811865475727 ) ) ;
#49389 = DIRECTION ( 'NONE',  ( -0.000000000000000000, 3.673940397442059868E-16, -1.000000000000000000 ) ) ;
#49390 = ORIENTED_EDGE ( 'NONE', *, *, #45949, .T. ) ;
#49391 = LINE ( 'NONE', #39109, #20582 ) ;
#49392 = ORIENTED_EDGE ( 'NONE', *, *, #35205, .T. ) ;
#49393 = DIRECTION ( 'NONE',  ( 0.000000000000000000, 0.000000000000000000, 1.000000000000000000 ) ) ;
#49394 = VERTEX_POINT ( 'NONE', #32038 ) ;
#49395 = VERTEX_POINT ( 'NONE', #50279 ) ;
#49396 = CARTESIAN_POINT ( 'NONE',  ( 4.456444791733522252E-16, 7.450000000000002842, -18.00000000000000000 ) ) ;
#49397 = ORIENTED_EDGE ( 'NONE', *, *, #50259, .T. ) ;
#49398 = DIRECTION ( 'NONE',  ( 0.000000000000000000, 0.7071067811865474617, -0.7071067811865474617 ) ) ;
#49399 = CARTESIAN_POINT ( 'NONE',  ( 4.456444791733522252E-16, 7.450000000000002842, -15.00000000000000000 ) ) ;
#49401 = ADVANCED_FACE ( 'NONE', ( #44972 ), #17764, .F. ) ;
#49400 = FACE_OUTER_BOUND ( 'NONE', #27380, .T. ) ;
#49402 = AXIS2_PLACEMENT_3D ( 'NONE', #30564, #67693, #12879 ) ;
#49403 = ORIENTED_EDGE ( 'NONE', *, *, #26635, .T. ) ;
#49405 = EDGE_CURVE ( 'NONE', #62698, #46179, #17996, .T. ) ;
#49404 = EDGE_LOOP ( 'NONE', ( #57138, #65086, #42105, #2559 ) ) ;
#49406 = CARTESIAN_POINT ( 'NONE',  ( -10.08346604330783336, -2.706483450353306175, 195.0000000000000284 ) ) ;
#49407 = DIRECTION ( 'NONE',  ( 0.000000000000000000, -0.000000000000000000, 1.000000000000000000 ) ) ;
#49408 = ORIENTED_EDGE ( 'NONE', *, *, #21945, .T. ) ;
#49409 = VERTEX_POINT ( 'NONE', #60543 ) ;
#49410 = ORIENTED_EDGE ( 'NONE', *, *, #42234, .F. ) ;
#49411 = AXIS2_PLACEMENT_3D ( 'NONE', #57349, #60649, #8548 ) ;
#49412 = AXIS2_PLACEMENT_3D ( 'NONE', #21073, #21773, #64222 ) ;
#49413 = DIRECTION ( 'NONE',  ( 1.000000000000000000, 0.000000000000000000, 0.000000000000000000 ) ) ;
#49415 = ORIENTED_EDGE ( 'NONE', *, *, #62598, .T. ) ;
#49414 = LINE ( 'NONE', #53678, #53342 ) ;
#49416 = VECTOR ( 'NONE', #5727, 1000.000000000000000 ) ;
#49417 = VECTOR ( 'NONE', #22027, 1000.000000000000000 ) ;
#49418 = DIRECTION ( 'NONE',  ( 1.000000000000000000, 0.000000000000000000, 0.000000000000000000 ) ) ;
#49419 = FACE_OUTER_BOUND ( 'NONE', #65728, .T. ) ;
#49420 = ORIENTED_EDGE ( 'NONE', *, *, #40759, .F. ) ;
#49421 = ORIENTED_EDGE ( 'NONE', *, *, #20903, .T. ) ;
#49422 = EDGE_LOOP ( 'NONE', ( #3416, #55392 ) ) ;
#49423 = AXIS2_PLACEMENT_3D ( 'NONE', #51423, #67687, #63086 ) ;
#49424 = VECTOR ( 'NONE', #41993, 1000.000000000000000 ) ;
#49425 = EDGE_LOOP ( 'NONE', ( #46939, #48796, #63446, #62009 ) ) ;
#49426 = CARTESIAN_POINT ( 'NONE',  ( 7.250000000000004441, 7.450000000000001954, -17.50000000000000000 ) ) ;
#49427 = LINE ( 'NONE', #989, #33510 ) ;
#49428 = ORIENTED_EDGE ( 'NONE', *, *, #22130, .F. ) ;
#49429 = AXIS2_PLACEMENT_3D ( 'NONE', #45141, #61395, #62100 ) ;
#49430 = ADVANCED_FACE ( 'NONE', ( #5166 ), #62014, .F. ) ;
#49431 = CARTESIAN_POINT ( 'NONE',  ( 7.250000000000004441, 7.450000000000001954, -15.50000000000000000 ) ) ;
#49433 = ORIENTED_EDGE ( 'NONE', *, *, #54904, .T. ) ;
#49432 = PRESENTATION_STYLE_ASSIGNMENT (( #54731 ) ) ;
#49434 = ORIENTED_EDGE ( 'NONE', *, *, #42634, .T. ) ;
#49435 = CARTESIAN_POINT ( 'NONE',  ( 4.046023737882794791, 3.142976262117205266, 54.00000000000000711 ) ) ;
#49436 = CARTESIAN_POINT ( 'NONE',  ( 30.00000000000000000, -12.00000000000000000, -11.00000000000000000 ) ) ;
#49437 = LINE ( 'NONE', #11238, #40382 ) ;
#49438 = CARTESIAN_POINT ( 'NONE',  ( -16.33565937784310762, -0.3156604612129118026, 21.53909249377453250 ) ) ;
#49439 = PLANE ( 'NONE',  #64669 ) ;
#49441 = VERTEX_POINT ( 'NONE', #7133 ) ;
#49440 = EDGE_CURVE ( 'NONE', #41070, #58001, #69955, .T. ) ;
#49442 = CARTESIAN_POINT ( 'NONE',  ( 8.250000000000005329, -7.249999999999998224, -14.00000000000000000 ) ) ;
#49443 = EDGE_CURVE ( 'NONE', #29674, #43112, #55591, .T. ) ;
#49444 = FACE_OUTER_BOUND ( 'NONE', #45702, .T. ) ;
#49445 = CARTESIAN_POINT ( 'NONE',  ( 7.249999999999995559, -7.848062532927998269, 5.000000000000000000 ) ) ;
#49446 = SURFACE_STYLE_USAGE ( .BOTH. , #42393 ) ;
#49447 = ADVANCED_FACE ( 'NONE', ( #33672 ), #64217, .T. ) ;
#49448 = STYLED_ITEM ( 'NONE', ( #63447 ), #20943 ) ;
#49449 = CARTESIAN_POINT ( 'NONE',  ( 283.0000000000000568, -42.00000000000000000, 15.00000000000000000 ) ) ;
#49450 = FACE_OUTER_BOUND ( 'NONE', #30190, .T. ) ;
#49451 = CARTESIAN_POINT ( 'NONE',  ( 8.930623737882818602, -8.930623737882855906, 54.00000000000000711 ) ) ;
#49452 = ORIENTED_EDGE ( 'NONE', *, *, #66413, .F. ) ;
#49453 = DIRECTION ( 'NONE',  ( -1.000000000000000000, 0.000000000000000000, 0.000000000000000000 ) ) ;
#49454 = DIRECTION ( 'NONE',  ( 1.000000000000000000, 0.000000000000000000, 0.000000000000000000 ) ) ;
#49455 = ORIENTED_EDGE ( 'NONE', *, *, #44090, .T. ) ;
#49456 = DIRECTION ( 'NONE',  ( 1.000000000000000000, 0.000000000000000000, 0.000000000000000000 ) ) ;
#49457 = DIRECTION ( 'NONE',  ( -1.062075597536821678E-14, -1.000000000000000000, 0.000000000000000000 ) ) ;
#49458 = CARTESIAN_POINT ( 'NONE',  ( -7.250000000000001776, -7.249999999999998224, -26.00000000000001066 ) ) ;
#49459 = DIRECTION ( 'NONE',  ( -1.000000000000000000, 0.000000000000000000, 0.000000000000000000 ) ) ;
#49460 = DIRECTION ( 'NONE',  ( 1.000000000000000000, -0.000000000000000000, -0.000000000000000000 ) ) ;
#49461 = AXIS2_PLACEMENT_3D ( 'NONE', #54428, #10938, #32158 ) ;
#49462 = LINE ( 'NONE', #6320, #12794 ) ;
#49463 = ORIENTED_EDGE ( 'NONE', *, *, #69362, .T. ) ;
#49464 = DIRECTION ( 'NONE',  ( -1.000000000000000000, -3.016910393003147986E-15, -0.000000000000000000 ) ) ;
#49465 = VERTEX_POINT ( 'NONE', #37684 ) ;
#49466 = FACE_OUTER_BOUND ( 'NONE', #21358, .T. ) ;
#49467 = AXIS2_PLACEMENT_3D ( 'NONE', #52273, #35279, #35640 ) ;
#49468 = LINE ( 'NONE', #16605, #24269 ) ;
#49469 = DIRECTION ( 'NONE',  ( -1.000000000000000000, 0.000000000000000000, 0.000000000000000000 ) ) ;
#49470 = ORIENTED_EDGE ( 'NONE', *, *, #32945, .T. ) ;
#49471 = ORIENTED_EDGE ( 'NONE', *, *, #66951, .T. ) ;
#49472 = CARTESIAN_POINT ( 'NONE',  ( 4.149127210878736705, 3.663616288757004291, 26.00000000000000711 ) ) ;
#49473 = EDGE_LOOP ( 'NONE', ( #15285, #45287, #10177, #34523 ) ) ;
#49474 = ORIENTED_EDGE ( 'NONE', *, *, #26721, .T. ) ;
#49475 = AXIS2_PLACEMENT_3D ( 'NONE', #15356, #2999, #57779 ) ;
#49476 = DIRECTION ( 'NONE',  ( 0.000000000000000000, -0.000000000000000000, 1.000000000000000000 ) ) ;
#49477 = LINE ( 'NONE', #38847, #47097 ) ;
#49478 = DIRECTION ( 'NONE',  ( -1.000000000000000000, -2.135044278125301343E-15, 0.000000000000000000 ) ) ;
#49479 = ORIENTED_EDGE ( 'NONE', *, *, #29751, .F. ) ;
#49480 = EDGE_CURVE ( 'NONE', #31236, #32954, #59249, .T. ) ;
#49481 = ADVANCED_FACE ( 'NONE', ( #1491 ), #16115, .F. ) ;
#49482 = LINE ( 'NONE', #1048, #44741 ) ;
#49483 = EDGE_CURVE ( 'NONE', #12124, #26706, #32661, .T. ) ;
#49485 = CARTESIAN_POINT ( 'NONE',  ( -7.252248008019532399, -6.619341603356871495, 455.0000000000000568 ) ) ;
#49484 = DIRECTION ( 'NONE',  ( -0.000000000000000000, 1.000000000000000000, -0.000000000000000000 ) ) ;
#49486 = VERTEX_POINT ( 'NONE', #58566 ) ;
#49488 = ORIENTED_EDGE ( 'NONE', *, *, #56278, .F. ) ;
#49487 = DIRECTION ( 'NONE',  ( -0.000000000000000000, 0.000000000000000000, -1.000000000000000000 ) ) ;
#49489 = ORIENTED_EDGE ( 'NONE', *, *, #45185, .F. ) ;
#49490 = EDGE_CURVE ( 'NONE', #52255, #53184, #18092, .T. ) ;
#49491 = FACE_OUTER_BOUND ( 'NONE', #48753, .T. ) ;
#49492 = CARTESIAN_POINT ( 'NONE',  ( 8.606483450353380249, -7.616533956692230767, 195.0000000000000284 ) ) ;
#49493 = VECTOR ( 'NONE', #60134, 1000.000000000000000 ) ;
#49494 = VERTEX_POINT ( 'NONE', #32388 ) ;
#49495 = ORIENTED_EDGE ( 'NONE', *, *, #31082, .F. ) ;
#49496 = DIRECTION ( 'NONE',  ( 0.000000000000000000, 1.000000000000000000, 0.000000000000000000 ) ) ;
#49497 = CARTESIAN_POINT ( 'NONE',  ( -9.293516549646827940, -10.92648345035338764, 455.0000000000000568 ) ) ;
#49498 = ORIENTED_EDGE ( 'NONE', *, *, #59672, .T. ) ;
#49499 = LINE ( 'NONE', #44174, #13887 ) ;
#49500 = CARTESIAN_POINT ( 'NONE',  ( 283.0000000000000568, -38.64999999999999858, -12.69999999999999929 ) ) ;
#49501 = LINE ( 'NONE', #44515, #36166 ) ;
#49502 = EDGE_LOOP ( 'NONE', ( #10606, #5414, #2385, #20118 ) ) ;
#49503 = AXIS2_PLACEMENT_3D ( 'NONE', #51897, #14764, #46228 ) ;
#49504 = LINE ( 'NONE', #38881, #12029 ) ;
#49505 = CARTESIAN_POINT ( 'NONE',  ( 19.90000000000000213, -0.2000000000089119934, -8.913009219568841313E-12 ) ) ;
#49507 = ORIENTED_EDGE ( 'NONE', *, *, #28035, .F. ) ;
#49506 = LINE ( 'NONE', #1075, #11480 ) ;
#49509 = ORIENTED_EDGE ( 'NONE', *, *, #45486, .T. ) ;
#49508 = DIRECTION ( 'NONE',  ( 1.000000000000000000, -5.981805089575194965E-17, 0.000000000000000000 ) ) ;
#49510 = CARTESIAN_POINT ( 'NONE',  ( 10.00000000000000000, -21.00000000000000000, -18.00000000000000355 ) ) ;
#49511 = VECTOR ( 'NONE', #51595, 1000.000000000000000 ) ;
#49512 = DIRECTION ( 'NONE',  ( -0.000000000000000000, -0.000000000000000000, 1.000000000000000000 ) ) ;
#49513 = CARTESIAN_POINT ( 'NONE',  ( 39.00000000000000000, 21.00000000000000000, -16.96999999999999886 ) ) ;
#49514 = CARTESIAN_POINT ( 'NONE',  ( -7.250000000000000000, -7.449999999999998401, -17.00000000000000000 ) ) ;
#49515 = DIRECTION ( 'NONE',  ( 0.000000000000000000, 0.000000000000000000, 1.000000000000000000 ) ) ;
#49516 = PLANE ( 'NONE',  #3288 ) ;
#49517 = ORIENTED_EDGE ( 'NONE', *, *, #40676, .F. ) ;
#49518 = DIRECTION ( 'NONE',  ( 0.000000000000000000, 0.000000000000000000, -1.000000000000000000 ) ) ;
#49519 = ADVANCED_FACE ( 'NONE', ( #69511 ), #60878, .F. ) ;
#49521 = ORIENTED_EDGE ( 'NONE', *, *, #17405, .F. ) ;
#49520 = CARTESIAN_POINT ( 'NONE',  ( -11.99351654964671354, 7.813516549646603693, 455.0000000000000568 ) ) ;
#49523 = ORIENTED_EDGE ( 'NONE', *, *, #49679, .T. ) ;
#49522 = CARTESIAN_POINT ( 'NONE',  ( 8.835729544836338434, -7.969523737882825642, 54.00000000000000711 ) ) ;
#49524 = LINE ( 'NONE', #32918, #25633 ) ;
#49525 = EDGE_CURVE ( 'NONE', #55726, #5045, #48638, .T. ) ;
#49526 = EDGE_CURVE ( 'NONE', #12501, #66919, #64905, .T. ) ;
#49527 = DIRECTION ( 'NONE',  ( 0.000000000000000000, 0.000000000000000000, 1.000000000000000000 ) ) ;
#49528 = ADVANCED_FACE ( 'NONE', ( #55247 ), #66200, .F. ) ;
#49529 = ORIENTED_EDGE ( 'NONE', *, *, #11056, .T. ) ;
#49530 = DIRECTION ( 'NONE',  ( -1.000000000000000000, 0.000000000000000000, 0.000000000000000000 ) ) ;
#49531 = DIRECTION ( 'NONE',  ( -1.000000000000000000, 0.000000000000000000, 0.000000000000000000 ) ) ;
#49532 = ORIENTED_EDGE ( 'NONE', *, *, #8481, .F. ) ;
#49533 = DIRECTION ( 'NONE',  ( 0.000000000000000000, 0.000000000000000000, -1.000000000000000000 ) ) ;
#49534 = CARTESIAN_POINT ( 'NONE',  ( -5.242976262117259978, 5.242976262117182706, 54.00000000000000711 ) ) ;
#49535 = EDGE_CURVE ( 'NONE', #53820, #63385, #46215, .T. ) ;
#49536 = CARTESIAN_POINT ( 'NONE',  ( 11.00000000000000000, -9.454754784057099570, 17.53999999999999915 ) ) ;
#49537 = ADVANCED_FACE ( 'NONE', ( #57439 ), #30568, .F. ) ;
#49538 = CARTESIAN_POINT ( 'NONE',  ( -10.91351654964680584, -9.306483450353375986, 455.0000000000000568 ) ) ;
#49539 = VERTEX_POINT ( 'NONE', #14655 ) ;
#49540 = CYLINDRICAL_SURFACE ( 'NONE', #13573, 0.5000000000000000000 ) ;
#49541 = ORIENTED_EDGE ( 'NONE', *, *, #49823, .T. ) ;
#49542 = ORIENTED_EDGE ( 'NONE', *, *, #14074, .T. ) ;
#49543 = FACE_BOUND ( 'NONE', #10580, .T. ) ;
#49544 = PLANE ( 'NONE',  #3317 ) ;
#49545 = CIRCLE ( 'NONE', #38306, 3.499999999999999556 ) ;
#49546 = CARTESIAN_POINT ( 'NONE',  ( 2.500000000000000000, 3.061616997868383141E-16, -29.90000000000000924 ) ) ;
#49547 = CARTESIAN_POINT ( 'NONE',  ( 38.90000000000000568, -14.06939075806902117, -20.80000000000000426 ) ) ;
#49548 = ORIENTED_EDGE ( 'NONE', *, *, #29051, .T. ) ;
#49549 = VERTEX_POINT ( 'NONE', #8991 ) ;
#49551 = ORIENTED_EDGE ( 'NONE', *, *, #46609, .T. ) ;
#49550 = CARTESIAN_POINT ( 'NONE',  ( 7.408280051175156977, 6.775514141871323837, 26.00000000000000711 ) ) ;
#49552 = ORIENTED_EDGE ( 'NONE', *, *, #28315, .F. ) ;
#49553 = AXIS2_PLACEMENT_3D ( 'NONE', #37566, #32253, #26957 ) ;
#49554 = DIRECTION ( 'NONE',  ( 0.000000000000000000, 1.000000000000000000, 0.000000000000000000 ) ) ;
#49555 = PLANE ( 'NONE',  #58005 ) ;
#49556 = CARTESIAN_POINT ( 'NONE',  ( 7.826483450353374671, 11.77351654964661876, 195.0000000000000284 ) ) ;
#49557 = AXIS2_PLACEMENT_3D ( 'NONE', #1936, #60965, #38718 ) ;
#49558 = DIRECTION ( 'NONE',  ( 1.000000000000000000, -5.981805089575196197E-17, 0.000000000000000000 ) ) ;
#49560 = CARTESIAN_POINT ( 'NONE',  ( -9.404046420174113408, -1.866219381641437636, 455.0000000000000568 ) ) ;
#49559 = CARTESIAN_POINT ( 'NONE',  ( 4.961189459950039904, -7.357023737882821379, 54.00000000000000711 ) ) ;
#49561 = ORIENTED_EDGE ( 'NONE', *, *, #10170, .T. ) ;
#49563 = EDGE_LOOP ( 'NONE', ( #61223, #11383, #10547, #22688 ) ) ;
#49562 = CARTESIAN_POINT ( 'NONE',  ( -7.517976262117260333, 6.651770455163663165, 54.00000000000000711 ) ) ;
#49564 = EDGE_LOOP ( 'NONE', ( #37112, #35810, #50755, #23163 ) ) ;
#49565 = ORIENTED_EDGE ( 'NONE', *, *, #34637, .F. ) ;
#49566 = AXIS2_PLACEMENT_3D ( 'NONE', #44921, #66484, #18038 ) ;
#49567 = CARTESIAN_POINT ( 'NONE',  ( 283.0000000000000568, -38.65000000000095781, -15.00000000000000000 ) ) ;
#49568 = CYLINDRICAL_SURFACE ( 'NONE', #54714, 0.3499999999999302558 ) ;
#49569 = AXIS2_PLACEMENT_3D ( 'NONE', #18991, #24295, #12620 ) ;
#49570 = CARTESIAN_POINT ( 'NONE',  ( 40.90000000000000568, 20.60000000000000142, -13.86939075806900057 ) ) ;
#49571 = CARTESIAN_POINT ( 'NONE',  ( -8.250000000000001776, 0.000000000000000000, -20.00000000000000000 ) ) ;
#49572 = ORIENTED_EDGE ( 'NONE', *, *, #38021, .F. ) ;
#49573 = ORIENTED_EDGE ( 'NONE', *, *, #6567, .F. ) ;
#49574 = CIRCLE ( 'NONE', #56378, 0.3499999999999308664 ) ;
#49575 = ADVANCED_FACE ( 'NONE', ( #19956 ), #47191, .T. ) ;
#49576 = FACE_BOUND ( 'NONE', #38544, .T. ) ;
#49577 = DIRECTION ( 'NONE',  ( 0.000000000000000000, 0.000000000000000000, 1.000000000000000000 ) ) ;
#49578 = ORIENTED_EDGE ( 'NONE', *, *, #58690, .F. ) ;
#49579 = ORIENTED_EDGE ( 'NONE', *, *, #34864, .T. ) ;
#49580 = DIRECTION ( 'NONE',  ( -2.135044278125299371E-15, 1.000000000000000000, 0.000000000000000000 ) ) ;
#49581 = EDGE_CURVE ( 'NONE', #63059, #60163, #69448, .T. ) ;
#49582 = CARTESIAN_POINT ( 'NONE',  ( -3.834182069070817711, -7.357023737882814274, 26.00000000000000711 ) ) ;
#49583 = ORIENTED_EDGE ( 'NONE', *, *, #2151, .F. ) ;
#49584 = CARTESIAN_POINT ( 'NONE',  ( -8.250000000000001776, 0.000000000000000000, -10.50000000000000000 ) ) ;
#49585 = ADVANCED_FACE ( 'NONE', ( #4757 ), #15365, .T. ) ;
#49587 = VERTEX_POINT ( 'NONE', #35876 ) ;
#49586 = DIRECTION ( 'NONE',  ( 0.000000000000000000, 0.000000000000000000, 1.000000000000000000 ) ) ;
#49588 = ORIENTED_EDGE ( 'NONE', *, *, #16806, .F. ) ;
#49589 = FACE_OUTER_BOUND ( 'NONE', #3943, .T. ) ;
#49590 = DIRECTION ( 'NONE',  ( -1.000000000000000000, 0.000000000000000000, 0.000000000000000000 ) ) ;
#49591 = LINE ( 'NONE', #59522, #2391 ) ;
#49592 = EDGE_CURVE ( 'NONE', #66065, #51967, #9353, .T. ) ;
#49593 = DIRECTION ( 'NONE',  ( -1.000000000000000000, 0.000000000000000000, 0.000000000000000000 ) ) ;
#49594 = VECTOR ( 'NONE', #60605, 1000.000000000000000 ) ;
#49595 = LINE ( 'NONE', #18096, #54235 ) ;
#49596 = ORIENTED_EDGE ( 'NONE', *, *, #60366, .T. ) ;
#49597 = DIRECTION ( 'NONE',  ( 0.000000000000000000, 0.000000000000000000, 1.000000000000000000 ) ) ;
#49598 = VECTOR ( 'NONE', #68336, 1000.000000000000000 ) ;
#49600 = ORIENTED_EDGE ( 'NONE', *, *, #27644, .F. ) ;
#49599 = LINE ( 'NONE', #26385, #35576 ) ;
#49601 = DIRECTION ( 'NONE',  ( 1.000000000000000000, 0.000000000000000000, 0.000000000000000000 ) ) ;
#49602 = PLANE ( 'NONE',  #11966 ) ;
#49603 = EDGE_CURVE ( 'NONE', #67007, #41511, #68403, .T. ) ;
#49604 = CARTESIAN_POINT ( 'NONE',  ( -9.722976262117258628, 3.667976262117184749, 54.00000000000000711 ) ) ;
#49605 = CYLINDRICAL_SURFACE ( 'NONE', #22765, 0.3499999999999996447 ) ;
#49606 = CIRCLE ( 'NONE', #14576, 0.2000000000000005107 ) ;
#49607 = LINE ( 'NONE', #22734, #57438 ) ;
#49608 = ORIENTED_EDGE ( 'NONE', *, *, #60935, .F. ) ;
#49609 = ORIENTED_EDGE ( 'NONE', *, *, #55339, .F. ) ;
#49610 = AXIS2_PLACEMENT_3D ( 'NONE', #1841, #53264, #49931 ) ;
#49611 = DIRECTION ( 'NONE',  ( 1.000000000000000000, -0.000000000000000000, 0.000000000000000000 ) ) ;
#49612 = ADVANCED_FACE ( 'NONE', ( #19599 ), #36942, .F. ) ;
#49613 = CARTESIAN_POINT ( 'NONE',  ( -8.598420958951633608, -1.480523737882746271, 54.00000000000000711 ) ) ;
#49614 = ADVANCED_FACE ( 'NONE', ( #62737 ), #30229, .F. ) ;
#49615 = AXIS2_PLACEMENT_3D ( 'NONE', #36218, #30231, #47193 ) ;
#49616 = ORIENTED_EDGE ( 'NONE', *, *, #30751, .F. ) ;
#49617 = DIRECTION ( 'NONE',  ( 1.000000000000000000, 0.000000000000000000, 0.000000000000000000 ) ) ;
#49618 = VERTEX_POINT ( 'NONE', #47873 ) ;
#49619 = ORIENTED_EDGE ( 'NONE', *, *, #34410, .T. ) ;
#49620 = CARTESIAN_POINT ( 'NONE',  ( 7.250000000000005329, -8.749999999999998224, -30.00000000000001066 ) ) ;
#49621 = CONICAL_SURFACE ( 'NONE', #15765, 6.000000000000005329, 0.1292750040481423779 ) ;
#49622 = DIRECTION ( 'NONE',  ( 0.000000000000000000, 1.000000000000000000, 0.000000000000000000 ) ) ;
#49623 = EDGE_LOOP ( 'NONE', ( #64542, #15989, #41748, #37133 ) ) ;
#49624 = CARTESIAN_POINT ( 'NONE',  ( -11.00000000000000000, -15.46862696659690073, 14.50000000000000000 ) ) ;
#49625 = EDGE_CURVE ( 'NONE', #1811, #18679, #5607, .T. ) ;
#49626 = PLANE ( 'NONE',  #61647 ) ;
#49627 = DIRECTION ( 'NONE',  ( 0.000000000000000000, -0.000000000000000000, 1.000000000000000000 ) ) ;
#49628 = DIRECTION ( 'NONE',  ( 0.000000000000000000, -1.000000000000000000, 0.000000000000000000 ) ) ;
#49629 = ORIENTED_EDGE ( 'NONE', *, *, #38816, .T. ) ;
#49631 = ORIENTED_EDGE ( 'NONE', *, *, #17855, .T. ) ;
#49630 = DIRECTION ( 'NONE',  ( 0.000000000000000000, 0.5000000000000199840, 0.8660254037844271613 ) ) ;
#49632 = DIRECTION ( 'NONE',  ( 1.836970198721029934E-16, -1.836970198721036344E-16, 1.000000000000000000 ) ) ;
#49633 = CARTESIAN_POINT ( 'NONE',  ( 7.000000000000000000, -38.64999999999999858, 12.69999999999999929 ) ) ;
#49634 = CARTESIAN_POINT ( 'NONE',  ( 4.046023737882789462, 3.142976262117210151, 26.00000000000000711 ) ) ;
#49635 = ORIENTED_EDGE ( 'NONE', *, *, #69876, .T. ) ;
#49636 = DIRECTION ( 'NONE',  ( 1.000000000000000000, 0.000000000000000000, 0.000000000000000000 ) ) ;
#49637 = CARTESIAN_POINT ( 'NONE',  ( 5.257023737882807524, 7.172176262117201162, 54.00000000000000711 ) ) ;
#49638 = ORIENTED_EDGE ( 'NONE', *, *, #42269, .F. ) ;
#49639 = ORIENTED_EDGE ( 'NONE', *, *, #67556, .T. ) ;
#49640 = EDGE_CURVE ( 'NONE', #62095, #41426, #9713, .T. ) ;
#49641 = VERTEX_POINT ( 'NONE', #15009 ) ;
#49642 = LINE ( 'NONE', #11462, #3952 ) ;
#49643 = CARTESIAN_POINT ( 'NONE',  ( 6.006483450353379716, -4.606483450353492159, 455.0000000000000568 ) ) ;
#49644 = VECTOR ( 'NONE', #51103, 1000.000000000000000 ) ;
#49645 = EDGE_CURVE ( 'NONE', #64214, #58583, #36566, .T. ) ;
#49646 = CYLINDRICAL_SURFACE ( 'NONE', #51865, 0.1999999999999987899 ) ;
#49647 = ORIENTED_EDGE ( 'NONE', *, *, #44147, .T. ) ;
#49648 = VERTEX_POINT ( 'NONE', #52860 ) ;
#49649 = VERTEX_POINT ( 'NONE', #47535 ) ;
#49650 = ADVANCED_FACE ( 'NONE', ( #43528 ), #69101, .F. ) ;
#49651 = AXIS2_PLACEMENT_3D ( 'NONE', #46288, #40981, #24731 ) ;
#49652 = PLANE ( 'NONE',  #38475 ) ;
#49653 = ORIENTED_EDGE ( 'NONE', *, *, #27489, .F. ) ;
#49654 = EDGE_CURVE ( 'NONE', #17772, #62784, #20650, .T. ) ;
#49655 = ORIENTED_EDGE ( 'NONE', *, *, #64102, .F. ) ;
#49656 = EDGE_LOOP ( 'NONE', ( #2160, #13069, #42367, #64673 ) ) ;
#49657 = CIRCLE ( 'NONE', #38366, 2.500000000000000000 ) ;
#49658 = EDGE_LOOP ( 'NONE', ( #2599, #52659, #41206, #29881 ) ) ;
#49659 = CARTESIAN_POINT ( 'NONE',  ( -30.00000000000000000, -11.50000000000000000, -15.00000000000000000 ) ) ;
#49660 = EDGE_CURVE ( 'NONE', #18694, #32607, #33841, .T. ) ;
#49662 = VERTEX_POINT ( 'NONE', #17702 ) ;
#49661 = CARTESIAN_POINT ( 'NONE',  ( -11.00000000000000000, -15.97213595500069871, -14.50000000000000000 ) ) ;
#49663 = AXIS2_PLACEMENT_3D ( 'NONE', #34032, #2215, #61243 ) ;
#49664 = DIRECTION ( 'NONE',  ( 0.6414496315691539108, -0.7671651518153028704, -2.587583378555131256E-16 ) ) ;
#49665 = CARTESIAN_POINT ( 'NONE',  ( 14.89999999999999680, -21.00000000000000000, 13.86939075806900057 ) ) ;
#49666 = PLANE ( 'NONE',  #8717 ) ;
#49667 = EDGE_CURVE ( 'NONE', #37106, #7061, #54845, .T. ) ;
#49668 = ORIENTED_EDGE ( 'NONE', *, *, #7258, .T. ) ;
#49669 = EDGE_CURVE ( 'NONE', #55919, #25422, #1778, .T. ) ;
#49670 = VECTOR ( 'NONE', #20986, 999.9999999999998863 ) ;
#49671 = ADVANCED_FACE ( 'NONE', ( #55187 ), #23687, .F. ) ;
#49672 = CARTESIAN_POINT ( 'NONE',  ( -7.593516549646791347, -11.78648345035336042, 195.0000000000000284 ) ) ;
#49673 = EDGE_CURVE ( 'NONE', #67323, #20378, #66135, .T. ) ;
#49674 = ADVANCED_FACE ( 'NONE', ( #60480 ), #65455, .F. ) ;
#49675 = FACE_OUTER_BOUND ( 'NONE', #19465, .T. ) ;
#49676 = DIRECTION ( 'NONE',  ( -1.000000000000000000, 0.000000000000000000, 0.000000000000000000 ) ) ;
#49677 = ORIENTED_EDGE ( 'NONE', *, *, #4202, .F. ) ;
#49678 = PLANE ( 'NONE',  #28108 ) ;
#49679 = EDGE_CURVE ( 'NONE', #10422, #3591, #1101, .T. ) ;
#49680 = DIRECTION ( 'NONE',  ( 0.000000000000000000, 0.000000000000000000, 1.000000000000000000 ) ) ;
#49681 = FACE_OUTER_BOUND ( 'NONE', #62120, .T. ) ;
#49682 = VECTOR ( 'NONE', #14363, 1000.000000000000000 ) ;
#49683 = EDGE_LOOP ( 'NONE', ( #69072, #5052, #55924, #57203 ) ) ;
#49684 = PLANE ( 'NONE',  #44847 ) ;
#49685 = DIRECTION ( 'NONE',  ( 1.000000000000000000, 0.000000000000000000, -0.000000000000000000 ) ) ;
#49686 = DIRECTION ( 'NONE',  ( 0.000000000000000000, -1.000000000000000000, 0.000000000000000000 ) ) ;
#49687 = LINE ( 'NONE', #1258, #29774 ) ;
#49688 = CARTESIAN_POINT ( 'NONE',  ( -8.130476262117324993, -9.562023737882769936, 54.00000000000000711 ) ) ;
#49689 = DIRECTION ( 'NONE',  ( 0.000000000000000000, 0.000000000000000000, -1.000000000000000000 ) ) ;
#49690 = EDGE_CURVE ( 'NONE', #10351, #53691, #49657, .T. ) ;
#49691 = VECTOR ( 'NONE', #6156, 999.9999999999998863 ) ;
#49692 = FILL_AREA_STYLE_COLOUR ( '', #68306 ) ;
#49693 = AXIS2_PLACEMENT_3D ( 'NONE', #41283, #68868, #47998 ) ;
#49694 = CARTESIAN_POINT ( 'NONE',  ( -30.00000000000000000, -14.33999999999999986, 14.50000000000000000 ) ) ;
#49695 = EDGE_CURVE ( 'NONE', #32276, #4210, #55872, .T. ) ;
#49696 = VECTOR ( 'NONE', #56050, 1000.000000000000000 ) ;
#49697 = EDGE_LOOP ( 'NONE', ( #32286, #54449, #6377, #58117 ) ) ;
#49698 = LINE ( 'NONE', #26752, #53021 ) ;
#49699 = FACE_OUTER_BOUND ( 'NONE', #35437, .T. ) ;
#49700 = AXIS2_PLACEMENT_3D ( 'NONE', #11243, #44802, #27180 ) ;
#49701 = FACE_OUTER_BOUND ( 'NONE', #16280, .T. ) ;
#49702 = CARTESIAN_POINT ( 'NONE',  ( 41.09999999999999432, 21.00000000000000000, 13.98999642601811999 ) ) ;
#49703 = VERTEX_POINT ( 'NONE', #49876 ) ;
#49704 = CARTESIAN_POINT ( 'NONE',  ( 17.00000000000000000, -17.35230188589299871, 15.35019951917099945 ) ) ;
#49705 = PLANE ( 'NONE',  #20374 ) ;
#49706 = CARTESIAN_POINT ( 'NONE',  ( 88.07321854994620480, 47.95351654967443977, 43.00000000000000000 ) ) ;
#49707 = CIRCLE ( 'NONE', #63239, 0.2000000000000005107 ) ;
#49708 = CYLINDRICAL_SURFACE ( 'NONE', #1505, 0.1749999999999998224 ) ;
#49709 = DIRECTION ( 'NONE',  ( -0.7071067811865475727, 0.7071067811865475727, 2.597868168706480597E-16 ) ) ;
#49710 = CIRCLE ( 'NONE', #55371, 2.458500000000000796 ) ;
#49711 = ORIENTED_EDGE ( 'NONE', *, *, #16855, .T. ) ;
#49712 = AXIS2_PLACEMENT_3D ( 'NONE', #6411, #7776, #13077 ) ;
#49713 = CARTESIAN_POINT ( 'NONE',  ( 7.450000000000004619, -1.336933437520057563E-15, -20.50000000000000000 ) ) ;
#49714 = CARTESIAN_POINT ( 'NONE',  ( -8.452095193409434160, -4.255011587777239868, 455.0000000000000568 ) ) ;
#49715 = ORIENTED_EDGE ( 'NONE', *, *, #46973, .F. ) ;
#49716 = AXIS2_PLACEMENT_3D ( 'NONE', #2454, #13412, #35308 ) ;
#49717 = AXIS2_PLACEMENT_3D ( 'NONE', #38022, #54629, #16793 ) ;
#49718 = CARTESIAN_POINT ( 'NONE',  ( -8.393516549646792058, -7.616533956692236096, 455.0000000000000568 ) ) ;
#49719 = ORIENTED_EDGE ( 'NONE', *, *, #57219, .T. ) ;
#49720 = CARTESIAN_POINT ( 'NONE',  ( 283.0000000000000568, -25.60000000000000142, -17.60000000000000142 ) ) ;
#49721 = ORIENTED_EDGE ( 'NONE', *, *, #55420, .T. ) ;
#49722 = VERTEX_POINT ( 'NONE', #39264 ) ;
#49723 = CYLINDRICAL_SURFACE ( 'NONE', #28347, 0.2000000000000005107 ) ;
#49724 = VERTEX_POINT ( 'NONE', #17013 ) ;
#49725 = LINE ( 'NONE', #22519, #37665 ) ;
#49726 = EDGE_CURVE ( 'NONE', #40313, #8070, #61162, .T. ) ;
#49727 = DIRECTION ( 'NONE',  ( -0.7671651518153006499, 0.6414496315691565753, -0.000000000000000000 ) ) ;
#49728 = CARTESIAN_POINT ( 'NONE',  ( 6.789561617636943325, -7.408280051175178293, 54.00000000000000711 ) ) ;
#49729 = VECTOR ( 'NONE', #45917, 1000.000000000000000 ) ;
#49730 = EDGE_LOOP ( 'NONE', ( #68830, #56399, #50373, #34524, #35830, #19892, #12237, #4456 ) ) ;
#49731 = VERTEX_POINT ( 'NONE', #60136 ) ;
#49732 = EDGE_CURVE ( 'NONE', #20510, #2132, #65794, .T. ) ;
#49733 = LINE ( 'NONE', #42694, #13158 ) ;
#49734 = LINE ( 'NONE', #44080, #6259 ) ;
#49735 = EDGE_LOOP ( 'NONE', ( #55802, #44151, #34504, #35744 ) ) ;
#49736 = EDGE_CURVE ( 'NONE', #18504, #58887, #30481, .T. ) ;
#49737 = ORIENTED_EDGE ( 'NONE', *, *, #21924, .F. ) ;
#49738 = ORIENTED_EDGE ( 'NONE', *, *, #23877, .F. ) ;
#49739 = CIRCLE ( 'NONE', #19251, 0.5000000000009459100 ) ;
#49740 = DIRECTION ( 'NONE',  ( -0.000000000000000000, -0.000000000000000000, -1.000000000000000000 ) ) ;
#49741 = ADVANCED_FACE ( 'NONE', ( #33277 ), #1432, .F. ) ;
#49742 = CARTESIAN_POINT ( 'NONE',  ( -8.000000000000000000, 7.281754163448145079, 5.000000000000000000 ) ) ;
#49743 = AXIS2_PLACEMENT_3D ( 'NONE', #44176, #12681, #34254 ) ;
#49745 = VERTEX_POINT ( 'NONE', #49536 ) ;
#49744 = DIRECTION ( 'NONE',  ( 0.7671651518153087546, 0.6414496315691468054, 0.000000000000000000 ) ) ;
#49746 = CYLINDRICAL_SURFACE ( 'NONE', #31167, 24.99999999998794920 ) ;
#49747 = VECTOR ( 'NONE', #40709, 1000.000000000000000 ) ;
#49748 = CARTESIAN_POINT ( 'NONE',  ( -25.50000000000000355, -15.50000000000000000, -22.50000000000000000 ) ) ;
#49749 = ORIENTED_EDGE ( 'NONE', *, *, #5489, .F. ) ;
#49750 = ORIENTED_EDGE ( 'NONE', *, *, #41238, .T. ) ;
#49751 = AXIS2_PLACEMENT_3D ( 'NONE', #68312, #41438, #62646 ) ;
#49752 = VERTEX_POINT ( 'NONE', #22665 ) ;
#49753 = VECTOR ( 'NONE', #6587, 1000.000000000000227 ) ;
#49754 = EDGE_CURVE ( 'NONE', #58797, #15862, #54509, .T. ) ;
#49755 = DIRECTION ( 'NONE',  ( 0.000000000000000000, -1.000000000000000000, 0.000000000000000000 ) ) ;
#49756 = DIRECTION ( 'NONE',  ( 1.836970198721029934E-16, 1.836970198721010706E-16, -1.000000000000000000 ) ) ;
#49757 = DIRECTION ( 'NONE',  ( -0.6414496315691645689, -0.7671651518152939886, -2.587583378555115478E-16 ) ) ;
#49758 = VECTOR ( 'NONE', #25995, 1000.000000000000000 ) ;
#49759 = CARTESIAN_POINT ( 'NONE',  ( 7.250000000000005329, -7.449999999999998401, -24.50000000000000000 ) ) ;
#49760 = DIRECTION ( 'NONE',  ( -1.000000000000000000, 0.000000000000000000, 0.000000000000000000 ) ) ;
#49762 = EDGE_LOOP ( 'NONE', ( #8690, #59990, #29963, #46444 ) ) ;
#49761 = LINE ( 'NONE', #7303, #44396 ) ;
#49763 = ORIENTED_EDGE ( 'NONE', *, *, #26934, .F. ) ;
#49764 = DIRECTION ( 'NONE',  ( 0.000000000000000000, 0.000000000000000000, -1.000000000000000000 ) ) ;
#49765 = AXIS2_PLACEMENT_3D ( 'NONE', #36029, #25081, #62908 ) ;
#49766 = DIRECTION ( 'NONE',  ( 0.000000000000000000, 0.000000000000000000, 1.000000000000000000 ) ) ;
#49767 = DIRECTION ( 'NONE',  ( 0.000000000000000000, 0.000000000000000000, -1.000000000000000000 ) ) ;
#49768 = DIRECTION ( 'NONE',  ( 1.836970198721029934E-16, 1.836970198721010706E-16, -1.000000000000000000 ) ) ;
#49769 = DIRECTION ( 'NONE',  ( 0.000000000000000000, 1.000000000000000000, 0.000000000000000000 ) ) ;
#49770 = ORIENTED_EDGE ( 'NONE', *, *, #7751, .T. ) ;
#49771 = DIRECTION ( 'NONE',  ( -0.000000000000000000, 3.673940397442059868E-16, -1.000000000000000000 ) ) ;
#49772 = CARTESIAN_POINT ( 'NONE',  ( 23.90000000000000213, 13.66939075806899240, 20.79999999999999361 ) ) ;
#49773 = EDGE_CURVE ( 'NONE', #42528, #14259, #38586, .T. ) ;
#49774 = LINE ( 'NONE', #50805, #26521 ) ;
#49775 = CARTESIAN_POINT ( 'NONE',  ( 2.420780051175169145, 8.697938382363084031, 54.00000000000000711 ) ) ;
#49777 = EDGE_CURVE ( 'NONE', #288, #7467, #12365, .T. ) ;
#49776 = SHAPE_REPRESENTATION ( 'Part1', ( #45918 ), #66261 ) ;
#49778 = AXIS2_PLACEMENT_3D ( 'NONE', #9852, #64982, #60704 ) ;
#49779 = DIRECTION ( 'NONE',  ( 0.000000000000000000, 0.000000000000000000, 1.000000000000000000 ) ) ;
#49780 = EDGE_CURVE ( 'NONE', #9391, #37986, #7427, .T. ) ;
#49781 = CARTESIAN_POINT ( 'NONE',  ( 31.89999999999999858, -0.2000000000089119934, 8.909539772616881237E-12 ) ) ;
#49782 = DIRECTION ( 'NONE',  ( -0.000000000000000000, 3.673940397442059868E-16, -1.000000000000000000 ) ) ;
#49783 = ORIENTED_EDGE ( 'NONE', *, *, #56287, .T. ) ;
#49784 = DIRECTION ( 'NONE',  ( 0.000000000000000000, -3.673940397442059868E-16, 1.000000000000000000 ) ) ;
#49785 = CARTESIAN_POINT ( 'NONE',  ( -8.250000000000001776, 7.250000000000000888, -26.00000000000001066 ) ) ;
#49786 = ORIENTED_EDGE ( 'NONE', *, *, #40550, .F. ) ;
#49787 = LINE ( 'NONE', #45510, #15418 ) ;
#49788 = DIRECTION ( 'NONE',  ( 1.000000000000000000, 0.000000000000000000, 0.000000000000000000 ) ) ;
#49789 = DIRECTION ( 'NONE',  ( 0.000000000000000000, 0.000000000000000000, 1.000000000000000000 ) ) ;
#49790 = DIRECTION ( 'NONE',  ( -1.794541526872559352E-16, -1.000000000000000000, 0.000000000000000000 ) ) ;
#49791 = CARTESIAN_POINT ( 'NONE',  ( 11.50000000000000000, -15.97213595500069871, -14.50000000000000000 ) ) ;
#49792 = CIRCLE ( 'NONE', #31744, 24.99999999998784972 ) ;
#49793 = DIRECTION ( 'NONE',  ( 0.000000000000000000, 1.000000000000000000, 0.000000000000000000 ) ) ;
#49794 = MECHANICAL_DESIGN_GEOMETRIC_PRESENTATION_REPRESENTATION (  '', ( #10287 ), #17090 ) ;
#49795 = ORIENTED_EDGE ( 'NONE', *, *, #43277, .F. ) ;
#49796 = CARTESIAN_POINT ( 'NONE',  ( 39.00000000000000000, 16.96999999999999886, -21.00000000000000000 ) ) ;
#49797 = VERTEX_POINT ( 'NONE', #39598 ) ;
#49798 = VECTOR ( 'NONE', #8461, 1000.000000000000000 ) ;
#49799 = LINE ( 'NONE', #11273, #17848 ) ;
#49800 = CIRCLE ( 'NONE', #36281, 0.5000000000023407942 ) ;
#49801 = CIRCLE ( 'NONE', #37408, 0.3499999999999996447 ) ;
#49802 = DIRECTION ( 'NONE',  ( -1.000000000000000000, 1.047444401652939849E-14, 0.000000000000000000 ) ) ;
#49803 = CARTESIAN_POINT ( 'NONE',  ( -28.00000000000000000, -15.50000000000000000, -14.50000000000000000 ) ) ;
#49804 = ORIENTED_EDGE ( 'NONE', *, *, #69272, .T. ) ;
#49805 = ORIENTED_EDGE ( 'NONE', *, *, #16783, .T. ) ;
#49806 = CARTESIAN_POINT ( 'NONE',  ( 7.000000000000000000, -38.15000000000000568, 13.19999999999999929 ) ) ;
#49807 = ORIENTED_EDGE ( 'NONE', *, *, #40003, .T. ) ;
#49808 = CIRCLE ( 'NONE', #64474, 24.99999999998784972 ) ;
#49809 = ORIENTED_EDGE ( 'NONE', *, *, #49828, .T. ) ;
#49810 = EDGE_CURVE ( 'NONE', #52907, #25548, #45097, .T. ) ;
#49811 = DIRECTION ( 'NONE',  ( 0.7071067811865464625, -0.7071067811865486830, -2.597868168706484048E-16 ) ) ;
#49812 = LINE ( 'NONE', #23282, #6470 ) ;
#49813 = DIRECTION ( 'NONE',  ( -1.000000000000000000, 1.260948829465470062E-14, -1.836970198721007008E-16 ) ) ;
#49814 = CIRCLE ( 'NONE', #19316, 5.200000000000009948 ) ;
#49815 = ORIENTED_EDGE ( 'NONE', *, *, #10878, .F. ) ;
#49816 = LINE ( 'NONE', #11289, #9756 ) ;
#49817 = AXIS2_PLACEMENT_3D ( 'NONE', #59536, #26307, #16392 ) ;
#49819 = FACE_OUTER_BOUND ( 'NONE', #9354, .T. ) ;
#49818 = PLANE ( 'NONE',  #11810 ) ;
#49820 = ORIENTED_EDGE ( 'NONE', *, *, #21733, .F. ) ;
#49822 = ORIENTED_EDGE ( 'NONE', *, *, #54017, .T. ) ;
#49821 = DIRECTION ( 'NONE',  ( -0.000000000000000000, 1.000000000000000000, -0.000000000000000000 ) ) ;
#49823 = EDGE_CURVE ( 'NONE', #20448, #19122, #3377, .T. ) ;
#49824 = VERTEX_POINT ( 'NONE', #66818 ) ;
#49825 = ADVANCED_FACE ( 'NONE', ( #40305 ), #19437, .F. ) ;
#49826 = DIRECTION ( 'NONE',  ( 1.000000000000000000, 0.000000000000000000, 0.000000000000000000 ) ) ;
#49827 = EDGE_CURVE ( 'NONE', #54853, #34859, #31615, .T. ) ;
#49828 = EDGE_CURVE ( 'NONE', #23630, #6256, #14493, .T. ) ;
#49829 = CARTESIAN_POINT ( 'NONE',  ( -3.663616288757094885, -6.364920264886888113, 54.00000000000000711 ) ) ;
#49830 = LINE ( 'NONE', #33902, #22415 ) ;
#49831 = EDGE_CURVE ( 'NONE', #42074, #16599, #13435, .T. ) ;
#49832 = AXIS2_PLACEMENT_3D ( 'NONE', #7986, #19303, #62797 ) ;
#49833 = ORIENTED_EDGE ( 'NONE', *, *, #28311, .T. ) ;
#49834 = ORIENTED_EDGE ( 'NONE', *, *, #63568, .T. ) ;
#49835 = CARTESIAN_POINT ( 'NONE',  ( 9.106483450353380249, -10.09643294401456259, 195.0000000000000284 ) ) ;
#49836 = CARTESIAN_POINT ( 'NONE',  ( 11.00000000000000000, -11.10796162543699950, 9.102987789146602893 ) ) ;
#49837 = ORIENTED_EDGE ( 'NONE', *, *, #18873, .F. ) ;
#49838 = LINE ( 'NONE', #38212, #39858 ) ;
#49839 = CARTESIAN_POINT ( 'NONE',  ( 30.00000000000000000, -11.50000000000082068, 10.20500000000000007 ) ) ;
#49840 = CARTESIAN_POINT ( 'NONE',  ( -8.598420958951683346, 1.466476262117183182, 54.00000000000000711 ) ) ;
#49841 = ORIENTED_EDGE ( 'NONE', *, *, #25001, .T. ) ;
#49842 = CIRCLE ( 'NONE', #64554, 3.500000000000000000 ) ;
#49843 = CARTESIAN_POINT ( 'NONE',  ( 30.00000000000000000, -14.33999999999999986, -14.50000000000000000 ) ) ;
#49844 = DIRECTION ( 'NONE',  ( 1.000000000000000000, 0.000000000000000000, 0.000000000000000000 ) ) ;
#49846 = ORIENTED_EDGE ( 'NONE', *, *, #18268, .F. ) ;
#49845 = DIRECTION ( 'NONE',  ( -1.000000000000000000, 0.000000000000000000, 0.000000000000000000 ) ) ;
#49848 = EDGE_LOOP ( 'NONE', ( #43168, #50492 ) ) ;
#49847 = DIRECTION ( 'NONE',  ( 1.062075597536821205E-14, 1.000000000000000000, 0.000000000000000000 ) ) ;
#49849 = CARTESIAN_POINT ( 'NONE',  ( 283.0000000000000568, -32.45000000000000995, -12.69999999999999929 ) ) ;
#49850 = DIRECTION ( 'NONE',  ( 0.7071067811865475727, -0.7071067811865475727, 0.000000000000000000 ) ) ;
#49851 = DIRECTION ( 'NONE',  ( 0.000000000000000000, -1.000000000000000000, 0.000000000000000000 ) ) ;
#49852 = LINE ( 'NONE', #56799, #7558 ) ;
#49853 = VECTOR ( 'NONE', #25196, 1000.000000000000000 ) ;
#49854 = CLOSED_SHELL ( 'NONE', ( #16032, #29384, #3406, #14375, #43359, #28700, #6852, #18534, #41736, #54355 ) ) ;
#49855 = CARTESIAN_POINT ( 'NONE',  ( -11.77351654964670935, 4.173516549646604901, 455.0000000000000568 ) ) ;
#49856 = LINE ( 'NONE', #64739, #66525 ) ;
#49857 = ORIENTED_EDGE ( 'NONE', *, *, #18125, .T. ) ;
#49858 = CARTESIAN_POINT ( 'NONE',  ( 7.265214908726123078, -5.393625297350022052, 455.0000000000000568 ) ) ;
#49859 = VECTOR ( 'NONE', #37217, 1000.000000000000000 ) ;
#49860 = CARTESIAN_POINT ( 'NONE',  ( -8.130476262117324993, -9.562023737882769936, 54.00000000000000711 ) ) ;
#49862 = ORIENTED_EDGE ( 'NONE', *, *, #51576, .F. ) ;
#49861 = CARTESIAN_POINT ( 'NONE',  ( 40.90000000000000568, -0.2000000000000000111, 0.000000000000000000 ) ) ;
#49863 = LINE ( 'NONE', #22987, #66246 ) ;
#49864 = EDGE_CURVE ( 'NONE', #57893, #6619, #51623, .T. ) ;
#49865 = DIRECTION ( 'NONE',  ( -4.336808689942025625E-15, -1.000000000000000000, 0.000000000000000000 ) ) ;
#49866 = EDGE_CURVE ( 'NONE', #62137, #62471, #46308, .T. ) ;
#49867 = VECTOR ( 'NONE', #2205, 1000.000000000000000 ) ;
#49868 = VERTEX_POINT ( 'NONE', #67541 ) ;
#49869 = DIRECTION ( 'NONE',  ( -0.000000000000000000, -0.000000000000000000, 1.000000000000000000 ) ) ;
#49870 = CARTESIAN_POINT ( 'NONE',  ( 7.250000000000005329, 7.250000000000000888, -23.50000000000000000 ) ) ;
#49872 = EDGE_LOOP ( 'NONE', ( #19021, #52732, #21738, #15128 ) ) ;
#49871 = ADVANCED_FACE ( 'NONE', ( #34648 ), #8831, .F. ) ;
#49873 = CARTESIAN_POINT ( 'NONE',  ( 7.250000000000005329, -7.249999999999998224, -18.00000000000000000 ) ) ;
#49874 = LINE ( 'NONE', #54505, #63166 ) ;
#49875 = LINE ( 'NONE', #22332, #11087 ) ;
#49876 = CARTESIAN_POINT ( 'NONE',  ( 8.250000000000005329, 7.250000000000000888, -11.00000000000000000 ) ) ;
#49877 = DIRECTION ( 'NONE',  ( 1.000000000000000000, -0.000000000000000000, -0.000000000000000000 ) ) ;
#49878 = ORIENTED_EDGE ( 'NONE', *, *, #24602, .T. ) ;
#49879 = VECTOR ( 'NONE', #1926, 1000.000000000000000 ) ;
#49880 = CARTESIAN_POINT ( 'NONE',  ( -6.858227778582867806, 2.989207322240119868, 54.00000000000000711 ) ) ;
#49881 = VERTEX_POINT ( 'NONE', #45598 ) ;
#49882 = ORIENTED_EDGE ( 'NONE', *, *, #58265, .F. ) ;
#49883 = DIRECTION ( 'NONE',  ( -1.000000000000000000, 0.000000000000000000, 0.000000000000000000 ) ) ;
#49884 = DIRECTION ( 'NONE',  ( -0.000000000000000000, -1.000000000000000000, 0.000000000000000000 ) ) ;
#49885 = DIRECTION ( 'NONE',  ( -1.000000000000000000, 0.000000000000000000, 0.000000000000000000 ) ) ;
#49886 = DIRECTION ( 'NONE',  ( 0.000000000000000000, 0.000000000000000000, -1.000000000000000000 ) ) ;
#49887 = ORIENTED_EDGE ( 'NONE', *, *, #42572, .F. ) ;
#49888 = ORIENTED_EDGE ( 'NONE', *, *, #61714, .F. ) ;
#49889 = AXIS2_PLACEMENT_3D ( 'NONE', #68653, #14905, #62277 ) ;
#49890 = LINE ( 'NONE', #66839, #41941 ) ;
#49891 = ORIENTED_EDGE ( 'NONE', *, *, #69147, .T. ) ;
#49892 = PRODUCT ( '6266N13_Heavy Duty Locking-Slotted Fitting1_6266N13', '6266N13_Heavy Duty Locking-Slotted Fitting1_6266N13', '', ( #35998 ) ) ;
#49893 = CYLINDRICAL_SURFACE ( 'NONE', #47330, 0.3500000000002719824 ) ;
#49894 = DIRECTION ( 'NONE',  ( 0.000000000000000000, 0.000000000000000000, 1.000000000000000000 ) ) ;
#49895 = DIRECTION ( 'NONE',  ( 0.000000000000000000, 0.000000000000000000, -1.000000000000000000 ) ) ;
#49896 = DIRECTION ( 'NONE',  ( 1.836970198721029934E-16, 1.836970198721010706E-16, -1.000000000000000000 ) ) ;
#49898 = LINE ( 'NONE', #22687, #23251 ) ;
#49897 = DIRECTION ( 'NONE',  ( 0.000000000000000000, 0.000000000000000000, -1.000000000000000000 ) ) ;
#49899 = VERTEX_POINT ( 'NONE', #56570 ) ;
#49901 = VERTEX_POINT ( 'NONE', #56228 ) ;
#49900 = DIRECTION ( 'NONE',  ( 0.000000000000000000, 0.000000000000000000, 1.000000000000000000 ) ) ;
#49902 = EDGE_LOOP ( 'NONE', ( #7189, #11082, #22346, #57451 ) ) ;
#49903 = EDGE_LOOP ( 'NONE', ( #21326, #21974, #3279, #18167, #9781, #30528, #47638, #15471, #9420, #28097, #5028, #29099, #40157, #44282, #10599, #37127, #36608, #23889, #2987, #2830, #15905, #32094, #3662, #14280, #40753, #16685, #56806, #48979, #60897, #40861, #52537, #13940, #62256, #47335, #2952, #40312, #11131, #13350, #41650, #64951, #35216, #3733, #32222, #21757, #54935, #41974, #34735, #9987, #17576, #31678, #57708, #15992, #10910, #51480, #8898, #15316 ) ) ;
#49904 = VECTOR ( 'NONE', #38760, 1000.000000000000000 ) ;
#49905 = CIRCLE ( 'NONE', #19415, 2.458500000000000796 ) ;
#49906 = EDGE_CURVE ( 'NONE', #63123, #8452, #14132, .T. ) ;
#49907 = LINE ( 'NONE', #13467, #8401 ) ;
#49908 = DIRECTION ( 'NONE',  ( -0.000000000000000000, 0.000000000000000000, 1.000000000000000000 ) ) ;
#49909 = EDGE_CURVE ( 'NONE', #17133, #62878, #8115, .T. ) ;
#49910 = DIRECTION ( 'NONE',  ( 0.000000000000000000, 0.000000000000000000, 1.000000000000000000 ) ) ;
#49911 = EDGE_LOOP ( 'NONE', ( #47429, #4388, #36679, #36178, #67707, #6719, #53361, #45520 ) ) ;
#49912 = EDGE_CURVE ( 'NONE', #28510, #19038, #40654, .T. ) ;
#49913 = ORIENTED_EDGE ( 'NONE', *, *, #11187, .F. ) ;
#49914 = VECTOR ( 'NONE', #59446, 1000.000000000000000 ) ;
#49915 = CARTESIAN_POINT ( 'NONE',  ( 4.155633711806643760, 5.779227145995235126, 26.00000000000000711 ) ) ;
#49916 = DIRECTION ( 'NONE',  ( -1.000000000000000000, 0.000000000000000000, 0.000000000000000000 ) ) ;
#49917 = ORIENTED_EDGE ( 'NONE', *, *, #32099, .T. ) ;
#49918 = VERTEX_POINT ( 'NONE', #62220 ) ;
#49919 = DIRECTION ( 'NONE',  ( -0.7071067811865348052, 0.7071067811865602293, 0.000000000000000000 ) ) ;
#49920 = CARTESIAN_POINT ( 'NONE',  ( -11.99351654964671354, 7.813516549646603693, 455.0000000000000568 ) ) ;
#49922 = VERTEX_POINT ( 'NONE', #62558 ) ;
#49921 = EDGE_CURVE ( 'NONE', #62492, #17912, #18045, .T. ) ;
#49923 = DIRECTION ( 'NONE',  ( -1.000000000000000000, 6.308085367188446447E-15, 0.000000000000000000 ) ) ;
#49925 = ORIENTED_EDGE ( 'NONE', *, *, #47286, .T. ) ;
#49924 = CYLINDRICAL_SURFACE ( 'NONE', #6883, 24.99999999998784972 ) ;
#49926 = ORIENTED_EDGE ( 'NONE', *, *, #9379, .T. ) ;
#49927 = CARTESIAN_POINT ( 'NONE',  ( 8.711985858128644011, 2.406732575409517239, 54.00000000000000711 ) ) ;
#49928 = DIRECTION ( 'NONE',  ( 0.000000000000000000, 0.000000000000000000, 1.000000000000000000 ) ) ;
#49929 = CARTESIAN_POINT ( 'NONE',  ( 30.00000000000000000, -16.64230188589299786, -14.64519951917100116 ) ) ;
#49930 = AXIS2_PLACEMENT_3D ( 'NONE', #32788, #54369, #49744 ) ;
#49931 = DIRECTION ( 'NONE',  ( 0.000000000000000000, 0.000000000000000000, -1.000000000000000000 ) ) ;
#49932 = CARTESIAN_POINT ( 'NONE',  ( -10.30047626211728939, -6.849523737882745600, 26.00000000000000000 ) ) ;
#49933 = LINE ( 'NONE', #65519, #5675 ) ;
#49934 = AXIS2_PLACEMENT_3D ( 'NONE', #23578, #6287, #6965 ) ;
#49935 = ORIENTED_EDGE ( 'NONE', *, *, #67714, .F. ) ;
#49936 = PLANE ( 'NONE',  #32658 ) ;
#49938 = VERTEX_POINT ( 'NONE', #30758 ) ;
#49937 = DIRECTION ( 'NONE',  ( 0.7671651518153006499, -0.6414496315691565753, -2.356647714346250026E-16 ) ) ;
#49939 = LINE ( 'NONE', #11760, #11797 ) ;
#49940 = PLANE ( 'NONE',  #47020 ) ;
#49941 = DIRECTION ( 'NONE',  ( -0.000000000000000000, -0.000000000000000000, -1.000000000000000000 ) ) ;
#49942 = CARTESIAN_POINT ( 'NONE',  ( 7.250000000000005329, 8.250000000000001776, -18.00000000000000000 ) ) ;
#49943 = LINE ( 'NONE', #23074, #51789 ) ;
#49944 = ORIENTED_EDGE ( 'NONE', *, *, #1840, .T. ) ;
#49946 = ORIENTED_EDGE ( 'NONE', *, *, #24276, .T. ) ;
#49945 = ADVANCED_FACE ( 'NONE', ( #2473 ), #67723, .F. ) ;
#49947 = CARTESIAN_POINT ( 'NONE',  ( 276.8000000000000682, -20.40000000000000213, 17.60000000000000142 ) ) ;
#49948 = CARTESIAN_POINT ( 'NONE',  ( 275.0000000000000000, -20.50000000000000000, -17.00000000000000000 ) ) ;
#49949 = CONICAL_SURFACE ( 'NONE', #25136, 2.000000000000001776, 0.7853981633974503884 ) ;
#49950 = EDGE_LOOP ( 'NONE', ( #41734, #49282, #41965, #57351 ) ) ;
#49951 = CARTESIAN_POINT ( 'NONE',  ( 3.664523737882778853, -10.50702373788280219, 26.00000000000000000 ) ) ;
#49952 = ORIENTED_EDGE ( 'NONE', *, *, #27846, .T. ) ;
#49953 = ORIENTED_EDGE ( 'NONE', *, *, #14980, .T. ) ;
#49954 = CARTESIAN_POINT ( 'NONE',  ( 6.665817930929297752, -7.532023737882823866, 54.00000000000000711 ) ) ;
#49955 = DIRECTION ( 'NONE',  ( 0.000000000000000000, 0.000000000000000000, 1.000000000000000000 ) ) ;
#49957 = EDGE_LOOP ( 'NONE', ( #53929, #39090, #43713, #18649 ) ) ;
#49956 = EDGE_CURVE ( 'NONE', #64055, #8098, #30404, .T. ) ;
#49958 = CARTESIAN_POINT ( 'NONE',  ( 13.00000000000000178, -16.28999999999710369, 14.50000000000000000 ) ) ;
#49959 = VECTOR ( 'NONE', #49790, 1000.000000000000000 ) ;
#49960 = DIRECTION ( 'NONE',  ( -1.000000000000000000, 0.000000000000000000, 0.000000000000000000 ) ) ;
#49961 = DIRECTION ( 'NONE',  ( -0.000000000000000000, -0.000000000000000000, -1.000000000000000000 ) ) ;
#49962 = EDGE_CURVE ( 'NONE', #66946, #59628, #50909, .T. ) ;
#49963 = VECTOR ( 'NONE', #47693, 1000.000000000000000 ) ;
#49964 = FACE_OUTER_BOUND ( 'NONE', #34616, .T. ) ;
#49965 = ORIENTED_EDGE ( 'NONE', *, *, #22653, .T. ) ;
#49967 = ORIENTED_EDGE ( 'NONE', *, *, #41471, .T. ) ;
#49966 = DIRECTION ( 'NONE',  ( -1.000000000000000000, 0.000000000000000000, 0.000000000000000000 ) ) ;
#49968 = DIRECTION ( 'NONE',  ( 1.349135440953254805E-14, 1.000000000000000000, 1.836970198721035604E-16 ) ) ;
#49969 = AXIS2_PLACEMENT_3D ( 'NONE', #69326, #25506, #31514 ) ;
#49970 = LINE ( 'NONE', #5819, #32734 ) ;
#49971 = PLANE ( 'NONE',  #57157 ) ;
#49972 = DIRECTION ( 'NONE',  ( -1.000000000000000000, 1.334402673828313093E-16, 0.000000000000000000 ) ) ;
#49973 = ORIENTED_EDGE ( 'NONE', *, *, #17074, .F. ) ;
#49974 = CARTESIAN_POINT ( 'NONE',  ( 25.50000000000000355, -15.50000000000000000, 24.50000000000000000 ) ) ;
#49975 = CARTESIAN_POINT ( 'NONE',  ( -14.25000000000000000, -2.500000000000000000, 23.22168783648699986 ) ) ;
#49976 = CIRCLE ( 'NONE', #54502, 24.99999999998784972 ) ;
#49977 = ORIENTED_EDGE ( 'NONE', *, *, #14626, .T. ) ;
#49978 = ORIENTED_EDGE ( 'NONE', *, *, #3929, .T. ) ;
#49979 = VERTEX_POINT ( 'NONE', #30047 ) ;
#49980 = CARTESIAN_POINT ( 'NONE',  ( 8.406483450353379183, -6.344579767990935260, 455.0000000000000568 ) ) ;
#49981 = VECTOR ( 'NONE', #14018, 1000.000000000000000 ) ;
#49982 = CARTESIAN_POINT ( 'NONE',  ( 8.835729544836338434, -8.144523737882813919, 26.00000000000000000 ) ) ;
#49984 = EDGE_CURVE ( 'NONE', #3700, #44054, #21449, .T. ) ;
#49983 = CARTESIAN_POINT ( 'NONE',  ( 48.99818295588534767, 0.7500000000000000000, 3.928729023727064451 ) ) ;
#49985 = EDGE_CURVE ( 'NONE', #26484, #48487, #25451, .T. ) ;
#49986 = CARTESIAN_POINT ( 'NONE',  ( 7.000000000000000000, -32.95000000000000284, 7.700000000000000178 ) ) ;
#49987 = ORIENTED_EDGE ( 'NONE', *, *, #34968, .F. ) ;
#49988 = ORIENTED_EDGE ( 'NONE', *, *, #35292, .T. ) ;
#49989 = EDGE_CURVE ( 'NONE', #24682, #52181, #47013, .T. ) ;
#49990 = ORIENTED_EDGE ( 'NONE', *, *, #22843, .F. ) ;
#49991 = VECTOR ( 'NONE', #42437, 1000.000000000000000 ) ;
#49992 = LINE ( 'NONE', #24530, #48622 ) ;
#49993 = VERTEX_POINT ( 'NONE', #47713 ) ;
#49994 = EDGE_CURVE ( 'NONE', #46156, #68853, #39493, .T. ) ;
#49995 = ORIENTED_EDGE ( 'NONE', *, *, #67796, .T. ) ;
#49997 = VERTEX_POINT ( 'NONE', #63279 ) ;
#49996 = EDGE_CURVE ( 'NONE', #24983, #1371, #14848, .T. ) ;
#49998 = ORIENTED_EDGE ( 'NONE', *, *, #41200, .F. ) ;
#49999 = CARTESIAN_POINT ( 'NONE',  ( 24.00000000000000000, -16.28999999999710369, -15.00000000000794920 ) ) ;
#50000 = ADVANCED_FACE ( 'NONE', ( #36401 ), #26159, .F. ) ;
#50002 = EDGE_LOOP ( 'NONE', ( #21897, #20453, #26613, #65111 ) ) ;
#50001 = DIRECTION ( 'NONE',  ( -0.000000000000000000, -0.000000000000000000, -1.000000000000000000 ) ) ;
#50003 = EDGE_CURVE ( 'NONE', #52054, #51180, #5669, .T. ) ;
#50004 = DIRECTION ( 'NONE',  ( 1.000000000000000000, -0.000000000000000000, -0.000000000000000000 ) ) ;
#50006 = CARTESIAN_POINT ( 'NONE',  ( 7.450000000000003730, -7.249999999999997335, -18.50000000000000000 ) ) ;
#50005 = AXIS2_PLACEMENT_3D ( 'NONE', #36882, #26259, #21651 ) ;
#50007 = DIRECTION ( 'NONE',  ( 0.000000000000000000, 0.000000000000000000, -1.000000000000000000 ) ) ;
#50009 = ORIENTED_EDGE ( 'NONE', *, *, #30479, .F. ) ;
#50008 = DIRECTION ( 'NONE',  ( 1.000000000000000000, 0.000000000000000000, 0.000000000000000000 ) ) ;
#50010 = CIRCLE ( 'NONE', #21763, 1.000000000000002665 ) ;
#50011 = CARTESIAN_POINT ( 'NONE',  ( -7.813516549646711162, 11.99351654964660341, 455.0000000000000568 ) ) ;
#50012 = FACE_OUTER_BOUND ( 'NONE', #14640, .T. ) ;
#50013 = DIRECTION ( 'NONE',  ( -1.000000000000000000, 0.000000000000000000, 0.000000000000000000 ) ) ;
#50014 = AXIS2_PLACEMENT_3D ( 'NONE', #7666, #49769, #6633 ) ;
#50015 = ORIENTED_EDGE ( 'NONE', *, *, #6943, .F. ) ;
#50016 = PLANE ( 'NONE',  #68750 ) ;
#50017 = CARTESIAN_POINT ( 'NONE',  ( -8.250000000000001776, 7.250000000000000888, -24.50000000000000000 ) ) ;
#50018 = AXIS2_PLACEMENT_3D ( 'NONE', #8077, #19052, #34948 ) ;
#50019 = DIRECTION ( 'NONE',  ( -0.000000000000000000, 3.673940397442059868E-16, -1.000000000000000000 ) ) ;
#50020 = EDGE_CURVE ( 'NONE', #42030, #50504, #68935, .T. ) ;
#50021 = ORIENTED_EDGE ( 'NONE', *, *, #60355, .T. ) ;
#50022 = DIRECTION ( 'NONE',  ( 0.000000000000000000, -1.000000000000000000, 0.000000000000000000 ) ) ;
#50023 = LINE ( 'NONE', #6889, #69178 ) ;
#50024 = CARTESIAN_POINT ( 'NONE',  ( 4.255011587777218551, -8.465062094116072799, 195.0000000000000284 ) ) ;
#50025 = AXIS2_PLACEMENT_3D ( 'NONE', #25984, #26323, #30237 ) ;
#50026 = EDGE_CURVE ( 'NONE', #67811, #5431, #47361, .T. ) ;
#50027 = VERTEX_POINT ( 'NONE', #4249 ) ;
#50028 = DIRECTION ( 'NONE',  ( 0.000000000000000000, 0.000000000000000000, 1.000000000000000000 ) ) ;
#50029 = LINE ( 'NONE', #17510, #15898 ) ;
#50030 = VECTOR ( 'NONE', #46956, 1000.000000000000000 ) ;
#50031 = CARTESIAN_POINT ( 'NONE',  ( -9.791916549646867196, -11.08848345035335115, 455.0000000000000568 ) ) ;
#50032 = EDGE_CURVE ( 'NONE', #29129, #20614, #16228, .T. ) ;
#50033 = LINE ( 'NONE', #1589, #2911 ) ;
#50034 = ORIENTED_EDGE ( 'NONE', *, *, #9253, .F. ) ;
#50035 = DIRECTION ( 'NONE',  ( 0.000000000000000000, 0.000000000000000000, -1.000000000000000000 ) ) ;
#50036 = DIRECTION ( 'NONE',  ( 0.000000000000000000, 1.000000000000000000, 0.000000000000000000 ) ) ;
#50037 = FACE_OUTER_BOUND ( 'NONE', #32453, .T. ) ;
#50038 = CIRCLE ( 'NONE', #69240, 1.224999999999998757 ) ;
#50039 = CARTESIAN_POINT ( 'NONE',  ( 84.77321854994620765, 47.95351654967443977, 29.00000000000000000 ) ) ;
#50040 = DIRECTION ( 'NONE',  ( 1.000000000000000000, -0.000000000000000000, 0.000000000000000000 ) ) ;
#50041 = EDGE_LOOP ( 'NONE', ( #35036, #18851, #24859, #28056 ) ) ;
#50042 = CARTESIAN_POINT ( 'NONE',  ( 30.00000000000000000, -14.04000000000000092, -17.04524521594300523 ) ) ;
#50043 = CARTESIAN_POINT ( 'NONE',  ( 283.0000000000000568, -25.60000000000000142, 17.60000000000000142 ) ) ;
#50044 = CARTESIAN_POINT ( 'NONE',  ( 23.75054448485400016, -15.50000000000000000, -25.53140320652400064 ) ) ;
#50045 = DIRECTION ( 'NONE',  ( 0.000000000000000000, 0.000000000000000000, 1.000000000000000000 ) ) ;
#50046 = ADVANCED_FACE ( 'NONE', ( #9539 ), #37464, .F. ) ;
#50047 = DIRECTION ( 'NONE',  ( 1.000000000000000000, -1.047444401652940007E-14, 1.836970198721010706E-16 ) ) ;
#50048 = ORIENTED_EDGE ( 'NONE', *, *, #59324, .F. ) ;
#50049 = EDGE_LOOP ( 'NONE', ( #47614, #39847, #23193, #31950 ) ) ;
#50050 = AXIS2_PLACEMENT_3D ( 'NONE', #21129, #24062, #45620 ) ;
#50051 = DIRECTION ( 'NONE',  ( -1.836970198721029934E-16, 1.836970198721036344E-16, -1.000000000000000000 ) ) ;
#50052 = CARTESIAN_POINT ( 'NONE',  ( -7.450000000000001954, 7.250000000000000000, -15.00000000000000000 ) ) ;
#50054 = ORIENTED_EDGE ( 'NONE', *, *, #32369, .F. ) ;
#50053 = ADVANCED_FACE ( 'NONE', ( #36770 ), #4934, .T. ) ;
#50055 = ADVANCED_FACE ( 'NONE', ( #4590, #69282 ), #20835, .T. ) ;
#50056 = VECTOR ( 'NONE', #68229, 1000.000000000000000 ) ;
#50057 = DIRECTION ( 'NONE',  ( -0.7671651518152939886, 0.6414496315691645689, 0.000000000000000000 ) ) ;
#50058 = AXIS2_PLACEMENT_3D ( 'NONE', #10362, #52448, #53164 ) ;
#50059 = EDGE_CURVE ( 'NONE', #23915, #57396, #15560, .T. ) ;
#50060 = ORIENTED_EDGE ( 'NONE', *, *, #64966, .T. ) ;
#50061 = EDGE_CURVE ( 'NONE', #62351, #44232, #58681, .T. ) ;
#50062 = EDGE_CURVE ( 'NONE', #6322, #45033, #9076, .T. ) ;
#50063 = FACE_OUTER_BOUND ( 'NONE', #53720, .T. ) ;
#50065 = EDGE_LOOP ( 'NONE', ( #44322, #8595, #55483, #25538 ) ) ;
#50064 = AXIS2_PLACEMENT_3D ( 'NONE', #64995, #22209, #43773 ) ;
#50066 = AXIS2_PLACEMENT_3D ( 'NONE', #68828, #20385, #4483 ) ;
#50067 = VERTEX_POINT ( 'NONE', #26859 ) ;
#50068 = CARTESIAN_POINT ( 'NONE',  ( 9.899999999999998579, 21.00000000000000355, -13.98999642601812354 ) ) ;
#50069 = DIRECTION ( 'NONE',  ( 0.000000000000000000, 0.000000000000000000, -1.000000000000000000 ) ) ;
#50070 = EDGE_CURVE ( 'NONE', #26986, #42030, #67482, .T. ) ;
#50071 = DIRECTION ( 'NONE',  ( -1.000000000000000000, 0.000000000000000000, 0.000000000000000000 ) ) ;
#50072 = CYLINDRICAL_SURFACE ( 'NONE', #23463, 3.499999999999850342 ) ;
#50073 = EDGE_CURVE ( 'NONE', #53577, #29958, #59369, .T. ) ;
#50074 = ORIENTED_EDGE ( 'NONE', *, *, #55932, .F. ) ;
#50075 = VERTEX_POINT ( 'NONE', #65713 ) ;
#50076 = FACE_OUTER_BOUND ( 'NONE', #38507, .T. ) ;
#50077 = EDGE_CURVE ( 'NONE', #46187, #42553, #16590, .T. ) ;
#50078 = LINE ( 'NONE', #5573, #33855 ) ;
#50079 = ORIENTED_EDGE ( 'NONE', *, *, #63821, .F. ) ;
#50080 = ORIENTED_EDGE ( 'NONE', *, *, #50694, .T. ) ;
#50081 = ORIENTED_EDGE ( 'NONE', *, *, #69354, .T. ) ;
#50082 = PLANE ( 'NONE',  #55297 ) ;
#50083 = DIRECTION ( 'NONE',  ( 0.000000000000000000, -0.7071067811865474617, -0.7071067811865474617 ) ) ;
#50084 = ADVANCED_FACE ( 'NONE', ( #44819 ), #673, .F. ) ;
#50086 = VERTEX_POINT ( 'NONE', #49791 ) ;
#50085 = DIRECTION ( 'NONE',  ( 1.000000000000000000, -0.000000000000000000, -0.000000000000000000 ) ) ;
#50087 = EDGE_CURVE ( 'NONE', #5747, #29034, #12285, .T. ) ;
#50088 = PLANE ( 'NONE',  #32267 ) ;
#50089 = DIRECTION ( 'NONE',  ( 0.000000000000000000, 0.000000000000000000, -1.000000000000000000 ) ) ;
#50090 = VERTEX_POINT ( 'NONE', #43800 ) ;
#50091 = ORIENTED_EDGE ( 'NONE', *, *, #11433, .F. ) ;
#50092 = EDGE_CURVE ( 'NONE', #2477, #23182, #28559, .T. ) ;
#50093 = DIRECTION ( 'NONE',  ( 0.000000000000000000, 0.000000000000000000, 1.000000000000000000 ) ) ;
#50094 = LINE ( 'NONE', #44428, #25664 ) ;
#50095 = DIRECTION ( 'NONE',  ( 0.000000000000000000, -1.000000000000000000, 0.000000000000000000 ) ) ;
#50096 = VECTOR ( 'NONE', #66812, 1000.000000000000000 ) ;
#50097 = AXIS2_PLACEMENT_3D ( 'NONE', #69833, #58883, #53932 ) ;
#50098 = CARTESIAN_POINT ( 'NONE',  ( 46.39999999999999858, 21.00000000000000000, -0.7500000000000000000 ) ) ;
#50099 = DIRECTION ( 'NONE',  ( -1.000000000000000000, 0.000000000000000000, 0.000000000000000000 ) ) ;
#50101 = ORIENTED_EDGE ( 'NONE', *, *, #13275, .T. ) ;
#50100 = LINE ( 'NONE', #44786, #19588 ) ;
#50102 = ORIENTED_EDGE ( 'NONE', *, *, #69960, .F. ) ;
#50103 = FACE_OUTER_BOUND ( 'NONE', #49658, .T. ) ;
#50104 = COLOUR_RGB ( '', 0.40784314, 0.44705882, 0.49803922) ;
#50106 = AXIS2_PLACEMENT_3D ( 'NONE', #47685, #25421, #6202 ) ;
#50105 = CARTESIAN_POINT ( 'NONE',  ( -2.406732575409589625, 8.697938382363036069, 54.00000000000000711 ) ) ;
#50107 = CARTESIAN_POINT ( 'NONE',  ( 8.250000000000005329, 8.250000000000001776, -26.00000000000001066 ) ) ;
#50108 = DIRECTION ( 'NONE',  ( 0.000000000000000000, 1.000000000000000000, 0.000000000000000000 ) ) ;
#50109 = EDGE_CURVE ( 'NONE', #38923, #32604, #14733, .T. ) ;
#50110 = AXIS2_PLACEMENT_3D ( 'NONE', #31570, #53148, #6430 ) ;
#50111 = AXIS2_PLACEMENT_3D ( 'NONE', #60526, #6773, #24081 ) ;
#50112 = LINE ( 'NONE', #62103, #61308 ) ;
#50113 = ORIENTED_EDGE ( 'NONE', *, *, #21994, .F. ) ;
#50114 = CARTESIAN_POINT ( 'NONE',  ( -11.18999999999999950, 11.25000000000000178, -5.000000000000000000 ) ) ;
#50115 = DIRECTION ( 'NONE',  ( 0.000000000000000000, 0.000000000000000000, 1.000000000000000000 ) ) ;
#50116 = CYLINDRICAL_SURFACE ( 'NONE', #14085, 2.250000000000001776 ) ;
#50117 = EDGE_CURVE ( 'NONE', #14877, #67332, #1356, .T. ) ;
#50118 = CARTESIAN_POINT ( 'NONE',  ( 15.00000000000000000, -21.00000000000000000, 0.000000000000000000 ) ) ;
#50119 = DIRECTION ( 'NONE',  ( 1.836970198721029934E-16, 1.836970198721010706E-16, -1.000000000000000000 ) ) ;
#50120 = DIRECTION ( 'NONE',  ( 0.000000000000000000, 1.000000000000000000, 0.000000000000000000 ) ) ;
#50121 = EDGE_CURVE ( 'NONE', #60080, #10676, #58760, .T. ) ;
#50122 = LINE ( 'NONE', #39172, #48797 ) ;
#50123 = ORIENTED_EDGE ( 'NONE', *, *, #49100, .F. ) ;
#50124 = DIRECTION ( 'NONE',  ( -1.000000000000000000, 0.000000000000000000, 0.000000000000000000 ) ) ;
#50125 = EDGE_CURVE ( 'NONE', #17228, #5931, #22920, .T. ) ;
#50126 = DIRECTION ( 'NONE',  ( 1.836970198721029934E-16, 1.836970198721010706E-16, -1.000000000000000000 ) ) ;
#50127 = ORIENTED_EDGE ( 'NONE', *, *, #31127, .F. ) ;
#50128 = DIRECTION ( 'NONE',  ( -1.000000000000000000, 0.000000000000000000, 0.000000000000000000 ) ) ;
#50129 = CARTESIAN_POINT ( 'NONE',  ( 8.406483450353384512, 4.383466043307721272, 455.0000000000000568 ) ) ;
#50130 = CARTESIAN_POINT ( 'NONE',  ( 6.500000000000000888, -6.500000000000002665, -1.000000000000000000 ) ) ;
#50131 = CARTESIAN_POINT ( 'NONE',  ( 9.247904806590689475, -9.955011587777253368, 195.0000000000000284 ) ) ;
#50132 = EDGE_CURVE ( 'NONE', #21706, #9319, #28223, .T. ) ;
#50133 = DIRECTION ( 'NONE',  ( -1.000000000000000000, 0.000000000000000000, 0.000000000000000000 ) ) ;
#50134 = ORIENTED_EDGE ( 'NONE', *, *, #2989, .F. ) ;
#50135 = CARTESIAN_POINT ( 'NONE',  ( -7.342976262117259623, 4.947141984184421304, 54.00000000000000711 ) ) ;
#50136 = ORIENTED_EDGE ( 'NONE', *, *, #38736, .T. ) ;
#50137 = LINE ( 'NONE', #34906, #65000 ) ;
#50138 = ORIENTED_EDGE ( 'NONE', *, *, #67340, .F. ) ;
#50139 = CIRCLE ( 'NONE', #30975, 0.3999999999999993006 ) ;
#50140 = DIRECTION ( 'NONE',  ( -1.000000000000000000, 0.000000000000000000, 0.000000000000000000 ) ) ;
#50141 = CIRCLE ( 'NONE', #68224, 0.1999999999999987899 ) ;
#50142 = EDGE_CURVE ( 'NONE', #25334, #1385, #17264, .T. ) ;
#50143 = DIRECTION ( 'NONE',  ( -0.5000000000000129896, -0.8660254037844311581, -2.509347957447868930E-16 ) ) ;
#50144 = CARTESIAN_POINT ( 'NONE',  ( 9.900000000000000355, -14.48845687959340012, 21.00000000000000000 ) ) ;
#50145 = ORIENTED_EDGE ( 'NONE', *, *, #10332, .T. ) ;
#50146 = EDGE_LOOP ( 'NONE', ( #30469, #22787 ) ) ;
#50147 = CARTESIAN_POINT ( 'NONE',  ( 30.00000000000000000, -5.599999999999999645, -27.00000000000000000 ) ) ;
#50148 = VERTEX_POINT ( 'NONE', #1025 ) ;
#50149 = ORIENTED_EDGE ( 'NONE', *, *, #31777, .T. ) ;
#50150 = CARTESIAN_POINT ( 'NONE',  ( 39.90000000000000568, 0.000000000000000000, 3.447897592003593022E-15 ) ) ;
#50151 = DIRECTION ( 'NONE',  ( -0.6414496315691420314, 0.7671651518153128624, 2.587583378555127804E-16 ) ) ;
#50152 = AXIS2_PLACEMENT_3D ( 'NONE', #69973, #5964, #55103 ) ;
#50153 = VECTOR ( 'NONE', #68356, 1000.000000000000000 ) ;
#50154 = DIRECTION ( 'NONE',  ( -1.000000000000000000, 0.000000000000000000, 0.000000000000000000 ) ) ;
#50155 = VERTEX_POINT ( 'NONE', #66400 ) ;
#50156 = DIRECTION ( 'NONE',  ( 0.000000000000000000, 0.000000000000000000, 1.000000000000000000 ) ) ;
#50158 = CARTESIAN_POINT ( 'NONE',  ( 41.09999999999999432, -14.06939075806900163, 20.80000000000000426 ) ) ;
#50157 = LINE ( 'NONE', #34224, #69427 ) ;
#50159 = AXIS2_PLACEMENT_3D ( 'NONE', #57284, #57982, #3901 ) ;
#50161 = ORIENTED_EDGE ( 'NONE', *, *, #8079, .F. ) ;
#50160 = VECTOR ( 'NONE', #20639, 1000.000000000000114 ) ;
#50163 = EDGE_LOOP ( 'NONE', ( #39796, #39826, #42271, #27807 ) ) ;
#50162 = DIRECTION ( 'NONE',  ( -1.000000000000000000, 1.260948829465470062E-14, -1.836970198721007008E-16 ) ) ;
#50164 = ORIENTED_EDGE ( 'NONE', *, *, #8105, .F. ) ;
#50165 =( NAMED_UNIT ( * ) PLANE_ANGLE_UNIT ( ) SI_UNIT ( $, .RADIAN. ) );
#50166 = CIRCLE ( 'NONE', #18512, 24.99999999998784972 ) ;
#50167 = CARTESIAN_POINT ( 'NONE',  ( -7.450000000000001954, 0.000000000000000000, -25.00000000000000000 ) ) ;
#50168 = ADVANCED_FACE ( 'NONE', ( #33531 ), #6319, .F. ) ;
#50169 = ORIENTED_EDGE ( 'NONE', *, *, #38441, .F. ) ;
#50170 = EDGE_CURVE ( 'NONE', #26479, #3872, #27200, .T. ) ;
#50171 = CARTESIAN_POINT ( 'NONE',  ( -2.893516549646673930, 11.11351654964657598, 455.0000000000000568 ) ) ;
#50172 = CARTESIAN_POINT ( 'NONE',  ( -15.50000000000000000, 998.9628421096749662, 22.50000000000000000 ) ) ;
#50173 = ORIENTED_EDGE ( 'NONE', *, *, #54075, .F. ) ;
#50174 = ORIENTED_EDGE ( 'NONE', *, *, #62173, .F. ) ;
#50175 = VECTOR ( 'NONE', #67201, 1000.000000000000000 ) ;
#50176 = DIRECTION ( 'NONE',  ( 4.336808689942006692E-15, 1.000000000000000000, 0.000000000000000000 ) ) ;
#50177 = CARTESIAN_POINT ( 'NONE',  ( 30.00000000000000000, -17.00000000000000000, 15.70499999999969809 ) ) ;
#50178 = ORIENTED_EDGE ( 'NONE', *, *, #69090, .F. ) ;
#50179 = CARTESIAN_POINT ( 'NONE',  ( -8.250000000000001776, -7.249999999999998224, -26.00000000000001066 ) ) ;
#50180 = CARTESIAN_POINT ( 'NONE',  ( -23.48000000000000043, -15.50000000000000000, 26.00000000000000355 ) ) ;
#50181 = FACE_OUTER_BOUND ( 'NONE', #12766, .T. ) ;
#50182 = ORIENTED_EDGE ( 'NONE', *, *, #52399, .F. ) ;
#50183 = CYLINDRICAL_SURFACE ( 'NONE', #66253, 1.000000000000000000 ) ;
#50184 = DIRECTION ( 'NONE',  ( 0.000000000000000000, -0.7046037717859411353, -0.7096009616573427659 ) ) ;
#50185 = VECTOR ( 'NONE', #31829, 1000.000000000000114 ) ;
#50187 = ORIENTED_EDGE ( 'NONE', *, *, #22656, .T. ) ;
#50186 = LINE ( 'NONE', #23321, #57774 ) ;
#50189 = ORIENTED_EDGE ( 'NONE', *, *, #47112, .T. ) ;
#50188 = DIRECTION ( 'NONE',  ( 0.000000000000000000, -3.673940397442059868E-16, 1.000000000000000000 ) ) ;
#50190 = DIRECTION ( 'NONE',  ( 0.000000000000000000, 0.000000000000000000, 1.000000000000000000 ) ) ;
#50191 = CARTESIAN_POINT ( 'NONE',  ( 7.450000000000006395, 7.250000000000000888, -19.50000000000000000 ) ) ;
#50192 = AXIS2_PLACEMENT_3D ( 'NONE', #57186, #68142, #58236 ) ;
#50193 = CARTESIAN_POINT ( 'NONE',  ( 9.106483450353419329, 11.11351654964656710, 455.0000000000000568 ) ) ;
#50194 = CARTESIAN_POINT ( 'NONE',  ( 35.89999999999999858, -21.00000000000000000, 13.86939075806900057 ) ) ;
#50195 = DIRECTION ( 'NONE',  ( -1.000000000000000000, 0.000000000000000000, 0.000000000000000000 ) ) ;
#50196 = EDGE_LOOP ( 'NONE', ( #62072, #35403, #53144, #22913 ) ) ;
#50197 = CARTESIAN_POINT ( 'NONE',  ( 3.682023737882818448, 9.722976262117203561, 54.00000000000000711 ) ) ;
#50198 = CARTESIAN_POINT ( 'NONE',  ( -7.450000000000001954, 0.000000000000000000, -8.500000000000000000 ) ) ;
#50199 = CARTESIAN_POINT ( 'NONE',  ( 41.09999999999999432, 14.08845687959340331, -21.00000000000000000 ) ) ;
#50200 = EDGE_CURVE ( 'NONE', #67430, #43499, #54270, .T. ) ;
#50202 = ORIENTED_EDGE ( 'NONE', *, *, #35388, .F. ) ;
#50201 = CARTESIAN_POINT ( 'NONE',  ( -1.620245201994373829, -8.241237374594328813, 54.00000000000000711 ) ) ;
#50203 = VECTOR ( 'NONE', #9809, 1000.000000000000000 ) ;
#50204 = AXIS2_PLACEMENT_3D ( 'NONE', #33899, #17294, #13018 ) ;
#50205 = LINE ( 'NONE', #34631, #38052 ) ;
#50206 = DIRECTION ( 'NONE',  ( 0.000000000000000000, 0.000000000000000000, -1.000000000000000000 ) ) ;
#50207 = ADVANCED_FACE ( 'NONE', ( #17610 ), #22581, .F. ) ;
#50208 = CIRCLE ( 'NONE', #58149, 0.5249999999999990230 ) ;
#50209 = AXIS2_PLACEMENT_3D ( 'NONE', #10940, #59727, #44829 ) ;
#50210 = EDGE_LOOP ( 'NONE', ( #32236, #24534, #26251, #44414 ) ) ;
#50211 = DIRECTION ( 'NONE',  ( 1.000000000000000000, 0.000000000000000000, 0.000000000000000000 ) ) ;
#50212 = EDGE_CURVE ( 'NONE', #10486, #30586, #48762, .T. ) ;
#50213 = FACE_OUTER_BOUND ( 'NONE', #52900, .T. ) ;
#50214 = EDGE_CURVE ( 'NONE', #18722, #25188, #49102, .T. ) ;
#50215 = VERTEX_POINT ( 'NONE', #38163 ) ;
#50216 = CARTESIAN_POINT ( 'NONE',  ( 4.155633711806649089, 5.779227145995230686, 54.00000000000000711 ) ) ;
#50217 = CARTESIAN_POINT ( 'NONE',  ( 11.00000000000000000, -12.00000000000000000, 11.03137303340310282 ) ) ;
#50218 = AXIS2_PLACEMENT_3D ( 'NONE', #14434, #36697, #67481 ) ;
#50219 = FACE_BOUND ( 'NONE', #52406, .T. ) ;
#50220 = ADVANCED_FACE ( 'NONE', ( #59713 ), #17950, .F. ) ;
#50221 = EDGE_CURVE ( 'NONE', #54436, #28576, #45163, .T. ) ;
#50222 = DIRECTION ( 'NONE',  ( -1.836970198721029934E-16, 1.836970198721036344E-16, -1.000000000000000000 ) ) ;
#50223 = DIRECTION ( 'NONE',  ( -0.7071067811865361374, 0.7071067811865588970, 2.810316974849854557E-30 ) ) ;
#50224 = AXIS2_PLACEMENT_3D ( 'NONE', #45854, #67440, #19672 ) ;
#50225 = EDGE_CURVE ( 'NONE', #29928, #36409, #49707, .T. ) ;
#50226 = ORIENTED_EDGE ( 'NONE', *, *, #23032, .F. ) ;
#50227 = DIRECTION ( 'NONE',  ( -0.7071067811865451302, 0.7071067811865500152, 0.000000000000000000 ) ) ;
#50228 = VERTEX_POINT ( 'NONE', #8028 ) ;
#50229 = ORIENTED_EDGE ( 'NONE', *, *, #58771, .T. ) ;
#50230 = AXIS2_PLACEMENT_3D ( 'NONE', #3211, #25126, #46683 ) ;
#50231 = LINE ( 'NONE', #18384, #62981 ) ;
#50232 = LINE ( 'NONE', #14046, #65456 ) ;
#50233 = DIRECTION ( 'NONE',  ( 0.000000000000000000, 0.000000000000000000, 1.000000000000000000 ) ) ;
#50234 = CARTESIAN_POINT ( 'NONE',  ( 2.544523737882785852, -9.737023737882790186, 26.00000000000000000 ) ) ;
#50235 = VERTEX_POINT ( 'NONE', #56144 ) ;
#50236 = ORIENTED_EDGE ( 'NONE', *, *, #3434, .F. ) ;
#50237 = DIRECTION ( 'NONE',  ( -0.000000000000000000, 3.673940397442059868E-16, -1.000000000000000000 ) ) ;
#50238 = ORIENTED_EDGE ( 'NONE', *, *, #47635, .F. ) ;
#50239 = CARTESIAN_POINT ( 'NONE',  ( -4.193516549646673752, 11.31351654964658771, 195.0000000000000284 ) ) ;
#50240 = DIRECTION ( 'NONE',  ( -0.7071067811865441310, 0.7071067811865510144, 0.000000000000000000 ) ) ;
#50241 = CARTESIAN_POINT ( 'NONE',  ( 30.00000000000000000, -11.10796162543699950, -9.102987789146602893 ) ) ;
#50242 = CARTESIAN_POINT ( 'NONE',  ( 47.00000000000000000, 0.000000000000000000, 0.000000000000000000 ) ) ;
#50244 = DIRECTION ( 'NONE',  ( -1.000000000000000000, 0.000000000000000000, 0.000000000000000000 ) ) ;
#50243 = FACE_OUTER_BOUND ( 'NONE', #37387, .T. ) ;
#50245 = ORIENTED_EDGE ( 'NONE', *, *, #38186, .F. ) ;
#50247 = VERTEX_POINT ( 'NONE', #62126 ) ;
#50246 = FACE_OUTER_BOUND ( 'NONE', #20435, .T. ) ;
#50248 = CIRCLE ( 'NONE', #31083, 0.9999999999999991118 ) ;
#50249 = VERTEX_POINT ( 'NONE', #45515 ) ;
#50250 = ORIENTED_EDGE ( 'NONE', *, *, #3572, .F. ) ;
#50251 = CARTESIAN_POINT ( 'NONE',  ( -4.734785091273985280, -5.393625297349913694, 195.0000000000000284 ) ) ;
#50252 = ADVANCED_FACE ( 'NONE', ( #29602 ), #68146, .F. ) ;
#50253 = AXIS2_PLACEMENT_3D ( 'NONE', #49522, #33261, #44902 ) ;
#50255 = CARTESIAN_POINT ( 'NONE',  ( 283.0000000000000568, -20.50000000000000000, 13.00000000000000178 ) ) ;
#50254 = AXIS2_PLACEMENT_3D ( 'NONE', #61459, #39886, #29279 ) ;
#50256 = CARTESIAN_POINT ( 'NONE',  ( 3.857023737882779635, -10.31452373788281029, 54.00000000000000711 ) ) ;
#50257 = EDGE_LOOP ( 'NONE', ( #44664, #21238, #61983, #48849, #25804, #28959 ) ) ;
#50258 = ORIENTED_EDGE ( 'NONE', *, *, #56104, .F. ) ;
#50259 = EDGE_CURVE ( 'NONE', #8234, #68958, #19223, .T. ) ;
#50260 = EDGE_CURVE ( 'NONE', #13113, #27714, #50485, .T. ) ;
#50261 = AXIS2_PLACEMENT_3D ( 'NONE', #49050, #17207, #6258 ) ;
#50262 = LINE ( 'NONE', #23394, #56875 ) ;
#50263 = CARTESIAN_POINT ( 'NONE',  ( 47.00000000000000000, -0.7500000000000000000, 3.418698582794335028 ) ) ;
#50264 = EDGE_CURVE ( 'NONE', #11691, #23447, #37312, .T. ) ;
#50265 = ORIENTED_EDGE ( 'NONE', *, *, #10129, .T. ) ;
#50266 = ORIENTED_EDGE ( 'NONE', *, *, #19025, .F. ) ;
#50267 = FACE_OUTER_BOUND ( 'NONE', #29642, .T. ) ;
#50268 = AXIS2_PLACEMENT_3D ( 'NONE', #42525, #64117, #15663 ) ;
#50269 = DIRECTION ( 'NONE',  ( 0.000000000000000000, -0.7084617869615144059, 0.7057491738679528837 ) ) ;
#50270 = VERTEX_POINT ( 'NONE', #34900 ) ;
#50271 = CIRCLE ( 'NONE', #45776, 1.000000000000000000 ) ;
#50272 = CARTESIAN_POINT ( 'NONE',  ( 22.14589803375000088, -17.50000000000000000, 21.50000000000000000 ) ) ;
#50273 = ORIENTED_EDGE ( 'NONE', *, *, #52217, .T. ) ;
#50274 = AXIS2_PLACEMENT_3D ( 'NONE', #19661, #9069, #30985 ) ;
#50275 = VERTEX_POINT ( 'NONE', #56480 ) ;
#50276 = DIRECTION ( 'NONE',  ( 1.836970198721029934E-16, 1.836970198721010706E-16, -1.000000000000000000 ) ) ;
#50277 = DIRECTION ( 'NONE',  ( 1.000000000000000000, -1.883404846338789915E-14, 1.836970198720995421E-16 ) ) ;
#50278 = DIRECTION ( 'NONE',  ( -3.491481338843132961E-15, -1.000000000000000000, -1.836970198721029934E-16 ) ) ;
#50279 = CARTESIAN_POINT ( 'NONE',  ( 36.90000000000000568, 20.60000000000000142, 13.86939075806900057 ) ) ;
#50280 = CARTESIAN_POINT ( 'NONE',  ( 7.000000000000000000, -23.29603921945599865, -12.50000000000000000 ) ) ;
#50281 = CARTESIAN_POINT ( 'NONE',  ( 11.19000000000000128, -12.00000000000000000, -4.250000000000000000 ) ) ;
#50282 = DIRECTION ( 'NONE',  ( 1.000000000000000000, 0.000000000000000000, 0.000000000000000000 ) ) ;
#50283 = EDGE_LOOP ( 'NONE', ( #52168, #49134, #40425, #60244, #56964, #50722, #62554, #20519, #24039, #469, #2501, #3488, #12470, #1070, #21695, #41379, #59665, #45814, #29695, #21054, #60493, #43413, #37329, #7563, #39270, #45728, #37328, #63201, #54208, #47090, #5117, #39044, #64912, #61734, #27303, #40225, #57830, #1498, #27831, #13678, #52451, #15141, #27178, #3161, #46536, #24146, #26506, #47916, #63773, #55319, #61352, #47642, #4297, #46074, #11950, #52315 ) ) ;
#50284 = CARTESIAN_POINT ( 'NONE',  ( -15.50000000000000000, -0.2038245569916614930, -21.05662432702600029 ) ) ;
#50286 = VERTEX_POINT ( 'NONE', #8747 ) ;
#50285 = CARTESIAN_POINT ( 'NONE',  ( 30.00000000000000000, -14.04000000000000092, -17.04524521594300523 ) ) ;
#50287 = EDGE_CURVE ( 'NONE', #43460, #38308, #51887, .T. ) ;
#50288 = DIRECTION ( 'NONE',  ( 0.000000000000000000, 0.000000000000000000, -1.000000000000000000 ) ) ;
#50289 = CARTESIAN_POINT ( 'NONE',  ( -6.835476262117334834, -10.50702373788278798, 54.00000000000000711 ) ) ;
#50290 = CARTESIAN_POINT ( 'NONE',  ( -10.03972626211731445, -8.930623737882747548, 26.00000000000000000 ) ) ;
#50291 = CARTESIAN_POINT ( 'NONE',  ( 7.000000000000000000, -39.80000000000000426, 12.69999999999999929 ) ) ;
#50292 = LINE ( 'NONE', #1863, #14537 ) ;
#50293 = VECTOR ( 'NONE', #67627, 1000.000000000000000 ) ;
#50294 = EDGE_LOOP ( 'NONE', ( #54717, #960, #42278, #41445 ) ) ;
#50295 = EDGE_LOOP ( 'NONE', ( #1347, #17217, #52820, #35294, #46031, #44255, #37475, #24617 ) ) ;
#50296 = AXIS2_PLACEMENT_3D ( 'NONE', #4155, #38079, #63893 ) ;
#50297 = FACE_OUTER_BOUND ( 'NONE', #48183, .T. ) ;
#50298 = EDGE_CURVE ( 'NONE', #67535, #61781, #35244, .T. ) ;
#50299 = EDGE_CURVE ( 'NONE', #59438, #66768, #61791, .T. ) ;
#50300 = CARTESIAN_POINT ( 'NONE',  ( 9.690000000000001279, 9.750000000000001776, -7.000000000000000000 ) ) ;
#50301 = AXIS2_PLACEMENT_3D ( 'NONE', #33740, #56705, #66615 ) ;
#50302 = AXIS2_PLACEMENT_3D ( 'NONE', #58323, #53707, #37105 ) ;
#50303 = AXIS2_PLACEMENT_3D ( 'NONE', #68885, #20784, #42355 ) ;
#50304 = DIRECTION ( 'NONE',  ( -0.8660254037850496633, 0.000000000000000000, -0.4999999999989417909 ) ) ;
#50305 = EDGE_CURVE ( 'NONE', #38230, #39720, #3448, .T. ) ;
#50306 = ORIENTED_EDGE ( 'NONE', *, *, #26792, .F. ) ;
#50307 = LINE ( 'NONE', #1873, #6753 ) ;
#50308 = VERTEX_POINT ( 'NONE', #39854 ) ;
#50309 = ORIENTED_EDGE ( 'NONE', *, *, #5600, .T. ) ;
#50310 = DIRECTION ( 'NONE',  ( -0.000000000000000000, 1.000000000000000000, -0.000000000000000000 ) ) ;
#50311 = FACE_OUTER_BOUND ( 'NONE', #52357, .T. ) ;
#50312 = VECTOR ( 'NONE', #25375, 1000.000000000000000 ) ;
#50313 = CIRCLE ( 'NONE', #25499, 1.000000000000002665 ) ;
#50314 = ORIENTED_EDGE ( 'NONE', *, *, #64107, .T. ) ;
#50315 = DIRECTION ( 'NONE',  ( 1.000000000000000000, -1.047444401652940007E-14, 1.836970198721010706E-16 ) ) ;
#50316 = VECTOR ( 'NONE', #1314, 1000.000000000000000 ) ;
#50317 = DIRECTION ( 'NONE',  ( -1.000000000000000000, 0.000000000000000000, 0.000000000000000000 ) ) ;
#50318 = DIRECTION ( 'NONE',  ( 0.000000000000000000, 0.000000000000000000, -1.000000000000000000 ) ) ;
#50319 = VERTEX_POINT ( 'NONE', #67794 ) ;
#50321 = VERTEX_POINT ( 'NONE', #51538 ) ;
#50320 = DIRECTION ( 'NONE',  ( 0.000000000000000000, 0.000000000000000000, -1.000000000000000000 ) ) ;
#50322 = CIRCLE ( 'NONE', #44653, 0.1999999999999987899 ) ;
#50323 = DIRECTION ( 'NONE',  ( -1.000000000000000000, 0.000000000000000000, 0.000000000000000000 ) ) ;
#50324 = DIRECTION ( 'NONE',  ( -0.000000000000000000, -0.000000000000000000, -1.000000000000000000 ) ) ;
#50325 = CARTESIAN_POINT ( 'NONE',  ( -9.828310488886049967, -2.290483450353357320, 455.0000000000000568 ) ) ;
#50326 = CARTESIAN_POINT ( 'NONE',  ( 25.57999999999999829, 0.000000000000000000, 5.250000000000000000 ) ) ;
#50327 = AXIS2_PLACEMENT_3D ( 'NONE', #55856, #55519, #28631 ) ;
#50328 = CYLINDRICAL_SURFACE ( 'NONE', #40100, 1.399999999999999245 ) ;
#50329 = DIRECTION ( 'NONE',  ( 1.000000000000000000, -5.981805089575194965E-17, 0.000000000000000000 ) ) ;
#50330 = ORIENTED_EDGE ( 'NONE', *, *, #18671, .F. ) ;
#50331 = EDGE_LOOP ( 'NONE', ( #11447, #11255, #52993, #32344 ) ) ;
#50332 = VERTEX_POINT ( 'NONE', #51176 ) ;
#50333 = LINE ( 'NONE', #23469, #48013 ) ;
#50334 = CARTESIAN_POINT ( 'NONE',  ( -13.00000000000000178, -15.50000000000000000, 14.50000000000000000 ) ) ;
#50335 = CARTESIAN_POINT ( 'NONE',  ( -6.344366288193437953, -5.793274621760813758, 54.00000000000000711 ) ) ;
#50336 = VERTEX_POINT ( 'NONE', #12980 ) ;
#50337 = ORIENTED_EDGE ( 'NONE', *, *, #282, .T. ) ;
#50338 = EDGE_LOOP ( 'NONE', ( #6330, #41129, #62074, #49247, #69557, #8762, #12355, #8488 ) ) ;
#50339 = ADVANCED_FACE ( 'NONE', ( #67455 ), #8380, .T. ) ;
#50340 = ADVANCED_FACE ( 'NONE', ( #24308 ), #3101, .F. ) ;
#50341 = EDGE_CURVE ( 'NONE', #52963, #15214, #46219, .T. ) ;
#50342 = DIRECTION ( 'NONE',  ( 0.000000000000000000, 0.000000000000000000, 1.000000000000000000 ) ) ;
#50343 = ORIENTED_EDGE ( 'NONE', *, *, #27494, .F. ) ;
#50344 = AXIS2_PLACEMENT_3D ( 'NONE', #17882, #45439, #39783 ) ;
#50345 = ORIENTED_EDGE ( 'NONE', *, *, #44954, .F. ) ;
#50346 = ADVANCED_FACE ( 'NONE', ( #57188 ), #41263, .F. ) ;
#50347 = VERTEX_POINT ( 'NONE', #28910 ) ;
#50348 = ORIENTED_EDGE ( 'NONE', *, *, #60245, .F. ) ;
#50349 = CIRCLE ( 'NONE', #15394, 0.5000000000001357803 ) ;
#50350 = LINE ( 'NONE', #11475, #40670 ) ;
#50352 = ORIENTED_EDGE ( 'NONE', *, *, #39260, .F. ) ;
#50351 = CARTESIAN_POINT ( 'NONE',  ( 34.89999999999999858, 13.66939075806899950, 20.80000000000000426 ) ) ;
#50353 = LINE ( 'NONE', #19230, #9761 ) ;
#50354 = AXIS2_PLACEMENT_3D ( 'NONE', #39316, #66532, #13125 ) ;
#50355 = AXIS2_PLACEMENT_3D ( 'NONE', #54661, #28130, #65612 ) ;
#50356 = AXIS2_PLACEMENT_3D ( 'NONE', #29382, #39311, #51305 ) ;
#50357 = CARTESIAN_POINT ( 'NONE',  ( 283.0000000000000568, -39.80000000000000426, 8.400000000000000355 ) ) ;
#50358 = DIRECTION ( 'NONE',  ( -1.000000000000000000, 0.000000000000000000, 0.000000000000000000 ) ) ;
#50360 = EDGE_LOOP ( 'NONE', ( #4949, #23618, #41747, #47401 ) ) ;
#50359 = DIRECTION ( 'NONE',  ( 0.9583148474998870459, 0.000000000000000000, -0.2857142857143623593 ) ) ;
#50361 = VECTOR ( 'NONE', #42978, 1000.000000000000000 ) ;
#50362 = VECTOR ( 'NONE', #27998, 1000.000000000000000 ) ;
#50363 = CIRCLE ( 'NONE', #59413, 24.99999999998794920 ) ;
#50364 = CARTESIAN_POINT ( 'NONE',  ( -5.993516549646711766, 5.993516549646603409, 195.0000000000000284 ) ) ;
#50365 = CARTESIAN_POINT ( 'NONE',  ( -10.30047626211729472, -6.849523737882750929, 54.00000000000000711 ) ) ;
#50366 = CARTESIAN_POINT ( 'NONE',  ( -15.50000000000000000, -2.500000000000000000, 23.94337567297399971 ) ) ;
#50367 = CIRCLE ( 'NONE', #67339, 1.000000000000000000 ) ;
#50368 = EDGE_CURVE ( 'NONE', #5249, #4384, #47978, .T. ) ;
#50369 = ORIENTED_EDGE ( 'NONE', *, *, #13231, .F. ) ;
#50370 = DIRECTION ( 'NONE',  ( 0.000000000000000000, 1.000000000000000000, 0.000000000000000000 ) ) ;
#50371 = CARTESIAN_POINT ( 'NONE',  ( 41.09999999999999432, 13.66939075806899950, 20.80000000000000426 ) ) ;
#50372 = CARTESIAN_POINT ( 'NONE',  ( 8.835729544836331328, 7.955476262117188391, 54.00000000000000711 ) ) ;
#50373 = ORIENTED_EDGE ( 'NONE', *, *, #66481, .F. ) ;
#50374 = COLOUR_RGB ( '', 0.40784314, 0.44705882, 0.49803922) ;
#50375 = FACE_OUTER_BOUND ( 'NONE', #43652, .T. ) ;
#50376 = FACE_OUTER_BOUND ( 'NONE', #46945, .T. ) ;
#50377 = CARTESIAN_POINT ( 'NONE',  ( 13.90000000000000213, 20.60000000000000142, -13.86939075806900057 ) ) ;
#50378 = ORIENTED_EDGE ( 'NONE', *, *, #69320, .F. ) ;
#50379 = CARTESIAN_POINT ( 'NONE',  ( -4.173516549646669738, 11.77351654964658678, 195.0000000000000284 ) ) ;
#50380 = CARTESIAN_POINT ( 'NONE',  ( 39.00000000000000000, 14.08845687959340331, -21.00000000000000000 ) ) ;
#50381 = DIRECTION ( 'NONE',  ( -1.000000000000000000, 0.000000000000000000, 0.000000000000000000 ) ) ;
#50382 = DIRECTION ( 'NONE',  ( 0.000000000000000000, 0.000000000000000000, 1.000000000000000000 ) ) ;
#50383 = EDGE_CURVE ( 'NONE', #41191, #21453, #35001, .T. ) ;
#50384 = ADVANCED_FACE ( 'NONE', ( #25364 ), #63551, .T. ) ;
#50385 = ORIENTED_EDGE ( 'NONE', *, *, #15445, .T. ) ;
#50386 = CARTESIAN_POINT ( 'NONE',  ( 7.000000000000000000, -38.15000000000000568, -14.50000000000000000 ) ) ;
#50387 = FACE_OUTER_BOUND ( 'NONE', #25838, .T. ) ;
#50388 = ADVANCED_FACE ( 'NONE', ( #9815 ), #30667, .F. ) ;
#50389 = CIRCLE ( 'NONE', #19913, 0.4999999999979497511 ) ;
#50390 = DIRECTION ( 'NONE',  ( 1.836970198721029934E-16, 1.836970198721010706E-16, -1.000000000000000000 ) ) ;
#50391 = DIRECTION ( 'NONE',  ( -1.000000000000000000, 0.000000000000000000, 0.000000000000000000 ) ) ;
#50392 = DIRECTION ( 'NONE',  ( -1.000000000000000000, 0.000000000000000000, 0.000000000000000000 ) ) ;
#50393 = ORIENTED_EDGE ( 'NONE', *, *, #40536, .F. ) ;
#50394 = CARTESIAN_POINT ( 'NONE',  ( -10.49297626211726175, 6.835476262117182955, 54.00000000000000711 ) ) ;
#50395 = PLANE ( 'NONE',  #40658 ) ;
#50396 = EDGE_CURVE ( 'NONE', #62286, #45123, #5200, .T. ) ;
#50397 = AXIS2_PLACEMENT_3D ( 'NONE', #55296, #61619, #13188 ) ;
#50398 = DIRECTION ( 'NONE',  ( 0.000000000000000000, 0.000000000000000000, -1.000000000000000000 ) ) ;
#50399 = ADVANCED_FACE ( 'NONE', ( #58937 ), #3794, .F. ) ;
#50400 = AXIS2_PLACEMENT_3D ( 'NONE', #68212, #24730, #31453 ) ;
#50402 = EDGE_CURVE ( 'NONE', #31564, #12232, #69548, .T. ) ;
#50401 = CIRCLE ( 'NONE', #3018, 0.2000000000000005107 ) ;
#50403 = LINE ( 'NONE', #27799, #12796 ) ;
#50404 = ADVANCED_FACE ( 'NONE', ( #41622 ), #52232, .T. ) ;
#50405 = FACE_OUTER_BOUND ( 'NONE', #50622, .T. ) ;
#50406 = ORIENTED_EDGE ( 'NONE', *, *, #196, .F. ) ;
#50408 = ORIENTED_EDGE ( 'NONE', *, *, #41596, .F. ) ;
#50407 = LINE ( 'NONE', #7616, #37506 ) ;
#50409 = EDGE_CURVE ( 'NONE', #56223, #50982, #66659, .T. ) ;
#50410 = VECTOR ( 'NONE', #50574, 1000.000000000000000 ) ;
#50411 = VECTOR ( 'NONE', #45070, 1000.000000000000000 ) ;
#50412 = LINE ( 'NONE', #68068, #40603 ) ;
#50413 = CARTESIAN_POINT ( 'NONE',  ( 8.000000000000001776, -6.879816696376140683, 0.000000000000000000 ) ) ;
#50414 = ORIENTED_EDGE ( 'NONE', *, *, #5649, .T. ) ;
#50415 = VECTOR ( 'NONE', #2885, 1000.000000000000000 ) ;
#50416 = VECTOR ( 'NONE', #52006, 1000.000000000000000 ) ;
#50417 = VECTOR ( 'NONE', #63491, 1000.000000000000000 ) ;
#50418 = CARTESIAN_POINT ( 'NONE',  ( -1.077516549646832189, -11.34648345035347994, 455.0000000000000568 ) ) ;
#50419 = VERTEX_POINT ( 'NONE', #10148 ) ;
#50420 = AXIS2_PLACEMENT_3D ( 'NONE', #66782, #18337, #1398 ) ;
#50421 = CARTESIAN_POINT ( 'NONE',  ( 27.90000000000000213, -21.00000000000000000, 13.86939075806900057 ) ) ;
#50422 = ORIENTED_EDGE ( 'NONE', *, *, #15129, .F. ) ;
#50423 = ORIENTED_EDGE ( 'NONE', *, *, #61405, .F. ) ;
#50424 = DIRECTION ( 'NONE',  ( 0.000000000000000000, 1.000000000000000000, 0.000000000000000000 ) ) ;
#50425 = CARTESIAN_POINT ( 'NONE',  ( -7.250000000000000000, -7.449999999999998401, -23.00000000000000000 ) ) ;
#50426 = DIRECTION ( 'NONE',  ( 0.000000000000000000, 0.000000000000000000, 1.000000000000000000 ) ) ;
#50427 = PLANE ( 'NONE',  #3028 ) ;
#50428 = EDGE_LOOP ( 'NONE', ( #62130, #15568, #48949, #44502 ) ) ;
#50429 = ORIENTED_EDGE ( 'NONE', *, *, #42728, .T. ) ;
#50430 = DIRECTION ( 'NONE',  ( 0.000000000000000000, -1.000000000000000000, 0.000000000000000000 ) ) ;
#50431 = CARTESIAN_POINT ( 'NONE',  ( 49.00000000000000000, -0.2000000000089119934, 8.909539772616881237E-12 ) ) ;
#50432 = ORIENTED_EDGE ( 'NONE', *, *, #6477, .F. ) ;
#50433 = VERTEX_POINT ( 'NONE', #26073 ) ;
#50435 = ORIENTED_EDGE ( 'NONE', *, *, #15523, .T. ) ;
#50434 = ITEM_DEFINED_TRANSFORMATION ( 'NONE', 'NONE', #40310,  #45918 ) ;
#50436 = DIRECTION ( 'NONE',  ( 0.6414496315691617934, 0.7671651518152962090, -0.000000000000000000 ) ) ;
#50438 = VERTEX_POINT ( 'NONE', #21452 ) ;
#50437 = CARTESIAN_POINT ( 'NONE',  ( 275.0000000000000000, -27.13000000000000611, 13.50000000000000000 ) ) ;
#50439 = DIRECTION ( 'NONE',  ( 0.000000000000000000, 0.000000000000000000, -1.000000000000000000 ) ) ;
#50440 = CARTESIAN_POINT ( 'NONE',  ( -7.250000000000000888, -8.249999999999998224, -23.00000000000000000 ) ) ;
#50441 = AXIS2_PLACEMENT_3D ( 'NONE', #69003, #24821, #41074 ) ;
#50442 = ORIENTED_EDGE ( 'NONE', *, *, #17265, .F. ) ;
#50443 = EDGE_LOOP ( 'NONE', ( #2397, #30949, #35614, #20272 ) ) ;
#50444 = EDGE_CURVE ( 'NONE', #45122, #9220, #46917, .T. ) ;
#50445 = STYLED_ITEM ( 'NONE', ( #35396 ), #19195 ) ;
#50446 = DIRECTION ( 'NONE',  ( 0.000000000000000000, 1.000000000000000000, 0.000000000000000000 ) ) ;
#50447 = LINE ( 'NONE', #6621, #7565 ) ;
#50448 = VECTOR ( 'NONE', #59347, 1000.000000000000000 ) ;
#50449 = VECTOR ( 'NONE', #39564, 1000.000000000000000 ) ;
#50450 = ADVANCED_FACE ( 'NONE', ( #42671 ), #36314, .T. ) ;
#50451 = DIRECTION ( 'NONE',  ( 0.000000000000000000, 0.000000000000000000, -1.000000000000000000 ) ) ;
#50452 = VECTOR ( 'NONE', #58228, 1000.000000000000000 ) ;
#50453 = AXIS2_PLACEMENT_3D ( 'NONE', #31430, #31775, #53341 ) ;
#50454 = CARTESIAN_POINT ( 'NONE',  ( -25.50000000000000355, 0.000000000000000000, -22.50000000000000000 ) ) ;
#50455 = DIRECTION ( 'NONE',  ( 0.000000000000000000, 0.000000000000000000, 1.000000000000000000 ) ) ;
#50456 = EDGE_CURVE ( 'NONE', #39125, #60969, #20752, .T. ) ;
#50458 = VERTEX_POINT ( 'NONE', #26415 ) ;
#50457 = CARTESIAN_POINT ( 'NONE',  ( 41.09999999999999432, -21.00000000000000000, -13.86939075806900057 ) ) ;
#50459 = ORIENTED_EDGE ( 'NONE', *, *, #17123, .F. ) ;
#50460 = CARTESIAN_POINT ( 'NONE',  ( 6.657023737882818537, -10.31452373788282095, 54.00000000000000711 ) ) ;
#50461 = VECTOR ( 'NONE', #47231, 1000.000000000000000 ) ;
#50462 = DIRECTION ( 'NONE',  ( -0.000000000000000000, 3.673940397442059868E-16, -1.000000000000000000 ) ) ;
#50463 = DIRECTION ( 'NONE',  ( 1.000000000000000000, -0.000000000000000000, -0.000000000000000000 ) ) ;
#50464 = EDGE_CURVE ( 'NONE', #11065, #47223, #115, .T. ) ;
#50465 = VECTOR ( 'NONE', #5590, 1000.000000000000000 ) ;
#50466 = CARTESIAN_POINT ( 'NONE',  ( -29.50000000000000355, -11.50000000000000000, -15.00000000000000000 ) ) ;
#50467 = ORIENTED_EDGE ( 'NONE', *, *, #35369, .F. ) ;
#50468 = LINE ( 'NONE', #8011, #8711 ) ;
#50469 = DIRECTION ( 'NONE',  ( -1.000000000000000000, 0.000000000000000000, 0.000000000000000000 ) ) ;
#50470 = LINE ( 'NONE', #38815, #24313 ) ;
#50471 = CIRCLE ( 'NONE', #27923, 24.99999999998784972 ) ;
#50472 = ADVANCED_FACE ( 'NONE', ( #25727 ), #10492, .T. ) ;
#50473 = CARTESIAN_POINT ( 'NONE',  ( 6.832023737882812142, 9.897976262117197166, 26.00000000000000711 ) ) ;
#50474 = DIRECTION ( 'NONE',  ( 1.000000000000000000, -0.000000000000000000, 0.000000000000000000 ) ) ;
#50475 = DIRECTION ( 'NONE',  ( 0.4998444328988824181, 0.000000000000000000, -0.8661152018640445593 ) ) ;
#50476 = ORIENTED_EDGE ( 'NONE', *, *, #56129, .T. ) ;
#50477 = DIRECTION ( 'NONE',  ( 0.000000000000000000, -0.7071067811865474617, -0.7071067811865474617 ) ) ;
#50478 = PLANE ( 'NONE',  #66745 ) ;
#50479 = ORIENTED_EDGE ( 'NONE', *, *, #24933, .T. ) ;
#50480 = CYLINDRICAL_SURFACE ( 'NONE', #6321, 0.2000000000000005107 ) ;
#50481 = CARTESIAN_POINT ( 'NONE',  ( -10.08346604330792928, -9.306483450353335130, 195.0000000000000284 ) ) ;
#50482 = CARTESIAN_POINT ( 'NONE',  ( -30.00000000000000000, -12.00000000000000000, 10.20500000000000007 ) ) ;
#50483 = DIRECTION ( 'NONE',  ( 0.000000000000000000, 0.000000000000000000, 1.000000000000000000 ) ) ;
#50484 = ADVANCED_FACE ( 'NONE', ( #41972 ), #15467, .T. ) ;
#50485 = LINE ( 'NONE', #40214, #68898 ) ;
#50486 = VERTEX_POINT ( 'NONE', #58597 ) ;
#50487 = EDGE_CURVE ( 'NONE', #33635, #39125, #5544, .T. ) ;
#50488 = PLANE ( 'NONE',  #69151 ) ;
#50489 = VERTEX_POINT ( 'NONE', #33099 ) ;
#50490 = DIRECTION ( 'NONE',  ( 0.000000000000000000, 0.000000000000000000, 1.000000000000000000 ) ) ;
#50491 = AXIS2_PLACEMENT_3D ( 'NONE', #53368, #4922, #69631 ) ;
#50492 = ORIENTED_EDGE ( 'NONE', *, *, #38008, .T. ) ;
#50493 = LINE ( 'NONE', #7342, #69848 ) ;
#50494 = EDGE_CURVE ( 'NONE', #30798, #57897, #11349, .T. ) ;
#50495 = PLANE ( 'NONE',  #20899 ) ;
#50496 = AXIS2_PLACEMENT_3D ( 'NONE', #40960, #34250, #18336 ) ;
#50497 = AXIS2_PLACEMENT_3D ( 'NONE', #1337, #7313, #55433 ) ;
#50498 = VECTOR ( 'NONE', #51504, 1000.000000000000000 ) ;
#50499 = DIRECTION ( 'NONE',  ( -1.000000000000000000, 0.000000000000000000, 0.000000000000000000 ) ) ;
#50500 = ORIENTED_EDGE ( 'NONE', *, *, #22, .F. ) ;
#50501 = ORIENTED_EDGE ( 'NONE', *, *, #11141, .F. ) ;
#50502 = CARTESIAN_POINT ( 'NONE',  ( 1.634292677759869195, 8.227189898828703107, 26.00000000000000711 ) ) ;
#50503 = ORIENTED_EDGE ( 'NONE', *, *, #34965, .T. ) ;
#50504 = VERTEX_POINT ( 'NONE', #32754 ) ;
#50505 = AXIS2_PLACEMENT_3D ( 'NONE', #33699, #43964, #66232 ) ;
#50506 = VECTOR ( 'NONE', #8618, 1000.000000000000000 ) ;
#50507 = DIRECTION ( 'NONE',  ( 1.034072152899300274E-14, 1.000000000000000000, 0.000000000000000000 ) ) ;
#50508 = DIRECTION ( 'NONE',  ( -1.000000000000000000, 0.000000000000000000, 0.000000000000000000 ) ) ;
#50509 = CYLINDRICAL_SURFACE ( 'NONE', #10711, 4.500000000000188294 ) ;
#50510 = PRODUCT_DEFINITION_FORMATION_WITH_SPECIFIED_SOURCE ( 'ANY', '', #57140, .NOT_KNOWN. ) ;
#50511 = ORIENTED_EDGE ( 'NONE', *, *, #32391, .F. ) ;
#50512 = DIRECTION ( 'NONE',  ( 1.000000000000000000, 0.000000000000000000, 0.000000000000000000 ) ) ;
#50513 = AXIS2_PLACEMENT_3D ( 'NONE', #41375, #3910, #68614 ) ;
#50515 = PLANE ( 'NONE',  #12992 ) ;
#50514 = LINE ( 'NONE', #28247, #38378 ) ;
#50516 = ORIENTED_EDGE ( 'NONE', *, *, #63329, .T. ) ;
#50518 = EDGE_LOOP ( 'NONE', ( #29438, #36135, #4343, #64973 ) ) ;
#50517 = DIRECTION ( 'NONE',  ( 0.000000000000000000, -1.000000000000000000, 0.000000000000000000 ) ) ;
#50519 = ORIENTED_EDGE ( 'NONE', *, *, #47887, .F. ) ;
#50520 = EDGE_CURVE ( 'NONE', #31198, #5559, #55370, .T. ) ;
#50521 = DIRECTION ( 'NONE',  ( -1.000000000000000000, 3.491481338843134144E-15, 0.000000000000000000 ) ) ;
#50522 = ORIENTED_EDGE ( 'NONE', *, *, #22446, .F. ) ;
#50523 = EDGE_CURVE ( 'NONE', #29779, #47005, #23810, .T. ) ;
#50524 = VECTOR ( 'NONE', #69522, 1000.000000000000000 ) ;
#50525 = CARTESIAN_POINT ( 'NONE',  ( 275.0000000000000000, -30.45000000000094786, 14.49999999999906031 ) ) ;
#50526 = DIRECTION ( 'NONE',  ( 0.000000000000000000, 1.000000000000000000, 0.000000000000000000 ) ) ;
#50527 = VERTEX_POINT ( 'NONE', #6912 ) ;
#50528 = ORIENTED_EDGE ( 'NONE', *, *, #64152, .F. ) ;
#50529 = EDGE_CURVE ( 'NONE', #24826, #22518, #38414, .T. ) ;
#50530 = DIRECTION ( 'NONE',  ( 0.000000000000000000, -1.000000000000000000, 0.000000000000000000 ) ) ;
#50531 = ADVANCED_FACE ( 'NONE', ( #54336 ), #16500, .F. ) ;
#50532 = PLANE ( 'NONE',  #9749 ) ;
#50533 = ORIENTED_EDGE ( 'NONE', *, *, #4809, .T. ) ;
#50534 = CARTESIAN_POINT ( 'NONE',  ( -10.08346604330783869, -2.906483450353305020, 195.0000000000000284 ) ) ;
#50535 = LINE ( 'NONE', #33576, #54937 ) ;
#50536 = EDGE_CURVE ( 'NONE', #53899, #26123, #11181, .T. ) ;
#50537 = FACE_BOUND ( 'NONE', #45902, .T. ) ;
#50538 = ORIENTED_EDGE ( 'NONE', *, *, #24933, .F. ) ;
#50539 = PLANE ( 'NONE',  #65167 ) ;
#50540 = DIRECTION ( 'NONE',  ( 0.000000000000000000, 0.000000000000000000, -1.000000000000000000 ) ) ;
#50541 = CIRCLE ( 'NONE', #6548, 0.1749999999999998224 ) ;
#50542 = ADVANCED_FACE ( 'NONE', ( #59969 ), #27454, .F. ) ;
#50544 = EDGE_LOOP ( 'NONE', ( #61090, #35346, #38787, #42426 ) ) ;
#50543 = CARTESIAN_POINT ( 'NONE',  ( 106.4257688009193998, 10.00000000000000000, 282.4830310981789125 ) ) ;
#50546 = ORIENTED_EDGE ( 'NONE', *, *, #27846, .F. ) ;
#50545 = CARTESIAN_POINT ( 'NONE',  ( -25.50000000000000355, -15.12100000000000044, -22.50000000000000000 ) ) ;
#50547 = EDGE_CURVE ( 'NONE', #45122, #66645, #32423, .T. ) ;
#50548 = DIRECTION ( 'NONE',  ( -1.836970198721029934E-16, -1.836970198721010706E-16, 1.000000000000000000 ) ) ;
#50549 = CARTESIAN_POINT ( 'NONE',  ( -3.842976262117221875, 10.30047626211716860, 54.00000000000000711 ) ) ;
#50550 = CARTESIAN_POINT ( 'NONE',  ( 15.50000000000000000, -15.50000000000000000, 22.50000000000000000 ) ) ;
#50551 = EDGE_CURVE ( 'NONE', #23827, #62386, #17180, .T. ) ;
#50552 = ADVANCED_FACE ( 'NONE', ( #28474 ), #59635, .F. ) ;
#50553 = FACE_OUTER_BOUND ( 'NONE', #57370, .T. ) ;
#50554 = CARTESIAN_POINT ( 'NONE',  ( 3.552713678800500929E-15, -0.4999999999999964473, 26.50000000000000355 ) ) ;
#50555 = VERTEX_POINT ( 'NONE', #28142 ) ;
#50556 = DIRECTION ( 'NONE',  ( 0.000000000000000000, 0.000000000000000000, 1.000000000000000000 ) ) ;
#50557 = CARTESIAN_POINT ( 'NONE',  ( 30.00000000000000000, -9.200000000000120082, 17.30000000000000071 ) ) ;
#50558 = EDGE_CURVE ( 'NONE', #58112, #26502, #27108, .T. ) ;
#50559 = CARTESIAN_POINT ( 'NONE',  ( 3.157023737882800773, 5.242976262117208464, 54.00000000000000711 ) ) ;
#50560 = VECTOR ( 'NONE', #69737, 1000.000000000000000 ) ;
#50563 = ORIENTED_EDGE ( 'NONE', *, *, #62701, .F. ) ;
#50562 = LINE ( 'NONE', #6049, #46819 ) ;
#50561 = CIRCLE ( 'NONE', #35875, 1.000000000000000000 ) ;
#50564 = LINE ( 'NONE', #18360, #59495 ) ;
#50565 = VECTOR ( 'NONE', #28623, 1000.000000000000000 ) ;
#50566 = CARTESIAN_POINT ( 'NONE',  ( -7.450000000000001954, 0.000000000000000000, -20.50000000000000000 ) ) ;
#50567 = VECTOR ( 'NONE', #4049, 1000.000000000000000 ) ;
#50568 = CIRCLE ( 'NONE', #17810, 0.5249999999999994671 ) ;
#50569 = EDGE_LOOP ( 'NONE', ( #65353, #26278, #40010, #40191 ) ) ;
#50570 = CARTESIAN_POINT ( 'NONE',  ( -8.079219948824961861, -8.711985858128649340, 54.00000000000000711 ) ) ;
#50571 = DIRECTION ( 'NONE',  ( 0.000000000000000000, 1.000000000000000000, 0.000000000000000000 ) ) ;
#50572 = ORIENTED_EDGE ( 'NONE', *, *, #69655, .F. ) ;
#50573 = CARTESIAN_POINT ( 'NONE',  ( 11.00000000000000000, -11.50000000000000000, -15.00000000000000000 ) ) ;
#50574 = DIRECTION ( 'NONE',  ( -0.000000000000000000, -1.000000000000000000, 0.000000000000000000 ) ) ;
#50575 = CARTESIAN_POINT ( 'NONE',  ( -6.350872789121327244, 6.822336235477381550, 26.00000000000000711 ) ) ;
#50576 = EDGE_CURVE ( 'NONE', #62061, #22868, #65626, .T. ) ;
#50577 = DIRECTION ( 'NONE',  ( 0.7671651518153131954, 0.6414496315691415873, 2.587583378555109562E-16 ) ) ;
#50578 = EDGE_CURVE ( 'NONE', #43565, #16217, #35053, .T. ) ;
#50579 = CIRCLE ( 'NONE', #49475, 8.000000000000000000 ) ;
#50580 = CARTESIAN_POINT ( 'NONE',  ( 275.0000000000000000, -40.30000000000000426, -12.20000000000000107 ) ) ;
#50581 = VERTEX_POINT ( 'NONE', #22154 ) ;
#50582 = DIRECTION ( 'NONE',  ( 0.000000000000000000, 1.000000000000000000, 0.000000000000000000 ) ) ;
#50583 = ORIENTED_EDGE ( 'NONE', *, *, #65791, .F. ) ;
#50584 = ORIENTED_EDGE ( 'NONE', *, *, #45695, .F. ) ;
#50585 = CARTESIAN_POINT ( 'NONE',  ( 30.00000000000000000, -11.70000000000000284, 12.50000000000000000 ) ) ;
#50586 = PLANE ( 'NONE',  #69409 ) ;
#50588 = CARTESIAN_POINT ( 'NONE',  ( 49.00000000000000000, 13.66939075806899950, 20.80000000000000426 ) ) ;
#50587 = DIRECTION ( 'NONE',  ( 1.000000000000000000, 0.000000000000000000, 0.000000000000000000 ) ) ;
#50589 = ORIENTED_EDGE ( 'NONE', *, *, #8803, .F. ) ;
#50590 = VERTEX_POINT ( 'NONE', #33451 ) ;
#50591 = CARTESIAN_POINT ( 'NONE',  ( 11.32648345035340576, 7.793516549646564151, 455.0000000000000568 ) ) ;
#50592 = VERTEX_POINT ( 'NONE', #55039 ) ;
#50593 = FACE_OUTER_BOUND ( 'NONE', #23825, .T. ) ;
#50594 = CARTESIAN_POINT ( 'NONE',  ( -7.450000000000001954, -7.249999999999998224, -22.50000000000000000 ) ) ;
#50595 = CARTESIAN_POINT ( 'NONE',  ( -8.250000000000001776, 7.250000000000000888, -26.00000000000001066 ) ) ;
#50596 = AXIS2_PLACEMENT_3D ( 'NONE', #406, #21967, #43876 ) ;
#50597 = DIRECTION ( 'NONE',  ( -1.000000000000000000, 0.000000000000000000, 0.000000000000000000 ) ) ;
#50599 = CARTESIAN_POINT ( 'NONE',  ( 33.89999999999999858, -0.1999999999911795112, 8.826273045769999343E-12 ) ) ;
#50598 = DIRECTION ( 'NONE',  ( 0.000000000000000000, 0.000000000000000000, 1.000000000000000000 ) ) ;
#50600 = ORIENTED_EDGE ( 'NONE', *, *, #12040, .T. ) ;
#50602 = ORIENTED_EDGE ( 'NONE', *, *, #17065, .F. ) ;
#50601 = FACE_OUTER_BOUND ( 'NONE', #49292, .T. ) ;
#50603 = EDGE_LOOP ( 'NONE', ( #68873, #37364, #16031, #19367, #19340, #53744 ) ) ;
#50604 = ORIENTED_EDGE ( 'NONE', *, *, #17161, .F. ) ;
#50605 = CARTESIAN_POINT ( 'NONE',  ( -8.750000000000001776, -7.249999999999998224, -30.00000000000001066 ) ) ;
#50606 = VECTOR ( 'NONE', #14502, 1000.000000000000000 ) ;
#50607 = EDGE_CURVE ( 'NONE', #14411, #28648, #11866, .T. ) ;
#50608 = CARTESIAN_POINT ( 'NONE',  ( -8.250000000000001776, -7.249999999999998224, -26.00000000000001066 ) ) ;
#50609 = VERTEX_POINT ( 'NONE', #60309 ) ;
#50610 = ORIENTED_EDGE ( 'NONE', *, *, #35378, .F. ) ;
#50611 = EDGE_CURVE ( 'NONE', #55024, #12559, #239, .T. ) ;
#50612 = CIRCLE ( 'NONE', #29154, 0.5000000000079367624 ) ;
#50613 = CARTESIAN_POINT ( 'NONE',  ( 283.0000000000000568, -37.61196062927500350, 8.008708659369300875 ) ) ;
#50614 = EDGE_CURVE ( 'NONE', #44864, #23372, #47493, .T. ) ;
#50615 = CYLINDRICAL_SURFACE ( 'NONE', #13038, 2.458500000000000796 ) ;
#50616 = ORIENTED_EDGE ( 'NONE', *, *, #11169, .F. ) ;
#50617 = EDGE_LOOP ( 'NONE', ( #45364, #29300, #13700, #64304 ) ) ;
#50618 = DIRECTION ( 'NONE',  ( 0.000000000000000000, 1.000000000000000000, 0.000000000000000000 ) ) ;
#50619 = EDGE_CURVE ( 'NONE', #69217, #10277, #32796, .T. ) ;
#50620 = ADVANCED_FACE ( 'NONE', ( #61340 ), #42992, .T. ) ;
#50621 = DIRECTION ( 'NONE',  ( -1.836970198721029934E-16, 1.836970198721036344E-16, -1.000000000000000000 ) ) ;
#50622 = EDGE_LOOP ( 'NONE', ( #18220, #16987, #29397 ) ) ;
#50623 = VECTOR ( 'NONE', #68398, 1000.000000000000000 ) ;
#50624 = CARTESIAN_POINT ( 'NONE',  ( 111.9257688011037146, 10.00000000000000000, 335.4830310981152479 ) ) ;
#50626 = ORIENTED_EDGE ( 'NONE', *, *, #30616, .F. ) ;
#50625 = DIRECTION ( 'NONE',  ( -1.000000000000000000, 0.000000000000000000, 0.000000000000000000 ) ) ;
#50627 = ORIENTED_EDGE ( 'NONE', *, *, #66432, .F. ) ;
#50628 = DIRECTION ( 'NONE',  ( -2.135044278125301343E-15, 1.000000000000000000, 0.000000000000000000 ) ) ;
#50629 = DIRECTION ( 'NONE',  ( 0.5000000000000004441, -0.8660254037844383745, 0.000000000000000000 ) ) ;
#50630 = CARTESIAN_POINT ( 'NONE',  ( 5.668387132715968058, 8.393516549646582448, 455.0000000000000568 ) ) ;
#50631 = CARTESIAN_POINT ( 'NONE',  ( -8.393516549646712122, 6.331612867284047041, 195.0000000000000284 ) ) ;
#50632 = FACE_OUTER_BOUND ( 'NONE', #40519, .T. ) ;
#50633 = LINE ( 'NONE', #40002, #41797 ) ;
#50634 = CYLINDRICAL_SURFACE ( 'NONE', #42633, 0.6000000000000003109 ) ;
#50635 = ORIENTED_EDGE ( 'NONE', *, *, #18726, .T. ) ;
#50636 = LINE ( 'NONE', #3601, #33747 ) ;
#50638 = EDGE_LOOP ( 'NONE', ( #48992, #24554, #65917, #8432 ) ) ;
#50637 = CARTESIAN_POINT ( 'NONE',  ( -16.75000000000000000, -2.500000000000000000, 23.22168783648699986 ) ) ;
#50639 = DIRECTION ( 'NONE',  ( 0.000000000000000000, 1.000000000000000000, 0.000000000000000000 ) ) ;
#50640 = FACE_OUTER_BOUND ( 'NONE', #15764, .T. ) ;
#50641 = LINE ( 'NONE', #45674, #53966 ) ;
#50642 = CARTESIAN_POINT ( 'NONE',  ( -30.00000000000000000, -10.85999999999999943, -9.350000000000269651 ) ) ;
#50643 = DIRECTION ( 'NONE',  ( 0.000000000000000000, 1.000000000000000000, 0.000000000000000000 ) ) ;
#50644 = ORIENTED_EDGE ( 'NONE', *, *, #56535, .F. ) ;
#50645 = ORIENTED_EDGE ( 'NONE', *, *, #64188, .F. ) ;
#50646 = CARTESIAN_POINT ( 'NONE',  ( -5.242976262117280406, -5.257023737882805747, 54.00000000000000711 ) ) ;
#50647 = AXIS2_PLACEMENT_3D ( 'NONE', #46574, #42326, #19696 ) ;
#50648 = EDGE_CURVE ( 'NONE', #20701, #16704, #39775, .T. ) ;
#50649 = CARTESIAN_POINT ( 'NONE',  ( -7.250000000000000000, -7.449999999999998401, -16.00000000000000000 ) ) ;
#50650 = ORIENTED_EDGE ( 'NONE', *, *, #4303, .F. ) ;
#50651 = CARTESIAN_POINT ( 'NONE',  ( -7.798499376344150136, -7.272650909786627871, 195.0000000000000284 ) ) ;
#50652 = ORIENTED_EDGE ( 'NONE', *, *, #41933, .T. ) ;
#50653 = EDGE_CURVE ( 'NONE', #46863, #49899, #50741, .T. ) ;
#50654 = ORIENTED_EDGE ( 'NONE', *, *, #41234, .T. ) ;
#50655 = AXIS2_PLACEMENT_3D ( 'NONE', #25069, #46619, #34257 ) ;
#50656 = CARTESIAN_POINT ( 'NONE',  ( 25.50000000000000355, -5.578999999999999737, -20.87899999999999778 ) ) ;
#50657 = CYLINDRICAL_SURFACE ( 'NONE', #45473, 1.000000000000000000 ) ;
#50658 = ORIENTED_EDGE ( 'NONE', *, *, #65382, .T. ) ;
#50659 = CARTESIAN_POINT ( 'NONE',  ( 10.74648345035337904, -1.690483450353395201, 195.0000000000000284 ) ) ;
#50660 = DIRECTION ( 'NONE',  ( 0.000000000000000000, 1.000000000000000000, 0.000000000000000000 ) ) ;
#50661 = DIRECTION ( 'NONE',  ( -0.7671651518153043137, 0.6414496315691521344, 2.587583378555129776E-16 ) ) ;
#50662 = ORIENTED_EDGE ( 'NONE', *, *, #52563, .F. ) ;
#50663 = ORIENTED_EDGE ( 'NONE', *, *, #9778, .T. ) ;
#50665 = VERTEX_POINT ( 'NONE', #35521 ) ;
#50664 = DIRECTION ( 'NONE',  ( 0.000000000000000000, 1.000000000000000000, 0.000000000000000000 ) ) ;
#50666 = ORIENTED_EDGE ( 'NONE', *, *, #38430, .T. ) ;
#50667 = AXIS2_PLACEMENT_3D ( 'NONE', #18451, #24118, #40016 ) ;
#50668 = LINE ( 'NONE', #3283, #7737 ) ;
#50669 = LINE ( 'NONE', #1888, #4537 ) ;
#50670 = CYLINDRICAL_SURFACE ( 'NONE', #50397, 0.2000000000000005107 ) ;
#50671 = CYLINDRICAL_SURFACE ( 'NONE', #5957, 1.929199999999998916 ) ;
#50672 = CARTESIAN_POINT ( 'NONE',  ( 7.000000000000000000, -42.50000000000000000, 15.10000000000000142 ) ) ;
#50673 = CARTESIAN_POINT ( 'NONE',  ( -7.415254214038336400, 2.993516549646603853, 455.0000000000000568 ) ) ;
#50674 = ORIENTED_EDGE ( 'NONE', *, *, #37103, .F. ) ;
#50675 = ORIENTED_EDGE ( 'NONE', *, *, #12729, .T. ) ;
#50676 = EDGE_LOOP ( 'NONE', ( #56838, #860, #3319, #55989 ) ) ;
#50677 = CARTESIAN_POINT ( 'NONE',  ( 4.255011587777221216, 8.452095193409324025, 195.0000000000000284 ) ) ;
#50678 = DIRECTION ( 'NONE',  ( -0.000000000000000000, 3.673940397442059868E-16, -1.000000000000000000 ) ) ;
#50679 = LINE ( 'NONE', #2595, #25889 ) ;
#50680 =( NAMED_UNIT ( * ) SI_UNIT ( $, .STERADIAN. ) SOLID_ANGLE_UNIT ( ) );
#50681 = EDGE_CURVE ( 'NONE', #42591, #55218, #45433, .T. ) ;
#50682 = EDGE_LOOP ( 'NONE', ( #60804, #50626, #44164, #69043, #25729 ) ) ;
#50683 = VERTEX_POINT ( 'NONE', #40836 ) ;
#50684 = ORIENTED_EDGE ( 'NONE', *, *, #61458, .T. ) ;
#50685 = DIRECTION ( 'NONE',  ( 0.000000000000000000, 0.000000000000000000, 1.000000000000000000 ) ) ;
#50686 = ORIENTED_EDGE ( 'NONE', *, *, #31104, .F. ) ;
#50687 = ORIENTED_EDGE ( 'NONE', *, *, #28703, .F. ) ;
#50688 = EDGE_CURVE ( 'NONE', #69932, #69253, #66661, .T. ) ;
#50689 = ADVANCED_FACE ( 'NONE', ( #34465 ), #8301, .T. ) ;
#50690 = ORIENTED_EDGE ( 'NONE', *, *, #48235, .F. ) ;
#50691 = AXIS2_PLACEMENT_3D ( 'NONE', #32354, #48617, #69481 ) ;
#50692 = EDGE_LOOP ( 'NONE', ( #58020, #39713, #64111, #23659 ) ) ;
#50693 = CARTESIAN_POINT ( 'NONE',  ( 7.900000000000000355, 18.00000000000000355, -21.00000000000000000 ) ) ;
#50694 = EDGE_CURVE ( 'NONE', #62756, #8699, #51096, .T. ) ;
#50695 = EDGE_CURVE ( 'NONE', #26381, #28340, #39437, .T. ) ;
#50697 = ORIENTED_EDGE ( 'NONE', *, *, #69269, .T. ) ;
#50696 = DIRECTION ( 'NONE',  ( -1.000000000000000000, 0.000000000000000000, 0.000000000000000000 ) ) ;
#50698 = VECTOR ( 'NONE', #6429, 1000.000000000000000 ) ;
#50699 = DIRECTION ( 'NONE',  ( 0.000000000000000000, 0.000000000000000000, 1.000000000000000000 ) ) ;
#50700 = CARTESIAN_POINT ( 'NONE',  ( -9.690000000000001279, 9.750000000000001776, -5.000000000000000000 ) ) ;
#50701 = EDGE_CURVE ( 'NONE', #45421, #54092, #45084, .T. ) ;
#50702 = DIRECTION ( 'NONE',  ( 0.000000000000000000, 0.000000000000000000, -1.000000000000000000 ) ) ;
#50704 = ORIENTED_EDGE ( 'NONE', *, *, #40175, .F. ) ;
#50703 = DIRECTION ( 'NONE',  ( -0.000000000000000000, 0.000000000000000000, 1.000000000000000000 ) ) ;
#50705 = VERTEX_POINT ( 'NONE', #18929 ) ;
#50706 = VECTOR ( 'NONE', #66548, 1000.000000000000000 ) ;
#50707 = CARTESIAN_POINT ( 'NONE',  ( 25.50000000000000355, -5.578999999999999737, 20.87900000000000134 ) ) ;
#50708 = PLANE ( 'NONE',  #62782 ) ;
#50709 = AXIS2_PLACEMENT_3D ( 'NONE', #53957, #37341, #27071 ) ;
#50710 = FACE_OUTER_BOUND ( 'NONE', #22690, .T. ) ;
#50711 = ORIENTED_EDGE ( 'NONE', *, *, #23519, .F. ) ;
#50712 = CARTESIAN_POINT ( 'NONE',  ( 105.8309041053263257, 3.657408540445008960, 10.00000000000000000 ) ) ;
#50714 = AXIS2_PLACEMENT_3D ( 'NONE', #48216, #26292, #59857 ) ;
#50713 = AXIS2_PLACEMENT_3D ( 'NONE', #9802, #16487, #22824 ) ;
#50715 = CARTESIAN_POINT ( 'NONE',  ( -11.77351654964674310, -4.406483450353321452, 455.0000000000000568 ) ) ;
#50716 = DIRECTION ( 'NONE',  ( 0.000000000000000000, -0.7084617869615144059, 0.7057491738679528837 ) ) ;
#50717 = ORIENTED_EDGE ( 'NONE', *, *, #13790, .T. ) ;
#50718 = DIRECTION ( 'NONE',  ( -1.000000000000000000, 0.000000000000000000, 0.000000000000000000 ) ) ;
#50719 = VECTOR ( 'NONE', #65770, 1000.000000000000000 ) ;
#50720 = CARTESIAN_POINT ( 'NONE',  ( 8.250000000000005329, 0.000000000000000000, -16.00000000000000000 ) ) ;
#50721 = CARTESIAN_POINT ( 'NONE',  ( -11.11351654964671631, -2.906483450353335218, 455.0000000000000568 ) ) ;
#50722 = ORIENTED_EDGE ( 'NONE', *, *, #57567, .T. ) ;
#50723 =( NAMED_UNIT ( * ) PLANE_ANGLE_UNIT ( ) SI_UNIT ( $, .RADIAN. ) );
#50724 = FACE_OUTER_BOUND ( 'NONE', #5136, .T. ) ;
#50725 = DIRECTION ( 'NONE',  ( 1.000000000000000000, 0.000000000000000000, 0.000000000000000000 ) ) ;
#50726 = PLANE ( 'NONE',  #60553 ) ;
#50727 = ORIENTED_EDGE ( 'NONE', *, *, #49285, .F. ) ;
#50728 = CARTESIAN_POINT ( 'NONE',  ( 15.50000000000000000, -0.1999999999999999556, -21.05000000000000426 ) ) ;
#50729 = DIRECTION ( 'NONE',  ( 0.000000000000000000, 0.000000000000000000, 1.000000000000000000 ) ) ;
#50730 = DIRECTION ( 'NONE',  ( -0.7071067811865530128, -0.7071067811865421326, 0.000000000000000000 ) ) ;
#50731 = EDGE_CURVE ( 'NONE', #5641, #33487, #2652, .T. ) ;
#50732 = EDGE_CURVE ( 'NONE', #49441, #14815, #67370, .T. ) ;
#50733 = CARTESIAN_POINT ( 'NONE',  ( 7.852485183456877849, 3.417780618358537748, 195.0000000000000284 ) ) ;
#50734 = CARTESIAN_POINT ( 'NONE',  ( -7.450000000000001954, -7.249999999999998224, -16.00000000000000000 ) ) ;
#50735 = ORIENTED_EDGE ( 'NONE', *, *, #67381, .F. ) ;
#50736 = CARTESIAN_POINT ( 'NONE',  ( 4.206483450353343478, -11.12648345035347575, 455.0000000000000568 ) ) ;
#50737 = LINE ( 'NONE', #40833, #48599 ) ;
#50738 = PLANE ( 'NONE',  #45801 ) ;
#50739 = ADVANCED_FACE ( 'NONE', ( #30243 ), #51802, .F. ) ;
#50740 = PRESENTATION_STYLE_ASSIGNMENT (( #30242 ) ) ;
#50741 = LINE ( 'NONE', #56747, #4605 ) ;
#50742 = ORIENTED_EDGE ( 'NONE', *, *, #21697, .F. ) ;
#50743 = VECTOR ( 'NONE', #56404, 1000.000000000000000 ) ;
#50745 = ORIENTED_EDGE ( 'NONE', *, *, #26575, .F. ) ;
#50744 = PLANE ( 'NONE',  #62311 ) ;
#50746 = VECTOR ( 'NONE', #57989, 1000.000000000000000 ) ;
#50747 = DIRECTION ( 'NONE',  ( 1.079558018506126625E-14, 1.000000000000000000, 1.836970198721016622E-16 ) ) ;
#50748 = DIRECTION ( 'NONE',  ( 0.000000000000000000, -1.901256929667050114E-12, 1.000000000000000000 ) ) ;
#50749 = VERTEX_POINT ( 'NONE', #34123 ) ;
#50750 = AXIS2_PLACEMENT_3D ( 'NONE', #34973, #66804, #2458 ) ;
#50751 = DIRECTION ( 'NONE',  ( 0.000000000000000000, 1.000000000000000000, 0.000000000000000000 ) ) ;
#50752 = ORIENTED_EDGE ( 'NONE', *, *, #21520, .F. ) ;
#50753 = AXIS2_PLACEMENT_3D ( 'NONE', #31117, #21537, #68592 ) ;
#50754 = DIRECTION ( 'NONE',  ( 0.000000000000000000, 0.000000000000000000, -1.000000000000000000 ) ) ;
#50755 = ORIENTED_EDGE ( 'NONE', *, *, #57006, .T. ) ;
#50756 = ORIENTED_EDGE ( 'NONE', *, *, #53998, .F. ) ;
#50757 = LINE ( 'NONE', #17195, #12539 ) ;
#50758 = FACE_OUTER_BOUND ( 'NONE', #10527, .T. ) ;
#50759 = AXIS2_PLACEMENT_3D ( 'NONE', #42576, #58143, #25268 ) ;
#50760 = FACE_OUTER_BOUND ( 'NONE', #20769, .T. ) ;
#50761 = CARTESIAN_POINT ( 'NONE',  ( 7.250000000000005329, 8.250000000000001776, -26.00000000000001066 ) ) ;
#50762 = VERTEX_POINT ( 'NONE', #29527 ) ;
#50763 = ORIENTED_EDGE ( 'NONE', *, *, #61282, .F. ) ;
#50764 = FACE_OUTER_BOUND ( 'NONE', #43542, .T. ) ;
#50766 = LINE ( 'NONE', #2681, #21461 ) ;
#50765 = AXIS2_PLACEMENT_3D ( 'NONE', #38714, #1573, #44015 ) ;
#50767 = EDGE_LOOP ( 'NONE', ( #51755, #6740, #36529, #19329 ) ) ;
#50768 = VERTEX_POINT ( 'NONE', #56398 ) ;
#50769 = ORIENTED_EDGE ( 'NONE', *, *, #9444, .F. ) ;
#50770 = DIRECTION ( 'NONE',  ( 0.000000000000000000, -1.000000000000000000, -7.802196388977322746E-10 ) ) ;
#50771 = EDGE_CURVE ( 'NONE', #34259, #8834, #45790, .T. ) ;
#50773 = VERTEX_POINT ( 'NONE', #3361 ) ;
#50772 = DIRECTION ( 'NONE',  ( 2.135044278125299371E-15, -1.000000000000000000, -3.673940397442060361E-16 ) ) ;
#50774 = EDGE_CURVE ( 'NONE', #24992, #16139, #28819, .T. ) ;
#50775 = DIRECTION ( 'NONE',  ( -0.5000000000000038858, -0.8660254037844363761, 0.000000000000000000 ) ) ;
#50776 = CARTESIAN_POINT ( 'NONE',  ( -10.91351654964680584, -9.106483450353376696, 455.0000000000000568 ) ) ;
#50777 = EDGE_CURVE ( 'NONE', #14914, #35164, #3020, .T. ) ;
#50778 = CIRCLE ( 'NONE', #29325, 0.3499999999999295341 ) ;
#50779 = ADVANCED_FACE ( 'NONE', ( #50405 ), #23530, .F. ) ;
#50780 = ORIENTED_EDGE ( 'NONE', *, *, #4897, .F. ) ;
#50781 = EDGE_LOOP ( 'NONE', ( #35271, #33501, #12316, #8439 ) ) ;
#50782 = EDGE_CURVE ( 'NONE', #32093, #31208, #4076, .T. ) ;
#50783 = CARTESIAN_POINT ( 'NONE',  ( -11.00000000000000000, -11.50000000000100009, 15.00000000000084910 ) ) ;
#50784 = CARTESIAN_POINT ( 'NONE',  ( -4.947141984184481700, 7.342976262117180575, 54.00000000000000711 ) ) ;
#50785 = EDGE_CURVE ( 'NONE', #43706, #65422, #36229, .T. ) ;
#50786 = AXIS2_PLACEMENT_3D ( 'NONE', #16774, #38342, #27726 ) ;
#50787 = EDGE_CURVE ( 'NONE', #46451, #17943, #3715, .T. ) ;
#50788 = AXIS2_PLACEMENT_3D ( 'NONE', #10511, #16169, #258 ) ;
#50789 = VECTOR ( 'NONE', #3095, 1000.000000000000000 ) ;
#50790 = DIRECTION ( 'NONE',  ( 1.000000000000000000, -0.000000000000000000, 0.000000000000000000 ) ) ;
#50791 = DIRECTION ( 'NONE',  ( 0.000000000000000000, 1.000000000000000000, 0.000000000000000000 ) ) ;
#50793 = ORIENTED_EDGE ( 'NONE', *, *, #66993, .F. ) ;
#50792 = DIRECTION ( 'NONE',  ( 0.000000000000000000, 0.000000000000000000, 1.000000000000000000 ) ) ;
#50794 = VERTEX_POINT ( 'NONE', #37294 ) ;
#50795 = DIRECTION ( 'NONE',  ( -0.000000000000000000, 3.673940397442059868E-16, -1.000000000000000000 ) ) ;
#50796 = AXIS2_PLACEMENT_3D ( 'NONE', #39497, #65690, #61059 ) ;
#50797 = CARTESIAN_POINT ( 'NONE',  ( 28.00000000000000000, -17.35230188589299871, -15.35019951917099945 ) ) ;
#50798 = CYLINDRICAL_SURFACE ( 'NONE', #67497, 4.000000000000000000 ) ;
#50799 = AXIS2_PLACEMENT_3D ( 'NONE', #15198, #31471, #52688 ) ;
#50800 = CARTESIAN_POINT ( 'NONE',  ( 14.50000000000000000, -42.00000000000000000, -27.00000000000000000 ) ) ;
#50801 = EDGE_LOOP ( 'NONE', ( #68152, #1054 ) ) ;
#50802 = CARTESIAN_POINT ( 'NONE',  ( 283.0000000000000568, -32.45000000000000995, 15.00000000000000000 ) ) ;
#50804 = AXIS2_PLACEMENT_3D ( 'NONE', #9320, #2961, #41498 ) ;
#50803 = PLANE ( 'NONE',  #22603 ) ;
#50805 = CARTESIAN_POINT ( 'NONE',  ( 29.25000000000000000, -5.000000000000000000, -11.75000000000000000 ) ) ;
#50806 = VECTOR ( 'NONE', #44297, 1000.000000000000000 ) ;
#50807 = DIRECTION ( 'NONE',  ( -0.000000000000000000, 1.000000000000000000, -0.000000000000000000 ) ) ;
#50808 = PLANE ( 'NONE',  #46176 ) ;
#50809 = LINE ( 'NONE', #29945, #1409 ) ;
#50810 = AXIS2_PLACEMENT_3D ( 'NONE', #60882, #6795, #12780 ) ;
#50811 = CARTESIAN_POINT ( 'NONE',  ( 8.580623737882843827, 9.689726262117162037, 26.00000000000000711 ) ) ;
#50812 = ORIENTED_EDGE ( 'NONE', *, *, #56202, .F. ) ;
#50813 = DIRECTION ( 'NONE',  ( 0.6414496315691494699, 0.7671651518153064231, 2.818519042764025305E-16 ) ) ;
#50814 = CARTESIAN_POINT ( 'NONE',  ( 17.00000000000000000, -16.28999999999710369, -15.00000000000794920 ) ) ;
#50815 = ORIENTED_EDGE ( 'NONE', *, *, #42089, .T. ) ;
#50816 = DIRECTION ( 'NONE',  ( 0.000000000000000000, 3.673940397442059868E-16, -1.000000000000000000 ) ) ;
#50817 = DIRECTION ( 'NONE',  ( 0.000000000000000000, -1.000000000000000000, -3.673940397442059868E-16 ) ) ;
#50818 = EDGE_CURVE ( 'NONE', #47021, #7568, #31309, .T. ) ;
#50819 = CARTESIAN_POINT ( 'NONE',  ( 11.32648345035337734, -4.406483450353491982, 455.0000000000000568 ) ) ;
#50820 = CARTESIAN_POINT ( 'NONE',  ( -11.00000000000000000, -11.85423089348099879, -9.852125413066602277 ) ) ;
#50821 = DIRECTION ( 'NONE',  ( 1.000000000000000000, 0.000000000000000000, 0.000000000000000000 ) ) ;
#50822 = ORIENTED_EDGE ( 'NONE', *, *, #58586, .T. ) ;
#50823 = CARTESIAN_POINT ( 'NONE',  ( 283.0000000000000568, -32.46196062927499781, 8.091291340630698770 ) ) ;
#50824 = ORIENTED_EDGE ( 'NONE', *, *, #1829, .F. ) ;
#50825 = AXIS2_PLACEMENT_3D ( 'NONE', #8949, #62694, #69055 ) ;
#50826 = CARTESIAN_POINT ( 'NONE',  ( -1.991476262117315432, -8.612468434717262866, 54.00000000000000711 ) ) ;
#50827 = EDGE_LOOP ( 'NONE', ( #30645, #45463, #43921, #25106 ) ) ;
#50828 = CARTESIAN_POINT ( 'NONE',  ( 7.250000000000005329, -7.449999999999998401, -17.50000000000000000 ) ) ;
#50829 = EDGE_CURVE ( 'NONE', #64273, #31007, #41545, .T. ) ;
#50830 = ORIENTED_EDGE ( 'NONE', *, *, #43588, .F. ) ;
#50831 = ADVANCED_FACE ( 'NONE', ( #19613 ), #9725, .T. ) ;
#50832 = CARTESIAN_POINT ( 'NONE',  ( 39.00000000000000000, 21.00000000000000000, 16.96999999999999886 ) ) ;
#50833 = ORIENTED_EDGE ( 'NONE', *, *, #28926, .F. ) ;
#50834 = VERTEX_POINT ( 'NONE', #41890 ) ;
#50835 = CARTESIAN_POINT ( 'NONE',  ( 5.257023737882819070, -5.257023737882815517, 26.00000000000000711 ) ) ;
#50836 = AXIS2_PLACEMENT_3D ( 'NONE', #69694, #53086, #16642 ) ;
#50837 = ORIENTED_EDGE ( 'NONE', *, *, #20405, .F. ) ;
#50838 = VERTEX_POINT ( 'NONE', #5116 ) ;
#50839 = CARTESIAN_POINT ( 'NONE',  ( -5.242976262117275077, -5.257023737882800418, 26.00000000000000711 ) ) ;
#50840 = LINE ( 'NONE', #67480, #46025 ) ;
#50842 = LINE ( 'NONE', #66423, #16317 ) ;
#50841 = AXIS2_PLACEMENT_3D ( 'NONE', #13958, #13262, #24924 ) ;
#50843 = ORIENTED_EDGE ( 'NONE', *, *, #11569, .F. ) ;
#50844 = CIRCLE ( 'NONE', #27151, 24.99999999998794920 ) ;
#50845 = DIRECTION ( 'NONE',  ( -0.000000000000000000, -0.000000000000000000, -1.000000000000000000 ) ) ;
#50847 = DIRECTION ( 'NONE',  ( 1.000000000000000000, 0.000000000000000000, -0.000000000000000000 ) ) ;
#50846 = LINE ( 'NONE', #45540, #25971 ) ;
#50848 = ORIENTED_EDGE ( 'NONE', *, *, #37480, .F. ) ;
#50850 = ORIENTED_EDGE ( 'NONE', *, *, #51079, .T. ) ;
#50849 = CARTESIAN_POINT ( 'NONE',  ( 5.793274621760843957, -6.358413763958980169, 54.00000000000000711 ) ) ;
#50851 = VERTEX_POINT ( 'NONE', #68063 ) ;
#50852 = EDGE_CURVE ( 'NONE', #22770, #57348, #15024, .T. ) ;
#50853 = AXIS2_PLACEMENT_3D ( 'NONE', #53992, #49709, #37723 ) ;
#50854 = APPLICATION_PROTOCOL_DEFINITION ( 'draft international standard', 'automotive_design', 1998, #9255 ) ;
#50856 = VECTOR ( 'NONE', #69415, 999.9999999999998863 ) ;
#50855 = DIRECTION ( 'NONE',  ( 0.000000000000000000, 1.000000000000000000, 0.000000000000000000 ) ) ;
#50857 = ORIENTED_EDGE ( 'NONE', *, *, #65320, .T. ) ;
#50858 = CARTESIAN_POINT ( 'NONE',  ( 17.51999999999999957, -15.50000000000000000, 26.00000000000000355 ) ) ;
#50859 = CARTESIAN_POINT ( 'NONE',  ( 7.450000000000003730, -7.249999999999997335, -11.00000000000000000 ) ) ;
#50860 = EDGE_CURVE ( 'NONE', #65338, #59076, #20665, .T. ) ;
#50861 = VERTEX_POINT ( 'NONE', #42235 ) ;
#50862 = ORIENTED_EDGE ( 'NONE', *, *, #17185, .F. ) ;
#50863 = AXIS2_PLACEMENT_3D ( 'NONE', #11327, #59781, #65435 ) ;
#50864 = AXIS2_PLACEMENT_3D ( 'NONE', #64890, #54279, #5838 ) ;
#50865 = CARTESIAN_POINT ( 'NONE',  ( 4.206483450353341702, -11.32648345035337911, 195.0000000000000284 ) ) ;
#50866 = CARTESIAN_POINT ( 'NONE',  ( 275.0000000000000000, -32.45000000000000995, -15.00000000000000000 ) ) ;
#50867 = ADVANCED_FACE ( 'NONE', ( #14668 ), #57450, .T. ) ;
#50868 = EDGE_LOOP ( 'NONE', ( #67909, #57382, #30397, #27746 ) ) ;
#50869 = DIRECTION ( 'NONE',  ( -1.000000000000000000, 1.047444401652940007E-14, -1.836970198721010952E-16 ) ) ;
#50870 = CARTESIAN_POINT ( 'NONE',  ( 17.00000000000000000, -15.50000000000000000, -19.33772233983200195 ) ) ;
#50871 = ADVANCED_FACE ( 'NONE', ( #9365 ), #10073, .F. ) ;
#50872 = DIRECTION ( 'NONE',  ( -0.000000000000000000, 3.673940397442059868E-16, -1.000000000000000000 ) ) ;
#50873 = ORIENTED_EDGE ( 'NONE', *, *, #679, .T. ) ;
#50874 = EDGE_CURVE ( 'NONE', #27858, #2479, #19976, .T. ) ;
#50875 = PLANE ( 'NONE',  #36955 ) ;
#50876 = VECTOR ( 'NONE', #57142, 1000.000000000000000 ) ;
#50877 = DIRECTION ( 'NONE',  ( -1.000000000000000000, 0.000000000000000000, 0.000000000000000000 ) ) ;
#50879 = ORIENTED_EDGE ( 'NONE', *, *, #54391, .T. ) ;
#50878 = CARTESIAN_POINT ( 'NONE',  ( 41.09999999999999432, -21.00000000000000000, 13.86939075806900057 ) ) ;
#50881 = ORIENTED_EDGE ( 'NONE', *, *, #19213, .T. ) ;
#50880 = DIRECTION ( 'NONE',  ( 0.000000000000000000, 3.673940397442059868E-16, -1.000000000000000000 ) ) ;
#50882 = DIRECTION ( 'NONE',  ( 0.000000000000000000, 0.000000000000000000, 1.000000000000000000 ) ) ;
#50883 = CARTESIAN_POINT ( 'NONE',  ( 7.749999999999998224, -7.348062532928000934, 5.000000000000000000 ) ) ;
#50884 = EDGE_CURVE ( 'NONE', #58562, #56437, #30628, .T. ) ;
#50885 = DIRECTION ( 'NONE',  ( 1.000000000000000000, 0.000000000000000000, 0.000000000000000000 ) ) ;
#50886 = DIRECTION ( 'NONE',  ( -1.794541526872559352E-16, -1.000000000000000000, 0.000000000000000000 ) ) ;
#50887 = CARTESIAN_POINT ( 'NONE',  ( 9.106483450353380249, -11.12648345035348640, 455.0000000000000568 ) ) ;
#50888 = ORIENTED_EDGE ( 'NONE', *, *, #35780, .F. ) ;
#50889 = CARTESIAN_POINT ( 'NONE',  ( 8.250000000000005329, 7.250000000000000888, -11.50000000000000000 ) ) ;
#50890 = DIRECTION ( 'NONE',  ( 0.8660254037850496633, 0.000000000000000000, -0.4999999999989417909 ) ) ;
#50891 = VECTOR ( 'NONE', #23840, 1000.000000000000000 ) ;
#50893 = VERTEX_POINT ( 'NONE', #4770 ) ;
#50892 = LINE ( 'NONE', #56893, #44634 ) ;
#50894 = VECTOR ( 'NONE', #28617, 1000.000000000000000 ) ;
#50895 = CARTESIAN_POINT ( 'NONE',  ( -7.250000000000000888, 7.450000000000003730, -8.500000000000000000 ) ) ;
#50896 = EDGE_CURVE ( 'NONE', #18842, #59664, #25644, .T. ) ;
#50897 = CARTESIAN_POINT ( 'NONE',  ( 146.5599459900709860, 0.000000000000000000, 276.7801873289890295 ) ) ;
#50898 = VECTOR ( 'NONE', #16312, 1000.000000000000000 ) ;
#50899 = VERTEX_POINT ( 'NONE', #4433 ) ;
#50900 = CARTESIAN_POINT ( 'NONE',  ( -8.566576262117260754, 9.689726262117185129, 54.00000000000000711 ) ) ;
#50901 = FACE_OUTER_BOUND ( 'NONE', #28742, .T. ) ;
#50902 = ORIENTED_EDGE ( 'NONE', *, *, #5439, .F. ) ;
#50903 = VECTOR ( 'NONE', #69115, 1000.000000000000000 ) ;
#50904 = AXIS2_PLACEMENT_3D ( 'NONE', #43114, #42772, #53742 ) ;
#50905 = EDGE_CURVE ( 'NONE', #15739, #7880, #163, .T. ) ;
#50906 = FACE_OUTER_BOUND ( 'NONE', #65319, .T. ) ;
#50907 = DIRECTION ( 'NONE',  ( -1.000000000000000000, 0.000000000000000000, 0.000000000000000000 ) ) ;
#50908 = DIRECTION ( 'NONE',  ( 0.000000000000000000, 0.000000000000000000, 1.000000000000000000 ) ) ;
#50909 = LINE ( 'NONE', #24036, #12382 ) ;
#50910 = VECTOR ( 'NONE', #42592, 1000.000000000000000 ) ;
#50911 = EDGE_CURVE ( 'NONE', #56111, #68694, #25992, .T. ) ;
#50912 = CARTESIAN_POINT ( 'NONE',  ( 10.14575131106465378, -20.50000000000000000, 17.00000000000000000 ) ) ;
#50913 = ORIENTED_EDGE ( 'NONE', *, *, #12949, .F. ) ;
#50914 = CYLINDRICAL_SURFACE ( 'NONE', #49712, 0.4000000000000600298 ) ;
#50915 = ORIENTED_EDGE ( 'NONE', *, *, #790, .F. ) ;
#50916 = ADVANCED_FACE ( 'NONE', ( #53224 ), #69464, .F. ) ;
#50917 = ORIENTED_EDGE ( 'NONE', *, *, #20163, .T. ) ;
#50918 = FACE_OUTER_BOUND ( 'NONE', #18966, .T. ) ;
#50919 = CIRCLE ( 'NONE', #55427, 0.4999999999991850963 ) ;
#50920 = CARTESIAN_POINT ( 'NONE',  ( -3.417780618358626565, 7.839518282750134404, 455.0000000000000568 ) ) ;
#50921 = EDGE_CURVE ( 'NONE', #37725, #31770, #48250, .T. ) ;
#50923 = FACE_OUTER_BOUND ( 'NONE', #61329, .T. ) ;
#50922 = DIRECTION ( 'NONE',  ( -1.000000000000000000, 0.000000000000000000, 0.000000000000000000 ) ) ;
#50924 = VERTEX_POINT ( 'NONE', #59889 ) ;
#50925 = EDGE_LOOP ( 'NONE', ( #21989, #57731, #59832, #60679 ) ) ;
#50926 = DIRECTION ( 'NONE',  ( 0.000000000000000000, 1.000000000000000000, 0.000000000000000000 ) ) ;
#50927 = ORIENTED_EDGE ( 'NONE', *, *, #31816, .F. ) ;
#50928 = CARTESIAN_POINT ( 'NONE',  ( 2.765062094116041980, -9.955011587777228499, 195.0000000000000284 ) ) ;
#50929 = FACE_OUTER_BOUND ( 'NONE', #53313, .T. ) ;
#50930 = LINE ( 'NONE', #56588, #39952 ) ;
#50931 = CIRCLE ( 'NONE', #69018, 3.500000000000003109 ) ;
#50932 = CARTESIAN_POINT ( 'NONE',  ( 0.000000000000000000, -7.449999999999998401, -18.50000000000000000 ) ) ;
#50933 = EDGE_CURVE ( 'NONE', #3671, #9740, #64515, .T. ) ;
#50934 = ORIENTED_EDGE ( 'NONE', *, *, #61152, .F. ) ;
#50935 = EDGE_CURVE ( 'NONE', #32668, #26887, #48706, .T. ) ;
#50936 = PLANE ( 'NONE',  #61602 ) ;
#50938 = LINE ( 'NONE', #2500, #41382 ) ;
#50937 = CARTESIAN_POINT ( 'NONE',  ( 2.369523737882786918, -9.562023737882787700, 26.00000000000000000 ) ) ;
#50939 = VERTEX_POINT ( 'NONE', #166 ) ;
#50942 = EDGE_CURVE ( 'NONE', #6930, #43292, #5814, .T. ) ;
#50941 = ORIENTED_EDGE ( 'NONE', *, *, #40103, .T. ) ;
#50940 = DIRECTION ( 'NONE',  ( -0.000000000000000000, -1.000000000000000000, -0.000000000000000000 ) ) ;
#50943 = ORIENTED_EDGE ( 'NONE', *, *, #24909, .T. ) ;
#50944 = ORIENTED_EDGE ( 'NONE', *, *, #31581, .T. ) ;
#50945 = EDGE_CURVE ( 'NONE', #47387, #36248, #49301, .T. ) ;
#50946 = EDGE_CURVE ( 'NONE', #68170, #24393, #16074, .T. ) ;
#50947 = LINE ( 'NONE', #7803, #17446 ) ;
#50948 = CIRCLE ( 'NONE', #20475, 0.4999999999991850963 ) ;
#50949 = EDGE_CURVE ( 'NONE', #61820, #54840, #55463, .T. ) ;
#50950 = CARTESIAN_POINT ( 'NONE',  ( 11.00000000000000000, -14.04000000000000092, 17.04524521594300523 ) ) ;
#50951 = VECTOR ( 'NONE', #37605, 999.9999999999998863 ) ;
#50952 = ADVANCED_FACE ( 'NONE', ( #32336 ), #6510, .F. ) ;
#50953 = ORIENTED_EDGE ( 'NONE', *, *, #3397, .F. ) ;
#50954 = ORIENTED_EDGE ( 'NONE', *, *, #57793, .T. ) ;
#50955 = EDGE_CURVE ( 'NONE', #21453, #32498, #69819, .T. ) ;
#50956 = PLANE ( 'NONE',  #47860 ) ;
#50957 = CARTESIAN_POINT ( 'NONE',  ( 6.364920264886885448, -3.677663764522628664, 54.00000000000000711 ) ) ;
#50958 = ORIENTED_EDGE ( 'NONE', *, *, #39356, .F. ) ;
#50959 = VECTOR ( 'NONE', #5215, 1000.000000000000000 ) ;
#50960 = AXIS2_PLACEMENT_3D ( 'NONE', #24604, #19630, #9027 ) ;
#50961 = EDGE_LOOP ( 'NONE', ( #3933, #52338, #29614, #2341 ) ) ;
#50962 = CARTESIAN_POINT ( 'NONE',  ( -7.250000000000000888, 7.450000000000003730, -22.50000000000000000 ) ) ;
#50963 = ADVANCED_FACE ( 'NONE', ( #54604 ), #1199, .F. ) ;
#50964 = CYLINDRICAL_SURFACE ( 'NONE', #68440, 0.7499999999999997780 ) ;
#50965 = ORIENTED_EDGE ( 'NONE', *, *, #2562, .T. ) ;
#50966 = VECTOR ( 'NONE', #36147, 1000.000000000000000 ) ;
#50967 = EDGE_CURVE ( 'NONE', #64136, #9816, #37644, .T. ) ;
#50968 = DIRECTION ( 'NONE',  ( -1.000000000000000000, 0.000000000000000000, 0.000000000000000000 ) ) ;
#50969 = CYLINDRICAL_SURFACE ( 'NONE', #31697, 0.5000000000009302559 ) ;
#50971 = ORIENTED_EDGE ( 'NONE', *, *, #22465, .F. ) ;
#50970 = DIRECTION ( 'NONE',  ( 0.000000000000000000, 0.000000000000000000, 1.000000000000000000 ) ) ;
#50972 = ORIENTED_EDGE ( 'NONE', *, *, #33146, .T. ) ;
#50974 = CARTESIAN_POINT ( 'NONE',  ( -4.393516549646788505, -11.78648345035339418, 195.0000000000000284 ) ) ;
#50973 = AXIS2_PLACEMENT_3D ( 'NONE', #61231, #12795, #33684 ) ;
#50975 = LINE ( 'NONE', #45655, #41371 ) ;
#50976 = CARTESIAN_POINT ( 'NONE',  ( 7.826483450353421745, 11.77351654964657257, 455.0000000000000568 ) ) ;
#50977 = EDGE_CURVE ( 'NONE', #12080, #61212, #28346, .T. ) ;
#50978 = LINE ( 'NONE', #67599, #25617 ) ;
#50979 = LINE ( 'NONE', #2532, #33505 ) ;
#50980 = CARTESIAN_POINT ( 'NONE',  ( 7.450000000000003730, -7.249999999999997335, -24.50000000000000000 ) ) ;
#50981 = DIRECTION ( 'NONE',  ( 0.000000000000000000, 0.000000000000000000, 1.000000000000000000 ) ) ;
#50982 = VERTEX_POINT ( 'NONE', #32675 ) ;
#50983 = DIRECTION ( 'NONE',  ( 0.000000000000000000, 0.000000000000000000, -1.000000000000000000 ) ) ;
#50985 = ORIENTED_EDGE ( 'NONE', *, *, #27557, .F. ) ;
#50984 = CARTESIAN_POINT ( 'NONE',  ( 17.00000000000000000, -15.50000000000000000, -19.33772233983200195 ) ) ;
#50986 = DIRECTION ( 'NONE',  ( 0.000000000000000000, 0.000000000000000000, 1.000000000000000000 ) ) ;
#50987 = CARTESIAN_POINT ( 'NONE',  ( 11.78648345035337819, -7.826483450353491023, 455.0000000000000568 ) ) ;
#50988 = CARTESIAN_POINT ( 'NONE',  ( -30.00000000000000000, -5.000000000000000000, -27.00000000000000000 ) ) ;
#50989 = LINE ( 'NONE', #50291, #23867 ) ;
#50990 = CARTESIAN_POINT ( 'NONE',  ( -11.25000000000000178, -11.18999999999999950, -4.250000000000000000 ) ) ;
#50991 = ORIENTED_EDGE ( 'NONE', *, *, #9540, .F. ) ;
#50992 = LINE ( 'NONE', #2550, #18443 ) ;
#50993 = EDGE_LOOP ( 'NONE', ( #63467, #57337, #43382, #66757 ) ) ;
#50994 = CARTESIAN_POINT ( 'NONE',  ( 30.00000000000000000, -5.599999999999999645, -9.000000000000001776 ) ) ;
#50995 = VECTOR ( 'NONE', #30810, 1000.000000000000000 ) ;
#50996 = CARTESIAN_POINT ( 'NONE',  ( 55.00000000000000000, 21.00000000000000000, 16.96999999999999886 ) ) ;
#50997 = ADVANCED_FACE ( 'NONE', ( #28068 ), #60579, .F. ) ;
#50998 = AXIS2_PLACEMENT_3D ( 'NONE', #19746, #68905, #42027 ) ;
#50999 = CARTESIAN_POINT ( 'NONE',  ( -9.234937905884127218, -9.955011587777249815, 455.0000000000000568 ) ) ;
#51000 = EDGE_LOOP ( 'NONE', ( #64741, #496, #2448, #24928, #45526, #12168, #51752, #35217, #60367, #1633 ) ) ;
#51001 = DIRECTION ( 'NONE',  ( 1.000000000000000000, 0.000000000000000000, 0.000000000000000000 ) ) ;
#51002 = ORIENTED_EDGE ( 'NONE', *, *, #33638, .T. ) ;
#51003 = EDGE_CURVE ( 'NONE', #6765, #40705, #54254, .T. ) ;
#51004 = ORIENTED_EDGE ( 'NONE', *, *, #51424, .T. ) ;
#51005 = DIRECTION ( 'NONE',  ( -1.000000000000000000, 0.000000000000000000, 0.000000000000000000 ) ) ;
#51006 = DIRECTION ( 'NONE',  ( 0.000000000000000000, 0.000000000000000000, 1.000000000000000000 ) ) ;
#51007 = ORIENTED_EDGE ( 'NONE', *, *, #51095, .T. ) ;
#51008 = LINE ( 'NONE', #54950, #16395 ) ;
#51009 = ADVANCED_FACE ( 'NONE', ( #48945 ), #16769, .F. ) ;
#51010 = AXIS2_PLACEMENT_3D ( 'NONE', #28484, #28151, #16854 ) ;
#51011 = AXIS2_PLACEMENT_3D ( 'NONE', #59719, #21543, #58345 ) ;
#51012 = LINE ( 'NONE', #61607, #62515 ) ;
#51013 = EDGE_CURVE ( 'NONE', #27724, #56702, #65548, .T. ) ;
#51014 = LINE ( 'NONE', #39359, #22708 ) ;
#51015 = EDGE_LOOP ( 'NONE', ( #45186, #6048, #43581, #62937, #64516, #43286, #57046, #10708, #43198, #14154, #4518, #67501, #46321, #28666, #55878, #30613, #17085, #46545, #52566, #28769, #27901, #6449, #17957, #40438, #23392, #33813, #15325, #57314, #59979, #15596, #57994, #35251, #37216, #62801, #24044, #69930, #13828, #47573, #52046, #63122, #10515, #63716, #44481, #3742, #45004, #69839, #37754, #52936, #64126, #12051, #1918, #63708, #59918, #19275, #24323, #34293 ) ) ;
#51016 = ORIENTED_EDGE ( 'NONE', *, *, #28175, .F. ) ;
#51018 = VERTEX_POINT ( 'NONE', #33023 ) ;
#51017 = CARTESIAN_POINT ( 'NONE',  ( 12.90000000000000213, -21.00000000000000000, 13.86939075806900057 ) ) ;
#51019 = CIRCLE ( 'NONE', #20538, 0.1999999999999987899 ) ;
#51020 = ORIENTED_EDGE ( 'NONE', *, *, #57477, .F. ) ;
#51021 = LINE ( 'NONE', #40413, #49598 ) ;
#51022 = CARTESIAN_POINT ( 'NONE',  ( 9.689999999999999503, -10.50000000000000178, -4.250000000000000000 ) ) ;
#51023 = DIRECTION ( 'NONE',  ( 0.000000000000000000, 0.000000000000000000, 1.000000000000000000 ) ) ;
#51024 = CARTESIAN_POINT ( 'NONE',  ( 22.90000000000000213, 13.66939075806899950, 20.80000000000000426 ) ) ;
#51025 = AXIS2_PLACEMENT_3D ( 'NONE', #33266, #60472, #12019 ) ;
#51026 = SURFACE_STYLE_USAGE ( .BOTH. , #7877 ) ;
#51027 = CARTESIAN_POINT ( 'NONE',  ( 289.7499999999998863, -0.2499999999999431288, 26.74999999999993250 ) ) ;
#51028 = VERTEX_POINT ( 'NONE', #27721 ) ;
#51029 = ORIENTED_EDGE ( 'NONE', *, *, #7025, .F. ) ;
#51030 = EDGE_LOOP ( 'NONE', ( #12892, #56498, #41841, #7882, #42157 ) ) ;
#51031 = EDGE_CURVE ( 'NONE', #2080, #68417, #38510, .T. ) ;
#51032 = EDGE_LOOP ( 'NONE', ( #19614, #46752, #53795, #59305 ) ) ;
#51033 = DIRECTION ( 'NONE',  ( 0.000000000000000000, 0.7071067811865474617, 0.7071067811865474617 ) ) ;
#51034 = CYLINDRICAL_SURFACE ( 'NONE', #20789, 2.458500000000000796 ) ;
#51035 = CARTESIAN_POINT ( 'NONE',  ( -4.706725378239246638, -4.155633711806646424, 26.00000000000000711 ) ) ;
#51036 = FACE_OUTER_BOUND ( 'NONE', #37737, .T. ) ;
#51037 = EDGE_LOOP ( 'NONE', ( #25117, #48908, #26420, #61905 ) ) ;
#51038 = ORIENTED_EDGE ( 'NONE', *, *, #13381, .F. ) ;
#51039 = ORIENTED_EDGE ( 'NONE', *, *, #11335, .T. ) ;
#51040 = CARTESIAN_POINT ( 'NONE',  ( -8.916576262117258622, 10.03972626211718477, 54.00000000000000711 ) ) ;
#51041 = ORIENTED_EDGE ( 'NONE', *, *, #37165, .T. ) ;
#51042 = ORIENTED_EDGE ( 'NONE', *, *, #54556, .T. ) ;
#51043 = VECTOR ( 'NONE', #59360, 1000.000000000000000 ) ;
#51044 = ORIENTED_EDGE ( 'NONE', *, *, #44778, .T. ) ;
#51045 = VERTEX_POINT ( 'NONE', #40752 ) ;
#51046 = CARTESIAN_POINT ( 'NONE',  ( 11.08848345035334404, -11.48848345035339591, 195.0000000000000284 ) ) ;
#51047 = AXIS2_PLACEMENT_3D ( 'NONE', #41679, #68206, #3510 ) ;
#51048 = EDGE_CURVE ( 'NONE', #2551, #11956, #13656, .T. ) ;
#51050 = EDGE_LOOP ( 'NONE', ( #54690, #19860, #64566, #65497 ) ) ;
#51049 = DIRECTION ( 'NONE',  ( 0.000000000000000000, 0.000000000000000000, 1.000000000000000000 ) ) ;
#51051 = ORIENTED_EDGE ( 'NONE', *, *, #28069, .F. ) ;
#51052 = FACE_OUTER_BOUND ( 'NONE', #18027, .T. ) ;
#51053 = EDGE_CURVE ( 'NONE', #36929, #9824, #47547, .T. ) ;
#51054 = CARTESIAN_POINT ( 'NONE',  ( -7.250000000000000000, -7.449999999999998401, -12.50000000000000000 ) ) ;
#51055 = DIRECTION ( 'NONE',  ( 0.000000000000000000, 1.000000000000000000, 0.000000000000000000 ) ) ;
#51056 = EDGE_CURVE ( 'NONE', #67984, #18617, #49800, .T. ) ;
#51057 = VECTOR ( 'NONE', #16344, 1000.000000000000000 ) ;
#51059 = EDGE_LOOP ( 'NONE', ( #28271, #41066, #69586, #66873 ) ) ;
#51058 = CARTESIAN_POINT ( 'NONE',  ( -11.00000000000000000, -13.79999999999979998, 17.30000000000000071 ) ) ;
#51060 = ORIENTED_EDGE ( 'NONE', *, *, #44844, .T. ) ;
#51061 = PLANE ( 'NONE',  #46405 ) ;
#51062 = VECTOR ( 'NONE', #61007, 1000.000000000000000 ) ;
#51063 = DIRECTION ( 'NONE',  ( 0.000000000000000000, -1.000000000000000000, 0.000000000000000000 ) ) ;
#51064 = CARTESIAN_POINT ( 'NONE',  ( 275.0000000000000000, -31.30000000000000071, 8.400000000000000355 ) ) ;
#51065 = ORIENTED_EDGE ( 'NONE', *, *, #30529, .F. ) ;
#51066 = CARTESIAN_POINT ( 'NONE',  ( 4.201500623656003519, -4.740315990920286104, 455.0000000000000568 ) ) ;
#51067 = PLANE ( 'NONE',  #13974 ) ;
#51068 = AXIS2_PLACEMENT_3D ( 'NONE', #64671, #16230, #37807 ) ;
#51069 = CARTESIAN_POINT ( 'NONE',  ( 7.000000000000000000, -30.45000000000000639, -15.00000000000000000 ) ) ;
#51070 = ORIENTED_EDGE ( 'NONE', *, *, #60045, .F. ) ;
#51071 = CARTESIAN_POINT ( 'NONE',  ( 3.677663764522614454, -6.364920264886879231, 54.00000000000000711 ) ) ;
#51072 = VECTOR ( 'NONE', #24296, 1000.000000000000000 ) ;
#51073 = CARTESIAN_POINT ( 'NONE',  ( 8.249999999999996447, 8.250000000000001776, -1.000000000000000000 ) ) ;
#51074 = CARTESIAN_POINT ( 'NONE',  ( -7.603567055985637424, -8.606483450353410447, 455.0000000000000568 ) ) ;
#51075 = VERTEX_POINT ( 'NONE', #24499 ) ;
#51076 = FILL_AREA_STYLE_COLOUR ( '', #61796 ) ;
#51077 = PLANE ( 'NONE',  #16426 ) ;
#51078 = DIRECTION ( 'NONE',  ( -1.000000000000000000, 0.000000000000000000, 0.000000000000000000 ) ) ;
#51079 = EDGE_CURVE ( 'NONE', #24080, #17336, #56318, .T. ) ;
#51080 = ORIENTED_EDGE ( 'NONE', *, *, #8385, .F. ) ;
#51081 = FACE_OUTER_BOUND ( 'NONE', #12387, .T. ) ;
#51082 = DIRECTION ( 'NONE',  ( 0.000000000000000000, 0.000000000000000000, 1.000000000000000000 ) ) ;
#51083 = LINE ( 'NONE', #62741, #36442 ) ;
#51084 = EDGE_CURVE ( 'NONE', #11694, #41475, #51014, .T. ) ;
#51085 = CARTESIAN_POINT ( 'NONE',  ( -6.486996718459913325, -3.157023737882783454, 54.00000000000000711 ) ) ;
#51086 = CARTESIAN_POINT ( 'NONE',  ( -11.99351654964671354, 11.18071654964658990, 455.0000000000000568 ) ) ;
#51087 = ORIENTED_EDGE ( 'NONE', *, *, #18820, .F. ) ;
#51088 = CARTESIAN_POINT ( 'NONE',  ( -15.08757311576351334, -0.3152598339557977081, -21.29473909966096556 ) ) ;
#51089 = PLANE ( 'NONE',  #47483 ) ;
#51090 = EDGE_CURVE ( 'NONE', #21069, #135, #6825, .T. ) ;
#51091 = AXIS2_PLACEMENT_3D ( 'NONE', #24221, #13609, #45783 ) ;
#51092 = EDGE_CURVE ( 'NONE', #33822, #41049, #7866, .T. ) ;
#51093 = CARTESIAN_POINT ( 'NONE',  ( 49.00000000000000000, -14.06939075806900163, -20.80000000000000426 ) ) ;
#51094 = FACE_OUTER_BOUND ( 'NONE', #905, .T. ) ;
#51095 = EDGE_CURVE ( 'NONE', #31596, #66404, #29791, .T. ) ;
#51096 = LINE ( 'NONE', #8665, #41835 ) ;
#51097 = EDGE_CURVE ( 'NONE', #57808, #35535, #66580, .T. ) ;
#51098 = CIRCLE ( 'NONE', #7076, 4.000000000000000000 ) ;
#51099 = VERTEX_POINT ( 'NONE', #23451 ) ;
#51101 = VERTEX_POINT ( 'NONE', #2224 ) ;
#51100 = DIRECTION ( 'NONE',  ( 0.000000000000000000, 0.000000000000000000, 1.000000000000000000 ) ) ;
#51102 = EDGE_CURVE ( 'NONE', #29889, #35918, #43044, .T. ) ;
#51103 = DIRECTION ( 'NONE',  ( 1.836970198721029934E-16, 1.836970198721010706E-16, -1.000000000000000000 ) ) ;
#51104 = CARTESIAN_POINT ( 'NONE',  ( -10.30047626211725742, 3.842976262117182351, 26.00000000000000711 ) ) ;
#51105 = ORIENTED_EDGE ( 'NONE', *, *, #8979, .T. ) ;
#51106 = CIRCLE ( 'NONE', #56756, 0.1999999999999996503 ) ;
#51107 = CARTESIAN_POINT ( 'NONE',  ( -7.450000000000001954, 0.000000000000000000, -11.50000000000000000 ) ) ;
#51108 = ORIENTED_EDGE ( 'NONE', *, *, #52968, .F. ) ;
#51109 = CARTESIAN_POINT ( 'NONE',  ( 49.00000000000000000, 13.66939075806899950, 20.80000000000000426 ) ) ;
#51110 = VERTEX_POINT ( 'NONE', #19186 ) ;
#51111 = VERTEX_POINT ( 'NONE', #45349 ) ;
#51112 = DIRECTION ( 'NONE',  ( 0.000000000000000000, 0.000000000000000000, 1.000000000000000000 ) ) ;
#51113 = LINE ( 'NONE', #13632, #65900 ) ;
#51114 = CARTESIAN_POINT ( 'NONE',  ( 3.857023737882813386, 10.30047626211720768, 26.00000000000000711 ) ) ;
#51115 = CARTESIAN_POINT ( 'NONE',  ( 9.899999999999998579, -21.00000000000001421, -13.86939075806900945 ) ) ;
#51116 = VECTOR ( 'NONE', #36965, 1000.000000000000000 ) ;
#51117 = ORIENTED_EDGE ( 'NONE', *, *, #18070, .T. ) ;
#51118 = ORIENTED_EDGE ( 'NONE', *, *, #37830, .T. ) ;
#51119 = CARTESIAN_POINT ( 'NONE',  ( -11.00000000000000000, -9.487228132326899654, 12.50000000000000000 ) ) ;
#51120 = CIRCLE ( 'NONE', #57891, 0.3499999999999996447 ) ;
#51121 = FACE_OUTER_BOUND ( 'NONE', #22094, .T. ) ;
#51122 = ORIENTED_EDGE ( 'NONE', *, *, #55375, .F. ) ;
#51123 = AXIS2_PLACEMENT_3D ( 'NONE', #36090, #52735, #47062 ) ;
#51124 = ORIENTED_EDGE ( 'NONE', *, *, #53856, .T. ) ;
#51125 = ORIENTED_EDGE ( 'NONE', *, *, #51541, .T. ) ;
#51126 = CARTESIAN_POINT ( 'NONE',  ( -9.689999999999999503, -10.50000000000000178, 0.000000000000000000 ) ) ;
#51128 = ORIENTED_EDGE ( 'NONE', *, *, #37355, .F. ) ;
#51127 = CARTESIAN_POINT ( 'NONE',  ( 8.250000000000005329, -8.249999999999998224, -26.00000000000001066 ) ) ;
#51129 = CARTESIAN_POINT ( 'NONE',  ( 4.456444791733522252E-16, 7.450000000000002842, -17.50000000000000000 ) ) ;
#51130 = ADVANCED_FACE ( 'NONE', ( #45697 ), #23092, .F. ) ;
#51131 = VECTOR ( 'NONE', #53085, 1000.000000000000000 ) ;
#51132 = DIRECTION ( 'NONE',  ( 1.000000000000000000, 0.000000000000000000, -0.000000000000000000 ) ) ;
#51133 = ORIENTED_EDGE ( 'NONE', *, *, #4756, .F. ) ;
#51134 = EDGE_CURVE ( 'NONE', #43261, #30530, #35436, .T. ) ;
#51135 = ORIENTED_EDGE ( 'NONE', *, *, #66656, .T. ) ;
#51136 = EDGE_CURVE ( 'NONE', #56003, #59410, #37407, .T. ) ;
#51137 = VECTOR ( 'NONE', #56314, 1000.000000000000000 ) ;
#51138 = EDGE_CURVE ( 'NONE', #61285, #17051, #24972, .T. ) ;
#51139 = LINE ( 'NONE', #7651, #7805 ) ;
#51140 = CARTESIAN_POINT ( 'NONE',  ( 9.404523737882817258, -1.480523737882826207, 54.00000000000000711 ) ) ;
#51141 = AXIS2_PLACEMENT_3D ( 'NONE', #42010, #3827, #37071 ) ;
#51142 = FACE_OUTER_BOUND ( 'NONE', #56735, .T. ) ;
#51143 = DIRECTION ( 'NONE',  ( 0.000000000000000000, 0.000000000000000000, 1.000000000000000000 ) ) ;
#51144 = DIRECTION ( 'NONE',  ( 0.000000000000000000, 0.000000000000000000, -1.000000000000000000 ) ) ;
#51146 = ORIENTED_EDGE ( 'NONE', *, *, #7773, .F. ) ;
#51145 = DIRECTION ( 'NONE',  ( 0.000000000000000000, 1.000000000000000000, 0.000000000000000000 ) ) ;
#51147 = ORIENTED_EDGE ( 'NONE', *, *, #4209, .T. ) ;
#51148 = AXIS2_PLACEMENT_3D ( 'NONE', #35633, #8779, #30346 ) ;
#51149 = DIRECTION ( 'NONE',  ( 0.000000000000000000, 0.000000000000000000, 1.000000000000000000 ) ) ;
#51150 = CARTESIAN_POINT ( 'NONE',  ( 30.90000000000000213, -0.1999999999911430404, -8.864436962241481021E-12 ) ) ;
#51151 = CARTESIAN_POINT ( 'NONE',  ( 40.90000000000000568, -21.00000000000000000, 13.86939075806900057 ) ) ;
#51152 = CARTESIAN_POINT ( 'NONE',  ( -3.667976262117228714, 9.722976262117169810, 54.00000000000000711 ) ) ;
#51153 = CARTESIAN_POINT ( 'NONE',  ( 4.149127210878726935, -6.836383711242993044, 26.00000000000000000 ) ) ;
#51154 = EDGE_LOOP ( 'NONE', ( #54118, #17286, #39371, #51016 ) ) ;
#51155 = CARTESIAN_POINT ( 'NONE',  ( -11.75000000000000000, -5.000000000000000000, 26.25000000000000000 ) ) ;
#51156 = DIRECTION ( 'NONE',  ( 0.000000000000000000, 0.000000000000000000, 1.000000000000000000 ) ) ;
#51157 =( LENGTH_UNIT ( ) NAMED_UNIT ( * ) SI_UNIT ( .MILLI., .METRE. ) );
#51158 = PLANE ( 'NONE',  #69551 ) ;
#51159 = EDGE_CURVE ( 'NONE', #4795, #47820, #12537, .T. ) ;
#51160 = VECTOR ( 'NONE', #35352, 1000.000000000000000 ) ;
#51161 = LINE ( 'NONE', #39839, #59764 ) ;
#51162 = DIRECTION ( 'NONE',  ( -1.000000000000000000, 0.000000000000000000, 0.000000000000000000 ) ) ;
#51163 = AXIS2_PLACEMENT_3D ( 'NONE', #58851, #69452, #20314 ) ;
#51164 = DIRECTION ( 'NONE',  ( -1.000000000000000000, 0.000000000000000000, 0.000000000000000000 ) ) ;
#51165 = VECTOR ( 'NONE', #66325, 1000.000000000000000 ) ;
#51166 = VERTEX_POINT ( 'NONE', #55971 ) ;
#51167 = VECTOR ( 'NONE', #59141, 1000.000000000000000 ) ;
#51168 = CARTESIAN_POINT ( 'NONE',  ( 0.000000000000000000, -20.50000000000000000, 17.79289321881345032 ) ) ;
#51169 = DIRECTION ( 'NONE',  ( 0.000000000000000000, 1.000000000000000000, 0.000000000000000000 ) ) ;
#51170 = ORIENTED_EDGE ( 'NONE', *, *, #37747, .T. ) ;
#51171 = DIRECTION ( 'NONE',  ( -1.000000000000000000, 0.000000000000000000, 0.000000000000000000 ) ) ;
#51172 = CARTESIAN_POINT ( 'NONE',  ( 78.77321854994620765, 47.95351654967443977, 15.00000000000000000 ) ) ;
#51173 = LINE ( 'NONE', #23261, #18544 ) ;
#51175 = CIRCLE ( 'NONE', #370, 0.3499999999998875677 ) ;
#51174 = CARTESIAN_POINT ( 'NONE',  ( 7.000000000000000000, -40.30000000000000426, -12.20000000000000107 ) ) ;
#51176 = CARTESIAN_POINT ( 'NONE',  ( 10.74648345035330443, 1.677516549646577371, 195.0000000000000284 ) ) ;
#51177 = EDGE_CURVE ( 'NONE', #66376, #17317, #24143, .T. ) ;
#51178 = VERTEX_POINT ( 'NONE', #7526 ) ;
#51179 = DIRECTION ( 'NONE',  ( 0.000000000000000000, 1.000000000000000000, 0.000000000000000000 ) ) ;
#51180 = VERTEX_POINT ( 'NONE', #51357 ) ;
#51181 = ADVANCED_FACE ( 'NONE', ( #49964 ), #61967, .F. ) ;
#51182 = DIRECTION ( 'NONE',  ( 1.000000000000000000, 0.000000000000000000, 0.000000000000000000 ) ) ;
#51183 = EDGE_LOOP ( 'NONE', ( #65571, #7946, #24486, #62680 ) ) ;
#51184 = FACE_OUTER_BOUND ( 'NONE', #34350, .T. ) ;
#51185 = CIRCLE ( 'NONE', #33126, 1.999999999999314770 ) ;
#51186 = ORIENTED_EDGE ( 'NONE', *, *, #32565, .F. ) ;
#51187 = DIRECTION ( 'NONE',  ( 1.000000000000000000, 0.000000000000000000, 0.000000000000000000 ) ) ;
#51188 = CYLINDRICAL_SURFACE ( 'NONE', #11933, 0.6000000000000000888 ) ;
#51189 = ORIENTED_EDGE ( 'NONE', *, *, #45684, .T. ) ;
#51190 = ORIENTED_EDGE ( 'NONE', *, *, #33843, .T. ) ;
#51191 = VECTOR ( 'NONE', #40903, 1000.000000000000000 ) ;
#51192 = DIRECTION ( 'NONE',  ( -5.120954910632640039E-15, -1.000000000000000000, -3.673940397442059868E-16 ) ) ;
#51193 = VERTEX_POINT ( 'NONE', #3632 ) ;
#51194 = ORIENTED_EDGE ( 'NONE', *, *, #66090, .T. ) ;
#51195 = EDGE_CURVE ( 'NONE', #34744, #16520, #9183, .T. ) ;
#51196 = DIRECTION ( 'NONE',  ( 1.000000000000000000, -0.000000000000000000, 0.000000000000000000 ) ) ;
#51197 = LINE ( 'NONE', #29979, #40371 ) ;
#51198 = DIRECTION ( 'NONE',  ( 0.000000000000000000, -0.000000000000000000, 1.000000000000000000 ) ) ;
#51199 = ORIENTED_EDGE ( 'NONE', *, *, #26218, .F. ) ;
#51200 = DIRECTION ( 'NONE',  ( 0.000000000000000000, 0.000000000000000000, -1.000000000000000000 ) ) ;
#51202 = FACE_BOUND ( 'NONE', #20910, .T. ) ;
#51201 = DIRECTION ( 'NONE',  ( 1.000000000000000000, 0.000000000000000000, 0.000000000000000000 ) ) ;
#51203 = VERTEX_POINT ( 'NONE', #63734 ) ;
#51205 = VERTEX_POINT ( 'NONE', #9992 ) ;
#51204 = CYLINDRICAL_SURFACE ( 'NONE', #11623, 2.215251240775983899 ) ;
#51206 = VERTEX_POINT ( 'NONE', #15645 ) ;
#51207 = CARTESIAN_POINT ( 'NONE',  ( 283.0000000000000568, -32.44999999999905071, -14.49999999999906031 ) ) ;
#51208 = VERTEX_POINT ( 'NONE', #67980 ) ;
#51209 = CARTESIAN_POINT ( 'NONE',  ( 11.50000000000000000, -11.50000000000100009, -15.00000000000084910 ) ) ;
#51210 = AXIS2_PLACEMENT_3D ( 'NONE', #28297, #49869, #1424 ) ;
#51211 = VECTOR ( 'NONE', #54351, 1000.000000000000000 ) ;
#51212 = FACE_OUTER_BOUND ( 'NONE', #34369, .T. ) ;
#51213 = ORIENTED_EDGE ( 'NONE', *, *, #61200, .T. ) ;
#51214 = ORIENTED_EDGE ( 'NONE', *, *, #25900, .T. ) ;
#51215 = EDGE_CURVE ( 'NONE', #49797, #54695, #8570, .T. ) ;
#51216 = CIRCLE ( 'NONE', #6068, 4.000000000000000888 ) ;
#51218 = CARTESIAN_POINT ( 'NONE',  ( 289.7500000000000000, -0.2500000000000000000, -26.75000000000000000 ) ) ;
#51217 = AXIS2_PLACEMENT_3D ( 'NONE', #9724, #68770, #4769 ) ;
#51219 = CIRCLE ( 'NONE', #29767, 0.7499999999999997780 ) ;
#51220 = DIRECTION ( 'NONE',  ( -1.000000000000000000, 0.000000000000000000, 0.000000000000000000 ) ) ;
#51221 = VERTEX_POINT ( 'NONE', #35795 ) ;
#51222 = ADVANCED_FACE ( 'NONE', ( #3982 ), #41095, .F. ) ;
#51223 = CARTESIAN_POINT ( 'NONE',  ( 0.000000000000000000, -7.449999999999998401, -21.50000000000000000 ) ) ;
#51224 = DIRECTION ( 'NONE',  ( 0.000000000000000000, 0.000000000000000000, -1.000000000000000000 ) ) ;
#51225 = AXIS2_PLACEMENT_3D ( 'NONE', #20467, #57941, #63613 ) ;
#51226 = AXIS2_PLACEMENT_3D ( 'NONE', #41103, #62672, #14250 ) ;
#51227 = VECTOR ( 'NONE', #53860, 1000.000000000000000 ) ;
#51228 = CARTESIAN_POINT ( 'NONE',  ( 11.00000000000000000, -9.199999999999999289, -12.34999999999989839 ) ) ;
#51229 = ORIENTED_EDGE ( 'NONE', *, *, #27017, .T. ) ;
#51230 = DIRECTION ( 'NONE',  ( 0.000000000000000000, 0.000000000000000000, -1.000000000000000000 ) ) ;
#51231 = CARTESIAN_POINT ( 'NONE',  ( -10.30047626211725742, 6.642976262117184838, 54.00000000000000711 ) ) ;
#51232 = ORIENTED_EDGE ( 'NONE', *, *, #55077, .T. ) ;
#51234 = ORIENTED_EDGE ( 'NONE', *, *, #64233, .T. ) ;
#51233 = DIRECTION ( 'NONE',  ( 1.836970198721029934E-16, 1.836970198721010706E-16, -1.000000000000000000 ) ) ;
#51235 = DIRECTION ( 'NONE',  ( -1.000000000000000000, 0.000000000000000000, 0.000000000000000000 ) ) ;
#51236 = CARTESIAN_POINT ( 'NONE',  ( 11.00000000000000000, -11.50000000000000000, 15.00000000000000000 ) ) ;
#51237 = CARTESIAN_POINT ( 'NONE',  ( 169.1780563256071446, -35.83962462487175316, 0.000000000000000000 ) ) ;
#51238 = CARTESIAN_POINT ( 'NONE',  ( -8.697938382363135545, 2.406732575409538111, 54.00000000000000711 ) ) ;
#51239 = EDGE_CURVE ( 'NONE', #62306, #19389, #57366, .T. ) ;
#51240 = DIRECTION ( 'NONE',  ( -1.053224967557348291E-14, -1.000000000000000000, 0.000000000000000000 ) ) ;
#51241 = ORIENTED_EDGE ( 'NONE', *, *, #54475, .T. ) ;
#51242 = LINE ( 'NONE', #23670, #60598 ) ;
#51243 = DIRECTION ( 'NONE',  ( 3.540251991789403884E-15, 1.000000000000000000, 0.000000000000000000 ) ) ;
#51244 = DIRECTION ( 'NONE',  ( 0.5773502691896257311, -0.5773502691896257311, -0.5773502691896257311 ) ) ;
#51246 = ORIENTED_EDGE ( 'NONE', *, *, #46700, .F. ) ;
#51245 = CARTESIAN_POINT ( 'NONE',  ( 275.0000000000000000, -27.13000000000000611, -15.49999999999930012 ) ) ;
#51247 = CYLINDRICAL_SURFACE ( 'NONE', #810, 1.929199999999998028 ) ;
#51248 = VECTOR ( 'NONE', #59194, 1000.000000000000000 ) ;
#51249 = DIRECTION ( 'NONE',  ( 0.4999999999999827360, 0.000000000000000000, 0.8660254037844485886 ) ) ;
#51250 = ORIENTED_EDGE ( 'NONE', *, *, #4415, .T. ) ;
#51251 = ORIENTED_EDGE ( 'NONE', *, *, #63568, .F. ) ;
#51252 = DIRECTION ( 'NONE',  ( 0.000000000000000000, 0.000000000000000000, -1.000000000000000000 ) ) ;
#51253 = DIRECTION ( 'NONE',  ( 1.000000000000000000, -0.000000000000000000, -0.000000000000000000 ) ) ;
#51254 = ORIENTED_EDGE ( 'NONE', *, *, #36927, .F. ) ;
#51255 = DIRECTION ( 'NONE',  ( -0.000000000000000000, -0.000000000000000000, -1.000000000000000000 ) ) ;
#51256 = FACE_OUTER_BOUND ( 'NONE', #7091, .T. ) ;
#51257 =( REPRESENTATION_RELATIONSHIP ('NONE','NONE', #4299, #26379 ) REPRESENTATION_RELATIONSHIP_WITH_TRANSFORMATION ( #52629 )SHAPE_REPRESENTATION_RELATIONSHIP( ) );
#51258 = DIRECTION ( 'NONE',  ( -0.000000000000000000, -0.000000000000000000, 1.000000000000000000 ) ) ;
#51259 = ADVANCED_FACE ( 'NONE', ( #69026 ), #30148, .F. ) ;
#51260 = LINE ( 'NONE', #68594, #65758 ) ;
#51261 = VECTOR ( 'NONE', #34193, 1000.000000000000000 ) ;
#51262 = VECTOR ( 'NONE', #45369, 1000.000000000000000 ) ;
#51263 = ORIENTED_EDGE ( 'NONE', *, *, #23183, .T. ) ;
#51264 = EDGE_CURVE ( 'NONE', #21251, #62304, #46751, .T. ) ;
#51265 = DIRECTION ( 'NONE',  ( -1.000000000000000000, 0.000000000000000000, 0.000000000000000000 ) ) ;
#51266 = ORIENTED_EDGE ( 'NONE', *, *, #5486, .F. ) ;
#51267 = EDGE_CURVE ( 'NONE', #58100, #51627, #42152, .T. ) ;
#51268 = ORIENTED_EDGE ( 'NONE', *, *, #1545, .F. ) ;
#51269 = LINE ( 'NONE', #13081, #8819 ) ;
#51270 = AXIS2_PLACEMENT_3D ( 'NONE', #11836, #15169, #48995 ) ;
#51271 = EDGE_CURVE ( 'NONE', #50794, #97, #20235, .T. ) ;
#51272 = PRODUCT_RELATED_PRODUCT_CATEGORY ( 'part', '', ( #62794 ) ) ;
#51273 = FACE_OUTER_BOUND ( 'NONE', #69702, .T. ) ;
#51274 = EDGE_CURVE ( 'NONE', #17772, #10, #62663, .T. ) ;
#51275 = VECTOR ( 'NONE', #26882, 1000.000000000000000 ) ;
#51276 = DIRECTION ( 'NONE',  ( -0.000000000000000000, -0.000000000000000000, -1.000000000000000000 ) ) ;
#51277 = ORIENTED_EDGE ( 'NONE', *, *, #11906, .F. ) ;
#51278 = EDGE_CURVE ( 'NONE', #68417, #19877, #63026, .T. ) ;
#51279 = ORIENTED_EDGE ( 'NONE', *, *, #7806, .F. ) ;
#51280 = CARTESIAN_POINT ( 'NONE',  ( 9.737023737882816832, -3.682023737882826886, 54.00000000000000711 ) ) ;
#51282 = ORIENTED_EDGE ( 'NONE', *, *, #38661, .T. ) ;
#51281 = EDGE_CURVE ( 'NONE', #57835, #43126, #14241, .T. ) ;
#51283 = ORIENTED_EDGE ( 'NONE', *, *, #45910, .F. ) ;
#51284 = CARTESIAN_POINT ( 'NONE',  ( 39.00000000000000000, 0.000000000000000000, 0.000000000000000000 ) ) ;
#51285 = CARTESIAN_POINT ( 'NONE',  ( 29.50000000000000355, -12.00000000000000000, -10.52786404500095863 ) ) ;
#51286 = DIRECTION ( 'NONE',  ( -0.000000000000000000, 3.673940397442059868E-16, -1.000000000000000000 ) ) ;
#51287 = CARTESIAN_POINT ( 'NONE',  ( 3.606483450353380249, -4.622483450353396250, 195.0000000000000284 ) ) ;
#51288 = ORIENTED_EDGE ( 'NONE', *, *, #1848, .T. ) ;
#51289 = VECTOR ( 'NONE', #47816, 1000.000000000000000 ) ;
#51290 = DIRECTION ( 'NONE',  ( 0.000000000000000000, 0.000000000000000000, 1.000000000000000000 ) ) ;
#51292 = CARTESIAN_POINT ( 'NONE',  ( -30.00000000000000000, -11.50000000000100009, -15.00000000000084910 ) ) ;
#51291 = CARTESIAN_POINT ( 'NONE',  ( -7.450000000000001954, 0.000000000000000000, -15.00000000000000000 ) ) ;
#51293 = VERTEX_POINT ( 'NONE', #57714 ) ;
#51295 = EDGE_LOOP ( 'NONE', ( #62718, #28758, #40300, #52279 ) ) ;
#51294 = DIRECTION ( 'NONE',  ( 0.000000000000000000, 0.000000000000000000, 1.000000000000000000 ) ) ;
#51296 = ORIENTED_EDGE ( 'NONE', *, *, #43617, .F. ) ;
#51297 = EDGE_LOOP ( 'NONE', ( #51277, #55516, #2201, #16180 ) ) ;
#51298 = DIRECTION ( 'NONE',  ( -0.000000000000000000, -0.000000000000000000, -1.000000000000000000 ) ) ;
#51299 = LINE ( 'NONE', #34681, #41712 ) ;
#51300 = EDGE_CURVE ( 'NONE', #31731, #51166, #9637, .T. ) ;
#51301 = VERTEX_POINT ( 'NONE', #36498 ) ;
#51302 = VERTEX_POINT ( 'NONE', #15293 ) ;
#51303 = VECTOR ( 'NONE', #46320, 1000.000000000000000 ) ;
#51304 = CARTESIAN_POINT ( 'NONE',  ( 35.89999999999999858, 0.000000000000000000, 0.000000000000000000 ) ) ;
#51305 = DIRECTION ( 'NONE',  ( -1.000000000000000000, 0.000000000000000000, 0.000000000000000000 ) ) ;
#51306 = CIRCLE ( 'NONE', #36684, 25.39999999999999858 ) ;
#51307 = ORIENTED_EDGE ( 'NONE', *, *, #24267, .F. ) ;
#51308 = ORIENTED_EDGE ( 'NONE', *, *, #7555, .T. ) ;
#51309 = FACE_OUTER_BOUND ( 'NONE', #13016, .T. ) ;
#51310 = CARTESIAN_POINT ( 'NONE',  ( 5.393625297349938563, 7.252248008019325454, 455.0000000000000568 ) ) ;
#51311 = ORIENTED_EDGE ( 'NONE', *, *, #55349, .T. ) ;
#51312 = AXIS2_PLACEMENT_3D ( 'NONE', #54675, #16837, #53636 ) ;
#51313 = CIRCLE ( 'NONE', #1591, 0.1749999999999989342 ) ;
#51314 = DIRECTION ( 'NONE',  ( 0.5773502691896257311, 0.5773502691896257311, 0.5773502691896257311 ) ) ;
#51315 = CARTESIAN_POINT ( 'NONE',  ( 30.00000000000000000, -14.33999999999999986, -14.50000000000000000 ) ) ;
#51317 = ORIENTED_EDGE ( 'NONE', *, *, #18864, .F. ) ;
#51316 = DIRECTION ( 'NONE',  ( 0.000000000000000000, -1.000000000000000000, -3.673940397442060361E-16 ) ) ;
#51318 = EDGE_LOOP ( 'NONE', ( #21236, #59124, #30852, #19297 ) ) ;
#51319 = DIRECTION ( 'NONE',  ( 0.000000000000000000, 0.000000000000000000, 1.000000000000000000 ) ) ;
#51320 = CARTESIAN_POINT ( 'NONE',  ( 34.89999999999999858, 20.60000000000000142, -13.86939075806900057 ) ) ;
#51321 = VECTOR ( 'NONE', #62367, 1000.000000000000000 ) ;
#51322 = CYLINDRICAL_SURFACE ( 'NONE', #65644, 4.000000000000000000 ) ;
#51323 = LINE ( 'NONE', #61569, #40273 ) ;
#51324 = LINE ( 'NONE', #55937, #45921 ) ;
#51325 = DIRECTION ( 'NONE',  ( 0.000000000000000000, 0.000000000000000000, 1.000000000000000000 ) ) ;
#51326 = VECTOR ( 'NONE', #55306, 1000.000000000000000 ) ;
#51327 = EDGE_CURVE ( 'NONE', #15112, #35206, #47590, .T. ) ;
#51328 = DIRECTION ( 'NONE',  ( 1.000000000000000000, -0.000000000000000000, -0.000000000000000000 ) ) ;
#51329 = EDGE_LOOP ( 'NONE', ( #59462, #58440 ) ) ;
#51330 = CARTESIAN_POINT ( 'NONE',  ( 41.09999999999999432, 20.60000000000000142, 13.86939075806900057 ) ) ;
#51332 = VERTEX_POINT ( 'NONE', #14941 ) ;
#51331 = DIRECTION ( 'NONE',  ( 0.000000000000000000, 0.000000000000000000, -1.000000000000000000 ) ) ;
#51333 = CARTESIAN_POINT ( 'NONE',  ( 40.90000000000000568, -0.1999999999911430404, -8.864436962241481021E-12 ) ) ;
#51334 = DIRECTION ( 'NONE',  ( -0.000000000000000000, -0.000000000000000000, -1.000000000000000000 ) ) ;
#51335 = EDGE_CURVE ( 'NONE', #40788, #56650, #66797, .T. ) ;
#51336 = DIRECTION ( 'NONE',  ( 1.000000000000000000, 0.000000000000000000, 0.000000000000000000 ) ) ;
#51337 = DIRECTION ( 'NONE',  ( 1.000000000000000000, -0.000000000000000000, 0.000000000000000000 ) ) ;
#51338 = CARTESIAN_POINT ( 'NONE',  ( 7.250000000000005329, 7.250000000000000888, -12.50000000000000000 ) ) ;
#51339 = EDGE_CURVE ( 'NONE', #37116, #51208, #58439, .T. ) ;
#51340 = EDGE_LOOP ( 'NONE', ( #46046, #64351, #55357, #19191 ) ) ;
#51341 = CARTESIAN_POINT ( 'NONE',  ( -9.791916549646712653, 10.19191654964664018, 195.0000000000000284 ) ) ;
#51342 = EDGE_CURVE ( 'NONE', #50768, #46357, #39697, .T. ) ;
#51343 = ORIENTED_EDGE ( 'NONE', *, *, #33259, .F. ) ;
#51344 = CARTESIAN_POINT ( 'NONE',  ( 78.77321854994620765, 47.95351654967443977, 25.00000000000000000 ) ) ;
#51345 = DIRECTION ( 'NONE',  ( 0.000000000000000000, 1.000000000000000000, 0.000000000000000000 ) ) ;
#51346 = EDGE_LOOP ( 'NONE', ( #17476, #26945, #14860, #26694 ) ) ;
#51347 = EDGE_CURVE ( 'NONE', #38001, #15827, #27633, .T. ) ;
#51348 = DIRECTION ( 'NONE',  ( 0.000000000000000000, 1.000000000000000000, 0.000000000000000000 ) ) ;
#51349 = VERTEX_POINT ( 'NONE', #65133 ) ;
#51350 = AXIS2_PLACEMENT_3D ( 'NONE', #17621, #5984, #65723 ) ;
#51351 = ORIENTED_EDGE ( 'NONE', *, *, #32159, .F. ) ;
#51352 = DIRECTION ( 'NONE',  ( 1.221996412923863792E-14, 1.000000000000000000, 1.836970198721013910E-16 ) ) ;
#51353 = DIRECTION ( 'NONE',  ( 1.000000000000000000, 0.000000000000000000, 0.000000000000000000 ) ) ;
#51354 = LINE ( 'NONE', #46749, #51409 ) ;
#51355 = CIRCLE ( 'NONE', #58132, 0.8100000000000017186 ) ;
#51356 = DIRECTION ( 'NONE',  ( 0.000000000000000000, 0.000000000000000000, -1.000000000000000000 ) ) ;
#51357 = CARTESIAN_POINT ( 'NONE',  ( -8.598420958951633608, -1.480523737882746271, 54.00000000000000711 ) ) ;
#51358 = VERTEX_POINT ( 'NONE', #10675 ) ;
#51359 = ADVANCED_FACE ( 'NONE', ( #16329, #21639 ), #425, .F. ) ;
#51360 = EDGE_LOOP ( 'NONE', ( #58780, #23383, #45174, #27912 ) ) ;
#51362 = ORIENTED_EDGE ( 'NONE', *, *, #65856, .F. ) ;
#51361 = CARTESIAN_POINT ( 'NONE',  ( -8.697938382363103571, -2.420780051175099423, 54.00000000000000711 ) ) ;
#51364 = ORIENTED_EDGE ( 'NONE', *, *, #60831, .T. ) ;
#51363 = EDGE_CURVE ( 'NONE', #15117, #28651, #37214, .T. ) ;
#51365 = VECTOR ( 'NONE', #47430, 1000.000000000000000 ) ;
#51366 = VECTOR ( 'NONE', #60778, 1000.000000000000000 ) ;
#51367 = CARTESIAN_POINT ( 'NONE',  ( 10.09643294401453062, 2.693516549646537417, 455.0000000000000568 ) ) ;
#51368 = CARTESIAN_POINT ( 'NONE',  ( 11.90000000000000036, -14.06939075806902117, -20.80000000000000426 ) ) ;
#51369 = CARTESIAN_POINT ( 'NONE',  ( -8.250000000000000000, 7.250000000000001776, -8.000000000000000000 ) ) ;
#51370 = DIRECTION ( 'NONE',  ( -0.000000000000000000, -0.000000000000000000, -1.000000000000000000 ) ) ;
#51371 = CARTESIAN_POINT ( 'NONE',  ( 4.406483450353420928, 11.77351654964658501, 455.0000000000000568 ) ) ;
#51372 = VECTOR ( 'NONE', #32162, 1000.000000000000000 ) ;
#51373 = DIRECTION ( 'NONE',  ( 1.000000000000000000, -0.000000000000000000, -0.000000000000000000 ) ) ;
#51374 = VERTEX_POINT ( 'NONE', #49547 ) ;
#51375 = ADVANCED_FACE ( 'NONE', ( #5394 ), #81, .F. ) ;
#51376 = ORIENTED_EDGE ( 'NONE', *, *, #8336, .F. ) ;
#51377 = EDGE_LOOP ( 'NONE', ( #30619, #36451, #56596, #61729 ) ) ;
#51379 = ORIENTED_EDGE ( 'NONE', *, *, #3869, .T. ) ;
#51378 = VECTOR ( 'NONE', #35817, 1000.000000000000000 ) ;
#51380 = CARTESIAN_POINT ( 'NONE',  ( 7.250000000000005329, 8.250000000000001776, -23.00000000000000000 ) ) ;
#51381 = DIRECTION ( 'NONE',  ( 0.000000000000000000, 0.000000000000000000, 1.000000000000000000 ) ) ;
#51382 = SHAPE_REPRESENTATION_RELATIONSHIP ( 'NONE' , 'NONE' ,  #49776, #8117 ) ;
#51383 = AXIS2_PLACEMENT_3D ( 'NONE', #40547, #8364, #20041 ) ;
#51384 = DIRECTION ( 'NONE',  ( -1.000000000000000000, 0.000000000000000000, 0.000000000000000000 ) ) ;
#51385 = ORIENTED_EDGE ( 'NONE', *, *, #33805, .F. ) ;
#51386 = EDGE_LOOP ( 'NONE', ( #30928, #351, #66987, #35277, #41081, #44051, #22634, #23047, #43267, #19579, #49064 ) ) ;
#51387 = ORIENTED_EDGE ( 'NONE', *, *, #43149, .F. ) ;
#51388 = VECTOR ( 'NONE', #15430, 1000.000000000000000 ) ;
#51389 = LINE ( 'NONE', #40437, #57648 ) ;
#51390 = ORIENTED_EDGE ( 'NONE', *, *, #33037, .F. ) ;
#51391 = VERTEX_POINT ( 'NONE', #11028 ) ;
#51392 = DIRECTION ( 'NONE',  ( -7.304098846218132892E-15, -1.000000000000000000, 0.000000000000000000 ) ) ;
#51393 = VERTEX_POINT ( 'NONE', #48511 ) ;
#51394 = EDGE_CURVE ( 'NONE', #55707, #9246, #32936, .T. ) ;
#51395 = VERTEX_POINT ( 'NONE', #1116 ) ;
#51396 = PLANE ( 'NONE',  #54226 ) ;
#51398 = EDGE_LOOP ( 'NONE', ( #62293, #59474, #64836, #42987 ) ) ;
#51397 = CARTESIAN_POINT ( 'NONE',  ( 151.5599459900709860, -10.00000000000000178, 280.6301873289890523 ) ) ;
#51399 = VERTEX_POINT ( 'NONE', #784 ) ;
#51400 = EDGE_CURVE ( 'NONE', #40232, #2123, #54175, .T. ) ;
#51401 = CARTESIAN_POINT ( 'NONE',  ( -9.791916549646856538, -10.20488345035338718, 455.0000000000000568 ) ) ;
#51402 = DIRECTION ( 'NONE',  ( 0.000000000000000000, 0.000000000000000000, 1.000000000000000000 ) ) ;
#51403 = CARTESIAN_POINT ( 'NONE',  ( 1.090483450353343819, -10.74648345035345365, 455.0000000000000568 ) ) ;
#51404 = EDGE_CURVE ( 'NONE', #30081, #58674, #10335, .T. ) ;
#51406 = ORIENTED_EDGE ( 'NONE', *, *, #14716, .F. ) ;
#51405 = FACE_OUTER_BOUND ( 'NONE', #16777, .T. ) ;
#51407 = ORIENTED_EDGE ( 'NONE', *, *, #49732, .F. ) ;
#51408 = EDGE_CURVE ( 'NONE', #28592, #49752, #43196, .T. ) ;
#51409 = VECTOR ( 'NONE', #52063, 1000.000000000000000 ) ;
#51410 = LINE ( 'NONE', #34086, #56551 ) ;
#51411 = CARTESIAN_POINT ( 'NONE',  ( -7.250000000000000888, -8.249999999999998224, -21.00000000000000000 ) ) ;
#51412 = CARTESIAN_POINT ( 'NONE',  ( 176.4833316329832940, 9.000000000000001776, 280.6301873289890523 ) ) ;
#51413 = EDGE_CURVE ( 'NONE', #63027, #1158, #59119, .T. ) ;
#51414 = ORIENTED_EDGE ( 'NONE', *, *, #21833, .F. ) ;
#51415 = DIRECTION ( 'NONE',  ( 0.000000000000000000, 3.673940397442059868E-16, -1.000000000000000000 ) ) ;
#51416 = CIRCLE ( 'NONE', #46871, 0.1999999999999996503 ) ;
#51417 = VECTOR ( 'NONE', #2805, 1000.000000000000000 ) ;
#51419 = DIRECTION ( 'NONE',  ( -1.836970198721029934E-16, 1.836970198721036344E-16, -1.000000000000000000 ) ) ;
#51418 = VECTOR ( 'NONE', #28513, 1000.000000000000000 ) ;
#51420 = CARTESIAN_POINT ( 'NONE',  ( 30.00000000000000000, -11.10796162543699950, -9.102987789146602893 ) ) ;
#51421 = VERTEX_POINT ( 'NONE', #53479 ) ;
#51422 = EDGE_CURVE ( 'NONE', #66946, #31134, #1304, .T. ) ;
#51423 = CARTESIAN_POINT ( 'NONE',  ( 3.677663764522608680, 6.350872789121272177, 54.00000000000000711 ) ) ;
#51424 = EDGE_CURVE ( 'NONE', #60302, #65501, #64558, .T. ) ;
#51425 = DIRECTION ( 'NONE',  ( -0.000000000000000000, -0.000000000000000000, -1.000000000000000000 ) ) ;
#51426 = VECTOR ( 'NONE', #9479, 1000.000000000000000 ) ;
#51427 = VECTOR ( 'NONE', #15389, 1000.000000000000000 ) ;
#51428 = DIRECTION ( 'NONE',  ( -1.221996412923863792E-14, -1.000000000000000000, 0.000000000000000000 ) ) ;
#51429 = DIRECTION ( 'NONE',  ( 0.8660254037850496633, 0.000000000000000000, 0.4999999999989417909 ) ) ;
#51430 = ADVANCED_FACE ( 'NONE', ( #42850 ), #21293, .F. ) ;
#51431 = EDGE_CURVE ( 'NONE', #974, #42297, #64430, .T. ) ;
#51432 = ORIENTED_EDGE ( 'NONE', *, *, #54969, .T. ) ;
#51433 = VECTOR ( 'NONE', #67042, 1000.000000000000000 ) ;
#51434 = CARTESIAN_POINT ( 'NONE',  ( 41.09999999999999432, -14.06939075806900163, 20.80000000000000426 ) ) ;
#51435 = CARTESIAN_POINT ( 'NONE',  ( 5.257023737882819070, -4.032023737882816761, 26.00000000000000711 ) ) ;
#51436 = EDGE_CURVE ( 'NONE', #17298, #61584, #65468, .T. ) ;
#51437 = CIRCLE ( 'NONE', #25453, 0.9999999999999991118 ) ;
#51438 = VERTEX_POINT ( 'NONE', #17024 ) ;
#51439 = DIRECTION ( 'NONE',  ( 0.8660254037844562491, 0.4999999999999695244, 2.509347957447841320E-16 ) ) ;
#51440 = FACE_OUTER_BOUND ( 'NONE', #31929, .T. ) ;
#51441 = DIRECTION ( 'NONE',  ( 0.000000000000000000, -1.000000000000000000, -3.673940397442059868E-16 ) ) ;
#51442 = VECTOR ( 'NONE', #31187, 1000.000000000000000 ) ;
#51443 = CARTESIAN_POINT ( 'NONE',  ( -15.50000000000000000, -0.4000000000005236034, -25.79999999999947136 ) ) ;
#51444 = CARTESIAN_POINT ( 'NONE',  ( 47.00000000000000000, -0.7500000000000000000, 3.418698582794334584 ) ) ;
#51445 = EDGE_LOOP ( 'NONE', ( #49655, #23126, #22823, #1824 ) ) ;
#51446 = DIRECTION ( 'NONE',  ( 1.000000000000000000, -8.540177112501197482E-15, 0.000000000000000000 ) ) ;
#51447 = CYLINDRICAL_SURFACE ( 'NONE', #54260, 0.5999999999999998668 ) ;
#51448 = CARTESIAN_POINT ( 'NONE',  ( 10.74648345035334529, 1.077516549646528876, 455.0000000000000568 ) ) ;
#51449 =( LENGTH_UNIT ( ) NAMED_UNIT ( * ) SI_UNIT ( .MILLI., .METRE. ) );
#51450 = CARTESIAN_POINT ( 'NONE',  ( -9.791916549646712653, 10.19191654964664018, 455.0000000000000568 ) ) ;
#51451 = EDGE_CURVE ( 'NONE', #16300, #64382, #27298, .T. ) ;
#51452 = ORIENTED_EDGE ( 'NONE', *, *, #47815, .F. ) ;
#51454 = ORIENTED_EDGE ( 'NONE', *, *, #63329, .F. ) ;
#51453 = FACE_OUTER_BOUND ( 'NONE', #69648, .T. ) ;
#51455 = ADVANCED_FACE ( 'NONE', ( #38257 ), #54861, .F. ) ;
#51456 = DIRECTION ( 'NONE',  ( 0.000000000000000000, 0.000000000000000000, 1.000000000000000000 ) ) ;
#51457 = PLANE ( 'NONE',  #17580 ) ;
#51458 = DIRECTION ( 'NONE',  ( -9.912705577010336396E-15, -1.000000000000000000, 0.000000000000000000 ) ) ;
#51459 = ORIENTED_EDGE ( 'NONE', *, *, #24679, .F. ) ;
#51460 = VECTOR ( 'NONE', #38383, 1000.000000000000000 ) ;
#51461 = CARTESIAN_POINT ( 'NONE',  ( -7.393516549646727221, -6.006483450353401921, 195.0000000000000284 ) ) ;
#51462 = VERTEX_POINT ( 'NONE', #50234 ) ;
#51463 = AXIS2_PLACEMENT_3D ( 'NONE', #51448, #2649, #62390 ) ;
#51464 = ORIENTED_EDGE ( 'NONE', *, *, #34942, .F. ) ;
#51465 = ORIENTED_EDGE ( 'NONE', *, *, #55080, .F. ) ;
#51466 = CYLINDRICAL_SURFACE ( 'NONE', #40776, 2.458500000000000796 ) ;
#51467 = CARTESIAN_POINT ( 'NONE',  ( -13.00000000000000178, -16.64230188589299786, 14.64519951917100116 ) ) ;
#51468 = CARTESIAN_POINT ( 'NONE',  ( 2.765062094116107705, 9.942044687070449527, 455.0000000000000568 ) ) ;
#51469 = CARTESIAN_POINT ( 'NONE',  ( 7.806483450353418618, 11.31351654964657172, 455.0000000000000568 ) ) ;
#51470 = VECTOR ( 'NONE', #20271, 1000.000000000000000 ) ;
#51471 = CIRCLE ( 'NONE', #20992, 0.9999999999999991118 ) ;
#51472 = CIRCLE ( 'NONE', #53767, 0.2999999999998732569 ) ;
#51473 = VERTEX_POINT ( 'NONE', #2140 ) ;
#51474 = ORIENTED_EDGE ( 'NONE', *, *, #52517, .F. ) ;
#51475 = CARTESIAN_POINT ( 'NONE',  ( 16.33757311576526305, -0.3152598339554795182, 21.54019739087904384 ) ) ;
#51476 = CARTESIAN_POINT ( 'NONE',  ( 275.0000000000000000, -31.30000000000000071, -12.69999999999999929 ) ) ;
#51477 = VECTOR ( 'NONE', #40084, 1000.000000000000000 ) ;
#51478 = VECTOR ( 'NONE', #47294, 1000.000000000000000 ) ;
#51479 = VECTOR ( 'NONE', #18058, 1000.000000000000000 ) ;
#51480 = ORIENTED_EDGE ( 'NONE', *, *, #12782, .T. ) ;
#51481 = EDGE_CURVE ( 'NONE', #37047, #24795, #9233, .T. ) ;
#51482 = ORIENTED_EDGE ( 'NONE', *, *, #19765, .F. ) ;
#51483 = ORIENTED_EDGE ( 'NONE', *, *, #23473, .T. ) ;
#51484 = CIRCLE ( 'NONE', #18774, 4.000000000000000000 ) ;
#51485 = LINE ( 'NONE', #63140, #34979 ) ;
#51487 = ORIENTED_EDGE ( 'NONE', *, *, #11487, .T. ) ;
#51486 = LINE ( 'NONE', #45827, #40541 ) ;
#51488 = ADVANCED_FACE ( 'NONE', ( #12731 ), #9108, .T. ) ;
#51489 = CARTESIAN_POINT ( 'NONE',  ( -11.50000000000000000, -12.00000000000000000, -11.00000000000000000 ) ) ;
#51490 = VECTOR ( 'NONE', #47710, 1000.000000000000000 ) ;
#51491 = CARTESIAN_POINT ( 'NONE',  ( 15.50000000000000000, -2.500000000000000000, -21.05662432702600029 ) ) ;
#51492 = ORIENTED_EDGE ( 'NONE', *, *, #41521, .T. ) ;
#51493 = AXIS2_PLACEMENT_3D ( 'NONE', #4919, #26482, #48045 ) ;
#51494 = EDGE_CURVE ( 'NONE', #61865, #60944, #18386, .T. ) ;
#51495 = VERTEX_POINT ( 'NONE', #66833 ) ;
#51496 = EDGE_CURVE ( 'NONE', #7623, #10256, #17716, .T. ) ;
#51497 = EDGE_CURVE ( 'NONE', #701, #51774, #35979, .T. ) ;
#51498 = CARTESIAN_POINT ( 'NONE',  ( -7.342976262117288933, -6.665817930929258672, 26.00000000000000000 ) ) ;
#51499 = DIRECTION ( 'NONE',  ( 0.000000000000000000, 1.000000000000000000, 0.000000000000000000 ) ) ;
#51500 = EDGE_CURVE ( 'NONE', #32498, #34317, #39953, .T. ) ;
#51501 = EDGE_CURVE ( 'NONE', #44814, #21914, #60492, .T. ) ;
#51502 = DIRECTION ( 'NONE',  ( 0.000000000000000000, 0.000000000000000000, -1.000000000000000000 ) ) ;
#51503 = DIRECTION ( 'NONE',  ( 1.000000000000000000, 0.000000000000000000, 0.000000000000000000 ) ) ;
#51504 = DIRECTION ( 'NONE',  ( -0.000000000000000000, -0.000000000000000000, -1.000000000000000000 ) ) ;
#51505 = VECTOR ( 'NONE', #65859, 1000.000000000000000 ) ;
#51507 = ORIENTED_EDGE ( 'NONE', *, *, #38116, .T. ) ;
#51506 = CARTESIAN_POINT ( 'NONE',  ( 7.450000000000004619, -1.336933437520057563E-15, -20.00000000000000000 ) ) ;
#51508 = VERTEX_POINT ( 'NONE', #14419 ) ;
#51509 = DIRECTION ( 'NONE',  ( -8.480870326997715333E-15, 0.000000000000000000, 1.000000000000000000 ) ) ;
#51510 = DIRECTION ( 'NONE',  ( 0.000000000000000000, 0.000000000000000000, 1.000000000000000000 ) ) ;
#51511 = DIRECTION ( 'NONE',  ( 0.000000000000000000, -1.000000000000000000, -1.922073611378672844E-12 ) ) ;
#51512 = VECTOR ( 'NONE', #59286, 1000.000000000000000 ) ;
#51513 = DIRECTION ( 'NONE',  ( 0.000000000000000000, -1.000000000000000000, -0.000000000000000000 ) ) ;
#51514 = CIRCLE ( 'NONE', #68432, 24.99999999998789946 ) ;
#51515 = CARTESIAN_POINT ( 'NONE',  ( -10.91351654964670637, 2.693516549646604030, 455.0000000000000568 ) ) ;
#51516 = ORIENTED_EDGE ( 'NONE', *, *, #22120, .T. ) ;
#51517 = DIRECTION ( 'NONE',  ( 1.000000000000000000, 0.000000000000000000, 0.000000000000000000 ) ) ;
#51518 = CARTESIAN_POINT ( 'NONE',  ( -31.00000000000000000, -2.500000000000000000, 0.000000000000000000 ) ) ;
#51519 = LINE ( 'NONE', #57169, #37965 ) ;
#51520 = VECTOR ( 'NONE', #11414, 1000.000000000000000 ) ;
#51521 = CIRCLE ( 'NONE', #26703, 1.000000000000000000 ) ;
#51522 = AXIS2_PLACEMENT_3D ( 'NONE', #47751, #38543, #53421 ) ;
#51523 = DIRECTION ( 'NONE',  ( 0.000000000000000000, 0.000000000000000000, -1.000000000000000000 ) ) ;
#51524 = DIRECTION ( 'NONE',  ( -1.000000000000000000, 0.000000000000000000, 0.000000000000000000 ) ) ;
#51525 = AXIS2_PLACEMENT_3D ( 'NONE', #54223, #10726, #16381 ) ;
#51526 = VECTOR ( 'NONE', #58082, 1000.000000000000000 ) ;
#51527 = CIRCLE ( 'NONE', #21053, 24.99999999998794920 ) ;
#51528 = LINE ( 'NONE', #20048, #40891 ) ;
#51529 = ORIENTED_EDGE ( 'NONE', *, *, #14356, .T. ) ;
#51530 = DIRECTION ( 'NONE',  ( 0.000000000000000000, 0.000000000000000000, 1.000000000000000000 ) ) ;
#51531 = CARTESIAN_POINT ( 'NONE',  ( 0.2500000000000000000, -0.2499999999999970302, -26.75000000000000000 ) ) ;
#51532 = ORIENTED_EDGE ( 'NONE', *, *, #53520, .T. ) ;
#51533 = FACE_OUTER_BOUND ( 'NONE', #64425, .T. ) ;
#51534 = CARTESIAN_POINT ( 'NONE',  ( 275.2500000000000000, -42.25000000000000000, -26.75000000000000000 ) ) ;
#51535 = VECTOR ( 'NONE', #49153, 1000.000000000000000 ) ;
#51536 = DIRECTION ( 'NONE',  ( -0.000000000000000000, 1.000000000000000000, -0.000000000000000000 ) ) ;
#51537 = CARTESIAN_POINT ( 'NONE',  ( -7.250000000000001776, -7.249999999999998224, -17.50000000000000000 ) ) ;
#51538 = CARTESIAN_POINT ( 'NONE',  ( 22.90000000000000213, -14.06939075806902117, -20.80000000000000426 ) ) ;
#51539 = ORIENTED_EDGE ( 'NONE', *, *, #31831, .F. ) ;
#51540 = DIRECTION ( 'NONE',  ( 1.836970198721029934E-16, -1.836970198721036344E-16, 1.000000000000000000 ) ) ;
#51541 = EDGE_CURVE ( 'NONE', #67695, #69235, #29507, .T. ) ;
#51542 = AXIS2_PLACEMENT_3D ( 'NONE', #7912, #29488, #45742 ) ;
#51543 = ORIENTED_EDGE ( 'NONE', *, *, #35693, .T. ) ;
#51544 = CARTESIAN_POINT ( 'NONE',  ( -23.48000000000000043, -15.50000000000000000, 26.00000000000000355 ) ) ;
#51545 = CARTESIAN_POINT ( 'NONE',  ( 30.00000000000000000, 0.000000000000000000, -27.00000000000000000 ) ) ;
#51546 = ORIENTED_EDGE ( 'NONE', *, *, #39047, .T. ) ;
#51547 = ADVANCED_FACE ( 'NONE', ( #24050 ), #39278, .F. ) ;
#51548 = CARTESIAN_POINT ( 'NONE',  ( 3.664523737882781518, -10.31452373788281029, 54.00000000000000711 ) ) ;
#51549 = ORIENTED_EDGE ( 'NONE', *, *, #17237, .T. ) ;
#51550 = DIRECTION ( 'NONE',  ( 1.836970198721029934E-16, 1.836970198721010706E-16, -1.000000000000000000 ) ) ;
#51551 = VERTEX_POINT ( 'NONE', #7087 ) ;
#51552 = EDGE_LOOP ( 'NONE', ( #16707, #63951, #48447, #52761 ) ) ;
#51553 = LINE ( 'NONE', #34916, #12633 ) ;
#51554 = ORIENTED_EDGE ( 'NONE', *, *, #4612, .T. ) ;
#51555 = ORIENTED_EDGE ( 'NONE', *, *, #30941, .F. ) ;
#51556 = CARTESIAN_POINT ( 'NONE',  ( -17.24945551514599984, -15.50000000000000000, -25.53140320652400064 ) ) ;
#51557 = DIRECTION ( 'NONE',  ( -0.7071067811865550112, -0.7071067811865401342, -2.597868168706466299E-16 ) ) ;
#51558 = DIRECTION ( 'NONE',  ( 1.000000000000000000, -0.000000000000000000, -0.000000000000000000 ) ) ;
#51559 = STYLED_ITEM ( 'NONE', ( #17334 ), #20363 ) ;
#51560 = ORIENTED_EDGE ( 'NONE', *, *, #46784, .F. ) ;
#51561 = FACE_OUTER_BOUND ( 'NONE', #68290, .T. ) ;
#51563 = DIRECTION ( 'NONE',  ( 0.000000000000000000, -1.000000000000000000, 0.000000000000000000 ) ) ;
#51562 = DIRECTION ( 'NONE',  ( 0.000000000000000000, 0.000000000000000000, 1.000000000000000000 ) ) ;
#51564 = ORIENTED_EDGE ( 'NONE', *, *, #20225, .F. ) ;
#51566 = ORIENTED_EDGE ( 'NONE', *, *, #18678, .F. ) ;
#51565 = FACE_OUTER_BOUND ( 'NONE', #9381, .T. ) ;
#51567 = AXIS2_PLACEMENT_3D ( 'NONE', #19897, #41467, #41104 ) ;
#51568 = ORIENTED_EDGE ( 'NONE', *, *, #3204, .F. ) ;
#51569 = SHAPE_DEFINITION_REPRESENTATION ( #13649, #64253 ) ;
#51570 = AXIS2_PLACEMENT_3D ( 'NONE', #54478, #33585, #6033 ) ;
#51571 = CIRCLE ( 'NONE', #25594, 1.000000000000000000 ) ;
#51572 = DIRECTION ( 'NONE',  ( 0.000000000000000000, 0.000000000000000000, 1.000000000000000000 ) ) ;
#51574 = ORIENTED_EDGE ( 'NONE', *, *, #4025, .T. ) ;
#51573 = CARTESIAN_POINT ( 'NONE',  ( 8.250000000000005329, 7.250000000000000888, -23.00000000000000000 ) ) ;
#51575 = AXIS2_PLACEMENT_3D ( 'NONE', #46904, #68494, #41612 ) ;
#51576 = EDGE_CURVE ( 'NONE', #40696, #39543, #60834, .T. ) ;
#51577 = AXIS2_PLACEMENT_3D ( 'NONE', #36358, #15156, #46265 ) ;
#51578 = CARTESIAN_POINT ( 'NONE',  ( -13.00000000000000178, -16.28999999999710369, 15.00000000000794920 ) ) ;
#51579 = DIRECTION ( 'NONE',  ( -0.7071067811865474617, 0.7071067811865474617, 0.000000000000000000 ) ) ;
#51580 = ORIENTED_EDGE ( 'NONE', *, *, #63512, .F. ) ;
#51581 = ORIENTED_EDGE ( 'NONE', *, *, #12897, .F. ) ;
#51582 = CIRCLE ( 'NONE', #42555, 0.8100000000000017186 ) ;
#51583 = VECTOR ( 'NONE', #18588, 1000.000000000000000 ) ;
#51584 = FACE_OUTER_BOUND ( 'NONE', #57638, .T. ) ;
#51585 = ORIENTED_EDGE ( 'NONE', *, *, #48827, .T. ) ;
#51586 = FACE_OUTER_BOUND ( 'NONE', #52082, .T. ) ;
#51587 = DIRECTION ( 'NONE',  ( 1.000000000000000000, -0.000000000000000000, 0.000000000000000000 ) ) ;
#51588 = EDGE_CURVE ( 'NONE', #69402, #43890, #59996, .T. ) ;
#51589 = LINE ( 'NONE', #13744, #62201 ) ;
#51590 = EDGE_CURVE ( 'NONE', #28734, #14243, #38561, .T. ) ;
#51591 = ORIENTED_EDGE ( 'NONE', *, *, #9938, .T. ) ;
#51592 = VECTOR ( 'NONE', #32213, 1000.000000000000000 ) ;
#51593 = EDGE_CURVE ( 'NONE', #40067, #15576, #29013, .T. ) ;
#51594 = CARTESIAN_POINT ( 'NONE',  ( 41.09999999999999432, 20.60000000000000142, -13.86939075806900057 ) ) ;
#51595 = DIRECTION ( 'NONE',  ( 1.079558018506126625E-14, 1.000000000000000000, 1.836970198721016622E-16 ) ) ;
#51597 = ORIENTED_EDGE ( 'NONE', *, *, #356, .T. ) ;
#51596 = LINE ( 'NONE', #9505, #369 ) ;
#51599 = ORIENTED_EDGE ( 'NONE', *, *, #52625, .F. ) ;
#51598 = DIRECTION ( 'NONE',  ( 1.000000000000000000, 0.000000000000000000, 0.000000000000000000 ) ) ;
#51600 = LINE ( 'NONE', #23662, #61098 ) ;
#51601 = CARTESIAN_POINT ( 'NONE',  ( 283.0000000000000568, -23.65000000000000568, 12.40000000000000213 ) ) ;
#51602 = LINE ( 'NONE', #39574, #52781 ) ;
#51603 = CARTESIAN_POINT ( 'NONE',  ( 11.78648345035337819, -4.406483450353490205, 455.0000000000000568 ) ) ;
#51604 = CARTESIAN_POINT ( 'NONE',  ( -5.993516549646711766, 5.993516549646603409, 195.0000000000000284 ) ) ;
#51605 = ORIENTED_EDGE ( 'NONE', *, *, #56858, .F. ) ;
#51606 = CARTESIAN_POINT ( 'NONE',  ( -11.00000000000000000, -16.64230188589299786, -14.64519951917100116 ) ) ;
#51607 = DIRECTION ( 'NONE',  ( 0.000000000000000000, 0.000000000000000000, 1.000000000000000000 ) ) ;
#51608 = LINE ( 'NONE', #26142, #30038 ) ;
#51610 = ORIENTED_EDGE ( 'NONE', *, *, #28229, .F. ) ;
#51609 = DIRECTION ( 'NONE',  ( -0.000000000000000000, -0.000000000000000000, -1.000000000000000000 ) ) ;
#51611 = CARTESIAN_POINT ( 'NONE',  ( 282.6457513110646005, -25.50000000000000355, 17.00000000000000000 ) ) ;
#51612 = VECTOR ( 'NONE', #36389, 1000.000000000000000 ) ;
#51613 = CARTESIAN_POINT ( 'NONE',  ( -2.277516549646682709, 9.828310488885916740, 455.0000000000000568 ) ) ;
#51614 = EDGE_LOOP ( 'NONE', ( #5841, #53173, #69407, #21851 ) ) ;
#51615 = ORIENTED_EDGE ( 'NONE', *, *, #7853, .F. ) ;
#51616 = CARTESIAN_POINT ( 'NONE',  ( 40.90000000000000568, 0.000000000000000000, 0.000000000000000000 ) ) ;
#51617 = LINE ( 'NONE', #62214, #46415 ) ;
#51618 = VERTEX_POINT ( 'NONE', #13087 ) ;
#51619 = LINE ( 'NONE', #36399, #17535 ) ;
#51620 = VECTOR ( 'NONE', #28540, 1000.000000000000000 ) ;
#51621 = LINE ( 'NONE', #23352, #14465 ) ;
#51622 = B_SPLINE_CURVE_WITH_KNOTS ( 'NONE', 3,
 ( #52240, #52955, #36678, #62850, #41978, #4513 ),
 .UNSPECIFIED., .F., .F.,
 ( 4, 2, 4 ),
 ( 0.0002380763768129734448, 0.7291065797294585815, 1.457975083082104328 ),
 .UNSPECIFIED. ) ;
#51623 = LINE ( 'NONE', #67885, #15798 ) ;
#51624 = AXIS2_PLACEMENT_3D ( 'NONE', #41091, #45340, #66912 ) ;
#51626 = DIRECTION ( 'NONE',  ( 1.000000000000000000, 0.000000000000000000, 0.000000000000000000 ) ) ;
#51625 = CIRCLE ( 'NONE', #45967, 0.5249999999999994671 ) ;
#51627 = VERTEX_POINT ( 'NONE', #34661 ) ;
#51628 = AXIS2_PLACEMENT_3D ( 'NONE', #23634, #45197, #17641 ) ;
#51629 = LINE ( 'NONE', #3193, #1173 ) ;
#51630 = EDGE_LOOP ( 'NONE', ( #16724, #67218, #47289, #9124 ) ) ;
#51631 = PLANE ( 'NONE',  #41984 ) ;
#51632 = ORIENTED_EDGE ( 'NONE', *, *, #31562, .F. ) ;
#51633 = ADVANCED_FACE ( 'NONE', ( #17359 ), #38931, .T. ) ;
#51634 = EDGE_CURVE ( 'NONE', #66814, #16172, #45344, .T. ) ;
#51635 = CARTESIAN_POINT ( 'NONE',  ( 7.000000000000000000, -30.80000000000000071, 12.20000000000000107 ) ) ;
#51636 = EDGE_CURVE ( 'NONE', #48269, #54080, #1443, .T. ) ;
#51637 = CIRCLE ( 'NONE', #15512, 1.000000000000000000 ) ;
#51638 = AXIS2_PLACEMENT_3D ( 'NONE', #62581, #30776, #67196 ) ;
#51639 = ADVANCED_FACE ( 'NONE', ( #66148 ), #59290, .F. ) ;
#51640 = CARTESIAN_POINT ( 'NONE',  ( 11.12648345035337982, -4.206483450353492692, 455.0000000000000568 ) ) ;
#51641 = VERTEX_POINT ( 'NONE', #26778 ) ;
#51642 = ORIENTED_EDGE ( 'NONE', *, *, #23682, .F. ) ;
#51643 = CARTESIAN_POINT ( 'NONE',  ( 7.250000000000005329, 7.250000000000000888, -26.00000000000001066 ) ) ;
#51644 = ORIENTED_EDGE ( 'NONE', *, *, #54726, .T. ) ;
#51645 = ORIENTED_EDGE ( 'NONE', *, *, #4944, .F. ) ;
#51646 = VECTOR ( 'NONE', #67521, 1000.000000000000000 ) ;
#51647 = FACE_OUTER_BOUND ( 'NONE', #33574, .T. ) ;
#51648 = CARTESIAN_POINT ( 'NONE',  ( 7.450000000000004619, -1.336933437520057563E-15, -24.50000000000000000 ) ) ;
#51649 = FACE_OUTER_BOUND ( 'NONE', #27637, .T. ) ;
#51650 = CARTESIAN_POINT ( 'NONE',  ( 41.09999999999999432, -14.06939075806901940, -20.80000000000000426 ) ) ;
#51651 = ORIENTED_EDGE ( 'NONE', *, *, #42493, .T. ) ;
#51652 = DIRECTION ( 'NONE',  ( 0.000000000000000000, 1.000000000000000000, 0.000000000000000000 ) ) ;
#51654 = DIRECTION ( 'NONE',  ( 0.5000000000000019984, 0.8660254037844375974, 3.181725716174716554E-16 ) ) ;
#51653 = CARTESIAN_POINT ( 'NONE',  ( -8.821682069070746479, -2.369523737882742953, 54.00000000000000711 ) ) ;
#51655 = ORIENTED_EDGE ( 'NONE', *, *, #23559, .F. ) ;
#51657 = EDGE_LOOP ( 'NONE', ( #12613, #45822, #998, #21619 ) ) ;
#51656 = DIRECTION ( 'NONE',  ( 0.000000000000000000, 1.000000000000000000, 0.000000000000000000 ) ) ;
#51658 = ORIENTED_EDGE ( 'NONE', *, *, #30121, .T. ) ;
#51659 = ORIENTED_EDGE ( 'NONE', *, *, #9454, .T. ) ;
#51660 = DIRECTION ( 'NONE',  ( 0.000000000000000000, -1.000000000000000000, 0.000000000000000000 ) ) ;
#51661 = DIRECTION ( 'NONE',  ( 0.000000000000000000, -0.1111111111108840643, -0.9938079899999319178 ) ) ;
#51662 = VERTEX_POINT ( 'NONE', #16160 ) ;
#51663 = AXIS2_PLACEMENT_3D ( 'NONE', #61237, #61588, #28727 ) ;
#51664 = ORIENTED_EDGE ( 'NONE', *, *, #51102, .T. ) ;
#51665 = DIRECTION ( 'NONE',  ( -0.000000000000000000, -0.000000000000000000, -1.000000000000000000 ) ) ;
#51666 = CARTESIAN_POINT ( 'NONE',  ( 10.90000000000000036, -0.1999999999911430404, -8.864436962241481021E-12 ) ) ;
#51667 = EDGE_LOOP ( 'NONE', ( #43047, #17135, #54634, #2605 ) ) ;
#51668 = ORIENTED_EDGE ( 'NONE', *, *, #38625, .T. ) ;
#51669 = CIRCLE ( 'NONE', #18907, 0.1999999999999996503 ) ;
#51670 = AXIS2_PLACEMENT_3D ( 'NONE', #25711, #30646, #58218 ) ;
#51672 = LINE ( 'NONE', #29738, #48890 ) ;
#51671 = VECTOR ( 'NONE', #9418, 1000.000000000000000 ) ;
#51673 = CARTESIAN_POINT ( 'NONE',  ( 289.5000000000000000, 0.000000000000000000, 26.50000000000000000 ) ) ;
#51674 = ORIENTED_EDGE ( 'NONE', *, *, #25862, .T. ) ;
#51675 = EDGE_CURVE ( 'NONE', #19785, #58687, #54416, .T. ) ;
#51676 = CIRCLE ( 'NONE', #3118, 24.99999999998784972 ) ;
#51677 = VECTOR ( 'NONE', #50968, 1000.000000000000000 ) ;
#51678 = EDGE_CURVE ( 'NONE', #58634, #856, #41981, .T. ) ;
#51679 = CARTESIAN_POINT ( 'NONE',  ( 5.257023737882819070, -5.257023737882825287, 54.00000000000000711 ) ) ;
#51680 = DIRECTION ( 'NONE',  ( -1.000000000000000000, 0.000000000000000000, 0.000000000000000000 ) ) ;
#51681 = EDGE_CURVE ( 'NONE', #59582, #64203, #20761, .T. ) ;
#51683 = ORIENTED_EDGE ( 'NONE', *, *, #15531, .F. ) ;
#51682 = DIRECTION ( 'NONE',  ( -1.000000000000000000, 0.000000000000000000, 0.000000000000000000 ) ) ;
#51684 = ORIENTED_EDGE ( 'NONE', *, *, #951, .T. ) ;
#51685 = CARTESIAN_POINT ( 'NONE',  ( 7.250000000000005329, -7.249999999999998224, -26.00000000000001066 ) ) ;
#51686 = CIRCLE ( 'NONE', #927, 1.449999999999999956 ) ;
#51687 = CYLINDRICAL_SURFACE ( 'NONE', #64994, 0.5000000000079367624 ) ;
#51688 = AXIS2_PLACEMENT_3D ( 'NONE', #23197, #33804, #65317 ) ;
#51689 = EDGE_CURVE ( 'NONE', #9560, #50838, #11484, .T. ) ;
#51690 = CARTESIAN_POINT ( 'NONE',  ( -7.342976262117252517, -3.848229544836288429, 54.00000000000000711 ) ) ;
#51691 = DIRECTION ( 'NONE',  ( 0.000000000000000000, -1.000000000000000000, 0.000000000000000000 ) ) ;
#51692 = LINE ( 'NONE', #40720, #8623 ) ;
#51693 = LINE ( 'NONE', #8532, #65575 ) ;
#51694 = ADVANCED_FACE ( 'NONE', ( #58606 ), #10851, .T. ) ;
#51695 = CARTESIAN_POINT ( 'NONE',  ( 15.50000000000000000, -5.000000000000000000, 26.50000000000000000 ) ) ;
#51696 = ORIENTED_EDGE ( 'NONE', *, *, #50062, .F. ) ;
#51697 = CARTESIAN_POINT ( 'NONE',  ( 1.090483450353338268, -11.34648345035335737, 195.0000000000000284 ) ) ;
#51698 = ADVANCED_FACE ( 'NONE', ( #31396 ), #48758, .T. ) ;
#51700 = ORIENTED_EDGE ( 'NONE', *, *, #58383, .F. ) ;
#51699 = CARTESIAN_POINT ( 'NONE',  ( 7.250000000000005329, 7.250000000000000888, -21.00000000000000000 ) ) ;
#51701 = VECTOR ( 'NONE', #40890, 1000.000000000000000 ) ;
#51702 = CARTESIAN_POINT ( 'NONE',  ( -4.727349090213461835, 4.188533722949259186, 195.0000000000000284 ) ) ;
#51703 = DIRECTION ( 'NONE',  ( 0.000000000000000000, 0.000000000000000000, -1.000000000000000000 ) ) ;
#51704 = CARTESIAN_POINT ( 'NONE',  ( 28.00000000000000000, -15.50000000000000000, 20.05051025721700242 ) ) ;
#51705 = CARTESIAN_POINT ( 'NONE',  ( 105.8309041053263257, 3.657408540445008960, 10.00000000000000000 ) ) ;
#51706 = CARTESIAN_POINT ( 'NONE',  ( -7.250000000000001776, -7.249999999999998224, -11.00000000000000000 ) ) ;
#51707 = ORIENTED_EDGE ( 'NONE', *, *, #28619, .F. ) ;
#51708 = LINE ( 'NONE', #19511, #36998 ) ;
#51709 = CYLINDRICAL_SURFACE ( 'NONE', #7942, 0.5000000000001357803 ) ;
#51710 = ORIENTED_EDGE ( 'NONE', *, *, #15717, .T. ) ;
#51711 = PLANE ( 'NONE',  #23442 ) ;
#51712 = DIRECTION ( 'NONE',  ( 0.000000000000000000, 0.000000000000000000, -1.000000000000000000 ) ) ;
#51713 = ORIENTED_EDGE ( 'NONE', *, *, #25297, .F. ) ;
#51714 = CARTESIAN_POINT ( 'NONE',  ( 28.00000000000000000, -17.00000000000000000, 15.70499999999969809 ) ) ;
#51715 = ORIENTED_EDGE ( 'NONE', *, *, #49912, .T. ) ;
#51716 = AXIS2_PLACEMENT_3D ( 'NONE', #8907, #63722, #57353 ) ;
#51717 = VERTEX_POINT ( 'NONE', #54002 ) ;
#51718 = FACE_OUTER_BOUND ( 'NONE', #23566, .T. ) ;
#51719 = FACE_OUTER_BOUND ( 'NONE', #58142, .T. ) ;
#51720 = FACE_OUTER_BOUND ( 'NONE', #61770, .T. ) ;
#51721 = CARTESIAN_POINT ( 'NONE',  ( -9.722976262117258628, 7.290476262117236317, 54.00000000000000711 ) ) ;
#51722 = DIRECTION ( 'NONE',  ( -1.000000000000000000, 0.000000000000000000, 0.000000000000000000 ) ) ;
#51723 = ORIENTED_EDGE ( 'NONE', *, *, #16070, .T. ) ;
#51724 = VERTEX_POINT ( 'NONE', #52607 ) ;
#51726 = VERTEX_POINT ( 'NONE', #15476 ) ;
#51725 = CARTESIAN_POINT ( 'NONE',  ( 5.257023737882801306, 5.242976262117200470, 54.00000000000000711 ) ) ;
#51727 = ORIENTED_EDGE ( 'NONE', *, *, #42479, .T. ) ;
#51728 = AXIS2_PLACEMENT_3D ( 'NONE', #67465, #1699, #17958 ) ;
#51729 = PLANE ( 'NONE',  #34841 ) ;
#51730 = LINE ( 'NONE', #67989, #13977 ) ;
#51731 = CARTESIAN_POINT ( 'NONE',  ( -8.393516549646712122, 4.383466043307770121, 195.0000000000000284 ) ) ;
#51732 = CARTESIAN_POINT ( 'NONE',  ( 0.000000000000000000, -7.449999999999998401, -20.50000000000000000 ) ) ;
#51733 = VECTOR ( 'NONE', #33222, 1000.000000000000000 ) ;
#51735 = DIRECTION ( 'NONE',  ( 0.000000000000000000, 0.000000000000000000, -1.000000000000000000 ) ) ;
#51734 = VECTOR ( 'NONE', #68789, 1000.000000000000000 ) ;
#51736 = EDGE_CURVE ( 'NONE', #50249, #24514, #15120, .T. ) ;
#51737 = DIRECTION ( 'NONE',  ( -1.836970198721029934E-16, 1.836970198721036344E-16, -1.000000000000000000 ) ) ;
#51738 = VERTEX_POINT ( 'NONE', #31738 ) ;
#51739 = ORIENTED_EDGE ( 'NONE', *, *, #59667, .F. ) ;
#51740 = ORIENTED_EDGE ( 'NONE', *, *, #60291, .F. ) ;
#51741 = VERTEX_POINT ( 'NONE', #57892 ) ;
#51742 = EDGE_CURVE ( 'NONE', #65063, #42085, #4749, .T. ) ;
#51743 = DIRECTION ( 'NONE',  ( -0.000000000000000000, -0.000000000000000000, -1.000000000000000000 ) ) ;
#51744 = DIRECTION ( 'NONE',  ( 0.000000000000000000, 0.000000000000000000, -1.000000000000000000 ) ) ;
#51745 = AXIS2_PLACEMENT_3D ( 'NONE', #49279, #43614, #69441 ) ;
#51746 = CARTESIAN_POINT ( 'NONE',  ( 8.835729544836331328, 8.130476262117188213, 54.00000000000000711 ) ) ;
#51747 = ORIENTED_EDGE ( 'NONE', *, *, #31827, .F. ) ;
#51748 = EDGE_LOOP ( 'NONE', ( #66687, #26284 ) ) ;
#51749 = VERTEX_POINT ( 'NONE', #32077 ) ;
#51750 = LINE ( 'NONE', #53170, #1188 ) ;
#51751 = EDGE_LOOP ( 'NONE', ( #14672, #11372, #58053 ) ) ;
#51752 = ORIENTED_EDGE ( 'NONE', *, *, #42701, .F. ) ;
#51753 = DIRECTION ( 'NONE',  ( -1.000000000000000000, 0.000000000000000000, 0.000000000000000000 ) ) ;
#51754 = EDGE_CURVE ( 'NONE', #40990, #1707, #38615, .T. ) ;
#51755 = ORIENTED_EDGE ( 'NONE', *, *, #33387, .T. ) ;
#51756 = EDGE_LOOP ( 'NONE', ( #32168, #56872, #56897, #1132 ) ) ;
#51757 = CARTESIAN_POINT ( 'NONE',  ( 283.0000000000000568, -26.28355339059299922, 9.766446609406699508 ) ) ;
#51758 = B_SPLINE_CURVE_WITH_KNOTS ( 'NONE', 3,
 ( #315, #53721, #1348, #43793, #38492, #64662 ),
 .UNSPECIFIED., .F., .F.,
 ( 4, 2, 4 ),
 ( 0.0002380763768132926339, 0.7291065797294586925, 1.457975083082104106 ),
 .UNSPECIFIED. ) ;
#51760 = ORIENTED_EDGE ( 'NONE', *, *, #22071, .T. ) ;
#51759 = CARTESIAN_POINT ( 'NONE',  ( 24.00000000000000000, -17.50000000000000000, 19.33772233983200195 ) ) ;
#51761 = VERTEX_POINT ( 'NONE', #20415 ) ;
#51762 = CARTESIAN_POINT ( 'NONE',  ( 8.144523737882817471, -9.562023737882817898, 54.00000000000000711 ) ) ;
#51763 = FACE_BOUND ( 'NONE', #52145, .T. ) ;
#51764 = EDGE_CURVE ( 'NONE', #31019, #19555, #26423, .T. ) ;
#51765 = CARTESIAN_POINT ( 'NONE',  ( 17.89999999999999858, 20.60000000000000142, 13.86939075806899702 ) ) ;
#51767 = ORIENTED_EDGE ( 'NONE', *, *, #64526, .F. ) ;
#51766 = CARTESIAN_POINT ( 'NONE',  ( 283.0000000000000568, -20.40000000000000213, -12.40000000000000213 ) ) ;
#51768 = VERTEX_POINT ( 'NONE', #9823 ) ;
#51769 = DIRECTION ( 'NONE',  ( 0.5773502691896175154, 0.5773502691896339467, -0.5773502691896257311 ) ) ;
#51770 = LINE ( 'NONE', #8627, #13696 ) ;
#51771 = CARTESIAN_POINT ( 'NONE',  ( -11.11351654964674474, -7.806483450353326248, 195.0000000000000284 ) ) ;
#51772 = CYLINDRICAL_SURFACE ( 'NONE', #27118, 2.204799999999999205 ) ;
#51773 = EDGE_CURVE ( 'NONE', #13228, #51111, #37731, .T. ) ;
#51774 = VERTEX_POINT ( 'NONE', #42680 ) ;
#51775 = DIRECTION ( 'NONE',  ( 0.000000000000000000, 1.000000000000000000, 0.000000000000000000 ) ) ;
#51776 = EDGE_CURVE ( 'NONE', #41058, #68319, #21462, .T. ) ;
#51777 = CIRCLE ( 'NONE', #56306, 0.5249999999999990230 ) ;
#51778 = DIRECTION ( 'NONE',  ( 0.6414496315691469164, -0.7671651518153087546, -2.587583378555128790E-16 ) ) ;
#51779 = CARTESIAN_POINT ( 'NONE',  ( -15.50000000000000000, -5.000000000000000000, 22.50000000000000000 ) ) ;
#51780 = ORIENTED_EDGE ( 'NONE', *, *, #17557, .T. ) ;
#51781 = CARTESIAN_POINT ( 'NONE',  ( -2.355476262117325525, -9.562023737882830332, 54.00000000000000711 ) ) ;
#51782 = DIRECTION ( 'NONE',  ( 0.000000000000000000, 0.000000000000000000, 1.000000000000000000 ) ) ;
#51783 = AXIS2_PLACEMENT_3D ( 'NONE', #14464, #16817, #22119 ) ;
#51784 = DIRECTION ( 'NONE',  ( 0.4999999999989417354, 0.000000000000000000, -0.8660254037850495523 ) ) ;
#51785 = EDGE_CURVE ( 'NONE', #19388, #17980, #61190, .T. ) ;
#51786 = EDGE_LOOP ( 'NONE', ( #32517, #31390, #8951, #26180 ) ) ;
#51787 = DIRECTION ( 'NONE',  ( -7.665540703601096574E-15, -1.000000000000000000, -3.673940397442059868E-16 ) ) ;
#51788 = CARTESIAN_POINT ( 'NONE',  ( -8.393516549646768965, -5.668387132715940524, 455.0000000000000568 ) ) ;
#51789 = VECTOR ( 'NONE', #1506, 1000.000000000000000 ) ;
#51790 = CARTESIAN_POINT ( 'NONE',  ( -9.293516549646710700, 10.91351654964659801, 455.0000000000000568 ) ) ;
#51791 = ORIENTED_EDGE ( 'NONE', *, *, #44925, .T. ) ;
#51792 = LINE ( 'NONE', #30570, #13468 ) ;
#51793 = LINE ( 'NONE', #47195, #45536 ) ;
#51794 = DIRECTION ( 'NONE',  ( -1.000000000000000000, 3.491481338843133355E-15, 0.000000000000000000 ) ) ;
#51795 = CYLINDRICAL_SURFACE ( 'NONE', #14374, 1.000000000000000000 ) ;
#51796 = CARTESIAN_POINT ( 'NONE',  ( -30.00000000000000000, -11.50000000000100009, 15.00000000000084910 ) ) ;
#51797 = ORIENTED_EDGE ( 'NONE', *, *, #30187, .F. ) ;
#51798 = DIRECTION ( 'NONE',  ( -0.000000000000000000, -0.000000000000000000, -1.000000000000000000 ) ) ;
#51799 = FACE_OUTER_BOUND ( 'NONE', #9612, .T. ) ;
#51800 = DIRECTION ( 'NONE',  ( -1.000000000000000000, 0.000000000000000000, 0.000000000000000000 ) ) ;
#51801 = EDGE_CURVE ( 'NONE', #18984, #69246, #69205, .T. ) ;
#51802 = PLANE ( 'NONE',  #9133 ) ;
#51803 = VERTEX_POINT ( 'NONE', #5554 ) ;
#51805 = ORIENTED_EDGE ( 'NONE', *, *, #6172, .F. ) ;
#51804 = CARTESIAN_POINT ( 'NONE',  ( 7.250000000000005329, -8.249999999999998224, -26.00000000000001066 ) ) ;
#51806 = EDGE_CURVE ( 'NONE', #28114, #20102, #20068, .T. ) ;
#51807 = FACE_OUTER_BOUND ( 'NONE', #2408, .T. ) ;
#51808 = CARTESIAN_POINT ( 'NONE',  ( 9.690000000000001279, 8.750000000000000000, -7.000000000000000000 ) ) ;
#51809 = DIRECTION ( 'NONE',  ( 1.000000000000000000, 0.000000000000000000, 0.000000000000000000 ) ) ;
#51810 = ORIENTED_EDGE ( 'NONE', *, *, #3929, .F. ) ;
#51811 = EDGE_CURVE ( 'NONE', #50899, #37032, #27815, .T. ) ;
#51812 = LINE ( 'NONE', #28827, #13757 ) ;
#51813 = EDGE_CURVE ( 'NONE', #67274, #59501, #39447, .T. ) ;
#51814 = ORIENTED_EDGE ( 'NONE', *, *, #9942, .F. ) ;
#51815 = CIRCLE ( 'NONE', #40496, 1.000000000000000000 ) ;
#51816 = ORIENTED_EDGE ( 'NONE', *, *, #30738, .T. ) ;
#51817 = EDGE_CURVE ( 'NONE', #34737, #57047, #67977, .T. ) ;
#51818 = EDGE_LOOP ( 'NONE', ( #22841, #32105, #14487, #46779 ) ) ;
#51819 = FACE_OUTER_BOUND ( 'NONE', #22515, .T. ) ;
#51820 = DIRECTION ( 'NONE',  ( 1.836970198721029934E-16, -1.836970198721036344E-16, 1.000000000000000000 ) ) ;
#51821 = VECTOR ( 'NONE', #37221, 1000.000000000000000 ) ;
#51822 = DIRECTION ( 'NONE',  ( 0.000000000000000000, -0.7046037717806115097, -0.7096009616626348659 ) ) ;
#51823 = FACE_OUTER_BOUND ( 'NONE', #47158, .T. ) ;
#51824 = EDGE_LOOP ( 'NONE', ( #18576, #42266, #39163, #412 ) ) ;
#51825 = EDGE_CURVE ( 'NONE', #8763, #37085, #45397, .T. ) ;
#51826 = VERTEX_POINT ( 'NONE', #43730 ) ;
#51827 = FACE_OUTER_BOUND ( 'NONE', #10535, .T. ) ;
#51828 = ADVANCED_FACE ( 'NONE', ( #65306 ), #49034, .F. ) ;
#51829 = CIRCLE ( 'NONE', #22510, 4.500000000000190958 ) ;
#51830 = CARTESIAN_POINT ( 'NONE',  ( -7.259684009079963474, -4.201500623656036382, 455.0000000000000568 ) ) ;
#51831 = ORIENTED_EDGE ( 'NONE', *, *, #15503, .F. ) ;
#51832 = EDGE_CURVE ( 'NONE', #51045, #52304, #5898, .T. ) ;
#51833 = VERTEX_POINT ( 'NONE', #17531 ) ;
#51834 = EDGE_CURVE ( 'NONE', #45446, #54520, #44061, .T. ) ;
#51835 = EDGE_CURVE ( 'NONE', #5241, #36344, #21809, .T. ) ;
#51836 = ORIENTED_EDGE ( 'NONE', *, *, #26448, .F. ) ;
#51837 = CIRCLE ( 'NONE', #58608, 4.000000000000000888 ) ;
#51838 = ORIENTED_EDGE ( 'NONE', *, *, #28232, .F. ) ;
#51839 = FACE_OUTER_BOUND ( 'NONE', #5757, .T. ) ;
#51841 = ORIENTED_EDGE ( 'NONE', *, *, #7408, .T. ) ;
#51840 = DIRECTION ( 'NONE',  ( 0.000000000000000000, -1.000000000000000000, 0.000000000000000000 ) ) ;
#51842 = ADVANCED_FACE ( 'NONE', ( #55717 ), #6592, .F. ) ;
#51844 = VECTOR ( 'NONE', #56099, 1000.000000000000000 ) ;
#51843 = VECTOR ( 'NONE', #42658, 1000.000000000000000 ) ;
#51845 = LINE ( 'NONE', #24626, #24324 ) ;
#51846 = DIRECTION ( 'NONE',  ( -1.000000000000000000, 0.000000000000000000, 0.000000000000000000 ) ) ;
#51847 = EDGE_CURVE ( 'NONE', #23882, #15959, #66333, .T. ) ;
#51848 = ORIENTED_EDGE ( 'NONE', *, *, #21271, .T. ) ;
#51849 = ORIENTED_EDGE ( 'NONE', *, *, #33836, .F. ) ;
#51850 = VECTOR ( 'NONE', #31533, 1000.000000000000000 ) ;
#51851 = CARTESIAN_POINT ( 'NONE',  ( -7.250000000000000000, -7.449999999999998401, -23.50000000000000000 ) ) ;
#51852 = DIRECTION ( 'NONE',  ( -1.000000000000000000, 0.000000000000000000, 0.000000000000000000 ) ) ;
#51853 = EDGE_CURVE ( 'NONE', #56701, #27098, #54689, .T. ) ;
#51854 = DIRECTION ( 'NONE',  ( -1.000000000000000000, 0.000000000000000000, 0.000000000000000000 ) ) ;
#51855 = ADVANCED_FACE ( 'NONE', ( #38426 ), #59976, .T. ) ;
#51856 = CARTESIAN_POINT ( 'NONE',  ( 8.580623737882849156, 9.689726262117156708, 54.00000000000000711 ) ) ;
#51857 = CARTESIAN_POINT ( 'NONE',  ( 290.0000000000000000, 0.000000000000000000, 27.00000000000000000 ) ) ;
#51859 = VERTEX_POINT ( 'NONE', #43370 ) ;
#51858 = LINE ( 'NONE', #51506, #1717 ) ;
#51860 = ORIENTED_EDGE ( 'NONE', *, *, #44870, .T. ) ;
#51861 = CARTESIAN_POINT ( 'NONE',  ( 34.89999999999999858, -21.00000000000000000, 13.86939075806900057 ) ) ;
#51862 = CARTESIAN_POINT ( 'NONE',  ( 7.250000000000005329, 7.250000000000000888, -26.00000000000001066 ) ) ;
#51863 = CARTESIAN_POINT ( 'NONE',  ( 12.90000000000000213, 20.60000000000000142, -13.86939075806900057 ) ) ;
#51864 = LINE ( 'NONE', #26049, #29075 ) ;
#51865 = AXIS2_PLACEMENT_3D ( 'NONE', #23817, #7885, #45370 ) ;
#51866 = DIRECTION ( 'NONE',  ( -1.000000000000000000, 0.000000000000000000, 0.000000000000000000 ) ) ;
#51867 = ORIENTED_EDGE ( 'NONE', *, *, #11775, .F. ) ;
#51868 = CARTESIAN_POINT ( 'NONE',  ( 7.450000000000003730, -7.249999999999997335, -23.00000000000000000 ) ) ;
#51869 = DIRECTION ( 'NONE',  ( -1.836970198721029934E-16, 1.836970198721036344E-16, -1.000000000000000000 ) ) ;
#51870 = VECTOR ( 'NONE', #8386, 1000.000000000000000 ) ;
#51871 = CARTESIAN_POINT ( 'NONE',  ( -11.11351654964674474, -7.806483450353326248, 195.0000000000000284 ) ) ;
#51872 = AXIS2_PLACEMENT_3D ( 'NONE', #44154, #17283, #60409 ) ;
#51873 = CARTESIAN_POINT ( 'NONE',  ( -7.955476262117259445, 8.821682069070703847, 54.00000000000000711 ) ) ;
#51874 = LINE ( 'NONE', #18279, #34856 ) ;
#51875 = DIRECTION ( 'NONE',  ( 0.000000000000000000, 0.000000000000000000, -1.000000000000000000 ) ) ;
#51876 = VECTOR ( 'NONE', #15960, 1000.000000000000000 ) ;
#51877 = CARTESIAN_POINT ( 'NONE',  ( 15.50000000000000000, -17.50000000000000000, -22.50000000000000000 ) ) ;
#51878 = ORIENTED_EDGE ( 'NONE', *, *, #32575, .F. ) ;
#51879 = CARTESIAN_POINT ( 'NONE',  ( 290.0000000000000000, 0.000000000000000000, 0.000000000000000000 ) ) ;
#51880 = LINE ( 'NONE', #23947, #32738 ) ;
#51881 = VERTEX_POINT ( 'NONE', #23187 ) ;
#51882 = DIRECTION ( 'NONE',  ( 1.000000000000000000, -5.981805089575194965E-17, 0.000000000000000000 ) ) ;
#51883 = DIRECTION ( 'NONE',  ( 1.000000000000000000, -0.000000000000000000, 0.000000000000000000 ) ) ;
#51884 = AXIS2_PLACEMENT_3D ( 'NONE', #46184, #41228, #25325 ) ;
#51885 = LINE ( 'NONE', #41620, #65985 ) ;
#51886 = CARTESIAN_POINT ( 'NONE',  ( -7.955476262117259445, 8.821682069070703847, 26.00000000000000711 ) ) ;
#51887 = LINE ( 'NONE', #23601, #11297 ) ;
#51888 = ORIENTED_EDGE ( 'NONE', *, *, #50967, .T. ) ;
#51889 = AXIS2_PLACEMENT_3D ( 'NONE', #38070, #59624, #65945 ) ;
#51890 = EDGE_CURVE ( 'NONE', #24192, #58614, #49391, .T. ) ;
#51891 = DIRECTION ( 'NONE',  ( 0.000000000000000000, 1.000000000000000000, 0.000000000000000000 ) ) ;
#51892 = VERTEX_POINT ( 'NONE', #1614 ) ;
#51893 = PLANE ( 'NONE',  #4929 ) ;
#51894 = CARTESIAN_POINT ( 'NONE',  ( 6.364920264886889001, 6.822336235477383326, 54.00000000000000711 ) ) ;
#51895 = ORIENTED_EDGE ( 'NONE', *, *, #27573, .T. ) ;
#51896 = ADVANCED_FACE ( 'NONE', ( #1283 ), #16513, .T. ) ;
#51897 = CARTESIAN_POINT ( 'NONE',  ( 0.5000000000000000000, -18.00000000000000355, 21.00000000000000000 ) ) ;
#51898 = CIRCLE ( 'NONE', #60912, 0.2000000000000005107 ) ;
#51899 = ADVANCED_FACE ( 'NONE', ( #38090, #33108 ), #17189, .T. ) ;
#51900 = EDGE_LOOP ( 'NONE', ( #14258, #69538, #53495, #31974 ) ) ;
#51901 = CARTESIAN_POINT ( 'NONE',  ( 7.250000000000005329, 8.250000000000001776, -13.50000000000000178 ) ) ;
#51902 = ORIENTED_EDGE ( 'NONE', *, *, #9912, .T. ) ;
#51903 = EDGE_CURVE ( 'NONE', #30310, #34997, #32765, .T. ) ;
#51904 = VERTEX_POINT ( 'NONE', #35903 ) ;
#51905 = FACE_OUTER_BOUND ( 'NONE', #68894, .T. ) ;
#51906 = ORIENTED_EDGE ( 'NONE', *, *, #30157, .F. ) ;
#51907 = ORIENTED_EDGE ( 'NONE', *, *, #24037, .F. ) ;
#51908 = CARTESIAN_POINT ( 'NONE',  ( -10.30047626211725742, 3.650476262117184234, 54.00000000000000711 ) ) ;
#51909 = LINE ( 'NONE', #3471, #11060 ) ;
#51910 = DIRECTION ( 'NONE',  ( 0.000000000000000000, 1.000000000000000000, 0.000000000000000000 ) ) ;
#51911 = VECTOR ( 'NONE', #56605, 1000.000000000000000 ) ;
#51912 = ORIENTED_EDGE ( 'NONE', *, *, #13180, .F. ) ;
#51913 = DIRECTION ( 'NONE',  ( 1.000000000000000000, -0.000000000000000000, -0.000000000000000000 ) ) ;
#51915 = FACE_OUTER_BOUND ( 'NONE', #8742, .T. ) ;
#51914 = LINE ( 'NONE', #47652, #31575 ) ;
#51916 = ORIENTED_EDGE ( 'NONE', *, *, #5210, .F. ) ;
#51918 = ORIENTED_EDGE ( 'NONE', *, *, #58865, .F. ) ;
#51917 = FACE_BOUND ( 'NONE', #65846, .T. ) ;
#51919 = VERTEX_POINT ( 'NONE', #3374 ) ;
#51920 = ADVANCED_FACE ( 'NONE', ( #45442 ), #57458, .F. ) ;
#51921 = APPLICATION_PROTOCOL_DEFINITION ( 'draft international standard', 'automotive_design', 1998, #20094 ) ;
#51922 = DIRECTION ( 'NONE',  ( 0.000000000000000000, 0.000000000000000000, -1.000000000000000000 ) ) ;
#51923 = VECTOR ( 'NONE', #37301, 1000.000000000000000 ) ;
#51924 = AXIS2_PLACEMENT_3D ( 'NONE', #34842, #7629, #62065 ) ;
#51926 = VERTEX_POINT ( 'NONE', #2663 ) ;
#51925 = CARTESIAN_POINT ( 'NONE',  ( 11.00000000000000000, -10.85999999999999943, 9.000000000000001776 ) ) ;
#51927 = DIRECTION ( 'NONE',  ( 0.000000000000000000, -1.000000000000000000, 0.000000000000000000 ) ) ;
#51928 = CIRCLE ( 'NONE', #59848, 0.1749999999999998224 ) ;
#51929 = DIRECTION ( 'NONE',  ( 1.000000000000000000, 0.000000000000000000, 0.000000000000000000 ) ) ;
#51930 = ORIENTED_EDGE ( 'NONE', *, *, #33843, .F. ) ;
#51931 = ORIENTED_EDGE ( 'NONE', *, *, #18678, .T. ) ;
#51932 = FACE_OUTER_BOUND ( 'NONE', #58967, .T. ) ;
#51933 = VERTEX_POINT ( 'NONE', #62056 ) ;
#51934 = CARTESIAN_POINT ( 'NONE',  ( -10.49297626211729018, -6.849523737882743823, 26.00000000000000000 ) ) ;
#51935 = LINE ( 'NONE', #34949, #31278 ) ;
#51936 = CYLINDRICAL_SURFACE ( 'NONE', #55450, 0.2000000000000005107 ) ;
#51937 = VECTOR ( 'NONE', #39387, 1000.000000000000000 ) ;
#51938 = EDGE_CURVE ( 'NONE', #30889, #7937, #34833, .T. ) ;
#51939 = EDGE_LOOP ( 'NONE', ( #49051, #34037, #3866, #69310 ) ) ;
#51940 = AXIS2_PLACEMENT_3D ( 'NONE', #68680, #14225, #46395 ) ;
#51941 = EDGE_CURVE ( 'NONE', #64793, #6389, #62402, .T. ) ;
#51942 = LINE ( 'NONE', #4219, #61751 ) ;
#51943 = FACE_OUTER_BOUND ( 'NONE', #47656, .T. ) ;
#51945 = VERTEX_POINT ( 'NONE', #50418 ) ;
#51944 = EDGE_CURVE ( 'NONE', #27522, #53301, #51812, .T. ) ;
#51947 = VERTEX_POINT ( 'NONE', #41192 ) ;
#51946 = CARTESIAN_POINT ( 'NONE',  ( -9.547976262117254365, 2.355476262117183417, 54.00000000000000711 ) ) ;
#51948 = DIRECTION ( 'NONE',  ( 0.4999999999989361843, 0.000000000000000000, 0.8660254037850529940 ) ) ;
#51949 = CIRCLE ( 'NONE', #28213, 0.1999999999999996503 ) ;
#51950 = VECTOR ( 'NONE', #13990, 1000.000000000000000 ) ;
#51951 = PLANE ( 'NONE',  #51047 ) ;
#51952 = FACE_OUTER_BOUND ( 'NONE', #29140, .T. ) ;
#51953 = PLANE ( 'NONE',  #77 ) ;
#51954 = DIRECTION ( 'NONE',  ( 0.000000000000000000, 1.000000000000000000, 0.000000000000000000 ) ) ;
#51955 = ORIENTED_EDGE ( 'NONE', *, *, #52722, .T. ) ;
#51956 = DIRECTION ( 'NONE',  ( -1.000000000000000000, 1.047444401652940007E-14, -1.836970198721010706E-16 ) ) ;
#51957 = DIRECTION ( 'NONE',  ( -0.000000000000000000, -0.000000000000000000, 1.000000000000000000 ) ) ;
#51958 = CARTESIAN_POINT ( 'NONE',  ( 7.250000000000005329, 7.250000000000000888, -21.50000000000000000 ) ) ;
#51960 = ORIENTED_EDGE ( 'NONE', *, *, #31562, .T. ) ;
#51959 = DIRECTION ( 'NONE',  ( 1.000000000000000000, -5.981805089575194965E-17, 0.000000000000000000 ) ) ;
#51961 = DIRECTION ( 'NONE',  ( 0.000000000000000000, 0.000000000000000000, -1.000000000000000000 ) ) ;
#51962 = VECTOR ( 'NONE', #20010, 1000.000000000000000 ) ;
#51963 = DIRECTION ( 'NONE',  ( -1.000000000000000000, 0.000000000000000000, 0.000000000000000000 ) ) ;
#51964 = ORIENTED_EDGE ( 'NONE', *, *, #31529, .T. ) ;
#51965 = CARTESIAN_POINT ( 'NONE',  ( 151.5599459900709860, 9.000000000000001776, 322.4587476295993156 ) ) ;
#51966 = CARTESIAN_POINT ( 'NONE',  ( -10.19191654964671301, 10.19191654964664018, 455.0000000000000568 ) ) ;
#51967 = VERTEX_POINT ( 'NONE', #23537 ) ;
#51968 = CARTESIAN_POINT ( 'NONE',  ( -3.650476262117221093, 10.49297626211717116, 54.00000000000000711 ) ) ;
#51969 = CARTESIAN_POINT ( 'NONE',  ( 41.09999999999999432, -21.00000000000000000, 13.86939075806900057 ) ) ;
#51970 = DIRECTION ( 'NONE',  ( 1.000000000000000000, 0.000000000000000000, 0.000000000000000000 ) ) ;
#51971 = CIRCLE ( 'NONE', #23745, 0.1999999999999987899 ) ;
#51972 = EDGE_CURVE ( 'NONE', #33646, #66510, #30731, .T. ) ;
#51973 = DIRECTION ( 'NONE',  ( 0.000000000000000000, 0.000000000000000000, -1.000000000000000000 ) ) ;
#51974 = CIRCLE ( 'NONE', #30520, 0.5000000000004167777 ) ;
#51975 = EDGE_LOOP ( 'NONE', ( #47565, #40711, #25577, #9750 ) ) ;
#51976 = CARTESIAN_POINT ( 'NONE',  ( -10.91351654964670637, 9.293516549646604119, 455.0000000000000568 ) ) ;
#51977 = ORIENTED_EDGE ( 'NONE', *, *, #17616, .F. ) ;
#51978 = CARTESIAN_POINT ( 'NONE',  ( -7.517976262117260333, 6.651770455163663165, 26.00000000000000711 ) ) ;
#51979 = ORIENTED_EDGE ( 'NONE', *, *, #28002, .F. ) ;
#51981 = EDGE_CURVE ( 'NONE', #39378, #42765, #19284, .T. ) ;
#51980 = AXIS2_PLACEMENT_3D ( 'NONE', #32733, #38394, #65281 ) ;
#51982 = CARTESIAN_POINT ( 'NONE',  ( 69.92576880110368620, 10.00000000000000000, 281.4830310981151911 ) ) ;
#51983 = ADVANCED_FACE ( 'NONE', ( #2322 ), #39785, .F. ) ;
#51984 = ADVANCED_FACE ( 'NONE', ( #7962 ), #35534, .T. ) ;
#51985 = AXIS2_PLACEMENT_3D ( 'NONE', #58340, #53037, #9900 ) ;
#51986 = DIRECTION ( 'NONE',  ( 0.000000000000000000, 0.000000000000000000, 1.000000000000000000 ) ) ;
#51987 = CARTESIAN_POINT ( 'NONE',  ( 49.00000000000000000, 13.66939075806899950, 20.80000000000000426 ) ) ;
#51988 = ORIENTED_EDGE ( 'NONE', *, *, #26777, .F. ) ;
#51989 = EDGE_CURVE ( 'NONE', #31769, #37208, #54464, .T. ) ;
#51990 = ORIENTED_EDGE ( 'NONE', *, *, #30224, .F. ) ;
#51991 = ADVANCED_FACE ( 'NONE', ( #66673 ), #30252, .F. ) ;
#51992 = AXIS2_PLACEMENT_3D ( 'NONE', #23403, #59844, #28020 ) ;
#51993 = FACE_OUTER_BOUND ( 'NONE', #26888, .T. ) ;
#51994 = ORIENTED_EDGE ( 'NONE', *, *, #29112, .F. ) ;
#51995 = ORIENTED_EDGE ( 'NONE', *, *, #62422, .F. ) ;
#51996 = DIRECTION ( 'NONE',  ( 8.673617379884087537E-15, 1.000000000000000000, 0.000000000000000000 ) ) ;
#51997 = LINE ( 'NONE', #57642, #44791 ) ;
#51998 = CARTESIAN_POINT ( 'NONE',  ( -16.54686605390241994, -0.2715358723599897717, -21.66103272505201360 ) ) ;
#51999 = EDGE_CURVE ( 'NONE', #31208, #58107, #3033, .T. ) ;
#52000 = LINE ( 'NONE', #51650, #23004 ) ;
#52001 = ORIENTED_EDGE ( 'NONE', *, *, #62202, .F. ) ;
#52002 = DIRECTION ( 'NONE',  ( 0.000000000000000000, 0.000000000000000000, -1.000000000000000000 ) ) ;
#52003 = VECTOR ( 'NONE', #20554, 1000.000000000000000 ) ;
#52004 = AXIS2_PLACEMENT_3D ( 'NONE', #7893, #50685, #61993 ) ;
#52006 = DIRECTION ( 'NONE',  ( -1.000000000000000000, 0.000000000000000000, 0.000000000000000000 ) ) ;
#52005 = DIRECTION ( 'NONE',  ( -0.000000000000000000, 1.000000000000000000, -0.000000000000000000 ) ) ;
#52007 = ORIENTED_EDGE ( 'NONE', *, *, #49200, .F. ) ;
#52009 = ORIENTED_EDGE ( 'NONE', *, *, #61454, .F. ) ;
#52008 = DIRECTION ( 'NONE',  ( 0.000000000000000000, -0.2142857142857146346, -0.9767710236555243730 ) ) ;
#52010 = VERTEX_POINT ( 'NONE', #56068 ) ;
#52011 = ORIENTED_EDGE ( 'NONE', *, *, #20670, .F. ) ;
#52012 = CARTESIAN_POINT ( 'NONE',  ( 8.711985858128693749, -8.093267424590459669, 26.00000000000000000 ) ) ;
#52013 = DIRECTION ( 'NONE',  ( -0.000000000000000000, -0.000000000000000000, -1.000000000000000000 ) ) ;
#52014 = CONICAL_SURFACE ( 'NONE', #39565, 1732.050807568789651, 1.047197551196575871 ) ;
#52015 = ORIENTED_EDGE ( 'NONE', *, *, #6875, .F. ) ;
#52016 = VERTEX_POINT ( 'NONE', #51461 ) ;
#52017 = DIRECTION ( 'NONE',  ( -1.000000000000000000, 0.000000000000000000, 0.000000000000000000 ) ) ;
#52018 = CARTESIAN_POINT ( 'NONE',  ( -7.250000000000001776, -7.249999999999998224, -7.500000000000000000 ) ) ;
#52019 = ORIENTED_EDGE ( 'NONE', *, *, #18728, .T. ) ;
#52020 = EDGE_LOOP ( 'NONE', ( #11787, #28911, #39827, #56208 ) ) ;
#52021 = DIRECTION ( 'NONE',  ( -0.000000000000000000, 3.673940397442059868E-16, -1.000000000000000000 ) ) ;
#52022 = DIRECTION ( 'NONE',  ( 0.000000000000000000, 0.000000000000000000, 1.000000000000000000 ) ) ;
#52023 = VECTOR ( 'NONE', #26466, 1000.000000000000000 ) ;
#52024 = ORIENTED_EDGE ( 'NONE', *, *, #13487, .F. ) ;
#52025 = VECTOR ( 'NONE', #62984, 1000.000000000000000 ) ;
#52026 = DIRECTION ( 'NONE',  ( -1.203165845134433242E-14, -1.000000000000000000, -1.836970198721014403E-16 ) ) ;
#52027 = DIRECTION ( 'NONE',  ( -0.000000000000000000, 3.673940397442059868E-16, -1.000000000000000000 ) ) ;
#52030 = ORIENTED_EDGE ( 'NONE', *, *, #45750, .T. ) ;
#52029 = ADVANCED_FACE ( 'NONE', ( #7622 ), #29179, .F. ) ;
#52028 = CARTESIAN_POINT ( 'NONE',  ( 2.765062094116041980, -9.955011587777324422, 455.0000000000000568 ) ) ;
#52031 = ORIENTED_EDGE ( 'NONE', *, *, #41299, .T. ) ;
#52032 = VECTOR ( 'NONE', #67538, 1000.000000000000000 ) ;
#52033 = ADVANCED_FACE ( 'NONE', ( #13625 ), #40133, .T. ) ;
#52034 = CARTESIAN_POINT ( 'NONE',  ( -5.993516549646711766, 5.993516549646603409, 195.0000000000000284 ) ) ;
#52035 = DIRECTION ( 'NONE',  ( 0.000000000000000000, 0.000000000000000000, 1.000000000000000000 ) ) ;
#52036 = CARTESIAN_POINT ( 'NONE',  ( -29.50000000000000355, -11.70000000000000284, -11.00000000000000000 ) ) ;
#52037 = LINE ( 'NONE', #68655, #8677 ) ;
#52038 = EDGE_CURVE ( 'NONE', #2156, #47666, #60048, .T. ) ;
#52039 = VECTOR ( 'NONE', #11958, 1000.000000000000000 ) ;
#52040 = DIRECTION ( 'NONE',  ( 0.000000000000000000, 0.7278708115913771204, 0.6857142857147648929 ) ) ;
#52041 = FACE_OUTER_BOUND ( 'NONE', #35997, .T. ) ;
#52042 = VERTEX_POINT ( 'NONE', #46150 ) ;
#52043 = FACE_OUTER_BOUND ( 'NONE', #1484, .T. ) ;
#52044 = VECTOR ( 'NONE', #11448, 1000.000000000000000 ) ;
#52046 = ORIENTED_EDGE ( 'NONE', *, *, #10525, .F. ) ;
#52045 = LINE ( 'NONE', #19503, #29984 ) ;
#52047 = CARTESIAN_POINT ( 'NONE',  ( 27.90000000000000213, -0.2000000000089119934, 8.909539772616881237E-12 ) ) ;
#52048 = DIRECTION ( 'NONE',  ( 1.000000000000000000, -0.000000000000000000, 0.000000000000000000 ) ) ;
#52049 = DIRECTION ( 'NONE',  ( 1.836970198721029934E-16, 1.836970198721010706E-16, -1.000000000000000000 ) ) ;
#52050 = VECTOR ( 'NONE', #20814, 1000.000000000000000 ) ;
#52051 = ORIENTED_EDGE ( 'NONE', *, *, #33978, .T. ) ;
#52052 = DIRECTION ( 'NONE',  ( 0.000000000000000000, 0.000000000000000000, 1.000000000000000000 ) ) ;
#52053 = CARTESIAN_POINT ( 'NONE',  ( 169.1780563256071446, -33.83962462487175316, 5.000000000000000000 ) ) ;
#52054 = VERTEX_POINT ( 'NONE', #36244 ) ;
#52055 = DIRECTION ( 'NONE',  ( -0.7071067811865475727, 0.7071067811865475727, 0.000000000000000000 ) ) ;
#52056 = LINE ( 'NONE', #30484, #48878 ) ;
#52057 = ORIENTED_EDGE ( 'NONE', *, *, #21265, .T. ) ;
#52058 = CYLINDRICAL_SURFACE ( 'NONE', #30483, 1.000000000000000000 ) ;
#52059 = ORIENTED_EDGE ( 'NONE', *, *, #4552, .T. ) ;
#52060 = ORIENTED_EDGE ( 'NONE', *, *, #43926, .F. ) ;
#52061 = DIRECTION ( 'NONE',  ( -1.000000000000000000, 0.000000000000000000, 0.000000000000000000 ) ) ;
#52062 = LINE ( 'NONE', #19526, #9411 ) ;
#52063 = DIRECTION ( 'NONE',  ( -1.000000000000000000, 0.000000000000000000, 0.000000000000000000 ) ) ;
#52064 = DIRECTION ( 'NONE',  ( 0.000000000000000000, 0.000000000000000000, 1.000000000000000000 ) ) ;
#52065 = DIRECTION ( 'NONE',  ( 0.000000000000000000, 0.000000000000000000, -1.000000000000000000 ) ) ;
#52066 = ORIENTED_EDGE ( 'NONE', *, *, #43846, .F. ) ;
#52067 = ORIENTED_EDGE ( 'NONE', *, *, #36789, .F. ) ;
#52068 = EDGE_CURVE ( 'NONE', #38301, #37330, #32006, .T. ) ;
#52070 = ORIENTED_EDGE ( 'NONE', *, *, #42007, .T. ) ;
#52069 = DIRECTION ( 'NONE',  ( 1.920885163218982051E-15, 1.000000000000000000, 1.836970198721033139E-16 ) ) ;
#52071 = ORIENTED_EDGE ( 'NONE', *, *, #13336, .T. ) ;
#52072 = VECTOR ( 'NONE', #48732, 1000.000000000000000 ) ;
#52073 = AXIS2_PLACEMENT_3D ( 'NONE', #39566, #49844, #1404 ) ;
#52074 = CARTESIAN_POINT ( 'NONE',  ( 7.450000000000003730, -7.249999999999997335, -19.00000000000000000 ) ) ;
#52075 = CARTESIAN_POINT ( 'NONE',  ( 7.250000000000005329, 8.250000000000001776, -26.00000000000001066 ) ) ;
#52076 = EDGE_CURVE ( 'NONE', #31863, #21068, #43141, .T. ) ;
#52077 = DIRECTION ( 'NONE',  ( -0.000000000000000000, 1.000000000000000000, -0.000000000000000000 ) ) ;
#52078 = LINE ( 'NONE', #57024, #358 ) ;
#52079 = AXIS2_PLACEMENT_3D ( 'NONE', #58932, #52948, #69191 ) ;
#52080 = CARTESIAN_POINT ( 'NONE',  ( 15.00000000000000000, -42.00000000000000000, -15.10000000000000142 ) ) ;
#52081 = PLANE ( 'NONE',  #3856 ) ;
#52082 = EDGE_LOOP ( 'NONE', ( #46352, #13293, #44341, #54949 ) ) ;
#52083 = ORIENTED_EDGE ( 'NONE', *, *, #27491, .F. ) ;
#52084 = ORIENTED_EDGE ( 'NONE', *, *, #57550, .F. ) ;
#52085 = VECTOR ( 'NONE', #40404, 1000.000000000000000 ) ;
#52086 = AXIS2_PLACEMENT_3D ( 'NONE', #59296, #11199, #59651 ) ;
#52087 = ORIENTED_EDGE ( 'NONE', *, *, #25832, .F. ) ;
#52088 = LINE ( 'NONE', #14603, #23155 ) ;
#52089 = LINE ( 'NONE', #20604, #69399 ) ;
#52090 = EDGE_CURVE ( 'NONE', #62485, #4332, #1352, .T. ) ;
#52091 = VECTOR ( 'NONE', #59123, 1000.000000000000000 ) ;
#52092 = LINE ( 'NONE', #13206, #52356 ) ;
#52093 = AXIS2_PLACEMENT_3D ( 'NONE', #7746, #67856, #50882 ) ;
#52094 = ORIENTED_EDGE ( 'NONE', *, *, #30879, .T. ) ;
#52095 = EDGE_LOOP ( 'NONE', ( #6427, #67271, #47994, #54942 ) ) ;
#52096 = ORIENTED_EDGE ( 'NONE', *, *, #46392, .T. ) ;
#52098 = FACE_OUTER_BOUND ( 'NONE', #66431, .T. ) ;
#52097 = CONICAL_SURFACE ( 'NONE', #21625, 1732.050807568789651, 1.047197551196575871 ) ;
#52099 = ORIENTED_EDGE ( 'NONE', *, *, #66524, .T. ) ;
#52100 = EDGE_LOOP ( 'NONE', ( #17988, #46975, #50793, #28686 ) ) ;
#52101 = FACE_OUTER_BOUND ( 'NONE', #51154, .T. ) ;
#52102 = ORIENTED_EDGE ( 'NONE', *, *, #20212, .T. ) ;
#52103 = ORIENTED_EDGE ( 'NONE', *, *, #51835, .F. ) ;
#52104 = CARTESIAN_POINT ( 'NONE',  ( 7.000000000000000000, -25.60000000000000142, 15.10000000000000142 ) ) ;
#52106 = VERTEX_POINT ( 'NONE', #14681 ) ;
#52105 = CARTESIAN_POINT ( 'NONE',  ( 36.90000000000000568, 13.66939075806899950, 20.80000000000000426 ) ) ;
#52107 = ORIENTED_EDGE ( 'NONE', *, *, #44140, .F. ) ;
#52108 = LINE ( 'NONE', #57406, #1866 ) ;
#52109 = PLANE ( 'NONE',  #60016 ) ;
#52110 = CIRCLE ( 'NONE', #57761, 1.000000000000000000 ) ;
#52111 = CARTESIAN_POINT ( 'NONE',  ( 31.89999999999999858, -21.00000000000000000, 13.86939075806900057 ) ) ;
#52113 = ORIENTED_EDGE ( 'NONE', *, *, #53056, .T. ) ;
#52112 = PLANE ( 'NONE',  #68461 ) ;
#52114 = ORIENTED_EDGE ( 'NONE', *, *, #31150, .F. ) ;
#52115 = CYLINDRICAL_SURFACE ( 'NONE', #20831, 0.7112000000000124889 ) ;
#52116 = DIRECTION ( 'NONE',  ( 1.000000000000000000, 0.000000000000000000, 0.000000000000000000 ) ) ;
#52117 = CARTESIAN_POINT ( 'NONE',  ( 7.000000000000000000, -26.50000000000000000, 5.809475019311129529 ) ) ;
#52118 = EDGE_CURVE ( 'NONE', #16302, #37166, #3725, .T. ) ;
#52119 = DIRECTION ( 'NONE',  ( 1.836970198721029934E-16, 1.836970198721010706E-16, -1.000000000000000000 ) ) ;
#52120 = AXIS2_PLACEMENT_3D ( 'NONE', #48912, #5080, #59859 ) ;
#52121 = EDGE_LOOP ( 'NONE', ( #1317, #24736, #29915, #46322 ) ) ;
#52122 = DIRECTION ( 'NONE',  ( -1.000000000000000000, 0.000000000000000000, 0.000000000000000000 ) ) ;
#52123 = CYLINDRICAL_SURFACE ( 'NONE', #1556, 1.399999999999999245 ) ;
#52124 =( GEOMETRIC_REPRESENTATION_CONTEXT ( 3 ) GLOBAL_UNCERTAINTY_ASSIGNED_CONTEXT ( ( #57832 ) ) GLOBAL_UNIT_ASSIGNED_CONTEXT ( ( #8524, #67937, #64052 ) ) REPRESENTATION_CONTEXT ( 'NONE', 'WORKASPACE' ) );
#52125 = PLANE ( 'NONE',  #18791 ) ;
#52126 = ORIENTED_EDGE ( 'NONE', *, *, #14971, .F. ) ;
#52127 = DIRECTION ( 'NONE',  ( -0.000000000000000000, 3.673940397442059868E-16, -1.000000000000000000 ) ) ;
#52128 = CARTESIAN_POINT ( 'NONE',  ( -11.99351654964679526, -7.826483450353362237, 455.0000000000000568 ) ) ;
#52129 = EDGE_CURVE ( 'NONE', #902, #68930, #47639, .T. ) ;
#52130 = DIRECTION ( 'NONE',  ( -0.000000000000000000, -0.000000000000000000, -1.000000000000000000 ) ) ;
#52131 = CLOSED_SHELL ( 'NONE', ( #69926, #23140, #36098, #43867, #23690, #55191, #4235, #60772, #32034, #14666, #13547, #21167, #55976, #772 ) ) ;
#52132 = EDGE_LOOP ( 'NONE', ( #65763, #28939, #6034, #19995 ) ) ;
#52133 = EDGE_CURVE ( 'NONE', #38076, #67332, #26005, .T. ) ;
#52134 = LINE ( 'NONE', #4754, #56194 ) ;
#52135 = LINE ( 'NONE', #19598, #625 ) ;
#52136 = VECTOR ( 'NONE', #45979, 1000.000000000000000 ) ;
#52137 = DIRECTION ( 'NONE',  ( 0.000000000000000000, 0.000000000000000000, 1.000000000000000000 ) ) ;
#52138 = EDGE_LOOP ( 'NONE', ( #40895, #40183, #17270, #3666, #8166, #61971, #65071, #22669 ) ) ;
#52139 = DIRECTION ( 'NONE',  ( 8.659560562354951347E-17, -0.7071067811865460184, 0.7071067811865489050 ) ) ;
#52140 = CARTESIAN_POINT ( 'NONE',  ( -9.234937905884127218, -9.955011587777249815, 455.0000000000000568 ) ) ;
#52141 = CARTESIAN_POINT ( 'NONE',  ( 27.00000000000000000, 0.000000000000000000, 0.000000000000000000 ) ) ;
#52142 = VECTOR ( 'NONE', #15966, 1000.000000000000000 ) ;
#52143 = LINE ( 'NONE', #13954, #12033 ) ;
#52144 = FACE_OUTER_BOUND ( 'NONE', #45052, .T. ) ;
#52145 = EDGE_LOOP ( 'NONE', ( #1078, #29146, #18048, #14766 ) ) ;
#52146 = DIRECTION ( 'NONE',  ( -1.000000000000000000, 0.000000000000000000, 0.000000000000000000 ) ) ;
#52147 = DIRECTION ( 'NONE',  ( -0.6414496315691617934, 0.7671651518152962090, 0.000000000000000000 ) ) ;
#52148 = CARTESIAN_POINT ( 'NONE',  ( 30.00000000000000000, -17.00000000000000000, -15.70499999999969809 ) ) ;
#52149 = CARTESIAN_POINT ( 'NONE',  ( -8.566576262117260754, 8.916576262117214213, 54.00000000000000711 ) ) ;
#52150 = DIRECTION ( 'NONE',  ( 1.000000000000000000, 0.000000000000000000, 0.000000000000000000 ) ) ;
#52151 = ORIENTED_EDGE ( 'NONE', *, *, #9777, .T. ) ;
#52153 = ORIENTED_EDGE ( 'NONE', *, *, #60821, .T. ) ;
#52152 = CARTESIAN_POINT ( 'NONE',  ( 29.50000000000000355, -15.46862696659690073, 14.50000000000000000 ) ) ;
#52154 = EDGE_CURVE ( 'NONE', #32932, #31078, #21385, .T. ) ;
#52155 = CARTESIAN_POINT ( 'NONE',  ( -3.663616288757085560, -4.149127210878725158, 26.00000000000000711 ) ) ;
#52156 = VECTOR ( 'NONE', #7211, 1000.000000000000000 ) ;
#52157 = EDGE_CURVE ( 'NONE', #12808, #938, #41555, .T. ) ;
#52158 = CYLINDRICAL_SURFACE ( 'NONE', #46967, 5.000000000000004441 ) ;
#52159 = CARTESIAN_POINT ( 'NONE',  ( 41.09999999999999432, -14.48845687959340012, 21.00000000000000000 ) ) ;
#52160 = ORIENTED_EDGE ( 'NONE', *, *, #4505, .T. ) ;
#52161 = EDGE_CURVE ( 'NONE', #26006, #36409, #53235, .T. ) ;
#52162 = DIRECTION ( 'NONE',  ( 0.000000000000000000, -0.7051282051282052876, -0.7090798363602477394 ) ) ;
#52163 = EDGE_CURVE ( 'NONE', #3626, #38637, #42947, .T. ) ;
#52164 = VERTEX_POINT ( 'NONE', #4443 ) ;
#52165 = EDGE_LOOP ( 'NONE', ( #64618, #8562, #37617, #17786 ) ) ;
#52166 = EDGE_CURVE ( 'NONE', #44324, #3209, #68426, .T. ) ;
#52167 = EDGE_LOOP ( 'NONE', ( #12661, #9680, #60817, #31170 ) ) ;
#52168 = ORIENTED_EDGE ( 'NONE', *, *, #9939, .T. ) ;
#52170 = EDGE_CURVE ( 'NONE', #2772, #37989, #4086, .T. ) ;
#52169 = DIRECTION ( 'NONE',  ( 0.000000000000000000, 0.000000000000000000, -1.000000000000000000 ) ) ;
#52171 = LINE ( 'NONE', #19997, #29761 ) ;
#52172 = EDGE_CURVE ( 'NONE', #2958, #5311, #64191, .T. ) ;
#52173 = CARTESIAN_POINT ( 'NONE',  ( 37.90000000000000568, -0.1999999999911795112, 8.826273045769999343E-12 ) ) ;
#52174 = DIRECTION ( 'NONE',  ( -0.000000000000000000, -0.000000000000000000, -1.000000000000000000 ) ) ;
#52175 = ORIENTED_EDGE ( 'NONE', *, *, #37663, .T. ) ;
#52176 = ORIENTED_EDGE ( 'NONE', *, *, #985, .F. ) ;
#52177 = PLANE ( 'NONE',  #30126 ) ;
#52178 = CARTESIAN_POINT ( 'NONE',  ( -25.50000000000000355, -5.200000000000001066, -24.75000000000000000 ) ) ;
#52179 = ORIENTED_EDGE ( 'NONE', *, *, #28049, .T. ) ;
#52180 = VERTEX_POINT ( 'NONE', #9019 ) ;
#52181 = VERTEX_POINT ( 'NONE', #4781 ) ;
#52182 = ORIENTED_EDGE ( 'NONE', *, *, #61714, .T. ) ;
#52183 = DIRECTION ( 'NONE',  ( -1.000000000000000000, 0.000000000000000000, 0.000000000000000000 ) ) ;
#52185 = ORIENTED_EDGE ( 'NONE', *, *, #25409, .T. ) ;
#52184 = DIRECTION ( 'NONE',  ( -1.836970198721029934E-16, 1.836970198721036344E-16, -1.000000000000000000 ) ) ;
#52186 = CIRCLE ( 'NONE', #31760, 0.1749999999999993783 ) ;
#52187 = LINE ( 'NONE', #9052, #66170 ) ;
#52188 = LINE ( 'NONE', #47933, #41910 ) ;
#52189 = EDGE_CURVE ( 'NONE', #45523, #13089, #53358, .T. ) ;
#52190 = ORIENTED_EDGE ( 'NONE', *, *, #11666, .F. ) ;
#52191 = ORIENTED_EDGE ( 'NONE', *, *, #47434, .T. ) ;
#52192 = AXIS2_PLACEMENT_3D ( 'NONE', #15879, #48404, #69633 ) ;
#52193 = EDGE_CURVE ( 'NONE', #22396, #12404, #47562, .T. ) ;
#52194 = CARTESIAN_POINT ( 'NONE',  ( 9.841277389592722358, -2.290483450353490547, 455.0000000000000568 ) ) ;
#52195 = CARTESIAN_POINT ( 'NONE',  ( -7.250000000000000888, 7.250000000000001776, -18.50000000000000000 ) ) ;
#52196 = ORIENTED_EDGE ( 'NONE', *, *, #18524, .T. ) ;
#52197 = DIRECTION ( 'NONE',  ( 0.000000000000000000, -1.000000000000000000, 0.000000000000000000 ) ) ;
#52198 = CARTESIAN_POINT ( 'NONE',  ( -6.749999999999998224, -7.348062532927999158, 5.000000000000000000 ) ) ;
#52199 = DIRECTION ( 'NONE',  ( 1.000000000000000000, 0.000000000000000000, 0.000000000000000000 ) ) ;
#52200 = ORIENTED_EDGE ( 'NONE', *, *, #56244, .T. ) ;
#52201 = CARTESIAN_POINT ( 'NONE',  ( 83.97321854994621049, 47.95351654967443977, 20.00000000000000000 ) ) ;
#52202 = CARTESIAN_POINT ( 'NONE',  ( 8.250000000000005329, -8.249999999999998224, -26.00000000000001066 ) ) ;
#52203 = CARTESIAN_POINT ( 'NONE',  ( 7.000000000000000000, -41.99999999999906208, -14.49999999999903899 ) ) ;
#52204 = DIRECTION ( 'NONE',  ( -1.000000000000000000, 0.000000000000000000, 0.000000000000000000 ) ) ;
#52205 = AXIS2_PLACEMENT_3D ( 'NONE', #63179, #20396, #14402 ) ;
#52206 = ADVANCED_FACE ( 'NONE', ( #19991 ), #52521, .F. ) ;
#52207 = LINE ( 'NONE', #63532, #8271 ) ;
#52208 = ORIENTED_EDGE ( 'NONE', *, *, #62429, .T. ) ;
#52209 = DIRECTION ( 'NONE',  ( -1.000000000000000000, 0.000000000000000000, 0.000000000000000000 ) ) ;
#52210 = LINE ( 'NONE', #10133, #29399 ) ;
#52211 = AXIS2_PLACEMENT_3D ( 'NONE', #48733, #42727, #37435 ) ;
#52212 = PRESENTATION_STYLE_ASSIGNMENT (( #35228 ) ) ;
#52213 = DIRECTION ( 'NONE',  ( -1.000000000000000000, 0.000000000000000000, 0.000000000000000000 ) ) ;
#52214 = CARTESIAN_POINT ( 'NONE',  ( 7.250000000000005329, 7.250000000000000888, -8.500000000000000000 ) ) ;
#52215 = ADVANCED_FACE ( 'NONE', ( #20337 ), #41901, .T. ) ;
#52216 = CARTESIAN_POINT ( 'NONE',  ( 8.612468434717182930, 1.466476262117163865, 54.00000000000000711 ) ) ;
#52217 = EDGE_CURVE ( 'NONE', #11146, #56487, #42247, .T. ) ;
#52218 = DIRECTION ( 'NONE',  ( -1.794541526872559352E-16, -1.000000000000000000, 0.000000000000000000 ) ) ;
#52219 = CARTESIAN_POINT ( 'NONE',  ( -7.450000000000001954, 0.000000000000000000, -12.00000000000000000 ) ) ;
#52220 = ORIENTED_EDGE ( 'NONE', *, *, #56678, .T. ) ;
#52221 = DIRECTION ( 'NONE',  ( -0.000000000000000000, -0.000000000000000000, -1.000000000000000000 ) ) ;
#52222 = CARTESIAN_POINT ( 'NONE',  ( -10.08346604330788665, -2.906483450353353426, 455.0000000000000568 ) ) ;
#52223 = EDGE_CURVE ( 'NONE', #31671, #67553, #36972, .T. ) ;
#52224 = ORIENTED_EDGE ( 'NONE', *, *, #15383, .T. ) ;
#52225 = LINE ( 'NONE', #35596, #66225 ) ;
#52227 = EDGE_CURVE ( 'NONE', #12509, #63544, #7036, .T. ) ;
#52226 = VECTOR ( 'NONE', #30161, 1000.000000000000114 ) ;
#52228 = EDGE_CURVE ( 'NONE', #5488, #50027, #44319, .T. ) ;
#52229 = CARTESIAN_POINT ( 'NONE',  ( -10.30047626211725742, 3.842976262117182351, 54.00000000000000711 ) ) ;
#52230 = DIRECTION ( 'NONE',  ( -1.000000000000000000, 0.000000000000000000, 0.000000000000000000 ) ) ;
#52231 = DIRECTION ( 'NONE',  ( -0.6414496315691494699, -0.7671651518153064231, -0.000000000000000000 ) ) ;
#52232 = CYLINDRICAL_SURFACE ( 'NONE', #22662, 0.1999999999999996503 ) ;
#52233 = ORIENTED_EDGE ( 'NONE', *, *, #40847, .T. ) ;
#52234 = ADVANCED_FACE ( 'NONE', ( #11458 ), #11119, .F. ) ;
#52235 = DIRECTION ( 'NONE',  ( 0.4999999999999695799, -0.8660254037844563602, -6.723777587269172655E-17 ) ) ;
#52236 = CIRCLE ( 'NONE', #26303, 1.620999999999997332 ) ;
#52237 = VERTEX_POINT ( 'NONE', #54965 ) ;
#52238 = PLANE ( 'NONE',  #31601 ) ;
#52239 = EDGE_CURVE ( 'NONE', #67654, #47832, #32688, .T. ) ;
#52240 = CARTESIAN_POINT ( 'NONE',  ( -15.50000000000000000, -0.2038245569916614930, 23.94337567297399971 ) ) ;
#52241 = VERTEX_POINT ( 'NONE', #44663 ) ;
#52242 = CARTESIAN_POINT ( 'NONE',  ( -17.51999999999999957, -15.50000000000000000, 26.00000000000000355 ) ) ;
#52243 = EDGE_CURVE ( 'NONE', #520, #22636, #6524, .T. ) ;
#52244 = CIRCLE ( 'NONE', #61246, 0.3499999999998875677 ) ;
#52245 = AXIS2_PLACEMENT_3D ( 'NONE', #14529, #41398, #31509 ) ;
#52246 = CARTESIAN_POINT ( 'NONE',  ( -8.198316549646774476, -6.006483450353403697, 455.0000000000000568 ) ) ;
#52247 = ORIENTED_EDGE ( 'NONE', *, *, #2364, .F. ) ;
#52248 = CARTESIAN_POINT ( 'NONE',  ( -4.609516549646713202, 3.593516549646603941, 195.0000000000000284 ) ) ;
#52249 = VERTEX_POINT ( 'NONE', #38347 ) ;
#52250 = CIRCLE ( 'NONE', #21766, 1.399999999999998579 ) ;
#52251 = ORIENTED_EDGE ( 'NONE', *, *, #4596, .F. ) ;
#52253 = EDGE_CURVE ( 'NONE', #58636, #54732, #5827, .T. ) ;
#52252 = LINE ( 'NONE', #63205, #14792 ) ;
#52254 = ORIENTED_EDGE ( 'NONE', *, *, #19014, .F. ) ;
#52255 = VERTEX_POINT ( 'NONE', #1211 ) ;
#52256 = EDGE_CURVE ( 'NONE', #29308, #36191, #32347, .T. ) ;
#52257 = DIRECTION ( 'NONE',  ( -0.000000000000000000, -0.000000000000000000, -1.000000000000000000 ) ) ;
#52258 = DIRECTION ( 'NONE',  ( 1.000000000000000000, -3.491481338843133750E-15, -1.836970198721036590E-16 ) ) ;
#52259 = DIRECTION ( 'NONE',  ( -1.000000000000000000, 0.000000000000000000, 0.000000000000000000 ) ) ;
#52260 = VERTEX_POINT ( 'NONE', #17812 ) ;
#52261 = LINE ( 'NONE', #47650, #23307 ) ;
#52263 = DIRECTION ( 'NONE',  ( 0.5773502691896257311, -0.5773502691896257311, -0.5773502691896257311 ) ) ;
#52262 = PLANE ( 'NONE',  #55282 ) ;
#52264 = VERTEX_POINT ( 'NONE', #53927 ) ;
#52266 = ORIENTED_EDGE ( 'NONE', *, *, #11155, .F. ) ;
#52265 = DIRECTION ( 'NONE',  ( -0.000000000000000000, -0.000000000000000000, -1.000000000000000000 ) ) ;
#52267 = EDGE_CURVE ( 'NONE', #19060, #49394, #10767, .T. ) ;
#52268 = ORIENTED_EDGE ( 'NONE', *, *, #59334, .F. ) ;
#52269 = APPLICATION_PROTOCOL_DEFINITION ( 'draft international standard', 'automotive_design', 1998, #11498 ) ;
#52270 = LINE ( 'NONE', #46955, #36751 ) ;
#52272 = EDGE_LOOP ( 'NONE', ( #66718, #28228, #2954, #53265 ) ) ;
#52271 = CARTESIAN_POINT ( 'NONE',  ( 16.75000000000000000, -0.3156864504677172611, -22.25638000318208398 ) ) ;
#52273 = CARTESIAN_POINT ( 'NONE',  ( -15.50000000000000000, -15.50000000000000000, -22.50000000000000000 ) ) ;
#52274 = CARTESIAN_POINT ( 'NONE',  ( 8.465062094116072799, 4.242044687070411157, 455.0000000000000568 ) ) ;
#52275 = ORIENTED_EDGE ( 'NONE', *, *, #28786, .T. ) ;
#52276 = ORIENTED_EDGE ( 'NONE', *, *, #8153, .T. ) ;
#52277 = AXIS2_PLACEMENT_3D ( 'NONE', #4280, #9221, #52723 ) ;
#52278 = CARTESIAN_POINT ( 'NONE',  ( 24.90000000000000213, -21.00000000000000000, 13.86939075806900057 ) ) ;
#52279 = ORIENTED_EDGE ( 'NONE', *, *, #11910, .F. ) ;
#52280 = EDGE_CURVE ( 'NONE', #57776, #62704, #47691, .T. ) ;
#52281 = LINE ( 'NONE', #48025, #35813 ) ;
#52282 = CARTESIAN_POINT ( 'NONE',  ( 8.711985858128681315, 8.079219948824839292, 26.00000000000000711 ) ) ;
#52283 = CARTESIAN_POINT ( 'NONE',  ( 1.866219381641484931, 9.404046420174006826, 455.0000000000000568 ) ) ;
#52284 = ORIENTED_EDGE ( 'NONE', *, *, #59186, .F. ) ;
#52285 = ADVANCED_FACE ( 'NONE', ( #27040 ), #6837, .F. ) ;
#52286 = AXIS2_PLACEMENT_3D ( 'NONE', #11711, #34308, #38939 ) ;
#52287 = DIRECTION ( 'NONE',  ( -0.000000000000000000, 3.673940397442059868E-16, -1.000000000000000000 ) ) ;
#52288 = CARTESIAN_POINT ( 'NONE',  ( 282.7711612342632179, -25.38939884375893641, -17.11060115624107425 ) ) ;
#52290 = ORIENTED_EDGE ( 'NONE', *, *, #39740, .F. ) ;
#52289 = CARTESIAN_POINT ( 'NONE',  ( 17.89999999999999858, 20.60000000000000142, -13.86939075806900057 ) ) ;
#52292 = EDGE_LOOP ( 'NONE', ( #16319, #33780, #57786, #53411 ) ) ;
#52291 = DIRECTION ( 'NONE',  ( 0.000000000000000000, 0.6857142857146703019, 0.7278708115914659382 ) ) ;
#52293 = EDGE_CURVE ( 'NONE', #6695, #4279, #14044, .T. ) ;
#52295 = DIRECTION ( 'NONE',  ( 0.000000000000000000, 0.000000000000000000, -1.000000000000000000 ) ) ;
#52294 = AXIS2_PLACEMENT_3D ( 'NONE', #55189, #44556, #11688 ) ;
#52296 = VECTOR ( 'NONE', #38499, 1000.000000000000000 ) ;
#52297 = DIRECTION ( 'NONE',  ( 0.000000000000000000, 0.000000000000000000, 1.000000000000000000 ) ) ;
#52298 = EDGE_CURVE ( 'NONE', #7002, #29126, #21732, .T. ) ;
#52299 = CARTESIAN_POINT ( 'NONE',  ( -11.99351654964683078, -11.19368345035334933, 455.0000000000000568 ) ) ;
#52300 = CARTESIAN_POINT ( 'NONE',  ( 283.0000000000000568, -25.50000000000000355, 17.00000000000000000 ) ) ;
#52301 = VECTOR ( 'NONE', #24991, 1000.000000000000000 ) ;
#52302 = EDGE_CURVE ( 'NONE', #57627, #65232, #64874, .T. ) ;
#52303 = DIRECTION ( 'NONE',  ( 2.891205793294683355E-15, 1.000000000000000000, 0.000000000000000000 ) ) ;
#52304 = VERTEX_POINT ( 'NONE', #16779 ) ;
#52305 = LINE ( 'NONE', #63263, #7542 ) ;
#52306 = DIRECTION ( 'NONE',  ( 0.000000000000000000, 1.000000000000000000, 0.000000000000000000 ) ) ;
#52307 = CARTESIAN_POINT ( 'NONE',  ( -6.642976262117260333, 10.30047626211718104, 26.00000000000000711 ) ) ;
#52309 = ORIENTED_EDGE ( 'NONE', *, *, #1572, .T. ) ;
#52308 = DIRECTION ( 'NONE',  ( 0.000000000000000000, 1.000000000000000000, 0.000000000000000000 ) ) ;
#52310 = DIRECTION ( 'NONE',  ( -1.000000000000000000, 0.000000000000000000, -0.000000000000000000 ) ) ;
#52311 = CIRCLE ( 'NONE', #22922, 0.2000000000000005107 ) ;
#52312 = LINE ( 'NONE', #57262, #65720 ) ;
#52313 = EDGE_CURVE ( 'NONE', #22714, #31391, #16433, .T. ) ;
#52314 = DIRECTION ( 'NONE',  ( -0.000000000000000000, -0.000000000000000000, -1.000000000000000000 ) ) ;
#52315 = ORIENTED_EDGE ( 'NONE', *, *, #63066, .T. ) ;
#52316 = DIRECTION ( 'NONE',  ( -0.000000000000000000, 3.673940397442059868E-16, -1.000000000000000000 ) ) ;
#52317 = CYLINDRICAL_SURFACE ( 'NONE', #3475, 0.3999999999999993006 ) ;
#52318 = CIRCLE ( 'NONE', #63633, 3.233000000000000096 ) ;
#52319 = ORIENTED_EDGE ( 'NONE', *, *, #42887, .T. ) ;
#52320 = DIRECTION ( 'NONE',  ( 1.000000000000000000, -0.000000000000000000, 0.000000000000000000 ) ) ;
#52321 = ADVANCED_FACE ( 'NONE', ( #49312 ), #6163, .T. ) ;
#52322 = DIRECTION ( 'NONE',  ( -1.000000000000000000, 0.000000000000000000, 0.000000000000000000 ) ) ;
#52323 = DIRECTION ( 'NONE',  ( 0.000000000000000000, -0.7057491738665943037, -0.7084617869628675457 ) ) ;
#52324 = AXIS2_PLACEMENT_3D ( 'NONE', #51073, #58417, #47433 ) ;
#52325 = CARTESIAN_POINT ( 'NONE',  ( 30.00000000000000000, -17.35230188589299871, 15.35019951917099945 ) ) ;
#52326 = EDGE_CURVE ( 'NONE', #67578, #5297, #60242, .T. ) ;
#52327 = PLANE ( 'NONE',  #20691 ) ;
#52328 = ORIENTED_EDGE ( 'NONE', *, *, #9846, .F. ) ;
#52329 = PLANE ( 'NONE',  #52961 ) ;
#52330 = ORIENTED_EDGE ( 'NONE', *, *, #16945, .F. ) ;
#52331 = CARTESIAN_POINT ( 'NONE',  ( 30.00000000000000000, -11.85423089348099879, 9.852125413066602277 ) ) ;
#52332 = ORIENTED_EDGE ( 'NONE', *, *, #32966, .F. ) ;
#52333 = ORIENTED_EDGE ( 'NONE', *, *, #21558, .T. ) ;
#52334 = CARTESIAN_POINT ( 'NONE',  ( 3.724485858128677940, -7.408280051175165859, 54.00000000000000711 ) ) ;
#52335 = DIRECTION ( 'NONE',  ( 0.000000000000000000, 0.7071067811865474617, -0.7071067811865474617 ) ) ;
#52336 = FACE_OUTER_BOUND ( 'NONE', #54192, .T. ) ;
#52337 = ORIENTED_EDGE ( 'NONE', *, *, #51092, .T. ) ;
#52338 = ORIENTED_EDGE ( 'NONE', *, *, #39572, .F. ) ;
#52340 = ADVANCED_FACE ( 'NONE', ( #45015 ), #34052, .T. ) ;
#52339 = DIRECTION ( 'NONE',  ( 1.000000000000000000, 0.000000000000000000, 0.000000000000000000 ) ) ;
#52341 = ORIENTED_EDGE ( 'NONE', *, *, #43353, .F. ) ;
#52342 = ORIENTED_EDGE ( 'NONE', *, *, #37897, .T. ) ;
#52343 = ADVANCED_FACE ( 'NONE', ( #12827 ), #34392, .F. ) ;
#52344 = DIRECTION ( 'NONE',  ( 1.000000000000000000, -0.000000000000000000, 0.000000000000000000 ) ) ;
#52345 = CARTESIAN_POINT ( 'NONE',  ( 33.89999999999999858, -0.2000000000089119934, -8.913009219568841313E-12 ) ) ;
#52346 = CIRCLE ( 'NONE', #25238, 0.1999999999999987899 ) ;
#52347 = AXIS2_PLACEMENT_3D ( 'NONE', #44750, #19289, #66679 ) ;
#52348 = CARTESIAN_POINT ( 'NONE',  ( -15.50000000000000000, -0.2038245569916614930, -21.05662432702600029 ) ) ;
#52349 = LINE ( 'NONE', #42687, #67012 ) ;
#52350 = VERTEX_POINT ( 'NONE', #39370 ) ;
#52351 = CIRCLE ( 'NONE', #48974, 1.000000000000000000 ) ;
#52352 = DIRECTION ( 'NONE',  ( 1.000000000000000000, -0.000000000000000000, 0.000000000000000000 ) ) ;
#52354 = DIRECTION ( 'NONE',  ( 1.000000000000000000, -0.000000000000000000, -0.000000000000000000 ) ) ;
#52353 = CARTESIAN_POINT ( 'NONE',  ( 25.50000000000000355, -15.50000000000000000, 24.50000000000000000 ) ) ;
#52355 = CIRCLE ( 'NONE', #56815, 1.000000000000000000 ) ;
#52357 = EDGE_LOOP ( 'NONE', ( #66923, #16422, #8123, #12295 ) ) ;
#52356 = VECTOR ( 'NONE', #8241, 1000.000000000000000 ) ;
#52359 = ORIENTED_EDGE ( 'NONE', *, *, #2569, .T. ) ;
#52358 = LINE ( 'NONE', #20520, #28533 ) ;
#52360 = VERTEX_POINT ( 'NONE', #7538 ) ;
#52361 = AXIS2_PLACEMENT_3D ( 'NONE', #28530, #29217, #50792 ) ;
#52362 = AXIS2_PLACEMENT_3D ( 'NONE', #32630, #59146, #6100 ) ;
#52363 = LINE ( 'NONE', #35372, #19710 ) ;
#52364 = CYLINDRICAL_SURFACE ( 'NONE', #46244, 2.000000000000000000 ) ;
#52365 = ORIENTED_EDGE ( 'NONE', *, *, #51500, .F. ) ;
#52366 = ORIENTED_EDGE ( 'NONE', *, *, #28567, .F. ) ;
#52367 = DIRECTION ( 'NONE',  ( 1.000000000000000000, 0.000000000000000000, 0.000000000000000000 ) ) ;
#52368 = DIRECTION ( 'NONE',  ( 0.000000000000000000, 0.6857142857142869419, -0.7278708115918273158 ) ) ;
#52369 = VERTEX_POINT ( 'NONE', #23806 ) ;
#52370 = ORIENTED_EDGE ( 'NONE', *, *, #54589, .F. ) ;
#52371 = CARTESIAN_POINT ( 'NONE',  ( 55.00000000000000000, 0.000000000000000000, 0.000000000000000000 ) ) ;
#52372 = DIRECTION ( 'NONE',  ( 0.000000000000000000, 1.000000000000000000, 0.000000000000000000 ) ) ;
#52373 = ORIENTED_EDGE ( 'NONE', *, *, #52298, .F. ) ;
#52374 = EDGE_CURVE ( 'NONE', #58876, #1978, #29115, .T. ) ;
#52375 = CARTESIAN_POINT ( 'NONE',  ( 25.50000000000000355, 0.000000000000000000, -22.50000000000000000 ) ) ;
#52376 = DIRECTION ( 'NONE',  ( 1.000000000000000000, -2.309061475090597584E-14, 1.836970198720987533E-16 ) ) ;
#52378 = ORIENTED_EDGE ( 'NONE', *, *, #9558, .F. ) ;
#52377 = CARTESIAN_POINT ( 'NONE',  ( -9.942044687070568543, 2.752095193409294982, 195.0000000000000284 ) ) ;
#52379 = VERTEX_POINT ( 'NONE', #12489 ) ;
#52380 = EDGE_CURVE ( 'NONE', #45362, #35367, #56333, .T. ) ;
#52381 = PLANE ( 'NONE',  #23070 ) ;
#52382 = FACE_OUTER_BOUND ( 'NONE', #66727, .T. ) ;
#52383 = EDGE_CURVE ( 'NONE', #61211, #69660, #45361, .T. ) ;
#52384 = CARTESIAN_POINT ( 'NONE',  ( 7.616533956692213003, -8.406483450353491094, 455.0000000000000568 ) ) ;
#52385 = EDGE_CURVE ( 'NONE', #18784, #37577, #35448, .T. ) ;
#52386 = PLANE ( 'NONE',  #3032 ) ;
#52387 = DIRECTION ( 'NONE',  ( -0.000000000000000000, -0.000000000000000000, -1.000000000000000000 ) ) ;
#52388 = ADVANCED_FACE ( 'NONE', ( #35098 ), #1895, .F. ) ;
#52389 = EDGE_CURVE ( 'NONE', #43073, #39553, #18486, .T. ) ;
#52390 = CARTESIAN_POINT ( 'NONE',  ( 280.0000000000000000, -20.49999999999999645, -20.00000000000000000 ) ) ;
#52391 = EDGE_LOOP ( 'NONE', ( #33067, #11449, #54862, #63168 ) ) ;
#52392 = PLANE ( 'NONE',  #41678 ) ;
#52394 = ORIENTED_EDGE ( 'NONE', *, *, #28057, .T. ) ;
#52393 = LINE ( 'NONE', #9968, #61564 ) ;
#52395 = DIRECTION ( 'NONE',  ( 1.000000000000000000, 0.000000000000000000, 0.000000000000000000 ) ) ;
#52396 = VECTOR ( 'NONE', #3439, 1000.000000000000000 ) ;
#52397 = VECTOR ( 'NONE', #66596, 1000.000000000000000 ) ;
#52398 = DIRECTION ( 'NONE',  ( 0.000000000000000000, 0.000000000000000000, -1.000000000000000000 ) ) ;
#52399 = EDGE_CURVE ( 'NONE', #67569, #41197, #40770, .T. ) ;
#52400 = CARTESIAN_POINT ( 'NONE',  ( -7.250000000000001776, -7.249999999999998224, -22.00000000000000000 ) ) ;
#52401 = CIRCLE ( 'NONE', #61392, 1.000000000000001776 ) ;
#52402 = VECTOR ( 'NONE', #36373, 1000.000000000000000 ) ;
#52403 = ORIENTED_EDGE ( 'NONE', *, *, #50121, .T. ) ;
#52404 = CARTESIAN_POINT ( 'NONE',  ( -16.75000000000000000, -0.2038245569916330158, 23.22168783648699986 ) ) ;
#52405 = DIRECTION ( 'NONE',  ( -1.000000000000000000, 0.000000000000000000, 0.000000000000000000 ) ) ;
#52406 = EDGE_LOOP ( 'NONE', ( #53039, #13260, #21239, #7190, #3822, #40080, #1711, #16626, #14458, #2214, #14127, #17730, #29658, #15920, #60852, #68372, #36515 ) ) ;
#52407 = DIRECTION ( 'NONE',  ( 0.000000000000000000, 0.000000000000000000, -1.000000000000000000 ) ) ;
#52408 = VECTOR ( 'NONE', #15863, 1000.000000000000000 ) ;
#52409 = VECTOR ( 'NONE', #9292, 1000.000000000000000 ) ;
#52410 = DIRECTION ( 'NONE',  ( -0.7071067811865474617, -0.7071067811865474617, 0.000000000000000000 ) ) ;
#52411 = AXIS2_PLACEMENT_3D ( 'NONE', #40021, #23780, #45333 ) ;
#52412 = FACE_OUTER_BOUND ( 'NONE', #37963, .T. ) ;
#52413 = ORIENTED_EDGE ( 'NONE', *, *, #9447, .F. ) ;
#52414 = CARTESIAN_POINT ( 'NONE',  ( 275.2500000000000000, -0.2499999999999893141, -26.74999999999999645 ) ) ;
#52415 = VERTEX_POINT ( 'NONE', #57027 ) ;
#52416 = ORIENTED_EDGE ( 'NONE', *, *, #13074, .F. ) ;
#52417 = VECTOR ( 'NONE', #21654, 1000.000000000000000 ) ;
#52418 = LINE ( 'NONE', #25549, #39248 ) ;
#52419 = DIRECTION ( 'NONE',  ( -1.000000000000000000, 0.000000000000000000, 0.000000000000000000 ) ) ;
#52420 = CARTESIAN_POINT ( 'NONE',  ( -6.350872789121319251, -3.677663764522589140, 54.00000000000000711 ) ) ;
#52421 = B_SPLINE_CURVE_WITH_KNOTS ( 'NONE', 3,
 ( #45025, #49983, #1546, #39377 ),
 .UNSPECIFIED., .F., .F.,
 ( 4, 4 ),
 ( 4.336808689942017736E-19, 0.002138888851505100618 ),
 .UNSPECIFIED. ) ;
#52422 = LINE ( 'NONE', #3981, #69357 ) ;
#52423 = DIRECTION ( 'NONE',  ( -0.000000000000000000, 3.673940397442059868E-16, -1.000000000000000000 ) ) ;
#52424 = ORIENTED_EDGE ( 'NONE', *, *, #57271, .F. ) ;
#52425 = ORIENTED_EDGE ( 'NONE', *, *, #61442, .F. ) ;
#52427 = ORIENTED_EDGE ( 'NONE', *, *, #56139, .T. ) ;
#52426 = CARTESIAN_POINT ( 'NONE',  ( 7.250000000000005329, -7.249999999999998224, -17.00000000000000000 ) ) ;
#52428 = ORIENTED_EDGE ( 'NONE', *, *, #852, .T. ) ;
#52429 = EDGE_CURVE ( 'NONE', #33919, #46313, #2238, .T. ) ;
#52430 = CARTESIAN_POINT ( 'NONE',  ( 11.00000000000000000, -16.64230188589299786, -14.64519951917100116 ) ) ;
#52431 = DIRECTION ( 'NONE',  ( 0.000000000000000000, 1.000000000000000000, 0.000000000000000000 ) ) ;
#52432 = CARTESIAN_POINT ( 'NONE',  ( 4.740315990920131561, -4.201500623656049704, 195.0000000000000284 ) ) ;
#52433 = CARTESIAN_POINT ( 'NONE',  ( -7.450000000000001954, 7.250000000000000000, -21.50000000000000000 ) ) ;
#52434 = CIRCLE ( 'NONE', #67094, 0.5000000000009459100 ) ;
#52435 = EDGE_CURVE ( 'NONE', #27762, #60691, #18146, .T. ) ;
#52436 = DIRECTION ( 'NONE',  ( 3.596772705736696467E-15, 1.000000000000000000, 0.000000000000000000 ) ) ;
#52438 = DIRECTION ( 'NONE',  ( 1.000000000000000000, 0.000000000000000000, 0.000000000000000000 ) ) ;
#52437 = CARTESIAN_POINT ( 'NONE',  ( 30.00000000000000000, -11.50000000000000000, 15.00000000000000000 ) ) ;
#52439 = VERTEX_POINT ( 'NONE', #3289 ) ;
#52440 = CIRCLE ( 'NONE', #43387, 4.500000000000190958 ) ;
#52441 = ORIENTED_EDGE ( 'NONE', *, *, #41043, .F. ) ;
#52442 = EDGE_CURVE ( 'NONE', #68520, #46672, #40048, .T. ) ;
#52443 = ORIENTED_EDGE ( 'NONE', *, *, #21024, .T. ) ;
#52444 = EDGE_LOOP ( 'NONE', ( #21466, #63942, #13769, #59135 ) ) ;
#52445 = LINE ( 'NONE', #58088, #40105 ) ;
#52446 = DIRECTION ( 'NONE',  ( 0.000000000000000000, -1.000000000000000000, 0.000000000000000000 ) ) ;
#52448 = DIRECTION ( 'NONE',  ( -1.000000000000000000, 1.819560449471430698E-15, 1.836970198721033385E-16 ) ) ;
#52447 = AXIS2_PLACEMENT_3D ( 'NONE', #28683, #61192, #54890 ) ;
#52449 = EDGE_LOOP ( 'NONE', ( #68553, #29837, #21243, #8606 ) ) ;
#52450 = ORIENTED_EDGE ( 'NONE', *, *, #827, .T. ) ;
#52451 = ORIENTED_EDGE ( 'NONE', *, *, #63495, .T. ) ;
#52452 = DIRECTION ( 'NONE',  ( -0.000000000000000000, -0.000000000000000000, -1.000000000000000000 ) ) ;
#52453 = ORIENTED_EDGE ( 'NONE', *, *, #66985, .T. ) ;
#52454 = CIRCLE ( 'NONE', #16308, 0.4000000000000609179 ) ;
#52455 = CIRCLE ( 'NONE', #56918, 0.1999999999999987899 ) ;
#52456 = ORIENTED_EDGE ( 'NONE', *, *, #49690, .F. ) ;
#52457 = DIRECTION ( 'NONE',  ( 1.000000000000000000, 0.000000000000000000, 0.000000000000000000 ) ) ;
#52458 = ORIENTED_EDGE ( 'NONE', *, *, #47474, .T. ) ;
#52459 = VERTEX_POINT ( 'NONE', #46073 ) ;
#52460 = CARTESIAN_POINT ( 'NONE',  ( 2.706483450353343478, -10.92648345035346225, 455.0000000000000568 ) ) ;
#52461 = CIRCLE ( 'NONE', #65959, 4.500000000000190958 ) ;
#52463 = ORIENTED_EDGE ( 'NONE', *, *, #46255, .T. ) ;
#52462 = DIRECTION ( 'NONE',  ( -1.000000000000000000, 1.280238727658158235E-15, 0.000000000000000000 ) ) ;
#52464 = ORIENTED_EDGE ( 'NONE', *, *, #12640, .T. ) ;
#52465 = EDGE_CURVE ( 'NONE', #60150, #16696, #34758, .T. ) ;
#52466 = CARTESIAN_POINT ( 'NONE',  ( -11.00000000000000000, -11.50000000000100009, 15.00000000000084910 ) ) ;
#52467 = FACE_OUTER_BOUND ( 'NONE', #24678, .T. ) ;
#52469 = ORIENTED_EDGE ( 'NONE', *, *, #1793, .F. ) ;
#52468 = CARTESIAN_POINT ( 'NONE',  ( 7.250000000000005329, -7.449999999999998401, -19.50000000000000000 ) ) ;
#52470 = AXIS2_PLACEMENT_3D ( 'NONE', #26885, #44160, #5662 ) ;
#52471 = VERTEX_POINT ( 'NONE', #18849 ) ;
#52472 = CARTESIAN_POINT ( 'NONE',  ( 46.39999999999999858, 21.00000000000000000, -0.7500000000000000000 ) ) ;
#52473 = DIRECTION ( 'NONE',  ( 0.000000000000000000, 1.000000000000000000, 0.000000000000000000 ) ) ;
#52474 = DIRECTION ( 'NONE',  ( 0.000000000000000000, 0.000000000000000000, 1.000000000000000000 ) ) ;
#52475 = FACE_OUTER_BOUND ( 'NONE', #521, .T. ) ;
#52476 = ADVANCED_FACE ( 'NONE', ( #13893 ), #40422, .F. ) ;
#52477 = EDGE_CURVE ( 'NONE', #62314, #45394, #17422, .T. ) ;
#52478 = ORIENTED_EDGE ( 'NONE', *, *, #66181, .T. ) ;
#52479 = DIRECTION ( 'NONE',  ( -1.794541526872559352E-16, -1.000000000000000000, 0.000000000000000000 ) ) ;
#52480 = DIRECTION ( 'NONE',  ( -1.000000000000000000, 0.000000000000000000, 0.000000000000000000 ) ) ;
#52481 = FILL_AREA_STYLE ('',( #15350 ) ) ;
#52482 = EDGE_CURVE ( 'NONE', #27939, #10, #24512, .T. ) ;
#52483 = ORIENTED_EDGE ( 'NONE', *, *, #30341, .T. ) ;
#52484 = CIRCLE ( 'NONE', #14099, 4.500000000000191847 ) ;
#52485 = DIRECTION ( 'NONE',  ( -0.000000000000000000, -0.000000000000000000, 1.000000000000000000 ) ) ;
#52486 = DIRECTION ( 'NONE',  ( -1.000000000000000000, 0.000000000000000000, 0.000000000000000000 ) ) ;
#52487 = DIRECTION ( 'NONE',  ( -1.000000000000000000, 0.000000000000000000, 0.000000000000000000 ) ) ;
#52488 = AXIS2_PLACEMENT_3D ( 'NONE', #42668, #65296, #63894 ) ;
#52489 = ORIENTED_EDGE ( 'NONE', *, *, #34185, .T. ) ;
#52490 = CARTESIAN_POINT ( 'NONE',  ( 7.500000000000000000, -53.81370849898476649, -16.00000000000000000 ) ) ;
#52491 = CARTESIAN_POINT ( 'NONE',  ( 49.00000000000000000, -14.06939075806900163, -20.80000000000000426 ) ) ;
#52492 = VECTOR ( 'NONE', #21576, 1000.000000000000000 ) ;
#52493 = CARTESIAN_POINT ( 'NONE',  ( 9.703773737882785966, -9.703773737882814387, 26.00000000000000000 ) ) ;
#52494 = ORIENTED_EDGE ( 'NONE', *, *, #35278, .T. ) ;
#52495 = CARTESIAN_POINT ( 'NONE',  ( -10.03972626211722918, 8.916576262117214213, 54.00000000000000711 ) ) ;
#52496 = DIRECTION ( 'NONE',  ( -0.8660254037844482555, 0.000000000000000000, 0.4999999999999831801 ) ) ;
#52497 = LINE ( 'NONE', #47196, #41023 ) ;
#52498 = PLANE ( 'NONE',  #7595 ) ;
#52499 = LINE ( 'NONE', #4069, #18369 ) ;
#52500 = AXIS2_PLACEMENT_3D ( 'NONE', #18656, #12298, #66749 ) ;
#52501 = EDGE_LOOP ( 'NONE', ( #14990, #67284, #36404, #51065 ) ) ;
#52502 = CARTESIAN_POINT ( 'NONE',  ( 47.00000000000000000, 0.7500000000000000000, -3.418698582794335028 ) ) ;
#52503 = CARTESIAN_POINT ( 'NONE',  ( 10.74648345035337904, -1.690483450353490680, 455.0000000000000568 ) ) ;
#52504 = LINE ( 'NONE', #21016, #35704 ) ;
#52505 = VECTOR ( 'NONE', #57032, 1000.000000000000114 ) ;
#52506 =( NAMED_UNIT ( * ) PLANE_ANGLE_UNIT ( ) SI_UNIT ( $, .RADIAN. ) );
#52507 = DIRECTION ( 'NONE',  ( -1.000000000000000000, 0.000000000000000000, 0.000000000000000000 ) ) ;
#52508 = ORIENTED_EDGE ( 'NONE', *, *, #4980, .F. ) ;
#52510 = ORIENTED_EDGE ( 'NONE', *, *, #286, .T. ) ;
#52509 = CARTESIAN_POINT ( 'NONE',  ( -4.706725378239257296, -6.358413763958960629, 54.00000000000000711 ) ) ;
#52511 =( GEOMETRIC_REPRESENTATION_CONTEXT ( 3 ) GLOBAL_UNCERTAINTY_ASSIGNED_CONTEXT ( ( #16803 ) ) GLOBAL_UNIT_ASSIGNED_CONTEXT ( ( #34449, #39418, #28129 ) ) REPRESENTATION_CONTEXT ( 'NONE', 'WORKASPACE' ) );
#52512 = LINE ( 'NONE', #15384, #29336 ) ;
#52513 = FACE_OUTER_BOUND ( 'NONE', #29970, .T. ) ;
#52514 = VECTOR ( 'NONE', #33669, 1000.000000000000000 ) ;
#52515 = CARTESIAN_POINT ( 'NONE',  ( 10.62249899919920004, -25.00000000000000000, 17.50000000000000000 ) ) ;
#52516 = ORIENTED_EDGE ( 'NONE', *, *, #58742, .T. ) ;
#52517 = EDGE_CURVE ( 'NONE', #39720, #42310, #3997, .T. ) ;
#52518 = EDGE_CURVE ( 'NONE', #10988, #54968, #48181, .T. ) ;
#52519 = EDGE_CURVE ( 'NONE', #3656, #35382, #23072, .T. ) ;
#52520 = SURFACE_STYLE_USAGE ( .BOTH. , #15035 ) ;
#52521 = PLANE ( 'NONE',  #38658 ) ;
#52522 = VERTEX_POINT ( 'NONE', #30862 ) ;
#52523 = ORIENTED_EDGE ( 'NONE', *, *, #334, .F. ) ;
#52524 = EDGE_CURVE ( 'NONE', #57275, #19769, #62586, .T. ) ;
#52525 = ORIENTED_EDGE ( 'NONE', *, *, #47422, .F. ) ;
#52526 = CARTESIAN_POINT ( 'NONE',  ( -8.916576262117343887, -8.930623737882761759, 26.00000000000000000 ) ) ;
#52527 = CARTESIAN_POINT ( 'NONE',  ( 3.857023737882779635, -10.31452373788280141, 26.00000000000000000 ) ) ;
#52528 = CIRCLE ( 'NONE', #61524, 4.000000000000001776 ) ;
#52529 = PLANE ( 'NONE',  #17928 ) ;
#52530 = CYLINDRICAL_SURFACE ( 'NONE', #46071, 1.224999999999998757 ) ;
#52531 = EDGE_LOOP ( 'NONE', ( #59720, #12078, #57671, #57730 ) ) ;
#52532 = ORIENTED_EDGE ( 'NONE', *, *, #26223, .F. ) ;
#52533 = CARTESIAN_POINT ( 'NONE',  ( -10.49297626211729551, -6.849523737882748264, 54.00000000000000711 ) ) ;
#52534 = LINE ( 'NONE', #63134, #9039 ) ;
#52535 = ORIENTED_EDGE ( 'NONE', *, *, #61879, .F. ) ;
#52536 = VECTOR ( 'NONE', #50315, 1000.000000000000000 ) ;
#52537 = ORIENTED_EDGE ( 'NONE', *, *, #51422, .T. ) ;
#52538 = VERTEX_POINT ( 'NONE', #14597 ) ;
#52539 = ORIENTED_EDGE ( 'NONE', *, *, #22090, .T. ) ;
#52540 = AXIS2_PLACEMENT_3D ( 'NONE', #62122, #46214, #14754 ) ;
#52541 = DIRECTION ( 'NONE',  ( -0.000000000000000000, 3.673940397442059868E-16, -1.000000000000000000 ) ) ;
#52543 = ORIENTED_EDGE ( 'NONE', *, *, #11274, .F. ) ;
#52542 = LINE ( 'NONE', #26366, #40091 ) ;
#52544 = LINE ( 'NONE', #25319, #25555 ) ;
#52545 = VECTOR ( 'NONE', #68803, 1000.000000000000000 ) ;
#52546 = VECTOR ( 'NONE', #51959, 1000.000000000000000 ) ;
#52547 = AXIS2_PLACEMENT_3D ( 'NONE', #1635, #49413, #43749 ) ;
#52548 = DIRECTION ( 'NONE',  ( 1.000000000000000000, -0.000000000000000000, -0.000000000000000000 ) ) ;
#52549 = AXIS2_PLACEMENT_3D ( 'NONE', #62963, #14516, #13460 ) ;
#52550 = CARTESIAN_POINT ( 'NONE',  ( -7.250000000000001776, -7.249999999999998224, -14.00000000000000000 ) ) ;
#52551 = ORIENTED_EDGE ( 'NONE', *, *, #60371, .F. ) ;
#52552 = VERTEX_POINT ( 'NONE', #3645 ) ;
#52553 = VECTOR ( 'NONE', #46949, 1000.000000000000000 ) ;
#52554 = VECTOR ( 'NONE', #9297, 1000.000000000000000 ) ;
#52555 = FACE_OUTER_BOUND ( 'NONE', #48882, .T. ) ;
#52556 = AXIS2_PLACEMENT_3D ( 'NONE', #35455, #58458, #9663 ) ;
#52557 = DIRECTION ( 'NONE',  ( 0.7671651518153006499, -0.6414496315691565753, -2.356647714346250026E-16 ) ) ;
#52558 = ORIENTED_EDGE ( 'NONE', *, *, #55038, .T. ) ;
#52559 = ADVANCED_FACE ( 'NONE', ( #68707 ), #10349, .F. ) ;
#52560 = VECTOR ( 'NONE', #57784, 1000.000000000000000 ) ;
#52561 = CARTESIAN_POINT ( 'NONE',  ( 7.250000000000005329, -8.249999999999998224, -13.50000000000000178 ) ) ;
#52562 = CARTESIAN_POINT ( 'NONE',  ( 15.00000000000000000, 0.000000000000000000, 27.00000000000000000 ) ) ;
#52563 = EDGE_CURVE ( 'NONE', #25374, #13215, #56935, .T. ) ;
#52564 = EDGE_CURVE ( 'NONE', #2326, #43590, #32124, .T. ) ;
#52565 = LINE ( 'NONE', #68470, #25407 ) ;
#52566 = ORIENTED_EDGE ( 'NONE', *, *, #22399, .F. ) ;
#52567 = DIRECTION ( 'NONE',  ( 0.3479852726768751237, 0.000000000000000000, -0.9375000000000004441 ) ) ;
#52568 = LINE ( 'NONE', #59611, #61822 ) ;
#52569 = DIRECTION ( 'NONE',  ( -1.000000000000000000, 0.000000000000000000, 0.000000000000000000 ) ) ;
#52570 = ADVANCED_FACE ( 'NONE', ( #57727 ), #20250, .F. ) ;
#52571 = CARTESIAN_POINT ( 'NONE',  ( -11.75000000000000000, -5.200000000000001066, 11.75000000000000000 ) ) ;
#52572 = ADVANCED_FACE ( 'NONE', ( #36510, #58081 ), #15657, .T. ) ;
#52573 = FACE_OUTER_BOUND ( 'NONE', #41628, .T. ) ;
#52574 = EDGE_CURVE ( 'NONE', #58003, #36321, #42162, .T. ) ;
#52575 = VERTEX_POINT ( 'NONE', #52804 ) ;
#52576 = FACE_OUTER_BOUND ( 'NONE', #6179, .T. ) ;
#52577 = CARTESIAN_POINT ( 'NONE',  ( -4.031976262117261456, 3.142976262117183506, 54.00000000000000711 ) ) ;
#52579 = EDGE_CURVE ( 'NONE', #43306, #48961, #10616, .T. ) ;
#52578 = FILL_AREA_STYLE_COLOUR ( '', #69468 ) ;
#52580 = CARTESIAN_POINT ( 'NONE',  ( -5.993516549646711766, 5.993516549646603409, 455.0000000000000568 ) ) ;
#52581 = CARTESIAN_POINT ( 'NONE',  ( 14.50000000000000000, -42.50000000000000000, -15.10000000000000142 ) ) ;
#52582 = VECTOR ( 'NONE', #39150, 1000.000000000000000 ) ;
#52583 = DIRECTION ( 'NONE',  ( 0.000000000000000000, 0.000000000000000000, 1.000000000000000000 ) ) ;
#52584 = DIRECTION ( 'NONE',  ( -0.000000000000000000, -0.000000000000000000, -1.000000000000000000 ) ) ;
#52585 = CARTESIAN_POINT ( 'NONE',  ( -29.50000000000000355, -12.00000000000000000, -10.52786404500095863 ) ) ;
#52586 = ORIENTED_EDGE ( 'NONE', *, *, #62428, .F. ) ;
#52587 = CARTESIAN_POINT ( 'NONE',  ( -6.350872789121327244, 6.822336235477381550, 54.00000000000000711 ) ) ;
#52588 = CARTESIAN_POINT ( 'NONE',  ( 275.0000000000000000, -0.5000000000000000000, 26.50000000000000000 ) ) ;
#52589 = AXIS2_PLACEMENT_3D ( 'NONE', #65717, #66047, #22246 ) ;
#52590 = CARTESIAN_POINT ( 'NONE',  ( -29.50000000000000355, -11.50000000000100009, -15.00000000000084910 ) ) ;
#52591 = CARTESIAN_POINT ( 'NONE',  ( -17.51999999999999957, -17.50000000000000000, -26.00000000000000355 ) ) ;
#52592 = DIRECTION ( 'NONE',  ( 1.000000000000000000, 0.000000000000000000, 0.000000000000000000 ) ) ;
#52593 = AXIS2_PLACEMENT_3D ( 'NONE', #35964, #29599, #35240 ) ;
#52594 = LINE ( 'NONE', #25726, #11640 ) ;
#52595 = CARTESIAN_POINT ( 'NONE',  ( 29.50000000000000355, -15.46862696659690073, -14.50000000000000000 ) ) ;
#52596 = ORIENTED_EDGE ( 'NONE', *, *, #3804, .T. ) ;
#52597 = AXIS2_PLACEMENT_3D ( 'NONE', #13570, #23128, #40072 ) ;
#52598 = VECTOR ( 'NONE', #53286, 1000.000000000000000 ) ;
#52599 = VECTOR ( 'NONE', #65499, 1000.000000000000000 ) ;
#52600 = EDGE_LOOP ( 'NONE', ( #25764, #44227 ) ) ;
#52601 = DIRECTION ( 'NONE',  ( 0.000000000000000000, 0.9760787414516765015, 0.2174173187354474512 ) ) ;
#52602 = DIRECTION ( 'NONE',  ( 0.000000000000000000, 0.000000000000000000, -1.000000000000000000 ) ) ;
#52603 = ORIENTED_EDGE ( 'NONE', *, *, #30757, .T. ) ;
#52604 = PLANE ( 'NONE',  #20179 ) ;
#52605 = AXIS2_PLACEMENT_3D ( 'NONE', #19361, #50499, #40581 ) ;
#52606 = AXIS2_PLACEMENT_3D ( 'NONE', #26961, #38268, #49558 ) ;
#52607 = CARTESIAN_POINT ( 'NONE',  ( -9.915476262117195461, -0.9555237378827157180, 26.00000000000000711 ) ) ;
#52608 = ORIENTED_EDGE ( 'NONE', *, *, #19390, .F. ) ;
#52609 = VECTOR ( 'NONE', #64659, 1000.000000000000000 ) ;
#52610 = CARTESIAN_POINT ( 'NONE',  ( 8.750000000000003553, 7.750000000000000000, 5.000000000000000000 ) ) ;
#52611 = ORIENTED_EDGE ( 'NONE', *, *, #28874, .F. ) ;
#52612 = EDGE_LOOP ( 'NONE', ( #57921, #30546, #38751, #32651 ) ) ;
#52613 = PLANE ( 'NONE',  #57836 ) ;
#52614 = ORIENTED_EDGE ( 'NONE', *, *, #25832, .T. ) ;
#52615 = ORIENTED_EDGE ( 'NONE', *, *, #4732, .F. ) ;
#52616 = DIRECTION ( 'NONE',  ( 0.000000000000000000, 0.000000000000000000, -1.000000000000000000 ) ) ;
#52617 = PLANE ( 'NONE',  #8775 ) ;
#52618 = VECTOR ( 'NONE', #37458, 1000.000000000000000 ) ;
#52619 = DIRECTION ( 'NONE',  ( -1.000000000000000000, 0.000000000000000000, 0.000000000000000000 ) ) ;
#52620 = ORIENTED_EDGE ( 'NONE', *, *, #52887, .F. ) ;
#52621 = AXIS2_PLACEMENT_3D ( 'NONE', #35676, #62914, #56892 ) ;
#52622 = DIRECTION ( 'NONE',  ( -1.000000000000000000, 0.000000000000000000, 0.000000000000000000 ) ) ;
#52624 = DIRECTION ( 'NONE',  ( -1.000000000000000000, 0.000000000000000000, 0.000000000000000000 ) ) ;
#52623 = CARTESIAN_POINT ( 'NONE',  ( -11.11351654964680336, -9.106483450353373144, 455.0000000000000568 ) ) ;
#52625 = EDGE_CURVE ( 'NONE', #4940, #24424, #36885, .T. ) ;
#52626 = ORIENTED_EDGE ( 'NONE', *, *, #67057, .F. ) ;
#52627 = ORIENTED_EDGE ( 'NONE', *, *, #495, .F. ) ;
#52628 = ORIENTED_EDGE ( 'NONE', *, *, #2090, .T. ) ;
#52629 = ITEM_DEFINED_TRANSFORMATION ( 'NONE', 'NONE', #15508,  #45918 ) ;
#52630 = ADVANCED_FACE ( 'NONE', ( #58450 ), #52081, .T. ) ;
#52631 = APPLICATION_CONTEXT ( 'automotive_design' ) ;
#52632 = DIRECTION ( 'NONE',  ( 9.799566706031580591E-15, 1.000000000000000000, 1.836970198721018348E-16 ) ) ;
#52634 = VERTEX_POINT ( 'NONE', #47471 ) ;
#52633 = DIRECTION ( 'NONE',  ( -1.000000000000000000, 0.000000000000000000, 0.000000000000000000 ) ) ;
#52635 = CARTESIAN_POINT ( 'NONE',  ( 7.250000000000005329, -7.249999999999998224, -26.00000000000001066 ) ) ;
#52636 = CARTESIAN_POINT ( 'NONE',  ( 10.50702373788281818, -9.795823737882802362, 26.00000000000000000 ) ) ;
#52637 = EDGE_LOOP ( 'NONE', ( #60028, #38380, #68112, #28507 ) ) ;
#52638 = EDGE_CURVE ( 'NONE', #5044, #60174, #11763, .T. ) ;
#52639 = CIRCLE ( 'NONE', #700, 5.000000000000004441 ) ;
#52640 = ORIENTED_EDGE ( 'NONE', *, *, #44937, .F. ) ;
#52641 = FACE_BOUND ( 'NONE', #38069, .T. ) ;
#52642 = AXIS2_PLACEMENT_3D ( 'NONE', #23886, #28825, #50748 ) ;
#52643 = ADVANCED_FACE ( 'NONE', ( #25211 ), #35809, .F. ) ;
#52644 = EDGE_LOOP ( 'NONE', ( #55699, #58260, #34760 ) ) ;
#52645 = LINE ( 'NONE', #21163, #38112 ) ;
#52646 = DIRECTION ( 'NONE',  ( 1.000000000000000000, -0.000000000000000000, 0.000000000000000000 ) ) ;
#52647 = VECTOR ( 'NONE', #68768, 1000.000000000000000 ) ;
#52648 = FACE_OUTER_BOUND ( 'NONE', #67070, .T. ) ;
#52649 = VERTEX_POINT ( 'NONE', #41109 ) ;
#52650 = VECTOR ( 'NONE', #41507, 999.9999999999998863 ) ;
#52651 = VECTOR ( 'NONE', #51078, 1000.000000000000000 ) ;
#52652 = VECTOR ( 'NONE', #25853, 1000.000000000000000 ) ;
#52653 = LINE ( 'NONE', #36020, #13197 ) ;
#52654 = EDGE_CURVE ( 'NONE', #17991, #31578, #46763, .T. ) ;
#52655 = LINE ( 'NONE', #64563, #64215 ) ;
#52657 = VERTEX_POINT ( 'NONE', #65145 ) ;
#52656 = CYLINDRICAL_SURFACE ( 'NONE', #37675, 5.200000000000009948 ) ;
#52659 = ORIENTED_EDGE ( 'NONE', *, *, #66979, .F. ) ;
#52658 = LINE ( 'NONE', #31445, #52402 ) ;
#52660 = LINE ( 'NONE', #46986, #476 ) ;
#52661 = CIRCLE ( 'NONE', #23306, 0.8128000000000145109 ) ;
#52662 = CIRCLE ( 'NONE', #30074, 0.9999999999999991118 ) ;
#52663 = CIRCLE ( 'NONE', #27814, 0.5000000000079367624 ) ;
#52664 = CARTESIAN_POINT ( 'NONE',  ( -10.49297626211725110, -3.664523737882711352, 54.00000000000000711 ) ) ;
#52665 = LINE ( 'NONE', #3511, #58429 ) ;
#52666 = PLANE ( 'NONE',  #6853 ) ;
#52667 = CIRCLE ( 'NONE', #49283, 0.06000000000000102474 ) ;
#52668 = LINE ( 'NONE', #37097, #61254 ) ;
#52669 = EDGE_CURVE ( 'NONE', #21676, #31344, #22686, .T. ) ;
#52670 = ORIENTED_EDGE ( 'NONE', *, *, #14141, .F. ) ;
#52671 = LINE ( 'NONE', #46995, #1900 ) ;
#52672 = CARTESIAN_POINT ( 'NONE',  ( -8.250000000000001776, 0.000000000000000000, -15.00000000000000000 ) ) ;
#52674 = EDGE_CURVE ( 'NONE', #59671, #9593, #16002, .T. ) ;
#52673 = SURFACE_STYLE_USAGE ( .BOTH. , #31094 ) ;
#52676 = ORIENTED_EDGE ( 'NONE', *, *, #68215, .F. ) ;
#52675 = LINE ( 'NONE', #64320, #7387 ) ;
#52677 = VECTOR ( 'NONE', #14037, 999.9999999999998863 ) ;
#52678 = DIRECTION ( 'NONE',  ( 0.000000000000000000, 1.000000000000000000, 0.000000000000000000 ) ) ;
#52679 = PLANE ( 'NONE',  #46527 ) ;
#52680 = CARTESIAN_POINT ( 'NONE',  ( -9.547976262117254365, 8.130476262117182884, 54.00000000000000711 ) ) ;
#52681 = ORIENTED_EDGE ( 'NONE', *, *, #64380, .F. ) ;
#52682 = CARTESIAN_POINT ( 'NONE',  ( -4.141586236041129077, -4.720772854004773755, 54.00000000000000711 ) ) ;
#52683 = CARTESIAN_POINT ( 'NONE',  ( 4.740315990920124456, 7.798499376343988487, 195.0000000000000284 ) ) ;
#52684 = EDGE_CURVE ( 'NONE', #26683, #18078, #6132, .T. ) ;
#52685 = ORIENTED_EDGE ( 'NONE', *, *, #22446, .T. ) ;
#52686 = CARTESIAN_POINT ( 'NONE',  ( 46.39999999999999858, 21.00000000000000000, 1.750000000000000222 ) ) ;
#52687 = PLANE ( 'NONE',  #53556 ) ;
#52688 = DIRECTION ( 'NONE',  ( 0.000000000000000000, 0.000000000000000000, -1.000000000000000000 ) ) ;
#52689 = LINE ( 'NONE', #8118, #55668 ) ;
#52690 = ORIENTED_EDGE ( 'NONE', *, *, #1152, .T. ) ;
#52691 = ORIENTED_EDGE ( 'NONE', *, *, #16132, .T. ) ;
#52692 = VERTEX_POINT ( 'NONE', #33642 ) ;
#52693 = ORIENTED_EDGE ( 'NONE', *, *, #63477, .T. ) ;
#52694 = ORIENTED_EDGE ( 'NONE', *, *, #61016, .T. ) ;
#52695 = LINE ( 'NONE', #57631, #54014 ) ;
#52696 = VECTOR ( 'NONE', #22762, 1000.000000000000000 ) ;
#52697 = ADVANCED_FACE ( 'NONE', ( #55214 ), #60160, .F. ) ;
#52698 = CARTESIAN_POINT ( 'NONE',  ( -3.834182069070823040, -7.357023737882818715, 54.00000000000000711 ) ) ;
#52699 = VECTOR ( 'NONE', #63695, 1000.000000000000000 ) ;
#52700 = VECTOR ( 'NONE', #57673, 1000.000000000000000 ) ;
#52701 = DIRECTION ( 'NONE',  ( 0.000000000000000000, 0.000000000000000000, -1.000000000000000000 ) ) ;
#52702 = ORIENTED_EDGE ( 'NONE', *, *, #29694, .F. ) ;
#52703 = ORIENTED_EDGE ( 'NONE', *, *, #27187, .T. ) ;
#52704 = LINE ( 'NONE', #19105, #6947 ) ;
#52705 = EDGE_LOOP ( 'NONE', ( #32801, #25187, #15162, #40757 ) ) ;
#52706 = ADVANCED_FACE ( 'NONE', ( #6759 ), #28326, .F. ) ;
#52707 = ORIENTED_EDGE ( 'NONE', *, *, #59966, .T. ) ;
#52708 = CIRCLE ( 'NONE', #56105, 0.2000000000000005107 ) ;
#52709 = VECTOR ( 'NONE', #49788, 1000.000000000000000 ) ;
#52710 = CIRCLE ( 'NONE', #34597, 0.3000000000005387246 ) ;
#52711 = CARTESIAN_POINT ( 'NONE',  ( 9.899999999999998579, -0.2000000000089119934, -8.913009219568841313E-12 ) ) ;
#52712 = CARTESIAN_POINT ( 'NONE',  ( 7.000000000000000000, -42.50000000000000000, 10.20000000000000107 ) ) ;
#52713 = CYLINDRICAL_SURFACE ( 'NONE', #15160, 0.1749999999999998224 ) ;
#52714 = ORIENTED_EDGE ( 'NONE', *, *, #47956, .T. ) ;
#52715 = ADVANCED_FACE ( 'NONE', ( #37574 ), #69751, .F. ) ;
#52716 = DIRECTION ( 'NONE',  ( 0.000000000000000000, 1.000000000000000000, 0.000000000000000000 ) ) ;
#52717 = AXIS2_PLACEMENT_3D ( 'NONE', #27349, #6119, #53884 ) ;
#52718 = AXIS2_PLACEMENT_3D ( 'NONE', #66685, #23550, #29551 ) ;
#52720 = LINE ( 'NONE', #48442, #61446 ) ;
#52719 = PLANE ( 'NONE',  #50230 ) ;
#52721 = ORIENTED_EDGE ( 'NONE', *, *, #11108, .F. ) ;
#52722 = EDGE_CURVE ( 'NONE', #3304, #69903, #16702, .T. ) ;
#52724 = VERTEX_POINT ( 'NONE', #42861 ) ;
#52723 = DIRECTION ( 'NONE',  ( -0.7071067811865500152, -0.7071067811865451302, 0.000000000000000000 ) ) ;
#52725 = VERTEX_POINT ( 'NONE', #16341 ) ;
#52726 = CIRCLE ( 'NONE', #69620, 24.99999999998789946 ) ;
#52727 = EDGE_CURVE ( 'NONE', #62021, #44522, #48524, .T. ) ;
#52728 = DIRECTION ( 'NONE',  ( -1.836970198721029934E-16, 1.836970198721036344E-16, -1.000000000000000000 ) ) ;
#52729 = AXIS2_PLACEMENT_3D ( 'NONE', #15617, #26212, #53791 ) ;
#52730 = DIRECTION ( 'NONE',  ( -0.000000000000000000, -0.000000000000000000, -1.000000000000000000 ) ) ;
#52731 = VERTEX_POINT ( 'NONE', #54187 ) ;
#52732 = ORIENTED_EDGE ( 'NONE', *, *, #26487, .F. ) ;
#52733 = EDGE_CURVE ( 'NONE', #9315, #8669, #21308, .T. ) ;
#52734 = EDGE_CURVE ( 'NONE', #60914, #7905, #12860, .T. ) ;
#52735 = DIRECTION ( 'NONE',  ( 1.836970198721029934E-16, 1.836970198721010706E-16, -1.000000000000000000 ) ) ;
#52736 = CARTESIAN_POINT ( 'NONE',  ( 7.250000000000005329, 8.250000000000001776, -26.00000000000001066 ) ) ;
#52737 = VERTEX_POINT ( 'NONE', #5745 ) ;
#52738 = ADVANCED_FACE ( 'NONE', ( #43210 ), #59482, .T. ) ;
#52739 = ADVANCED_FACE ( 'NONE', ( #64443 ), #60509, .F. ) ;
#52740 = ORIENTED_EDGE ( 'NONE', *, *, #51084, .T. ) ;
#52741 = CARTESIAN_POINT ( 'NONE',  ( 8.900000000000002132, 18.00000000000000355, 21.00000000000000000 ) ) ;
#52742 = DIRECTION ( 'NONE',  ( 0.000000000000000000, 0.000000000000000000, -1.000000000000000000 ) ) ;
#52743 = ORIENTED_EDGE ( 'NONE', *, *, #68999, .T. ) ;
#52744 = EDGE_CURVE ( 'NONE', #15490, #59745, #27646, .T. ) ;
#52745 = DIRECTION ( 'NONE',  ( -1.000000000000000000, 0.000000000000000000, 0.000000000000000000 ) ) ;
#52746 = CARTESIAN_POINT ( 'NONE',  ( 39.90000000000000568, 21.00000000000000000, -13.98999642601811999 ) ) ;
#52747 = CIRCLE ( 'NONE', #30101, 25.40000000000000213 ) ;
#52748 = ORIENTED_EDGE ( 'NONE', *, *, #24145, .F. ) ;
#52750 = ORIENTED_EDGE ( 'NONE', *, *, #64189, .F. ) ;
#52749 = DIRECTION ( 'NONE',  ( -0.000000000000000000, -0.000000000000000000, -1.000000000000000000 ) ) ;
#52751 = DIRECTION ( 'NONE',  ( 0.000000000000000000, 0.000000000000000000, 1.000000000000000000 ) ) ;
#52752 = STYLED_ITEM ( 'NONE', ( #6279 ), #19304 ) ;
#52753 = CARTESIAN_POINT ( 'NONE',  ( 4.456444791733522252E-16, 7.450000000000002842, -9.000000000000001776 ) ) ;
#52754 = PLANE ( 'NONE',  #34612 ) ;
#52755 = PLANE ( 'NONE',  #54983 ) ;
#52756 = DIRECTION ( 'NONE',  ( -8.903847840905249551E-15, -1.000000000000000000, -1.836970198721027222E-16 ) ) ;
#52757 = VECTOR ( 'NONE', #19419, 1000.000000000000000 ) ;
#52758 = VECTOR ( 'NONE', #3849, 1000.000000000000000 ) ;
#52759 = CARTESIAN_POINT ( 'NONE',  ( 3.157023737882800329, 6.486996718459884903, 26.00000000000000711 ) ) ;
#52760 = EDGE_CURVE ( 'NONE', #55829, #17506, #61409, .T. ) ;
#52761 = ORIENTED_EDGE ( 'NONE', *, *, #37584, .F. ) ;
#52762 = LINE ( 'NONE', #4321, #51876 ) ;
#52765 = VERTEX_POINT ( 'NONE', #65816 ) ;
#52764 = EDGE_CURVE ( 'NONE', #37068, #69196, #54878, .T. ) ;
#52763 = CARTESIAN_POINT ( 'NONE',  ( -17.00000000000000000, -16.64230188589299786, -14.64519951917100116 ) ) ;
#52766 = CIRCLE ( 'NONE', #5369, 0.2000000000000005107 ) ;
#52768 = CARTESIAN_POINT ( 'NONE',  ( 5.257023737882801306, 5.242976262117200470, 54.00000000000000711 ) ) ;
#52767 = VECTOR ( 'NONE', #20364, 1000.000000000000000 ) ;
#52769 = LINE ( 'NONE', #46728, #24454 ) ;
#52770 =( GEOMETRIC_REPRESENTATION_CONTEXT ( 3 ) GLOBAL_UNCERTAINTY_ASSIGNED_CONTEXT ( ( #64207 ) ) GLOBAL_UNIT_ASSIGNED_CONTEXT ( ( #29277, #34232, #43224 ) ) REPRESENTATION_CONTEXT ( 'NONE', 'WORKASPACE' ) );
#52771 = CARTESIAN_POINT ( 'NONE',  ( 0.000000000000000000, -42.00000000000000000, -26.50000000000000000 ) ) ;
#52772 = DIRECTION ( 'NONE',  ( 0.000000000000000000, -0.7071067811865077157, 0.7071067811865873187 ) ) ;
#52773 = AXIS2_PLACEMENT_3D ( 'NONE', #32905, #37524, #6039 ) ;
#52774 = VECTOR ( 'NONE', #8136, 1000.000000000000000 ) ;
#52775 = VERTEX_POINT ( 'NONE', #23720 ) ;
#52776 = DIRECTION ( 'NONE',  ( 0.000000000000000000, 0.5547756303226741847, -0.8320000000000477014 ) ) ;
#52777 = DIRECTION ( 'NONE',  ( 0.000000000000000000, 0.000000000000000000, 1.000000000000000000 ) ) ;
#52778 = VERTEX_POINT ( 'NONE', #61183 ) ;
#52779 = DIRECTION ( 'NONE',  ( 0.000000000000000000, 1.000000000000000000, 0.000000000000000000 ) ) ;
#52780 = VECTOR ( 'NONE', #54042, 1000.000000000000000 ) ;
#52781 = VECTOR ( 'NONE', #34264, 1000.000000000000000 ) ;
#52782 = LINE ( 'NONE', #68316, #59011 ) ;
#52783 = EDGE_CURVE ( 'NONE', #16805, #38091, #64841, .T. ) ;
#52784 = VERTEX_POINT ( 'NONE', #60846 ) ;
#52785 = LINE ( 'NONE', #30840, #56418 ) ;
#52786 = ORIENTED_EDGE ( 'NONE', *, *, #9379, .F. ) ;
#52787 = ORIENTED_EDGE ( 'NONE', *, *, #60453, .T. ) ;
#52788 = CARTESIAN_POINT ( 'NONE',  ( 27.90000000000000213, 20.60000000000000142, 13.86939075806899702 ) ) ;
#52789 = DIRECTION ( 'NONE',  ( 1.000000000000000000, -0.000000000000000000, -0.000000000000000000 ) ) ;
#52790 = CYLINDRICAL_SURFACE ( 'NONE', #64950, 5.250000000000000000 ) ;
#52791 = PLANE ( 'NONE',  #49062 ) ;
#52792 = CARTESIAN_POINT ( 'NONE',  ( -9.547976262117254365, 2.355476262117183417, 26.00000000000000711 ) ) ;
#52793 = ORIENTED_EDGE ( 'NONE', *, *, #53069, .F. ) ;
#52794 = ORIENTED_EDGE ( 'NONE', *, *, #26789, .T. ) ;
#52796 = ORIENTED_EDGE ( 'NONE', *, *, #2801, .T. ) ;
#52795 = CARTESIAN_POINT ( 'NONE',  ( -9.690000000000001279, 9.690000000000001279, -4.250000000000000000 ) ) ;
#52797 = EDGE_LOOP ( 'NONE', ( #9686, #25743, #54189, #51659 ) ) ;
#52798 = EDGE_CURVE ( 'NONE', #53583, #65777, #484, .T. ) ;
#52799 = CARTESIAN_POINT ( 'NONE',  ( 8.612468434717188259, 1.991476262117162888, 54.00000000000000711 ) ) ;
#52800 = FACE_OUTER_BOUND ( 'NONE', #61921, .T. ) ;
#52801 = CARTESIAN_POINT ( 'NONE',  ( 10.50702373788278265, 3.650476262117142934, 54.00000000000000711 ) ) ;
#52802 = EDGE_CURVE ( 'NONE', #31596, #55024, #34311, .T. ) ;
#52803 = CARTESIAN_POINT ( 'NONE',  ( 11.00000000000000000, -12.00000000000000000, -10.52786404500095863 ) ) ;
#52805 = CARTESIAN_POINT ( 'NONE',  ( 275.0000000000000000, -23.65000000000000568, 12.40000000000000213 ) ) ;
#52804 = CARTESIAN_POINT ( 'NONE',  ( -7.250000000000000888, -8.249999999999998224, -19.00000000000000000 ) ) ;
#52806 = EDGE_CURVE ( 'NONE', #37820, #51075, #2154, .T. ) ;
#52807 = ORIENTED_EDGE ( 'NONE', *, *, #45184, .F. ) ;
#52808 = EDGE_LOOP ( 'NONE', ( #28169, #41257, #21136, #6197 ) ) ;
#52809 = ORIENTED_EDGE ( 'NONE', *, *, #59334, .T. ) ;
#52810 = CIRCLE ( 'NONE', #46008, 0.1999999999999992339 ) ;
#52811 = VECTOR ( 'NONE', #13161, 1000.000000000000000 ) ;
#52812 = AXIS2_PLACEMENT_3D ( 'NONE', #53613, #20721, #37007 ) ;
#52813 = FACE_OUTER_BOUND ( 'NONE', #32712, .T. ) ;
#52814 = ADVANCED_FACE ( 'NONE', ( #7097 ), #19116, .T. ) ;
#52815 = DIRECTION ( 'NONE',  ( 0.5000000000000004441, -0.8660254037844383745, 0.000000000000000000 ) ) ;
#52816 = AXIS2_PLACEMENT_3D ( 'NONE', #5806, #6500, #11101 ) ;
#52817 = AXIS2_PLACEMENT_3D ( 'NONE', #9683, #14288, #31946 ) ;
#52818 = DIRECTION ( 'NONE',  ( 0.000000000000000000, 0.000000000000000000, -1.000000000000000000 ) ) ;
#52819 = EDGE_LOOP ( 'NONE', ( #39182, #65249, #1552, #36907 ) ) ;
#52820 = ORIENTED_EDGE ( 'NONE', *, *, #66438, .T. ) ;
#52821 = ORIENTED_EDGE ( 'NONE', *, *, #39740, .T. ) ;
#52822 = LINE ( 'NONE', #42534, #59879 ) ;
#52823 = VECTOR ( 'NONE', #13594, 1000.000000000000000 ) ;
#52824 = VECTOR ( 'NONE', #15485, 1000.000000000000000 ) ;
#52825 = ORIENTED_EDGE ( 'NONE', *, *, #14352, .F. ) ;
#52826 = ORIENTED_EDGE ( 'NONE', *, *, #54242, .T. ) ;
#52827 = DIRECTION ( 'NONE',  ( 0.7071067811865514585, 0.7071067811865435759, -0.000000000000000000 ) ) ;
#52828 = ORIENTED_EDGE ( 'NONE', *, *, #31819, .F. ) ;
#52829 = EDGE_CURVE ( 'NONE', #59828, #18594, #33971, .T. ) ;
#52830 = ORIENTED_EDGE ( 'NONE', *, *, #40317, .T. ) ;
#52831 = CARTESIAN_POINT ( 'NONE',  ( 15.89999999999999680, -14.06939075806900874, 20.80000000000001137 ) ) ;
#52833 = ORIENTED_EDGE ( 'NONE', *, *, #47671, .F. ) ;
#52832 = DIRECTION ( 'NONE',  ( 1.920292680692490463E-14, 1.000000000000000000, 0.000000000000000000 ) ) ;
#52834 = ORIENTED_EDGE ( 'NONE', *, *, #35071, .T. ) ;
#52835 = AXIS2_PLACEMENT_3D ( 'NONE', #42648, #16479, #54309 ) ;
#52836 = CARTESIAN_POINT ( 'NONE',  ( 0.000000000000000000, 17.79289321881345032, 20.50000000000000000 ) ) ;
#52837 = DIRECTION ( 'NONE',  ( 3.491481338843133355E-15, 1.000000000000000000, 1.836970198721029934E-16 ) ) ;
#52839 = ORIENTED_EDGE ( 'NONE', *, *, #21341, .F. ) ;
#52838 = CARTESIAN_POINT ( 'NONE',  ( 13.00000000000000178, -16.28999999999710369, 15.00000000000794920 ) ) ;
#52840 = EDGE_LOOP ( 'NONE', ( #16111, #24741, #45206, #44747 ) ) ;
#52841 = CARTESIAN_POINT ( 'NONE',  ( -6.822336235477446387, 6.350872789121265072, 54.00000000000000711 ) ) ;
#52842 = CARTESIAN_POINT ( 'NONE',  ( -6.331612867284196255, -8.406483450353375630, 195.0000000000000284 ) ) ;
#52843 = DIRECTION ( 'NONE',  ( 0.000000000000000000, 0.000000000000000000, -1.000000000000000000 ) ) ;
#52844 = PLANE ( 'NONE',  #37277 ) ;
#52845 = ADVANCED_FACE ( 'NONE', ( #50243 ), #66847, .F. ) ;
#52846 = ORIENTED_EDGE ( 'NONE', *, *, #1840, .F. ) ;
#52847 = DIRECTION ( 'NONE',  ( 0.000000000000000000, 0.000000000000000000, -1.000000000000000000 ) ) ;
#52848 = EDGE_CURVE ( 'NONE', #15217, #50527, #8370, .T. ) ;
#52849 = CARTESIAN_POINT ( 'NONE',  ( 39.90000000000000568, 0.000000000000000000, 0.000000000000000000 ) ) ;
#52850 = LINE ( 'NONE', #47519, #24401 ) ;
#52851 = VECTOR ( 'NONE', #37978, 1000.000000000000000 ) ;
#52852 = ADVANCED_FACE ( 'NONE', ( #44578 ), #12399, .F. ) ;
#52853 = DIRECTION ( 'NONE',  ( 0.000000000000000000, 1.000000000000000000, 0.000000000000000000 ) ) ;
#52854 = DIRECTION ( 'NONE',  ( 0.000000000000000000, 0.000000000000000000, 1.000000000000000000 ) ) ;
#52855 = DIRECTION ( 'NONE',  ( 1.000000000000000000, -0.000000000000000000, 0.000000000000000000 ) ) ;
#52856 = ORIENTED_EDGE ( 'NONE', *, *, #62259, .F. ) ;
#52857 = CARTESIAN_POINT ( 'NONE',  ( 20.90000000000000213, 20.60000000000000142, -13.86939075806900057 ) ) ;
#52858 = DIRECTION ( 'NONE',  ( -0.000000000000000000, -0.000000000000000000, -1.000000000000000000 ) ) ;
#52859 = AXIS2_PLACEMENT_3D ( 'NONE', #20579, #14936, #42144 ) ;
#52860 = CARTESIAN_POINT ( 'NONE',  ( -4.706725378239217328, 4.141586236041038482, 26.00000000000000711 ) ) ;
#52861 = EDGE_LOOP ( 'NONE', ( #23186, #43733, #50406, #57310, #19020, #67132, #21749, #37763 ) ) ;
#52862 = PLANE ( 'NONE',  #46221 ) ;
#52864 = EDGE_CURVE ( 'NONE', #57125, #48543, #44939, .T. ) ;
#52863 = LINE ( 'NONE', #25981, #18539 ) ;
#52865 = FACE_OUTER_BOUND ( 'NONE', #8589, .T. ) ;
#52866 = AXIS2_PLACEMENT_3D ( 'NONE', #22732, #37970, #11088 ) ;
#52867 = CARTESIAN_POINT ( 'NONE',  ( 283.0000000000000568, -30.45000000000000639, -15.00000000000000000 ) ) ;
#52868 = AXIS2_PLACEMENT_3D ( 'NONE', #42955, #52174, #64539 ) ;
#52869 = FACE_OUTER_BOUND ( 'NONE', #47709, .T. ) ;
#52870 = ORIENTED_EDGE ( 'NONE', *, *, #7420, .T. ) ;
#52871 = FACE_OUTER_BOUND ( 'NONE', #66849, .T. ) ;
#52872 = LINE ( 'NONE', #20660, #38503 ) ;
#52873 = CARTESIAN_POINT ( 'NONE',  ( 6.344579767990805585, 8.393516549646626856, 195.0000000000000284 ) ) ;
#52874 = DIRECTION ( 'NONE',  ( 1.000000000000000000, -0.000000000000000000, -0.000000000000000000 ) ) ;
#52875 = DIRECTION ( 'NONE',  ( 2.135044278125299371E-15, 1.000000000000000000, 0.000000000000000000 ) ) ;
#52876 = VERTEX_POINT ( 'NONE', #35358 ) ;
#52878 = VERTEX_POINT ( 'NONE', #8496 ) ;
#52877 = CARTESIAN_POINT ( 'NONE',  ( 9.417013320880768035, 1.853252480934615809, 455.0000000000000568 ) ) ;
#52879 = ADVANCED_BREP_SHAPE_REPRESENTATION ( '', ( #21410, #45918 ), #44782 ) ;
#52880 = VECTOR ( 'NONE', #41161, 1000.000000000000000 ) ;
#52881 = EDGE_CURVE ( 'NONE', #52379, #57399, #44509, .T. ) ;
#52882 = LINE ( 'NONE', #63820, #21434 ) ;
#52883 = DIRECTION ( 'NONE',  ( -1.000000000000000000, 0.000000000000000000, 0.000000000000000000 ) ) ;
#52884 = DIRECTION ( 'NONE',  ( 0.7071067811865486830, 0.7071067811865464625, 0.000000000000000000 ) ) ;
#52885 = ORIENTED_EDGE ( 'NONE', *, *, #41301, .F. ) ;
#52886 = DIRECTION ( 'NONE',  ( 8.659560562354963673E-17, 0.7071067811865450192, -0.7071067811865500152 ) ) ;
#52887 = EDGE_CURVE ( 'NONE', #14877, #32707, #45624, .T. ) ;
#52888 = CARTESIAN_POINT ( 'NONE',  ( -7.250000000000000888, 7.250000000000001776, -26.00000000000001066 ) ) ;
#52889 = ADVANCED_FACE ( 'NONE', ( #7454 ), #56251, .F. ) ;
#52890 = ORIENTED_EDGE ( 'NONE', *, *, #68540, .T. ) ;
#52891 = EDGE_LOOP ( 'NONE', ( #32782, #39279, #34179, #30330, #62664, #53249, #12757, #34779, #19916, #61371, #54653, #50752, #33049, #7198, #25123, #42006, #65906, #7033, #20638, #35859, #11134, #12374, #47904, #20269, #68663, #14179, #34656, #10420, #2262, #36525, #59610, #24846, #54630, #64763 ) ) ;
#52892 = EDGE_CURVE ( 'NONE', #28725, #34946, #29366, .T. ) ;
#52893 = ORIENTED_EDGE ( 'NONE', *, *, #49203, .T. ) ;
#52894 = EDGE_CURVE ( 'NONE', #22289, #45362, #2499, .T. ) ;
#52895 = ADVANCED_FACE ( 'NONE', ( #24429 ), #56937, .T. ) ;
#52896 = LINE ( 'NONE', #57817, #30942 ) ;
#52897 = CARTESIAN_POINT ( 'NONE',  ( 151.5599459900709860, 0.000000000000000000, 282.8454385697650082 ) ) ;
#52898 = LINE ( 'NONE', #16091, #6563 ) ;
#52899 = ADVANCED_FACE ( 'NONE', ( #17728 ), #10720, .T. ) ;
#52900 = EDGE_LOOP ( 'NONE', ( #38532, #3677, #13548, #40295 ) ) ;
#52901 = ORIENTED_EDGE ( 'NONE', *, *, #37842, .F. ) ;
#52902 = DIRECTION ( 'NONE',  ( 0.000000000000000000, 0.000000000000000000, -1.000000000000000000 ) ) ;
#52903 = CARTESIAN_POINT ( 'NONE',  ( -11.77351654964679284, -7.826483450353365789, 455.0000000000000568 ) ) ;
#52904 = VERTEX_POINT ( 'NONE', #47045 ) ;
#52905 = ORIENTED_EDGE ( 'NONE', *, *, #59288, .F. ) ;
#52906 = ORIENTED_EDGE ( 'NONE', *, *, #13366, .T. ) ;
#52907 = VERTEX_POINT ( 'NONE', #58708 ) ;
#52908 = CARTESIAN_POINT ( 'NONE',  ( 7.250000000000005329, 7.250000000000000888, -13.50000000000000178 ) ) ;
#52909 = UNCERTAINTY_MEASURE_WITH_UNIT (LENGTH_MEASURE( 1.000000000000000082E-05 ), #33960, 'distance_accuracy_value', 'NONE');
#52911 = ORIENTED_EDGE ( 'NONE', *, *, #57016, .F. ) ;
#52910 = LINE ( 'NONE', #4114, #59352 ) ;
#52912 = AXIS2_PLACEMENT_3D ( 'NONE', #4943, #48076, #36411 ) ;
#52913 = CARTESIAN_POINT ( 'NONE',  ( 8.250000000000005329, -7.249999999999998224, -14.50000000000000000 ) ) ;
#52914 = CARTESIAN_POINT ( 'NONE',  ( -4.135079735113167843, 6.822336235477362010, 54.00000000000000711 ) ) ;
#52915 = DIRECTION ( 'NONE',  ( -0.000000000000000000, -0.000000000000000000, -1.000000000000000000 ) ) ;
#52916 = VERTEX_POINT ( 'NONE', #41384 ) ;
#52917 = ORIENTED_EDGE ( 'NONE', *, *, #50935, .F. ) ;
#52918 = AXIS2_PLACEMENT_3D ( 'NONE', #9141, #3830, #45915 ) ;
#52919 = DIRECTION ( 'NONE',  ( -1.000000000000000000, 0.000000000000000000, 0.000000000000000000 ) ) ;
#52920 = DIRECTION ( 'NONE',  ( -0.000000000000000000, -0.000000000000000000, -1.000000000000000000 ) ) ;
#52921 = VERTEX_POINT ( 'NONE', #4621 ) ;
#52922 = VECTOR ( 'NONE', #658, 1000.000000000000114 ) ;
#52923 = EDGE_CURVE ( 'NONE', #22860, #10855, #12909, .T. ) ;
#52924 = DIRECTION ( 'NONE',  ( 1.000000000000000000, -8.339399738404101090E-15, 0.000000000000000000 ) ) ;
#52925 = CARTESIAN_POINT ( 'NONE',  ( 25.90000000000000213, -0.2000000000089119934, -8.913009219568841313E-12 ) ) ;
#52926 = DIRECTION ( 'NONE',  ( -1.000000000000000000, 0.000000000000000000, 0.000000000000000000 ) ) ;
#52927 = ORIENTED_EDGE ( 'NONE', *, *, #34876, .T. ) ;
#52928 = EDGE_CURVE ( 'NONE', #41344, #520, #58370, .T. ) ;
#52929 = DIRECTION ( 'NONE',  ( -0.8660254037844400399, -0.4999999999999973910, 6.723777587268495961E-17 ) ) ;
#52930 = DIRECTION ( 'NONE',  ( -1.000000000000000000, 1.047444401652940007E-14, -1.836970198721010952E-16 ) ) ;
#52931 = ADVANCED_FACE ( 'NONE', ( #64028 ), #52719, .F. ) ;
#52932 = CARTESIAN_POINT ( 'NONE',  ( 39.90000000000000568, -21.00000000000000000, 13.86939075806900057 ) ) ;
#52933 = DIRECTION ( 'NONE',  ( 0.000000000000000000, 0.000000000000000000, 1.000000000000000000 ) ) ;
#52934 = EDGE_CURVE ( 'NONE', #41126, #67437, #42434, .T. ) ;
#52935 = DIRECTION ( 'NONE',  ( 0.000000000000000000, -0.6857142857147903170, -0.7278708115913530285 ) ) ;
#52936 = ORIENTED_EDGE ( 'NONE', *, *, #54726, .F. ) ;
#52937 = CARTESIAN_POINT ( 'NONE',  ( 15.00000000000000000, -21.00000000000000000, 0.000000000000000000 ) ) ;
#52938 = CARTESIAN_POINT ( 'NONE',  ( -11.00000000000000000, -9.454754784057099570, 17.53999999999999915 ) ) ;
#52939 = DIRECTION ( 'NONE',  ( 1.000000000000000000, 7.751221965937476285E-17, -0.000000000000000000 ) ) ;
#52940 = LINE ( 'NONE', #31000, #46978 ) ;
#52941 = ORIENTED_EDGE ( 'NONE', *, *, #25872, .F. ) ;
#52942 = DIRECTION ( 'NONE',  ( -1.000000000000000000, 0.000000000000000000, 0.000000000000000000 ) ) ;
#52943 = CARTESIAN_POINT ( 'NONE',  ( -3.663616288757055806, 4.135079735113128763, 54.00000000000000711 ) ) ;
#52944 = CARTESIAN_POINT ( 'NONE',  ( 0.000000000000000000, 0.000000000000000000, -16.50000000000000000 ) ) ;
#52945 = CARTESIAN_POINT ( 'NONE',  ( -2.752095193409509033, -9.955011587777317317, 455.0000000000000568 ) ) ;
#52946 = VERTEX_POINT ( 'NONE', #68619 ) ;
#52947 = CARTESIAN_POINT ( 'NONE',  ( 290.0000000000000000, -42.00000000000000000, -26.50000000000000000 ) ) ;
#52948 = DIRECTION ( 'NONE',  ( 0.000000000000000000, -1.000000000000000000, 0.000000000000000000 ) ) ;
#52949 = DIRECTION ( 'NONE',  ( 1.836970198721029934E-16, 1.836970198721010706E-16, -1.000000000000000000 ) ) ;
#52950 = CARTESIAN_POINT ( 'NONE',  ( 283.0000000000000568, -32.95000000000000284, -13.19999999999999929 ) ) ;
#52951 = DIRECTION ( 'NONE',  ( -1.000000000000000000, 0.000000000000000000, 0.000000000000000000 ) ) ;
#52952 = VERTEX_POINT ( 'NONE', #62962 ) ;
#52953 = ORIENTED_EDGE ( 'NONE', *, *, #20583, .T. ) ;
#52954 = CARTESIAN_POINT ( 'NONE',  ( 7.000000000000000000, -32.95000000000000284, -7.700000000000000178 ) ) ;
#52955 = CARTESIAN_POINT ( 'NONE',  ( -15.29686605391142606, -0.2715358723588648937, 23.82609623451821079 ) ) ;
#52956 = EDGE_LOOP ( 'NONE', ( #54411, #36590, #38589, #57765, #15283, #67023, #40959, #7989 ) ) ;
#52957 = CYLINDRICAL_SURFACE ( 'NONE', #46115, 3.499999999999999556 ) ;
#52958 = VECTOR ( 'NONE', #20292, 1000.000000000000000 ) ;
#52959 = CARTESIAN_POINT ( 'NONE',  ( 15.50000000000000000, -1.037157890325000054, 18.50000000000000000 ) ) ;
#52960 = ORIENTED_EDGE ( 'NONE', *, *, #44659, .T. ) ;
#52961 = AXIS2_PLACEMENT_3D ( 'NONE', #20148, #41709, #63284 ) ;
#52962 = FACE_OUTER_BOUND ( 'NONE', #21335, .T. ) ;
#52963 = VERTEX_POINT ( 'NONE', #57997 ) ;
#52964 = VERTEX_POINT ( 'NONE', #9218 ) ;
#52965 = CARTESIAN_POINT ( 'NONE',  ( -8.393516549646712122, 7.603567055985436696, 195.0000000000000284 ) ) ;
#52966 = EDGE_CURVE ( 'NONE', #66065, #54243, #61466, .T. ) ;
#52967 = ORIENTED_EDGE ( 'NONE', *, *, #7151, .T. ) ;
#52968 = EDGE_CURVE ( 'NONE', #13636, #34259, #24778, .T. ) ;
#52970 = AXIS2_PLACEMENT_3D ( 'NONE', #65180, #3407, #10036 ) ;
#52969 = AXIS2_PLACEMENT_3D ( 'NONE', #5958, #5617, #309 ) ;
#52971 = DIRECTION ( 'NONE',  ( -1.836970198721029934E-16, -1.836970198721010706E-16, 1.000000000000000000 ) ) ;
#52972 = DIRECTION ( 'NONE',  ( 1.000000000000000000, 0.000000000000000000, 0.000000000000000000 ) ) ;
#52973 = LINE ( 'NONE', #6843, #32163 ) ;
#52974 = EDGE_CURVE ( 'NONE', #33597, #65210, #35533, .T. ) ;
#52975 = EDGE_CURVE ( 'NONE', #15576, #58661, #25353, .T. ) ;
#52976 = ORIENTED_EDGE ( 'NONE', *, *, #4604, .T. ) ;
#52977 = DIRECTION ( 'NONE',  ( -1.000000000000000000, 3.491481338843132961E-15, 1.836970198721036344E-16 ) ) ;
#52980 = CARTESIAN_POINT ( 'NONE',  ( 25.90000000000000213, -14.06939075806900874, 20.80000000000001137 ) ) ;
#52979 = DIRECTION ( 'NONE',  ( 0.000000000000000000, 0.000000000000000000, -1.000000000000000000 ) ) ;
#52978 = CIRCLE ( 'NONE', #1035, 0.5249999999999994671 ) ;
#52981 = ORIENTED_EDGE ( 'NONE', *, *, #13480, .T. ) ;
#52982 = VERTEX_POINT ( 'NONE', #51653 ) ;
#52983 = ORIENTED_EDGE ( 'NONE', *, *, #67652, .F. ) ;
#52984 = PRODUCT_DEFINITION ( 'UNKNOWN', '', #883, #60760 ) ;
#52985 = EDGE_LOOP ( 'NONE', ( #12189, #58366, #67530, #45614 ) ) ;
#52986 = EDGE_CURVE ( 'NONE', #63705, #38341, #31494, .T. ) ;
#52987 = LINE ( 'NONE', #37755, #58193 ) ;
#52988 = ADVANCED_FACE ( 'NONE', ( #57649 ), #57298, .F. ) ;
#52990 = ORIENTED_EDGE ( 'NONE', *, *, #42043, .T. ) ;
#52989 = CARTESIAN_POINT ( 'NONE',  ( 283.0000000000000568, -23.65000000000000568, -12.40000000000000213 ) ) ;
#52991 = DIRECTION ( 'NONE',  ( -1.000000000000000000, 0.000000000000000000, 0.000000000000000000 ) ) ;
#52992 = CARTESIAN_POINT ( 'NONE',  ( 10.00000000000000000, -18.00000000000000355, -21.00000000000000000 ) ) ;
#52993 = ORIENTED_EDGE ( 'NONE', *, *, #50777, .T. ) ;
#52994 = ORIENTED_EDGE ( 'NONE', *, *, #45749, .T. ) ;
#52995 = CARTESIAN_POINT ( 'NONE',  ( 34.89999999999999858, 0.000000000000000000, 2.458500000000000796 ) ) ;
#52996 = ORIENTED_EDGE ( 'NONE', *, *, #57344, .F. ) ;
#52997 = VECTOR ( 'NONE', #18495, 1000.000000000000000 ) ;
#52998 = DIRECTION ( 'NONE',  ( 0.000000000000000000, 0.000000000000000000, 1.000000000000000000 ) ) ;
#52999 = CARTESIAN_POINT ( 'NONE',  ( 7.000000000000000000, -42.50000000000000000, 9.700000000000002842 ) ) ;
#53000 = CARTESIAN_POINT ( 'NONE',  ( 41.09999999999999432, 20.60000000000000142, -13.86939075806900057 ) ) ;
#53001 = ORIENTED_EDGE ( 'NONE', *, *, #63111, .F. ) ;
#53002 = CIRCLE ( 'NONE', #22505, 0.1999999999999987899 ) ;
#53003 = CARTESIAN_POINT ( 'NONE',  ( -15.50000000000000000, -0.4000000000005236034, 22.50000000000000000 ) ) ;
#53004 = DIRECTION ( 'NONE',  ( 0.000000000000000000, 0.000000000000000000, -1.000000000000000000 ) ) ;
#53006 = EDGE_LOOP ( 'NONE', ( #19258, #52483 ) ) ;
#53005 = SURFACE_STYLE_USAGE ( .BOTH. , #47683 ) ;
#53008 = VERTEX_POINT ( 'NONE', #42083 ) ;
#53007 = DIRECTION ( 'NONE',  ( -2.135044278125299371E-15, -1.000000000000000000, -3.673940397442060361E-16 ) ) ;
#53009 = CARTESIAN_POINT ( 'NONE',  ( 0.5000000000000000000, 21.00000000000000000, 18.00000000000000355 ) ) ;
#53010 = VECTOR ( 'NONE', #20558, 1000.000000000000000 ) ;
#53011 = CYLINDRICAL_SURFACE ( 'NONE', #8131, 0.1749999999999998224 ) ;
#53012 = DIRECTION ( 'NONE',  ( 0.7071067811865474617, 0.7071067811865474617, 2.597868168706479611E-16 ) ) ;
#53013 = DIRECTION ( 'NONE',  ( -1.836970198721029934E-16, -1.836970198721010706E-16, 1.000000000000000000 ) ) ;
#53014 = EDGE_CURVE ( 'NONE', #69896, #58380, #19733, .T. ) ;
#53015 = AXIS2_PLACEMENT_3D ( 'NONE', #56103, #67422, #7654 ) ;
#53016 = DIRECTION ( 'NONE',  ( -0.000000000000000000, 3.673940397442059868E-16, -1.000000000000000000 ) ) ;
#53017 = VERTEX_POINT ( 'NONE', #30430 ) ;
#53018 = DIRECTION ( 'NONE',  ( 0.000000000000000000, 1.000000000000000000, 0.000000000000000000 ) ) ;
#53019 = DIRECTION ( 'NONE',  ( 1.000000000000000000, -5.981805089575196197E-17, 0.000000000000000000 ) ) ;
#53020 = DIRECTION ( 'NONE',  ( -0.000000000000000000, -0.000000000000000000, -1.000000000000000000 ) ) ;
#53021 = VECTOR ( 'NONE', #69875, 1000.000000000000114 ) ;
#53023 = ORIENTED_EDGE ( 'NONE', *, *, #44047, .T. ) ;
#53022 = LINE ( 'NONE', #15182, #8506 ) ;
#53024 = DIRECTION ( 'NONE',  ( -1.000000000000000000, 0.000000000000000000, 0.000000000000000000 ) ) ;
#53025 = CARTESIAN_POINT ( 'NONE',  ( 4.149127210878741145, 3.663616288756999406, 54.00000000000000711 ) ) ;
#53026 = FACE_OUTER_BOUND ( 'NONE', #57280, .T. ) ;
#53027 = EDGE_CURVE ( 'NONE', #35617, #40989, #36658, .T. ) ;
#53028 = CARTESIAN_POINT ( 'NONE',  ( 8.406483450353384512, 4.383466043307721272, 455.0000000000000568 ) ) ;
#53029 = VERTEX_POINT ( 'NONE', #14872 ) ;
#53030 = DIRECTION ( 'NONE',  ( 0.000000000000000000, 0.7071067811865455743, 0.7071067811865495711 ) ) ;
#53031 = CARTESIAN_POINT ( 'NONE',  ( -11.00000000000000000, -9.487228132326899654, 12.50000000000000000 ) ) ;
#53032 = ORIENTED_EDGE ( 'NONE', *, *, #6570, .T. ) ;
#53033 = DIRECTION ( 'NONE',  ( 1.000000000000000000, -0.000000000000000000, 0.000000000000000000 ) ) ;
#53034 = DIRECTION ( 'NONE',  ( 1.000000000000000000, -0.000000000000000000, -0.000000000000000000 ) ) ;
#53035 = SHAPE_REPRESENTATION ( 'Mounting Feet', ( #45918 ), #64023 ) ;
#53036 = EDGE_CURVE ( 'NONE', #42264, #55585, #37144, .T. ) ;
#53037 = DIRECTION ( 'NONE',  ( -1.000000000000000000, 0.000000000000000000, 0.000000000000000000 ) ) ;
#53038 = CARTESIAN_POINT ( 'NONE',  ( 11.50000000000000000, -12.00000000000000000, 10.52786404500095863 ) ) ;
#53039 = ORIENTED_EDGE ( 'NONE', *, *, #25074, .F. ) ;
#53040 = ORIENTED_EDGE ( 'NONE', *, *, #32523, .T. ) ;
#53041 = CARTESIAN_POINT ( 'NONE',  ( 6.501044194225490180, -3.157023737882824754, 54.00000000000000711 ) ) ;
#53042 = VECTOR ( 'NONE', #9226, 1000.000000000000000 ) ;
#53043 = EDGE_LOOP ( 'NONE', ( #46235, #19458, #6611, #24084, #54699, #63658, #12648, #28182, #30094, #31324, #48452 ) ) ;
#53044 = ORIENTED_EDGE ( 'NONE', *, *, #65392, .F. ) ;
#53045 = CARTESIAN_POINT ( 'NONE',  ( 275.0000000000000000, -25.60000000000000142, 15.10000000000000142 ) ) ;
#53046 = EDGE_CURVE ( 'NONE', #39509, #35023, #4277, .T. ) ;
#53047 = CARTESIAN_POINT ( 'NONE',  ( 47.00000000000000000, 0.000000000000000000, 5.000000000000000000 ) ) ;
#53048 = CYLINDRICAL_SURFACE ( 'NONE', #40025, 4.000000000000000000 ) ;
#53049 = ORIENTED_EDGE ( 'NONE', *, *, #39745, .F. ) ;
#53050 = VERTEX_POINT ( 'NONE', #63669 ) ;
#53051 = DIRECTION ( 'NONE',  ( -0.8660254037844435926, -0.4999999999999913403, 0.000000000000000000 ) ) ;
#53052 = CIRCLE ( 'NONE', #29280, 0.1749999999999980738 ) ;
#53053 = ORIENTED_EDGE ( 'NONE', *, *, #36276, .T. ) ;
#53054 = VECTOR ( 'NONE', #54094, 1000.000000000000114 ) ;
#53055 = VERTEX_POINT ( 'NONE', #15225 ) ;
#53056 = EDGE_CURVE ( 'NONE', #25235, #29129, #40014, .T. ) ;
#53057 = CARTESIAN_POINT ( 'NONE',  ( 290.0000000000000000, -0.5000000000000000000, 26.50000000000000000 ) ) ;
#53058 = LINE ( 'NONE', #4616, #65183 ) ;
#53059 = LINE ( 'NONE', #36427, #67068 ) ;
#53060 = ADVANCED_FACE ( 'NONE', ( #21567 ), #15918, .T. ) ;
#53061 = ADVANCED_FACE ( 'NONE', ( #59048 ), #32540, .F. ) ;
#53062 = ORIENTED_EDGE ( 'NONE', *, *, #25621, .T. ) ;
#53063 = AXIS2_PLACEMENT_3D ( 'NONE', #31881, #54141, #53446 ) ;
#53064 = CYLINDRICAL_SURFACE ( 'NONE', #58310, 0.3999999999993835154 ) ;
#53066 = CARTESIAN_POINT ( 'NONE',  ( 7.450000000000006395, 7.250000000000000888, -8.500000000000000000 ) ) ;
#53065 = CARTESIAN_POINT ( 'NONE',  ( 0.000000000000000000, 0.000000000000000000, 0.000000000000000000 ) ) ;
#53067 = EDGE_LOOP ( 'NONE', ( #6453, #37358, #59993, #24560 ) ) ;
#53070 = ORIENTED_EDGE ( 'NONE', *, *, #45311, .T. ) ;
#53069 = EDGE_CURVE ( 'NONE', #14810, #30263, #43414, .T. ) ;
#53068 = LINE ( 'NONE', #68966, #49991 ) ;
#53071 = VERTEX_POINT ( 'NONE', #37489 ) ;
#53072 = VECTOR ( 'NONE', #23354, 1000.000000000000114 ) ;
#53073 = EDGE_CURVE ( 'NONE', #61999, #21563, #4960, .T. ) ;
#53074 = CARTESIAN_POINT ( 'NONE',  ( 5.552858015815571591, 7.342976262117199227, 54.00000000000000711 ) ) ;
#53075 = EDGE_CURVE ( 'NONE', #29966, #42141, #27916, .T. ) ;
#53076 = AXIS2_PLACEMENT_3D ( 'NONE', #5724, #64090, #59803 ) ;
#53077 = DIRECTION ( 'NONE',  ( 0.000000000000000000, 0.000000000000000000, 1.000000000000000000 ) ) ;
#53078 = ORIENTED_EDGE ( 'NONE', *, *, #66398, .F. ) ;
#53079 = VECTOR ( 'NONE', #14783, 1000.000000000000000 ) ;
#53080 = CARTESIAN_POINT ( 'NONE',  ( 7.000000000000000000, -32.45000000000000995, 12.69999999999999929 ) ) ;
#53081 = CARTESIAN_POINT ( 'NONE',  ( 283.0000000000000568, -32.95000000000000284, 14.50000000000000000 ) ) ;
#53082 = EDGE_CURVE ( 'NONE', #57476, #50581, #28496, .T. ) ;
#53083 = ORIENTED_EDGE ( 'NONE', *, *, #3178, .F. ) ;
#53084 = ORIENTED_EDGE ( 'NONE', *, *, #18629, .T. ) ;
#53085 = DIRECTION ( 'NONE',  ( -1.000000000000000000, 0.000000000000000000, 0.000000000000000000 ) ) ;
#53086 = DIRECTION ( 'NONE',  ( 1.000000000000000000, -0.000000000000000000, -0.000000000000000000 ) ) ;
#53087 = EDGE_LOOP ( 'NONE', ( #7991, #63112, #51651, #45327 ) ) ;
#53088 = CARTESIAN_POINT ( 'NONE',  ( 11.50000000000000000, -11.50000000000100009, -15.00000000000084910 ) ) ;
#53089 = VECTOR ( 'NONE', #52183, 1000.000000000000000 ) ;
#53090 = EDGE_CURVE ( 'NONE', #18754, #67430, #63780, .T. ) ;
#53091 = DIRECTION ( 'NONE',  ( -2.135044278125299371E-15, -1.000000000000000000, 0.000000000000000000 ) ) ;
#53093 = ORIENTED_EDGE ( 'NONE', *, *, #56457, .T. ) ;
#53092 = FILL_AREA_STYLE_COLOUR ( '', #39685 ) ;
#53095 = ORIENTED_EDGE ( 'NONE', *, *, #45853, .F. ) ;
#53094 = CARTESIAN_POINT ( 'NONE',  ( 15.50000000000000000, -0.4000000000000000222, -22.50000000000000000 ) ) ;
#53096 = DIRECTION ( 'NONE',  ( 1.053224967557347660E-14, 1.000000000000000000, 0.000000000000000000 ) ) ;
#53097 = LINE ( 'NONE', #14544, #64590 ) ;
#53098 = DIRECTION ( 'NONE',  ( 0.000000000000000000, -1.000000000000000000, 0.000000000000000000 ) ) ;
#53099 = CARTESIAN_POINT ( 'NONE',  ( 9.690000000000001279, 9.690000000000001279, -4.250000000000000000 ) ) ;
#53100 = EDGE_CURVE ( 'NONE', #67710, #1557, #5998, .T. ) ;
#53101 = CARTESIAN_POINT ( 'NONE',  ( 49.00000000000000000, -14.06939075806900163, -20.80000000000000426 ) ) ;
#53102 = CARTESIAN_POINT ( 'NONE',  ( 12.90000000000000213, 0.000000000000000000, 4.309871990004491277E-16 ) ) ;
#53103 = ORIENTED_EDGE ( 'NONE', *, *, #23655, .T. ) ;
#53104 = CARTESIAN_POINT ( 'NONE',  ( 7.450000000000006395, 7.250000000000000888, -16.50000000000000000 ) ) ;
#53105 = VECTOR ( 'NONE', #15732, 1000.000000000000000 ) ;
#53106 = AXIS2_PLACEMENT_3D ( 'NONE', #30692, #42689, #46585 ) ;
#53107 = ADVANCED_FACE ( 'NONE', ( #38192 ), #16959, .F. ) ;
#53109 = ORIENTED_EDGE ( 'NONE', *, *, #38200, .F. ) ;
#53108 = SURFACE_SIDE_STYLE ('',( #15264 ) ) ;
#53110 = CARTESIAN_POINT ( 'NONE',  ( -11.11351654964670743, 9.093516549646603053, 195.0000000000000284 ) ) ;
#53111 = VECTOR ( 'NONE', #21105, 1000.000000000000000 ) ;
#53112 = DIRECTION ( 'NONE',  ( -0.000000000000000000, -0.000000000000000000, -1.000000000000000000 ) ) ;
#53113 = EDGE_CURVE ( 'NONE', #3391, #6834, #49132, .T. ) ;
#53114 = CARTESIAN_POINT ( 'NONE',  ( -5.993516549646711766, 8.198316549646602169, 455.0000000000000568 ) ) ;
#53115 = CIRCLE ( 'NONE', #63234, 0.9999999999999991118 ) ;
#53116 = ORIENTED_EDGE ( 'NONE', *, *, #5618, .T. ) ;
#53117 = CYLINDRICAL_SURFACE ( 'NONE', #61344, 0.2999999999998732569 ) ;
#53118 = DIRECTION ( 'NONE',  ( 0.000000000000000000, 0.000000000000000000, -1.000000000000000000 ) ) ;
#53119 = ORIENTED_EDGE ( 'NONE', *, *, #49828, .F. ) ;
#53120 = VECTOR ( 'NONE', #37806, 1000.000000000000000 ) ;
#53121 = PLANE ( 'NONE',  #57171 ) ;
#53122 = EDGE_CURVE ( 'NONE', #69832, #33868, #48790, .T. ) ;
#53123 = AXIS2_PLACEMENT_3D ( 'NONE', #38704, #19923, #25595 ) ;
#53124 = VECTOR ( 'NONE', #14136, 1000.000000000000000 ) ;
#53125 = CARTESIAN_POINT ( 'NONE',  ( 6.836383711242975281, 4.135079735113102117, 54.00000000000000711 ) ) ;
#53126 = VERTEX_POINT ( 'NONE', #10602 ) ;
#53127 = FACE_OUTER_BOUND ( 'NONE', #5679, .T. ) ;
#53128 = VERTEX_POINT ( 'NONE', #21234 ) ;
#53129 = ADVANCED_FACE ( 'NONE', ( #64359 ), #17288, .F. ) ;
#53130 = VERTEX_POINT ( 'NONE', #43124 ) ;
#53131 = EDGE_CURVE ( 'NONE', #17252, #2339, #21909, .T. ) ;
#53132 = DIRECTION ( 'NONE',  ( -0.7071067811865514585, -0.7071067811865435759, -2.597868168706465806E-16 ) ) ;
#53133 = CIRCLE ( 'NONE', #32763, 0.4999999999979551912 ) ;
#53134 = DIRECTION ( 'NONE',  ( 0.000000000000000000, 1.000000000000000000, 0.000000000000000000 ) ) ;
#53135 = VECTOR ( 'NONE', #24955, 1000.000000000000000 ) ;
#53136 = EDGE_CURVE ( 'NONE', #9829, #29192, #64697, .T. ) ;
#53137 = EDGE_CURVE ( 'NONE', #14914, #28218, #3913, .T. ) ;
#53138 = EDGE_CURVE ( 'NONE', #31731, #60141, #18574, .T. ) ;
#53139 = CARTESIAN_POINT ( 'NONE',  ( -7.450000000000001954, -7.249999999999998224, -21.50000000000000000 ) ) ;
#53140 = DIRECTION ( 'NONE',  ( -0.000000000000000000, -0.000000000000000000, -1.000000000000000000 ) ) ;
#53141 = ORIENTED_EDGE ( 'NONE', *, *, #18502, .T. ) ;
#53142 = VERTEX_POINT ( 'NONE', #11969 ) ;
#53144 = ORIENTED_EDGE ( 'NONE', *, *, #34771, .F. ) ;
#53143 = CARTESIAN_POINT ( 'NONE',  ( -5.380658396643233310, 7.252248008019342329, 195.0000000000000284 ) ) ;
#53145 = EDGE_CURVE ( 'NONE', #57228, #38183, #6678, .T. ) ;
#53146 = EDGE_LOOP ( 'NONE', ( #3879, #69449, #13868, #44377 ) ) ;
#53147 = DIRECTION ( 'NONE',  ( 1.000000000000000000, 0.000000000000000000, 0.000000000000000000 ) ) ;
#53148 = DIRECTION ( 'NONE',  ( -0.000000000000000000, -0.000000000000000000, 1.000000000000000000 ) ) ;
#53149 = VECTOR ( 'NONE', #20964, 1000.000000000000000 ) ;
#53150 = ADVANCED_FACE ( 'NONE', ( #24338 ), #49818, .F. ) ;
#53151 = FACE_OUTER_BOUND ( 'NONE', #24829, .T. ) ;
#53152 = ADVANCED_FACE ( 'NONE', ( #61104 ), #67115, .F. ) ;
#53153 = DIRECTION ( 'NONE',  ( 0.7071067811865348052, -0.7071067811865602293, -3.278703137324831017E-30 ) ) ;
#53155 = CARTESIAN_POINT ( 'NONE',  ( 11.32648345035337734, -4.406483450353395170, 195.0000000000000284 ) ) ;
#53154 = DIRECTION ( 'NONE',  ( 1.000000000000000000, -0.000000000000000000, 0.000000000000000000 ) ) ;
#53156 = ORIENTED_EDGE ( 'NONE', *, *, #48335, .F. ) ;
#53157 = VERTEX_POINT ( 'NONE', #1381 ) ;
#53158 = VERTEX_POINT ( 'NONE', #33891 ) ;
#53159 = LINE ( 'NONE', #68353, #51378 ) ;
#53160 = EDGE_CURVE ( 'NONE', #66073, #67897, #33556, .T. ) ;
#53161 = DIRECTION ( 'NONE',  ( 0.000000000000000000, -1.000000000000000000, 0.000000000000000000 ) ) ;
#53163 = ADVANCED_FACE ( 'NONE', ( #18316 ), #34925, .F. ) ;
#53162 = DIRECTION ( 'NONE',  ( 1.000000000000000000, 0.000000000000000000, 0.000000000000000000 ) ) ;
#53164 = DIRECTION ( 'NONE',  ( -1.819560449471430698E-15, -1.000000000000000000, 0.000000000000000000 ) ) ;
#53165 = VECTOR ( 'NONE', #36576, 1000.000000000000000 ) ;
#53166 = ORIENTED_EDGE ( 'NONE', *, *, #2012, .F. ) ;
#53167 = EDGE_LOOP ( 'NONE', ( #38168, #25057, #49046, #63473 ) ) ;
#53168 = ORIENTED_EDGE ( 'NONE', *, *, #57607, .T. ) ;
#53169 = VECTOR ( 'NONE', #14737, 1000.000000000000000 ) ;
#53170 = CARTESIAN_POINT ( 'NONE',  ( 10.00000000000000000, 21.00000000000000000, 18.00000000000000355 ) ) ;
#53171 = EDGE_LOOP ( 'NONE', ( #20112, #32899, #39184, #38880 ) ) ;
#53172 = LINE ( 'NONE', #69412, #5155 ) ;
#53173 = ORIENTED_EDGE ( 'NONE', *, *, #32301, .F. ) ;
#53174 = VECTOR ( 'NONE', #13616, 1000.000000000000000 ) ;
#53175 = ORIENTED_EDGE ( 'NONE', *, *, #47138, .T. ) ;
#53176 = CARTESIAN_POINT ( 'NONE',  ( -8.393516549646712122, 5.655420232009161552, 455.0000000000000568 ) ) ;
#53178 = EDGE_LOOP ( 'NONE', ( #27926, #49887, #36897, #57367 ) ) ;
#53177 = LINE ( 'NONE', #53870, #18700 ) ;
#53179 = ORIENTED_EDGE ( 'NONE', *, *, #52189, .T. ) ;
#53180 = DIRECTION ( 'NONE',  ( 1.836970198721029934E-16, -1.836970198721036344E-16, 1.000000000000000000 ) ) ;
#53181 = PLANE ( 'NONE',  #11050 ) ;
#53183 = ORIENTED_EDGE ( 'NONE', *, *, #33066, .T. ) ;
#53182 = DIRECTION ( 'NONE',  ( 8.673617379884051249E-15, 1.000000000000000000, 0.000000000000000000 ) ) ;
#53184 = VERTEX_POINT ( 'NONE', #2760 ) ;
#53186 = LINE ( 'NONE', #4730, #18614 ) ;
#53185 = AXIS2_PLACEMENT_3D ( 'NONE', #12347, #54826, #6384 ) ;
#53187 = LINE ( 'NONE', #30200, #52650 ) ;
#53188 = DIRECTION ( 'NONE',  ( 0.000000000000000000, 0.000000000000000000, 1.000000000000000000 ) ) ;
#53189 = PLANE ( 'NONE',  #68493 ) ;
#53190 = EDGE_CURVE ( 'NONE', #19581, #27218, #50157, .T. ) ;
#53191 = FACE_OUTER_BOUND ( 'NONE', #19406, .T. ) ;
#53192 = ORIENTED_EDGE ( 'NONE', *, *, #39034, .F. ) ;
#53193 = FACE_BOUND ( 'NONE', #58991, .T. ) ;
#53194 = ADVANCED_FACE ( 'NONE', ( #56507 ), #1719, .F. ) ;
#53195 = VERTEX_POINT ( 'NONE', #66426 ) ;
#53196 = DIRECTION ( 'NONE',  ( -1.000000000000000000, 0.000000000000000000, 0.000000000000000000 ) ) ;
#53197 = CARTESIAN_POINT ( 'NONE',  ( 16.75000000000000355, -0.2715193793361441177, 22.98718409945082897 ) ) ;
#53198 = CIRCLE ( 'NONE', #1237, 2.250000000000001776 ) ;
#53200 = EDGE_CURVE ( 'NONE', #27591, #55844, #29628, .T. ) ;
#53199 = LINE ( 'NONE', #41864, #57330 ) ;
#53201 = PLANE ( 'NONE',  #31826 ) ;
#53202 = DIRECTION ( 'NONE',  ( 0.8660254037844482555, 0.000000000000000000, 0.4999999999999831801 ) ) ;
#53203 = ADVANCED_FACE ( 'NONE', ( #13011 ), #17974, .F. ) ;
#53204 = ORIENTED_EDGE ( 'NONE', *, *, #26705, .T. ) ;
#53205 = ADVANCED_FACE ( 'NONE', ( #55816 ), #39208, .T. ) ;
#53206 = VECTOR ( 'NONE', #8267, 1000.000000000000000 ) ;
#53207 = CARTESIAN_POINT ( 'NONE',  ( 7.265214908726139065, 5.380658396643097419, 455.0000000000000568 ) ) ;
#53208 = VECTOR ( 'NONE', #65760, 1000.000000000000000 ) ;
#53209 = DIRECTION ( 'NONE',  ( 0.000000000000000000, 0.000000000000000000, -1.000000000000000000 ) ) ;
#53210 = EDGE_LOOP ( 'NONE', ( #53629, #33036, #49254, #12713 ) ) ;
#53211 = DIRECTION ( 'NONE',  ( -0.7071067811865550112, -0.7071067811865401342, -2.597868168706467285E-16 ) ) ;
#53212 = FACE_OUTER_BOUND ( 'NONE', #34768, .T. ) ;
#53213 = CARTESIAN_POINT ( 'NONE',  ( -7.450000000000001954, 7.250000000000000000, -18.50000000000000000 ) ) ;
#53214 = VECTOR ( 'NONE', #14489, 1000.000000000000114 ) ;
#53215 = DIRECTION ( 'NONE',  ( 1.000000000000000000, 0.000000000000000000, 0.000000000000000000 ) ) ;
#53216 = DIRECTION ( 'NONE',  ( -0.000000000000000000, 0.000000000000000000, 1.000000000000000000 ) ) ;
#53217 = ORIENTED_EDGE ( 'NONE', *, *, #27337, .F. ) ;
#53218 = DIRECTION ( 'NONE',  ( 0.000000000000000000, 0.000000000000000000, -1.000000000000000000 ) ) ;
#53219 = FACE_OUTER_BOUND ( 'NONE', #9920, .T. ) ;
#53220 = CARTESIAN_POINT ( 'NONE',  ( 30.00000000000000000, -13.79999999999979998, 17.30000000000000071 ) ) ;
#53221 = AXIS2_PLACEMENT_3D ( 'NONE', #28395, #34042, #50318 ) ;
#53222 = EDGE_CURVE ( 'NONE', #25548, #53017, #50514, .T. ) ;
#53223 = CARTESIAN_POINT ( 'NONE',  ( -30.00000000000000000, -11.50000000000000000, -19.00000000000000000 ) ) ;
#53224 = FACE_OUTER_BOUND ( 'NONE', #42179, .T. ) ;
#53225 = ORIENTED_EDGE ( 'NONE', *, *, #22007, .F. ) ;
#53227 = ORIENTED_EDGE ( 'NONE', *, *, #17230, .T. ) ;
#53226 = DIRECTION ( 'NONE',  ( 0.000000000000000000, 0.000000000000000000, -1.000000000000000000 ) ) ;
#53228 = VECTOR ( 'NONE', #54607, 1000.000000000000000 ) ;
#53229 = DIRECTION ( 'NONE',  ( 1.000000000000000000, 0.000000000000000000, 0.000000000000000000 ) ) ;
#53230 = PLANE ( 'NONE',  #48199 ) ;
#53231 = CARTESIAN_POINT ( 'NONE',  ( 28.00000000000000000, -16.64230188589299786, 14.64519951917100116 ) ) ;
#53232 = ORIENTED_EDGE ( 'NONE', *, *, #61727, .T. ) ;
#53233 = AXIS2_PLACEMENT_3D ( 'NONE', #21178, #69619, #41681 ) ;
#53234 = DIRECTION ( 'NONE',  ( -1.000000000000000000, 0.000000000000000000, 0.000000000000000000 ) ) ;
#53235 = LINE ( 'NONE', #30948, #65707 ) ;
#53236 = VERTEX_POINT ( 'NONE', #2071 ) ;
#53237 = ORIENTED_EDGE ( 'NONE', *, *, #61679, .F. ) ;
#53238 = EDGE_LOOP ( 'NONE', ( #55667, #15357, #44173, #18553, #19023, #66752, #10531, #24249 ) ) ;
#53239 = ADVANCED_FACE ( 'NONE', ( #7711 ), #49621, .T. ) ;
#53240 = LINE ( 'NONE', #57466, #61385 ) ;
#53241 = DIRECTION ( 'NONE',  ( 1.000000000000000000, 0.000000000000000000, 0.000000000000000000 ) ) ;
#53243 = EDGE_CURVE ( 'NONE', #39690, #1158, #50846, .T. ) ;
#53242 = FACE_OUTER_BOUND ( 'NONE', #13900, .T. ) ;
#53244 = VECTOR ( 'NONE', #44344, 1000.000000000000000 ) ;
#53245 = ORIENTED_EDGE ( 'NONE', *, *, #42802, .F. ) ;
#53246 = ORIENTED_EDGE ( 'NONE', *, *, #4985, .T. ) ;
#53247 = DIRECTION ( 'NONE',  ( -1.047444401652940007E-14, -1.000000000000000000, -1.836970198721029934E-16 ) ) ;
#53248 = ORIENTED_EDGE ( 'NONE', *, *, #26258, .T. ) ;
#53249 = ORIENTED_EDGE ( 'NONE', *, *, #1322, .T. ) ;
#53250 = ORIENTED_EDGE ( 'NONE', *, *, #10275, .F. ) ;
#53251 = ORIENTED_EDGE ( 'NONE', *, *, #20212, .F. ) ;
#53252 = CARTESIAN_POINT ( 'NONE',  ( 8.689999999999999503, -8.750000000000000000, -7.000000000000000000 ) ) ;
#53253 = VECTOR ( 'NONE', #37956, 1000.000000000000114 ) ;
#53255 = ORIENTED_EDGE ( 'NONE', *, *, #69046, .T. ) ;
#53254 = DIRECTION ( 'NONE',  ( 0.000000000000000000, -1.000000000000000000, -1.838806884531994514E-12 ) ) ;
#53256 = CARTESIAN_POINT ( 'NONE',  ( 0.000000000000000000, -8.249999999999998224, -22.00000000000000000 ) ) ;
#53257 = CARTESIAN_POINT ( 'NONE',  ( -11.00000000000000000, -11.10796162543699950, 9.102987789146602893 ) ) ;
#53258 = LINE ( 'NONE', #15420, #67425 ) ;
#53259 = EDGE_LOOP ( 'NONE', ( #6858, #63876, #55607, #10584 ) ) ;
#53260 = VERTEX_POINT ( 'NONE', #40241 ) ;
#53261 = AXIS2_PLACEMENT_3D ( 'NONE', #4681, #26249, #64096 ) ;
#53262 = CLOSED_SHELL ( 'NONE', ( #59036, #32368, #30993, #17199, #30473, #50084, #61229, #34566, #2089, #48121, #1709, #52572 ) ) ;
#53263 = CARTESIAN_POINT ( 'NONE',  ( -8.750000000000001776, 0.000000000000000000, -26.00000000000001066 ) ) ;
#53264 = DIRECTION ( 'NONE',  ( -1.000000000000000000, 0.000000000000000000, 0.000000000000000000 ) ) ;
#53265 = ORIENTED_EDGE ( 'NONE', *, *, #60198, .F. ) ;
#53266 = AXIS2_PLACEMENT_3D ( 'NONE', #6077, #48514, #788 ) ;
#53267 = ADVANCED_FACE ( 'NONE', ( #61824 ), #13376, .T. ) ;
#53268 = PLANE ( 'NONE',  #10826 ) ;
#53269 = PLANE ( 'NONE',  #52812 ) ;
#53270 = FACE_OUTER_BOUND ( 'NONE', #65701, .T. ) ;
#53271 = ORIENTED_EDGE ( 'NONE', *, *, #18356, .T. ) ;
#53272 = DIRECTION ( 'NONE',  ( 0.000000000000000000, 1.000000000000000000, 0.000000000000000000 ) ) ;
#53274 = ADVANCED_FACE ( 'NONE', ( #13722 ), #52262, .F. ) ;
#53273 = CARTESIAN_POINT ( 'NONE',  ( -3.650476262117221093, 10.49297626211717116, 54.00000000000000711 ) ) ;
#53275 = CIRCLE ( 'NONE', #20502, 3.499999999999999556 ) ;
#53276 = CARTESIAN_POINT ( 'NONE',  ( 9.899999999999998579, 21.00000000000000355, 13.98999642601812354 ) ) ;
#53277 = DIRECTION ( 'NONE',  ( -1.000000000000000000, -2.135044278125301343E-15, 0.000000000000000000 ) ) ;
#53278 = EDGE_CURVE ( 'NONE', #61884, #33102, #31043, .T. ) ;
#53279 = EDGE_CURVE ( 'NONE', #8459, #34152, #14069, .T. ) ;
#53280 = DIRECTION ( 'NONE',  ( 2.135044278125299371E-15, -1.000000000000000000, -3.673940397442060361E-16 ) ) ;
#53282 = VERTEX_POINT ( 'NONE', #19714 ) ;
#53281 = EDGE_CURVE ( 'NONE', #43741, #57348, #40938, .T. ) ;
#53283 = CARTESIAN_POINT ( 'NONE',  ( 40.90000000000000568, -21.00000000000000000, -14.57806571531351914 ) ) ;
#53284 = ADVANCED_FACE ( 'NONE', ( #14442 ), #56850, .F. ) ;
#53285 = PLANE ( 'NONE',  #56505 ) ;
#53286 = DIRECTION ( 'NONE',  ( -1.920292680692490463E-14, -1.000000000000000000, -1.836970198721045958E-16 ) ) ;
#53287 = ADVANCED_FACE ( 'NONE', ( #29987 ), #68530, .F. ) ;
#53288 = ORIENTED_EDGE ( 'NONE', *, *, #34277, .T. ) ;
#53289 = CARTESIAN_POINT ( 'NONE',  ( 30.00000000000000000, -11.50000000000100009, -10.50000000000065903 ) ) ;
#53290 = CARTESIAN_POINT ( 'NONE',  ( 0.000000000000000000, -7.449999999999998401, -8.000000000000000000 ) ) ;
#53291 = DIRECTION ( 'NONE',  ( 1.000000000000000000, 0.000000000000000000, 0.000000000000000000 ) ) ;
#53292 = DIRECTION ( 'NONE',  ( -1.000000000000000000, 0.000000000000000000, 0.000000000000000000 ) ) ;
#53293 = ORIENTED_EDGE ( 'NONE', *, *, #18023, .T. ) ;
#53294 = DIRECTION ( 'NONE',  ( 0.000000000000000000, 0.000000000000000000, 1.000000000000000000 ) ) ;
#53295 = LINE ( 'NONE', #10832, #39638 ) ;
#53296 = FACE_OUTER_BOUND ( 'NONE', #4274, .T. ) ;
#53297 = DIRECTION ( 'NONE',  ( 0.8660254037844322683, -0.5000000000000111022, 6.723777587268230953E-17 ) ) ;
#53298 = LINE ( 'NONE', #10491, #59059 ) ;
#53299 = DIRECTION ( 'NONE',  ( -0.6414496315691645689, -0.7671651518152939886, -2.587583378555115478E-16 ) ) ;
#53300 = AXIS2_PLACEMENT_3D ( 'NONE', #43504, #11661, #44 ) ;
#53301 = VERTEX_POINT ( 'NONE', #69221 ) ;
#53302 = VECTOR ( 'NONE', #17671, 1000.000000000000000 ) ;
#53303 = VERTEX_POINT ( 'NONE', #41648 ) ;
#53304 = DIRECTION ( 'NONE',  ( 0.7071067811865451302, -0.7071067811865500152, -2.597868168706484541E-16 ) ) ;
#53305 = DIRECTION ( 'NONE',  ( -1.000000000000000000, -0.000000000000000000, -0.000000000000000000 ) ) ;
#53306 = ORIENTED_EDGE ( 'NONE', *, *, #37299, .F. ) ;
#53307 = LINE ( 'NONE', #67805, #10045 ) ;
#53308 = DIRECTION ( 'NONE',  ( 0.000000000000000000, 0.000000000000000000, -1.000000000000000000 ) ) ;
#53309 = EDGE_LOOP ( 'NONE', ( #65292, #1289, #14599, #36794 ) ) ;
#53310 = VECTOR ( 'NONE', #44392, 1000.000000000000000 ) ;
#53311 = CIRCLE ( 'NONE', #16053, 0.5249999999999990230 ) ;
#53312 = DIRECTION ( 'NONE',  ( 1.000000000000000000, -0.000000000000000000, 0.000000000000000000 ) ) ;
#53313 = EDGE_LOOP ( 'NONE', ( #45554, #7965, #10979, #38851 ) ) ;
#53314 = EDGE_LOOP ( 'NONE', ( #30533, #3805, #34205, #69041 ) ) ;
#53315 = CARTESIAN_POINT ( 'NONE',  ( 7.250000000000005329, 7.250000000000000888, -26.00000000000001066 ) ) ;
#53316 = VERTEX_POINT ( 'NONE', #20087 ) ;
#53317 = CARTESIAN_POINT ( 'NONE',  ( -7.250000000000001776, -7.249999999999998224, -19.00000000000000000 ) ) ;
#53319 = ADVANCED_FACE ( 'NONE', ( #3477, #25044 ), #8776, .T. ) ;
#53318 = LINE ( 'NONE', #57905, #64129 ) ;
#53320 = DIRECTION ( 'NONE',  ( 0.000000000000000000, 0.000000000000000000, 1.000000000000000000 ) ) ;
#53321 = ORIENTED_EDGE ( 'NONE', *, *, #54240, .F. ) ;
#53323 = EDGE_CURVE ( 'NONE', #2395, #61211, #36342, .T. ) ;
#53322 = ORIENTED_EDGE ( 'NONE', *, *, #37308, .T. ) ;
#53324 = LINE ( 'NONE', #68529, #23365 ) ;
#53325 = EDGE_CURVE ( 'NONE', #15713, #27791, #3129, .T. ) ;
#53326 = AXIS2_PLACEMENT_3D ( 'NONE', #58045, #8901, #67961 ) ;
#53328 = CARTESIAN_POINT ( 'NONE',  ( -17.00000000000000000, -17.50000000000000000, 15.70499999999969809 ) ) ;
#53327 = CARTESIAN_POINT ( 'NONE',  ( -11.47551654964678214, -11.08848345035328542, 195.0000000000000284 ) ) ;
#53329 = ORIENTED_EDGE ( 'NONE', *, *, #69231, .T. ) ;
#53330 = VERTEX_POINT ( 'NONE', #46591 ) ;
#53331 = ADVANCED_FACE ( 'NONE', ( #68877 ), #30343, .F. ) ;
#53333 = VERTEX_POINT ( 'NONE', #41999 ) ;
#53332 = CONTEXT_DEPENDENT_SHAPE_REPRESENTATION ( #6568, #31800 ) ;
#53334 = FACE_OUTER_BOUND ( 'NONE', #2229, .T. ) ;
#53336 = ORIENTED_EDGE ( 'NONE', *, *, #65097, .T. ) ;
#53335 = LINE ( 'NONE', #9484, #27483 ) ;
#53337 = LINE ( 'NONE', #10532, #8518 ) ;
#53338 = CYLINDRICAL_SURFACE ( 'NONE', #13635, 0.1999999999999987899 ) ;
#53339 = ORIENTED_EDGE ( 'NONE', *, *, #854, .T. ) ;
#53340 = VERTEX_POINT ( 'NONE', #36700 ) ;
#53341 = DIRECTION ( 'NONE',  ( 1.000000000000000000, 0.000000000000000000, 0.000000000000000000 ) ) ;
#53342 = VECTOR ( 'NONE', #48367, 1000.000000000000000 ) ;
#53343 = ORIENTED_EDGE ( 'NONE', *, *, #47070, .F. ) ;
#53344 = FACE_OUTER_BOUND ( 'NONE', #33586, .T. ) ;
#53345 = CARTESIAN_POINT ( 'NONE',  ( -7.450000000000001954, -7.249999999999998224, -10.50000000000000000 ) ) ;
#53346 = DIRECTION ( 'NONE',  ( 0.000000000000000000, 0.000000000000000000, 1.000000000000000000 ) ) ;
#53347 = VECTOR ( 'NONE', #21175, 1000.000000000000000 ) ;
#53348 = ORIENTED_EDGE ( 'NONE', *, *, #44517, .F. ) ;
#53349 = EDGE_CURVE ( 'NONE', #4233, #34215, #51914, .T. ) ;
#53350 =( LENGTH_UNIT ( ) NAMED_UNIT ( * ) SI_UNIT ( .MILLI., .METRE. ) );
#53351 = DIRECTION ( 'NONE',  ( 0.000000000000000000, 0.000000000000000000, 1.000000000000000000 ) ) ;
#53353 = ORIENTED_EDGE ( 'NONE', *, *, #13187, .F. ) ;
#53352 =( NAMED_UNIT ( * ) PLANE_ANGLE_UNIT ( ) SI_UNIT ( $, .RADIAN. ) );
#53354 = ORIENTED_EDGE ( 'NONE', *, *, #37438, .F. ) ;
#53355 = CARTESIAN_POINT ( 'NONE',  ( 36.90000000000000568, -0.2000000000089119934, 8.909539772616881237E-12 ) ) ;
#53356 = CARTESIAN_POINT ( 'NONE',  ( -17.00000000000000000, -17.50000000000000000, -15.70500000000000007 ) ) ;
#53357 = LINE ( 'NONE', #15867, #9866 ) ;
#53358 = CIRCLE ( 'NONE', #22847, 7.800000000000000711 ) ;
#53359 = DIRECTION ( 'NONE',  ( 1.000000000000000000, 0.000000000000000000, -0.000000000000000000 ) ) ;
#53360 = CARTESIAN_POINT ( 'NONE',  ( -6.817976262117321440, -9.737023737882781305, 26.00000000000000000 ) ) ;
#53361 = ORIENTED_EDGE ( 'NONE', *, *, #54622, .F. ) ;
#53362 = FACE_OUTER_BOUND ( 'NONE', #50257, .T. ) ;
#53363 = ADVANCED_FACE ( 'NONE', ( #30698 ), #3818, .F. ) ;
#53364 = CARTESIAN_POINT ( 'NONE',  ( 6.006483450353379716, -6.006483450353490738, 455.0000000000000568 ) ) ;
#53365 = DIRECTION ( 'NONE',  ( -6.508391731846281342E-15, -1.000000000000000000, -1.836970198721024757E-16 ) ) ;
#53367 = VERTEX_POINT ( 'NONE', #46948 ) ;
#53366 = LINE ( 'NONE', #21185, #2857 ) ;
#53368 = CARTESIAN_POINT ( 'NONE',  ( 30.00000000000000000, -16.28999999999710369, 15.00000000000794920 ) ) ;
#53369 = AXIS2_PLACEMENT_3D ( 'NONE', #53922, #32343, #6158 ) ;
#53370 = ADVANCED_FACE ( 'NONE', ( #4184, #25756 ), #19374, .T. ) ;
#53371 = DIRECTION ( 'NONE',  ( -1.000000000000000000, 0.000000000000000000, 0.000000000000000000 ) ) ;
#53372 = CARTESIAN_POINT ( 'NONE',  ( 49.00000000000000000, 13.66939075806899950, 20.80000000000000426 ) ) ;
#53373 = CIRCLE ( 'NONE', #38669, 0.4000000000000010214 ) ;
#53374 = DIRECTION ( 'NONE',  ( 0.000000000000000000, -0.9938079899998859545, 0.1111111111112941946 ) ) ;
#53375 = ORIENTED_EDGE ( 'NONE', *, *, #66956, .F. ) ;
#53376 = CARTESIAN_POINT ( 'NONE',  ( -7.250000000000000000, -7.449999999999998401, -20.50000000000000000 ) ) ;
#53377 = CARTESIAN_POINT ( 'NONE',  ( -4.609516549646752281, -3.606483450353441533, 455.0000000000000568 ) ) ;
#53378 = EDGE_LOOP ( 'NONE', ( #43792, #16542, #8311, #51964, #27550, #10581, #47938, #4921 ) ) ;
#53379 = CARTESIAN_POINT ( 'NONE',  ( -8.916576262117349216, -8.930623737882767088, 54.00000000000000711 ) ) ;
#53380 = CARTESIAN_POINT ( 'NONE',  ( -8.250000000000001776, -8.249999999999998224, -26.00000000000001066 ) ) ;
#53381 = CARTESIAN_POINT ( 'NONE',  ( 7.000000000000000000, -26.42999999999999972, -9.412893218813501051 ) ) ;
#53382 = DIRECTION ( 'NONE',  ( -0.000000000000000000, -0.000000000000000000, -1.000000000000000000 ) ) ;
#53384 = EDGE_CURVE ( 'NONE', #4139, #63093, #26099, .T. ) ;
#53383 = DIRECTION ( 'NONE',  ( 0.000000000000000000, 0.000000000000000000, -1.000000000000000000 ) ) ;
#53385 = AXIS2_PLACEMENT_3D ( 'NONE', #819, #22376, #60181 ) ;
#53386 = ORIENTED_EDGE ( 'NONE', *, *, #2032, .F. ) ;
#53387 = EDGE_LOOP ( 'NONE', ( #47450, #30064, #57662, #38236 ) ) ;
#53388 = DIRECTION ( 'NONE',  ( -0.7671651518153006499, -0.6414496315691565753, 0.000000000000000000 ) ) ;
#53389 = ORIENTED_EDGE ( 'NONE', *, *, #34813, .T. ) ;
#53390 = VERTEX_POINT ( 'NONE', #12161 ) ;
#53391 = CARTESIAN_POINT ( 'NONE',  ( -11.00000000000000000, -11.50000000000100009, -10.50000000000065903 ) ) ;
#53392 = VECTOR ( 'NONE', #42662, 1000.000000000000000 ) ;
#53393 = FACE_OUTER_BOUND ( 'NONE', #40802, .T. ) ;
#53394 = DIRECTION ( 'NONE',  ( 0.000000000000000000, -1.000000000000000000, 0.000000000000000000 ) ) ;
#53395 = VERTEX_POINT ( 'NONE', #15492 ) ;
#53396 = ORIENTED_EDGE ( 'NONE', *, *, #9468, .T. ) ;
#53397 = AXIS2_PLACEMENT_3D ( 'NONE', #27429, #929, #11496 ) ;
#53398 = CARTESIAN_POINT ( 'NONE',  ( 0.000000000000000000, -20.50000000000000000, -17.79289321881345032 ) ) ;
#53399 = EDGE_LOOP ( 'NONE', ( #53943, #43774, #34070, #5815, #4851, #62188, #8033 ) ) ;
#53400 = ORIENTED_EDGE ( 'NONE', *, *, #43998, .F. ) ;
#53401 = DIRECTION ( 'NONE',  ( 0.000000000000000000, -3.673940397442059868E-16, 1.000000000000000000 ) ) ;
#53402 = DIRECTION ( 'NONE',  ( 0.000000000000000000, 0.000000000000000000, -1.000000000000000000 ) ) ;
#53403 = CARTESIAN_POINT ( 'NONE',  ( 39.00000000000000000, 0.000000000000000000, 0.000000000000000000 ) ) ;
#53404 = ORIENTED_EDGE ( 'NONE', *, *, #6846, .F. ) ;
#53405 = ADVANCED_FACE ( 'NONE', ( #43040 ), #16528, .F. ) ;
#53406 = CARTESIAN_POINT ( 'NONE',  ( 7.250000000000005329, 8.250000000000001776, -26.00000000000001066 ) ) ;
#53408 = LINE ( 'NONE', #69307, #26458 ) ;
#53407 = DIRECTION ( 'NONE',  ( 0.7071067811865527908, 0.7071067811865422437, 0.000000000000000000 ) ) ;
#53409 = ORIENTED_EDGE ( 'NONE', *, *, #58729, .F. ) ;
#53411 = ORIENTED_EDGE ( 'NONE', *, *, #8428, .T. ) ;
#53410 = DIRECTION ( 'NONE',  ( 0.000000000000000000, 0.000000000000000000, 1.000000000000000000 ) ) ;
#53412 = ORIENTED_EDGE ( 'NONE', *, *, #36690, .T. ) ;
#53413 = EDGE_CURVE ( 'NONE', #14823, #18830, #21138, .T. ) ;
#53414 = FACE_OUTER_BOUND ( 'NONE', #27466, .T. ) ;
#53415 = DIRECTION ( 'NONE',  ( -0.000000000000000000, 3.673940397442059868E-16, -1.000000000000000000 ) ) ;
#53416 = AXIS2_PLACEMENT_3D ( 'NONE', #47128, #68703, #20247 ) ;
#53417 = VERTEX_POINT ( 'NONE', #43384 ) ;
#53418 = AXIS2_PLACEMENT_3D ( 'NONE', #38071, #12547, #16833 ) ;
#53420 = CARTESIAN_POINT ( 'NONE',  ( 283.0000000000000568, -23.50007830495750127, 12.28007262201345995 ) ) ;
#53419 = VECTOR ( 'NONE', #68144, 1000.000000000000114 ) ;
#53421 = DIRECTION ( 'NONE',  ( 1.000000000000000000, 0.000000000000000000, 0.000000000000000000 ) ) ;
#53422 = ORIENTED_EDGE ( 'NONE', *, *, #55739, .F. ) ;
#53423 = VERTEX_POINT ( 'NONE', #10869 ) ;
#53424 = DIRECTION ( 'NONE',  ( -1.000000000000000000, 0.000000000000000000, 0.000000000000000000 ) ) ;
#53425 = LINE ( 'NONE', #42457, #14298 ) ;
#53426 = EDGE_CURVE ( 'NONE', #68804, #45972, #20301, .T. ) ;
#53427 = AXIS2_PLACEMENT_3D ( 'NONE', #48041, #38479, #37783 ) ;
#53428 = DIRECTION ( 'NONE',  ( -0.000000000000000000, -0.000000000000000000, -1.000000000000000000 ) ) ;
#53429 = EDGE_LOOP ( 'NONE', ( #16405, #66837, #67869, #42773 ) ) ;
#53430 = VECTOR ( 'NONE', #1066, 1000.000000000000000 ) ;
#53431 = CARTESIAN_POINT ( 'NONE',  ( -8.689999999999999503, 8.750000000000000000, -7.000000000000000000 ) ) ;
#53432 = CARTESIAN_POINT ( 'NONE',  ( -10.03972626211732688, -9.703773737882722017, 54.00000000000000711 ) ) ;
#53434 = ORIENTED_EDGE ( 'NONE', *, *, #24931, .F. ) ;
#53433 = DIRECTION ( 'NONE',  ( 0.000000000000000000, 0.000000000000000000, 1.000000000000000000 ) ) ;
#53436 = ORIENTED_EDGE ( 'NONE', *, *, #54295, .F. ) ;
#53435 = CYLINDRICAL_SURFACE ( 'NONE', #1845, 0.5249999999999994671 ) ;
#53437 = CYLINDRICAL_SURFACE ( 'NONE', #10235, 0.1999999999999996503 ) ;
#53438 = DIRECTION ( 'NONE',  ( 1.000000000000000000, 1.570596175624152290E-15, 5.770276737693577136E-31 ) ) ;
#53439 = CIRCLE ( 'NONE', #29683, 4.500000000000190958 ) ;
#53440 = FACE_OUTER_BOUND ( 'NONE', #58714, .T. ) ;
#53441 = CARTESIAN_POINT ( 'NONE',  ( 15.50000000000000000, -1.037157890325000054, 26.00000000000000000 ) ) ;
#53442 = LINE ( 'NONE', #59083, #12449 ) ;
#53443 = CARTESIAN_POINT ( 'NONE',  ( -11.11351654964670921, 8.333516549646644123, 455.0000000000000568 ) ) ;
#53444 = VECTOR ( 'NONE', #55226, 1000.000000000000000 ) ;
#53445 = ORIENTED_EDGE ( 'NONE', *, *, #66967, .F. ) ;
#53446 = DIRECTION ( 'NONE',  ( 0.000000000000000000, 0.000000000000000000, -1.000000000000000000 ) ) ;
#53447 = EDGE_CURVE ( 'NONE', #53029, #61001, #10520, .T. ) ;
#53449 = ORIENTED_EDGE ( 'NONE', *, *, #45539, .T. ) ;
#53448 = CARTESIAN_POINT ( 'NONE',  ( 7.000000000000000000, -30.80000000000000071, -8.900000000000000355 ) ) ;
#53450 = PLANE ( 'NONE',  #17493 ) ;
#53451 =( NAMED_UNIT ( * ) PLANE_ANGLE_UNIT ( ) SI_UNIT ( $, .RADIAN. ) );
#53452 = ADVANCED_FACE ( 'NONE', ( #42697 ), #41743, .T. ) ;
#53453 = EDGE_CURVE ( 'NONE', #23904, #10855, #58621, .T. ) ;
#53454 = VECTOR ( 'NONE', #17291, 1000.000000000000000 ) ;
#53455 = CARTESIAN_POINT ( 'NONE',  ( -7.250000000000000888, 8.750000000000001776, -30.00000000000001066 ) ) ;
#53456 = EDGE_CURVE ( 'NONE', #20195, #34803, #10174, .T. ) ;
#53457 = ORIENTED_EDGE ( 'NONE', *, *, #50225, .F. ) ;
#53458 = LINE ( 'NONE', #25886, #38793 ) ;
#53459 = PLANE ( 'NONE',  #40767 ) ;
#53460 = ORIENTED_EDGE ( 'NONE', *, *, #41199, .T. ) ;
#53461 = EDGE_CURVE ( 'NONE', #35182, #47329, #31755, .T. ) ;
#53462 = CARTESIAN_POINT ( 'NONE',  ( 7.000000000000000000, -30.80000000000000071, 12.20000000000000107 ) ) ;
#53463 = DIRECTION ( 'NONE',  ( -1.000000000000000000, 0.000000000000000000, 0.000000000000000000 ) ) ;
#53464 = EDGE_CURVE ( 'NONE', #8621, #67098, #64616, .T. ) ;
#53465 = EDGE_CURVE ( 'NONE', #64137, #68801, #21413, .T. ) ;
#53466 = CYLINDRICAL_SURFACE ( 'NONE', #25301, 0.5000000000023432367 ) ;
#53467 = CIRCLE ( 'NONE', #22953, 2.458500000000000796 ) ;
#53468 = ORIENTED_EDGE ( 'NONE', *, *, #27267, .T. ) ;
#53469 = DIRECTION ( 'NONE',  ( 0.000000000000000000, 0.000000000000000000, 1.000000000000000000 ) ) ;
#53470 = VERTEX_POINT ( 'NONE', #53667 ) ;
#53471 = ORIENTED_EDGE ( 'NONE', *, *, #9065, .T. ) ;
#53472 = VECTOR ( 'NONE', #47014, 1000.000000000000000 ) ;
#53473 = DIRECTION ( 'NONE',  ( 0.000000000000000000, 1.000000000000000000, 3.673940397442059868E-16 ) ) ;
#53474 = CARTESIAN_POINT ( 'NONE',  ( 22.90000000000000213, 13.66939075806899240, 20.79999999999999361 ) ) ;
#53475 = AXIS2_PLACEMENT_3D ( 'NONE', #55369, #43719, #7250 ) ;
#53476 = AXIS2_PLACEMENT_3D ( 'NONE', #37588, #68718, #43225 ) ;
#53477 = DIRECTION ( 'NONE',  ( -1.000000000000000000, -0.000000000000000000, -0.000000000000000000 ) ) ;
#53478 = VECTOR ( 'NONE', #63875, 1000.000000000000000 ) ;
#53479 = CARTESIAN_POINT ( 'NONE',  ( 7.450000000000003730, -7.249999999999997335, -8.500000000000000000 ) ) ;
#53480 = VERTEX_POINT ( 'NONE', #64968 ) ;
#53481 = ORIENTED_EDGE ( 'NONE', *, *, #4360, .F. ) ;
#53483 = EDGE_LOOP ( 'NONE', ( #60328, #44114, #5235, #54140 ) ) ;
#53482 = DIRECTION ( 'NONE',  ( 0.000000000000000000, 0.000000000000000000, 1.000000000000000000 ) ) ;
#53484 = VERTEX_POINT ( 'NONE', #53327 ) ;
#53485 = DIRECTION ( 'NONE',  ( -1.000000000000000000, 0.000000000000000000, 0.000000000000000000 ) ) ;
#53486 = LINE ( 'NONE', #60503, #477 ) ;
#53487 = CARTESIAN_POINT ( 'NONE',  ( 9.562023737882759278, 2.355476262117158104, 26.00000000000000711 ) ) ;
#53488 = DIRECTION ( 'NONE',  ( -1.000000000000000000, 0.000000000000000000, 0.000000000000000000 ) ) ;
#53490 = DIRECTION ( 'NONE',  ( 0.000000000000000000, -1.000000000000000000, 0.000000000000000000 ) ) ;
#53489 = CARTESIAN_POINT ( 'NONE',  ( -7.250000000000001776, -7.249999999999998224, -7.500000000000000000 ) ) ;
#53491 = VERTEX_POINT ( 'NONE', #33729 ) ;
#53492 = VECTOR ( 'NONE', #66144, 1000.000000000000000 ) ;
#53493 = ORIENTED_EDGE ( 'NONE', *, *, #53675, .F. ) ;
#53494 = ORIENTED_EDGE ( 'NONE', *, *, #7611, .F. ) ;
#53495 = ORIENTED_EDGE ( 'NONE', *, *, #62513, .F. ) ;
#53496 = CARTESIAN_POINT ( 'NONE',  ( 30.00000000000000000, -15.97213595500069871, -14.50000000000000000 ) ) ;
#53497 = B_SPLINE_CURVE_WITH_KNOTS ( 'NONE', 3,
 ( #38305, #32989, #43248, #60196, #44275, #836 ),
 .UNSPECIFIED., .F., .F.,
 ( 4, 2, 4 ),
 ( 0.0002380763768129734448, 0.7291065797294589146, 1.457975083082104995 ),
 .UNSPECIFIED. ) ;
#53498 = CARTESIAN_POINT ( 'NONE',  ( 7.250000000000005329, -8.249999999999998224, -9.000000000000001776 ) ) ;
#53499 = CARTESIAN_POINT ( 'NONE',  ( 85.07034715830089056, 47.46054028752842413, 227.7837994620735458 ) ) ;
#53500 = CARTESIAN_POINT ( 'NONE',  ( -11.50000000000000000, -15.97213595500069871, -14.50000000000000000 ) ) ;
#53501 = ORIENTED_EDGE ( 'NONE', *, *, #39704, .T. ) ;
#53502 = ORIENTED_EDGE ( 'NONE', *, *, #23067, .T. ) ;
#53503 = ORIENTED_EDGE ( 'NONE', *, *, #23405, .T. ) ;
#53504 = AXIS2_PLACEMENT_3D ( 'NONE', #29517, #60987, #39083 ) ;
#53505 = LINE ( 'NONE', #44861, #58787 ) ;
#53506 = ORIENTED_EDGE ( 'NONE', *, *, #23725, .F. ) ;
#53507 = EDGE_CURVE ( 'NONE', #57928, #60252, #51898, .T. ) ;
#53508 = CARTESIAN_POINT ( 'NONE',  ( 1.090483450353338268, -11.34648345035335737, 195.0000000000000284 ) ) ;
#53509 = DIRECTION ( 'NONE',  ( -1.000000000000000000, 0.000000000000000000, 0.000000000000000000 ) ) ;
#53510 = EDGE_LOOP ( 'NONE', ( #22276, #42175, #24002, #31477 ) ) ;
#53511 = ORIENTED_EDGE ( 'NONE', *, *, #53325, .T. ) ;
#53512 = DIRECTION ( 'NONE',  ( 0.000000000000000000, 0.000000000000000000, 1.000000000000000000 ) ) ;
#53513 = EDGE_CURVE ( 'NONE', #6935, #63729, #6708, .T. ) ;
#53515 = ORIENTED_EDGE ( 'NONE', *, *, #57894, .T. ) ;
#53514 = LINE ( 'NONE', #22379, #69550 ) ;
#53516 = VERTEX_POINT ( 'NONE', #49986 ) ;
#53517 = CIRCLE ( 'NONE', #34238, 5.250000000000000000 ) ;
#53518 = AXIS2_PLACEMENT_3D ( 'NONE', #45987, #3560, #3208 ) ;
#53519 = DIRECTION ( 'NONE',  ( 0.000000000000000000, -0.7071067811828075644, 0.7071067811902875810 ) ) ;
#53520 = EDGE_CURVE ( 'NONE', #61120, #36648, #44671, .T. ) ;
#53522 = ORIENTED_EDGE ( 'NONE', *, *, #37584, .T. ) ;
#53521 = CARTESIAN_POINT ( 'NONE',  ( 39.90000000000000568, 21.00000000000000000, 16.96999999999999886 ) ) ;
#53523 = EDGE_LOOP ( 'NONE', ( #39204, #28636, #28580, #21822 ) ) ;
#53524 = CARTESIAN_POINT ( 'NONE',  ( -7.450000000000001954, -7.249999999999998224, -20.50000000000000000 ) ) ;
#53525 = CARTESIAN_POINT ( 'NONE',  ( 27.90000000000000213, 20.60000000000000142, 2.154935995002245293E-15 ) ) ;
#53526 = VECTOR ( 'NONE', #65597, 1000.000000000000000 ) ;
#53527 = DIRECTION ( 'NONE',  ( -1.062075597536821205E-14, -1.000000000000000000, 0.000000000000000000 ) ) ;
#53528 = EDGE_CURVE ( 'NONE', #18151, #62060, #58964, .T. ) ;
#53529 = CARTESIAN_POINT ( 'NONE',  ( 49.00000000000000000, 20.60000000000000142, -13.86939075806900057 ) ) ;
#53530 = CARTESIAN_POINT ( 'NONE',  ( 7.250000000000005329, -8.249999999999998224, -26.00000000000001066 ) ) ;
#53531 = VECTOR ( 'NONE', #44236, 1000.000000000000000 ) ;
#53532 = ORIENTED_EDGE ( 'NONE', *, *, #50911, .T. ) ;
#53533 = CARTESIAN_POINT ( 'NONE',  ( 9.703773737882817940, 10.03972626211715280, 54.00000000000000711 ) ) ;
#53534 = ORIENTED_EDGE ( 'NONE', *, *, #25314, .T. ) ;
#53535 = CARTESIAN_POINT ( 'NONE',  ( -9.093516549646828651, -11.12648345035338870, 455.0000000000000568 ) ) ;
#53536 = DIRECTION ( 'NONE',  ( 1.000000000000000000, -0.000000000000000000, 0.000000000000000000 ) ) ;
#53537 = ADVANCED_FACE ( 'NONE', ( #50710 ), #2622, .F. ) ;
#53538 = CYLINDRICAL_SURFACE ( 'NONE', #32520, 4.000000000000000000 ) ;
#53539 = DIRECTION ( 'NONE',  ( -5.163402228214836012E-15, -1.000000000000000000, -1.836970198721026976E-16 ) ) ;
#53540 = DIRECTION ( 'NONE',  ( -1.000000000000000000, 0.000000000000000000, 0.000000000000000000 ) ) ;
#53541 = VERTEX_POINT ( 'NONE', #60963 ) ;
#53542 = LINE ( 'NONE', #31288, #5406 ) ;
#53543 = EDGE_CURVE ( 'NONE', #43882, #29308, #22804, .T. ) ;
#53544 = CARTESIAN_POINT ( 'NONE',  ( 11.50000000000000000, -11.50000000000100009, 15.00000000000084910 ) ) ;
#53545 = EDGE_CURVE ( 'NONE', #10010, #8859, #60273, .T. ) ;
#53546 = ORIENTED_EDGE ( 'NONE', *, *, #38883, .T. ) ;
#53547 = LINE ( 'NONE', #6139, #60903 ) ;
#53548 = CARTESIAN_POINT ( 'NONE',  ( 6.832023737882815695, 9.722976262117192903, 54.00000000000000711 ) ) ;
#53549 = DIRECTION ( 'NONE',  ( 0.000000000000000000, 0.7096009616570518874, -0.7046037717862339012 ) ) ;
#53550 = ORIENTED_EDGE ( 'NONE', *, *, #2023, .T. ) ;
#53551 = FACE_OUTER_BOUND ( 'NONE', #13746, .T. ) ;
#53552 = PLANE ( 'NONE',  #37640 ) ;
#53553 = VERTEX_POINT ( 'NONE', #17150 ) ;
#53554 = DIRECTION ( 'NONE',  ( -1.356437060717832013E-15, -1.000000000000000000, -1.836970198721033878E-16 ) ) ;
#53555 = ADVANCED_FACE ( 'NONE', ( #17489 ), #39064, .F. ) ;
#53556 = AXIS2_PLACEMENT_3D ( 'NONE', #25810, #67884, #68227 ) ;
#53557 = CARTESIAN_POINT ( 'NONE',  ( 38.90000000000000568, -14.06939075806900163, -20.80000000000000426 ) ) ;
#53558 = CARTESIAN_POINT ( 'NONE',  ( 9.562023737882814345, -2.544523737882825820, 54.00000000000000711 ) ) ;
#53559 = CARTESIAN_POINT ( 'NONE',  ( -10.49297626211726175, 6.835476262117182955, 54.00000000000000711 ) ) ;
#53560 = ORIENTED_EDGE ( 'NONE', *, *, #49773, .F. ) ;
#53562 = ORIENTED_EDGE ( 'NONE', *, *, #17405, .T. ) ;
#53561 = LINE ( 'NONE', #5118, #52044 ) ;
#53563 = CIRCLE ( 'NONE', #17395, 4.000000000000000888 ) ;
#53564 = AXIS2_PLACEMENT_3D ( 'NONE', #68786, #25669, #31667 ) ;
#53565 = LINE ( 'NONE', #46842, #44031 ) ;
#53566 = DIRECTION ( 'NONE',  ( 0.000000000000000000, 0.000000000000000000, -1.000000000000000000 ) ) ;
#53567 = DIRECTION ( 'NONE',  ( -1.000000000000000000, 0.000000000000000000, 0.000000000000000000 ) ) ;
#53568 = ORIENTED_EDGE ( 'NONE', *, *, #21028, .T. ) ;
#53569 = SURFACE_STYLE_FILL_AREA ( #21731 ) ;
#53570 = AXIS2_PLACEMENT_3D ( 'NONE', #58352, #63651, #51986 ) ;
#53571 = DIRECTION ( 'NONE',  ( 0.000000000000000000, 0.000000000000000000, -1.000000000000000000 ) ) ;
#53572 = VECTOR ( 'NONE', #68745, 1000.000000000000000 ) ;
#53573 = VERTEX_POINT ( 'NONE', #12524 ) ;
#53574 = ORIENTED_EDGE ( 'NONE', *, *, #1996, .F. ) ;
#53575 = ADVANCED_FACE ( 'NONE', ( #56026 ), #65593, .F. ) ;
#53577 = VERTEX_POINT ( 'NONE', #12183 ) ;
#53576 = VECTOR ( 'NONE', #22938, 1000.000000000000000 ) ;
#53578 = DIRECTION ( 'NONE',  ( -1.047444401652940007E-14, -1.000000000000000000, -1.836970198721029934E-16 ) ) ;
#53579 = ADVANCED_FACE ( 'NONE', ( #39744, #33419 ), #23499, .F. ) ;
#53580 = DIRECTION ( 'NONE',  ( 0.5773502691896201799, -0.5773502691896285066, -0.5773502691896285066 ) ) ;
#53581 = LINE ( 'NONE', #48277, #42696 ) ;
#53582 = ORIENTED_EDGE ( 'NONE', *, *, #22543, .T. ) ;
#53583 = VERTEX_POINT ( 'NONE', #33751 ) ;
#53584 = ADVANCED_FACE ( 'NONE', ( #55338 ), #34963, .F. ) ;
#53585 = VECTOR ( 'NONE', #68345, 1000.000000000000000 ) ;
#53586 = DIRECTION ( 'NONE',  ( -1.836970198721029934E-16, 1.836970198721036344E-16, -1.000000000000000000 ) ) ;
#53587 = ORIENTED_EDGE ( 'NONE', *, *, #60423, .T. ) ;
#53588 = ADVANCED_FACE ( 'NONE', ( #13232 ), #6877, .F. ) ;
#53589 = ORIENTED_EDGE ( 'NONE', *, *, #25569, .F. ) ;
#53590 = ORIENTED_EDGE ( 'NONE', *, *, #7721, .F. ) ;
#53591 = ORIENTED_EDGE ( 'NONE', *, *, #37753, .T. ) ;
#53592 = CARTESIAN_POINT ( 'NONE',  ( 275.0000000000000000, -26.28355339059299922, -9.766446609406699508 ) ) ;
#53593 = UNCERTAINTY_MEASURE_WITH_UNIT (LENGTH_MEASURE( 1.000000000000000082E-05 ), #26311, 'distance_accuracy_value', 'NONE');
#53594 = EDGE_CURVE ( 'NONE', #43722, #8790, #7919, .T. ) ;
#53596 = VERTEX_POINT ( 'NONE', #23139 ) ;
#53595 = DIRECTION ( 'NONE',  ( 0.000000000000000000, -0.7278708115916125987, 0.6857142857145147596 ) ) ;
#53597 = CARTESIAN_POINT ( 'NONE',  ( -4.173516549646666185, 11.99351654964658920, 455.0000000000000568 ) ) ;
#53598 = CARTESIAN_POINT ( 'NONE',  ( 27.90000000000000213, -0.2000000000089119934, -8.913009219568841313E-12 ) ) ;
#53599 = LINE ( 'NONE', #36993, #66308 ) ;
#53600 = EDGE_CURVE ( 'NONE', #69904, #53395, #29144, .T. ) ;
#53601 = ORIENTED_EDGE ( 'NONE', *, *, #59586, .F. ) ;
#53602 = EDGE_CURVE ( 'NONE', #45591, #53754, #44698, .T. ) ;
#53603 = VECTOR ( 'NONE', #69193, 1000.000000000000000 ) ;
#53604 = EDGE_CURVE ( 'NONE', #14259, #938, #19131, .T. ) ;
#53605 = ADVANCED_FACE ( 'NONE', ( #34793 ), #66970, .F. ) ;
#53606 = DIRECTION ( 'NONE',  ( 1.000000000000000000, 0.000000000000000000, 0.000000000000000000 ) ) ;
#53607 = CARTESIAN_POINT ( 'NONE',  ( 275.0000000000000000, -24.99999999999915090, 9.080000000000110205 ) ) ;
#53608 = EDGE_LOOP ( 'NONE', ( #42749, #10534, #37983, #33188 ) ) ;
#53609 = ADVANCED_FACE ( 'NONE', ( #56368 ), #29493, .F. ) ;
#53610 = AXIS2_PLACEMENT_3D ( 'NONE', #22498, #38742, #37371 ) ;
#53611 = VECTOR ( 'NONE', #10014, 1000.000000000000000 ) ;
#53612 = FACE_OUTER_BOUND ( 'NONE', #16248, .T. ) ;
#53613 = CARTESIAN_POINT ( 'NONE',  ( 11.48848345035334617, -11.08848345035349148, 455.0000000000000568 ) ) ;
#53614 = ORIENTED_EDGE ( 'NONE', *, *, #33230, .F. ) ;
#53615 = CYLINDRICAL_SURFACE ( 'NONE', #67433, 0.2000000000000005107 ) ;
#53616 = EDGE_CURVE ( 'NONE', #10422, #11140, #41150, .T. ) ;
#53617 = CIRCLE ( 'NONE', #35565, 0.9999999999999991118 ) ;
#53618 = DIRECTION ( 'NONE',  ( 0.000000000000000000, 0.000000000000000000, -1.000000000000000000 ) ) ;
#53619 = DIRECTION ( 'NONE',  ( 0.000000000000000000, 0.000000000000000000, -1.000000000000000000 ) ) ;
#53620 = VECTOR ( 'NONE', #65566, 1000.000000000000000 ) ;
#53621 = CARTESIAN_POINT ( 'NONE',  ( 75.42576880091937142, 10.00000000000000000, 285.9830310981789125 ) ) ;
#53622 = DIRECTION ( 'NONE',  ( 0.000000000000000000, 0.000000000000000000, -1.000000000000000000 ) ) ;
#53623 = DIRECTION ( 'NONE',  ( 0.000000000000000000, 0.000000000000000000, 1.000000000000000000 ) ) ;
#53624 = ADVANCED_FACE ( 'NONE', ( #63077 ), #25250, .T. ) ;
#53625 = CARTESIAN_POINT ( 'NONE',  ( 3.606483450353402009, 5.993516549646589198, 455.0000000000000568 ) ) ;
#53626 = PLANE ( 'NONE',  #67269 ) ;
#53627 = ADVANCED_FACE ( 'NONE', ( #30206 ), #51772, .F. ) ;
#53628 = VECTOR ( 'NONE', #36651, 1000.000000000000000 ) ;
#53629 = ORIENTED_EDGE ( 'NONE', *, *, #67643, .F. ) ;
#53630 = CARTESIAN_POINT ( 'NONE',  ( 30.00000000000000000, -11.70000000000000284, -12.50000000000000000 ) ) ;
#53631 = PLANE ( 'NONE',  #63561 ) ;
#53632 = VECTOR ( 'NONE', #16624, 1000.000000000000000 ) ;
#53633 = DIRECTION ( 'NONE',  ( 0.7071067811865529018, 0.7071067811865422437, 0.000000000000000000 ) ) ;
#53634 = LINE ( 'NONE', #4497, #48848 ) ;
#53635 = EDGE_LOOP ( 'NONE', ( #29823, #59256, #5919, #616 ) ) ;
#53636 = DIRECTION ( 'NONE',  ( 0.000000000000000000, 1.000000000000000000, 0.000000000000000000 ) ) ;
#53637 = CARTESIAN_POINT ( 'NONE',  ( -7.250000000000001776, -7.249999999999998224, -13.00000000000000178 ) ) ;
#53638 = DIRECTION ( 'NONE',  ( 0.000000000000000000, -1.000000000000000000, 0.000000000000000000 ) ) ;
#53639 = CARTESIAN_POINT ( 'NONE',  ( 13.00000000000000178, -15.50000000000000000, -20.05051025721700242 ) ) ;
#53640 = LINE ( 'NONE', #31726, #36495 ) ;
#53641 = DIRECTION ( 'NONE',  ( 0.000000000000000000, 1.000000000000000000, 0.000000000000000000 ) ) ;
#53642 = EDGE_LOOP ( 'NONE', ( #52807, #44424, #61378, #546 ) ) ;
#53643 = ORIENTED_EDGE ( 'NONE', *, *, #27289, .T. ) ;
#53644 = CARTESIAN_POINT ( 'NONE',  ( -27.50000000000000000, -5.200000000000001066, 22.50000000000000000 ) ) ;
#53645 = CARTESIAN_POINT ( 'NONE',  ( 14.25000000000000000, -2.500000000000000000, -23.22168783648699986 ) ) ;
#53646 = ORIENTED_EDGE ( 'NONE', *, *, #46835, .F. ) ;
#53647 = AXIS2_PLACEMENT_3D ( 'NONE', #21893, #17274, #43457 ) ;
#53648 = CARTESIAN_POINT ( 'NONE',  ( -2.617976262117251540, 6.486996718459834277, 26.00000000000000711 ) ) ;
#53649 = DIRECTION ( 'NONE',  ( 1.000000000000000000, -0.000000000000000000, 0.000000000000000000 ) ) ;
#53650 = AXIS2_PLACEMENT_3D ( 'NONE', #69459, #5470, #58521 ) ;
#53651 = ORIENTED_EDGE ( 'NONE', *, *, #56682, .T. ) ;
#53652 = DIRECTION ( 'NONE',  ( 0.000000000000000000, 0.000000000000000000, -1.000000000000000000 ) ) ;
#53653 = VERTEX_POINT ( 'NONE', #24196 ) ;
#53654 = ORIENTED_EDGE ( 'NONE', *, *, #31436, .T. ) ;
#53655 = DIRECTION ( 'NONE',  ( 0.000000000000000000, 0.000000000000000000, -1.000000000000000000 ) ) ;
#53656 = ORIENTED_EDGE ( 'NONE', *, *, #38041, .F. ) ;
#53657 = LINE ( 'NONE', #27823, #19574 ) ;
#53658 = EDGE_CURVE ( 'NONE', #62865, #34324, #68382, .T. ) ;
#53659 = CARTESIAN_POINT ( 'NONE',  ( -2.530476262117233865, 8.821682069070682530, 54.00000000000000711 ) ) ;
#53660 = CARTESIAN_POINT ( 'NONE',  ( 69.92576880110416937, 0.000000000000000000, 335.4830310981152479 ) ) ;
#53661 = CIRCLE ( 'NONE', #49104, 0.5000000000004306555 ) ;
#53662 = AXIS2_PLACEMENT_3D ( 'NONE', #4627, #43132, #16267 ) ;
#53663 = ORIENTED_EDGE ( 'NONE', *, *, #25563, .F. ) ;
#53664 = VERTEX_POINT ( 'NONE', #63432 ) ;
#53665 = EDGE_CURVE ( 'NONE', #26867, #59828, #24840, .T. ) ;
#53666 = DIRECTION ( 'NONE',  ( 0.000000000000000000, 0.000000000000000000, 1.000000000000000000 ) ) ;
#53668 = DIRECTION ( 'NONE',  ( 1.000000000000000000, -0.000000000000000000, -0.000000000000000000 ) ) ;
#53667 = CARTESIAN_POINT ( 'NONE',  ( -30.00000000000000000, -12.00000000000000000, 10.52786404500095863 ) ) ;
#53669 = EDGE_LOOP ( 'NONE', ( #41436, #38992, #10024, #1470 ) ) ;
#53670 = EDGE_CURVE ( 'NONE', #64892, #34655, #19941, .T. ) ;
#53671 = ORIENTED_EDGE ( 'NONE', *, *, #51090, .F. ) ;
#53672 = EDGE_CURVE ( 'NONE', #1231, #52952, #62070, .T. ) ;
#53673 = ORIENTED_EDGE ( 'NONE', *, *, #58388, .F. ) ;
#53674 = AXIS2_PLACEMENT_3D ( 'NONE', #45366, #29464, #13551 ) ;
#53675 = EDGE_CURVE ( 'NONE', #41573, #60909, #56718, .T. ) ;
#53676 = ADVANCED_FACE ( 'NONE', ( #25612 ), #68031, .F. ) ;
#53677 = DIRECTION ( 'NONE',  ( -1.000000000000000000, 0.000000000000000000, 0.000000000000000000 ) ) ;
#53679 = ORIENTED_EDGE ( 'NONE', *, *, #31093, .T. ) ;
#53678 = CARTESIAN_POINT ( 'NONE',  ( -3.667976262117228714, 9.722976262117169810, 26.00000000000000711 ) ) ;
#53680 = DIRECTION ( 'NONE',  ( -0.000000000000000000, -0.000000000000000000, -1.000000000000000000 ) ) ;
#53681 = VECTOR ( 'NONE', #49286, 1000.000000000000000 ) ;
#53682 = DIRECTION ( 'NONE',  ( -0.000000000000000000, -0.000000000000000000, -1.000000000000000000 ) ) ;
#53683 = VERTEX_POINT ( 'NONE', #14297 ) ;
#53684 = ORIENTED_EDGE ( 'NONE', *, *, #22950, .F. ) ;
#53685 = AXIS2_PLACEMENT_3D ( 'NONE', #57850, #8720, #19319 ) ;
#53686 = DIRECTION ( 'NONE',  ( 0.000000000000000000, 0.000000000000000000, 1.000000000000000000 ) ) ;
#53687 = ORIENTED_EDGE ( 'NONE', *, *, #120, .T. ) ;
#53688 = DIRECTION ( 'NONE',  ( -1.000000000000000000, 0.000000000000000000, 0.000000000000000000 ) ) ;
#53689 = CARTESIAN_POINT ( 'NONE',  ( 6.500000000000002665, 6.500000000000000888, -1.000000000000000000 ) ) ;
#53690 = FACE_OUTER_BOUND ( 'NONE', #26665, .T. ) ;
#53691 = VERTEX_POINT ( 'NONE', #29842 ) ;
#53692 = CARTESIAN_POINT ( 'NONE',  ( -4.141586236041100655, 5.779227145995200488, 54.00000000000000711 ) ) ;
#53693 = DIRECTION ( 'NONE',  ( -1.836970198721029934E-16, 1.836970198721036590E-16, -1.000000000000000000 ) ) ;
#53694 = VERTEX_POINT ( 'NONE', #36552 ) ;
#53695 = ORIENTED_EDGE ( 'NONE', *, *, #16984, .F. ) ;
#53696 = DIRECTION ( 'NONE',  ( 0.000000000000000000, -1.000000000000000000, 0.000000000000000000 ) ) ;
#53697 = DIRECTION ( 'NONE',  ( -1.062075597536822467E-14, -1.000000000000000000, 0.000000000000000000 ) ) ;
#53698 = VECTOR ( 'NONE', #47288, 1000.000000000000000 ) ;
#53699 = DIRECTION ( 'NONE',  ( -1.000000000000000000, 0.000000000000000000, 0.000000000000000000 ) ) ;
#53700 = DIRECTION ( 'NONE',  ( 0.000000000000000000, 0.000000000000000000, 1.000000000000000000 ) ) ;
#53701 = CIRCLE ( 'NONE', #2854, 0.1749999999999998224 ) ;
#53702 = DIRECTION ( 'NONE',  ( -1.836970198721029934E-16, 1.836970198721036344E-16, -1.000000000000000000 ) ) ;
#53703 = ORIENTED_EDGE ( 'NONE', *, *, #2713, .T. ) ;
#53704 = DIRECTION ( 'NONE',  ( 0.000000000000000000, 1.000000000000000000, 0.000000000000000000 ) ) ;
#53705 = CARTESIAN_POINT ( 'NONE',  ( 29.50000000000000355, -12.00000000000000000, 11.00000000000000000 ) ) ;
#53706 = CYLINDRICAL_SURFACE ( 'NONE', #61621, 0.6000000000000007550 ) ;
#53708 = ORIENTED_EDGE ( 'NONE', *, *, #19900, .F. ) ;
#53707 = DIRECTION ( 'NONE',  ( -0.000000000000000000, -0.000000000000000000, -1.000000000000000000 ) ) ;
#53709 = EDGE_CURVE ( 'NONE', #49302, #40699, #2985, .T. ) ;
#53710 = CIRCLE ( 'NONE', #25436, 0.3999999999993835154 ) ;
#53711 = VECTOR ( 'NONE', #1010, 1000.000000000000000 ) ;
#53712 = VECTOR ( 'NONE', #5239, 1000.000000000000114 ) ;
#53713 =( LENGTH_UNIT ( ) NAMED_UNIT ( * ) SI_UNIT ( .MILLI., .METRE. ) );
#53714 = DIRECTION ( 'NONE',  ( 0.000000000000000000, 0.000000000000000000, 1.000000000000000000 ) ) ;
#53715 = EDGE_CURVE ( 'NONE', #30081, #37047, #58123, .T. ) ;
#53716 = LINE ( 'NONE', #69273, #25092 ) ;
#53717 = CIRCLE ( 'NONE', #7397, 4.000000000000000000 ) ;
#53718 = AXIS2_PLACEMENT_3D ( 'NONE', #1894, #11794, #65891 ) ;
#53719 = DIRECTION ( 'NONE',  ( -0.000000000000000000, -0.000000000000000000, -1.000000000000000000 ) ) ;
#53720 = EDGE_LOOP ( 'NONE', ( #2792, #43844, #62215, #65761 ) ) ;
#53721 = CARTESIAN_POINT ( 'NONE',  ( -14.45313394609757651, -0.2715358723599896051, 21.66103272505202781 ) ) ;
#53722 = DIRECTION ( 'NONE',  ( 1.000000000000000000, -0.000000000000000000, 0.000000000000000000 ) ) ;
#53723 = ORIENTED_EDGE ( 'NONE', *, *, #15597, .F. ) ;
#53724 = DIRECTION ( 'NONE',  ( 0.000000000000000000, 0.7096009616570518874, 0.7046037717862339012 ) ) ;
#53725 = DIRECTION ( 'NONE',  ( -1.000000000000000000, 0.000000000000000000, 0.000000000000000000 ) ) ;
#53726 = CIRCLE ( 'NONE', #36768, 1.000000000000000000 ) ;
#53727 = CARTESIAN_POINT ( 'NONE',  ( 4.155633711806649089, 5.779227145995230686, 54.00000000000000711 ) ) ;
#53728 = CARTESIAN_POINT ( 'NONE',  ( -7.798499376344067535, 7.259684009079840017, 195.0000000000000284 ) ) ;
#53729 = DIRECTION ( 'NONE',  ( 1.000000000000000000, 0.000000000000000000, 0.000000000000000000 ) ) ;
#53730 = AXIS2_PLACEMENT_3D ( 'NONE', #60383, #37803, #59365 ) ;
#53731 = ORIENTED_EDGE ( 'NONE', *, *, #61200, .F. ) ;
#53732 = ORIENTED_EDGE ( 'NONE', *, *, #23162, .T. ) ;
#53733 = DIRECTION ( 'NONE',  ( 1.000000000000000000, -0.000000000000000000, 0.000000000000000000 ) ) ;
#53734 = ORIENTED_EDGE ( 'NONE', *, *, #15089, .T. ) ;
#53735 = ORIENTED_EDGE ( 'NONE', *, *, #44785, .F. ) ;
#53736 = VECTOR ( 'NONE', #1763, 1000.000000000000114 ) ;
#53737 = LINE ( 'NONE', #59031, #63034 ) ;
#53738 = CARTESIAN_POINT ( 'NONE',  ( 283.0000000000000568, -42.50000000000000000, -15.10000000000000142 ) ) ;
#53739 = DIRECTION ( 'NONE',  ( 0.000000000000000000, 0.000000000000000000, -1.000000000000000000 ) ) ;
#53740 = ORIENTED_EDGE ( 'NONE', *, *, #30285, .T. ) ;
#53741 = EDGE_LOOP ( 'NONE', ( #549, #63688, #6863, #1192 ) ) ;
#53742 = DIRECTION ( 'NONE',  ( -1.000000000000000000, 0.000000000000000000, 0.000000000000000000 ) ) ;
#53743 = ORIENTED_EDGE ( 'NONE', *, *, #40418, .T. ) ;
#53744 = ORIENTED_EDGE ( 'NONE', *, *, #6477, .T. ) ;
#53745 = ADVANCED_FACE ( 'NONE', ( #52475 ), #52844, .F. ) ;
#53746 = LINE ( 'NONE', #30775, #34935 ) ;
#53747 = CARTESIAN_POINT ( 'NONE',  ( 6.884529946162100345, -21.00000000000000000, 8.000000000000000000 ) ) ;
#53748 = CARTESIAN_POINT ( 'NONE',  ( -7.793516549646712477, 11.11351654964660085, 455.0000000000000568 ) ) ;
#53749 = STYLED_ITEM ( 'NONE', ( #41590 ), #19540 ) ;
#53750 = ORIENTED_EDGE ( 'NONE', *, *, #57743, .T. ) ;
#53751 = DIRECTION ( 'NONE',  ( 0.000000000000000000, -5.800915303574361727E-12, -1.000000000000000000 ) ) ;
#53753 = DIRECTION ( 'NONE',  ( -1.836970198721029934E-16, -1.836970198721010706E-16, 1.000000000000000000 ) ) ;
#53752 = DIRECTION ( 'NONE',  ( -0.000000000000000000, -0.000000000000000000, 1.000000000000000000 ) ) ;
#53754 = VERTEX_POINT ( 'NONE', #57063 ) ;
#53755 = EDGE_LOOP ( 'NONE', ( #62418, #22648, #5734, #25311 ) ) ;
#53757 = ORIENTED_EDGE ( 'NONE', *, *, #45954, .F. ) ;
#53756 = CARTESIAN_POINT ( 'NONE',  ( 7.450000000000003730, -7.249999999999997335, -12.50000000000000000 ) ) ;
#53758 = VECTOR ( 'NONE', #24594, 1000.000000000000000 ) ;
#53759 = ADVANCED_FACE ( 'NONE', ( #4040 ), #30553, .T. ) ;
#53760 = ORIENTED_EDGE ( 'NONE', *, *, #54782, .F. ) ;
#53761 = EDGE_CURVE ( 'NONE', #32685, #35273, #24897, .T. ) ;
#53762 = EDGE_CURVE ( 'NONE', #21321, #55707, #59872, .T. ) ;
#53763 = EDGE_CURVE ( 'NONE', #29352, #5145, #30904, .T. ) ;
#53764 = CARTESIAN_POINT ( 'NONE',  ( -1.991476262117315432, -8.612468434717262866, 54.00000000000000711 ) ) ;
#53765 = AXIS2_PLACEMENT_3D ( 'NONE', #20970, #42544, #64815 ) ;
#53766 = AXIS2_PLACEMENT_3D ( 'NONE', #52580, #4143, #4490 ) ;
#53768 = CARTESIAN_POINT ( 'NONE',  ( -7.342976262117269393, -4.961189459949999936, 26.00000000000000711 ) ) ;
#53767 = AXIS2_PLACEMENT_3D ( 'NONE', #42099, #26195, #3227 ) ;
#53769 = ADVANCED_FACE ( 'NONE', ( #11081 ), #38307, .F. ) ;
#53770 = VERTEX_POINT ( 'NONE', #26298 ) ;
#53771 = VECTOR ( 'NONE', #41729, 1000.000000000000000 ) ;
#53772 = DIRECTION ( 'NONE',  ( -0.000000000000000000, 3.673940397442059868E-16, -1.000000000000000000 ) ) ;
#53773 = LINE ( 'NONE', #59757, #15400 ) ;
#53774 = ORIENTED_EDGE ( 'NONE', *, *, #48788, .T. ) ;
#53775 = ORIENTED_EDGE ( 'NONE', *, *, #56636, .F. ) ;
#53776 = FACE_OUTER_BOUND ( 'NONE', #61441, .T. ) ;
#53778 = AXIS2_PLACEMENT_3D ( 'NONE', #57139, #56433, #62078 ) ;
#53777 = CARTESIAN_POINT ( 'NONE',  ( -0.9414762621172249046, 9.915476262117151052, 54.00000000000000711 ) ) ;
#53779 = CARTESIAN_POINT ( 'NONE',  ( 8.250000000000005329, 0.000000000000000000, -10.50000000000000000 ) ) ;
#53780 = VERTEX_POINT ( 'NONE', #31616 ) ;
#53781 = VECTOR ( 'NONE', #22914, 1000.000000000000000 ) ;
#53782 = DIRECTION ( 'NONE',  ( -0.000000000000000000, -0.000000000000000000, -1.000000000000000000 ) ) ;
#53783 = DIRECTION ( 'NONE',  ( -1.000000000000000000, 0.000000000000000000, 0.000000000000000000 ) ) ;
#53785 = ORIENTED_EDGE ( 'NONE', *, *, #54401, .F. ) ;
#53784 = DIRECTION ( 'NONE',  ( 0.000000000000000000, 3.673940397442059868E-16, -1.000000000000000000 ) ) ;
#53786 = VECTOR ( 'NONE', #65357, 1000.000000000000000 ) ;
#53788 = EDGE_LOOP ( 'NONE', ( #20281, #18159, #57413, #55384, #12512, #34618, #36820, #59864, #22279 ) ) ;
#53787 = CYLINDRICAL_SURFACE ( 'NONE', #13143, 1.000000000000001776 ) ;
#53789 = DIRECTION ( 'NONE',  ( 0.000000000000000000, -1.000000000000000000, 0.000000000000000000 ) ) ;
#53790 = CARTESIAN_POINT ( 'NONE',  ( -11.11351654964671098, 7.793516549646603231, 455.0000000000000568 ) ) ;
#53791 = DIRECTION ( 'NONE',  ( 0.000000000000000000, 0.000000000000000000, -1.000000000000000000 ) ) ;
#53792 = DIRECTION ( 'NONE',  ( -1.000000000000000000, -0.000000000000000000, -0.000000000000000000 ) ) ;
#53793 = DIRECTION ( 'NONE',  ( 0.000000000000000000, 0.000000000000000000, 1.000000000000000000 ) ) ;
#53794 = DIRECTION ( 'NONE',  ( 0.000000000000000000, 1.000000000000000000, 0.000000000000000000 ) ) ;
#53795 = ORIENTED_EDGE ( 'NONE', *, *, #45725, .F. ) ;
#53796 = FACE_OUTER_BOUND ( 'NONE', #53087, .T. ) ;
#53797 = VERTEX_POINT ( 'NONE', #32990 ) ;
#53799 = ORIENTED_EDGE ( 'NONE', *, *, #42089, .F. ) ;
#53798 = CARTESIAN_POINT ( 'NONE',  ( 283.0000000000000568, -39.80000000000000426, -8.400000000000000355 ) ) ;
#53800 = LINE ( 'NONE', #32584, #21074 ) ;
#53801 = AXIS2_PLACEMENT_3D ( 'NONE', #34798, #39750, #50716 ) ;
#53802 = EDGE_CURVE ( 'NONE', #34368, #62916, #5449, .T. ) ;
#53803 = LINE ( 'NONE', #53114, #18253 ) ;
#53804 = EDGE_CURVE ( 'NONE', #10955, #15345, #32650, .T. ) ;
#53805 = EDGE_CURVE ( 'NONE', #35336, #59438, #65529, .T. ) ;
#53806 = VECTOR ( 'NONE', #52883, 1000.000000000000000 ) ;
#53807 = ORIENTED_EDGE ( 'NONE', *, *, #5396, .T. ) ;
#53808 = FACE_OUTER_BOUND ( 'NONE', #25287, .T. ) ;
#53809 = DIRECTION ( 'NONE',  ( 0.000000000000000000, 1.000000000000000000, -0.000000000000000000 ) ) ;
#53811 = EDGE_LOOP ( 'NONE', ( #57841, #61653, #68759, #36406 ) ) ;
#53810 = EDGE_CURVE ( 'NONE', #15525, #48685, #15341, .T. ) ;
#53812 = DIRECTION ( 'NONE',  ( 0.000000000000000000, 0.000000000000000000, -1.000000000000000000 ) ) ;
#53813 = CARTESIAN_POINT ( 'NONE',  ( 283.0000000000000568, -24.99999999999915090, 9.080000000000110205 ) ) ;
#53814 = AXIS2_PLACEMENT_3D ( 'NONE', #15021, #27027, #15725 ) ;
#53815 = VECTOR ( 'NONE', #7125, 1000.000000000000000 ) ;
#53816 = DIRECTION ( 'NONE',  ( 0.000000000000000000, 0.000000000000000000, 1.000000000000000000 ) ) ;
#53817 = VECTOR ( 'NONE', #23756, 1000.000000000000000 ) ;
#53818 = VECTOR ( 'NONE', #4245, 1000.000000000000000 ) ;
#53819 = VECTOR ( 'NONE', #67503, 1000.000000000000000 ) ;
#53820 = VERTEX_POINT ( 'NONE', #42204 ) ;
#53821 = DIRECTION ( 'NONE',  ( 1.000000000000000000, 0.000000000000000000, 0.000000000000000000 ) ) ;
#53822 = ORIENTED_EDGE ( 'NONE', *, *, #21781, .T. ) ;
#53823 = ORIENTED_EDGE ( 'NONE', *, *, #29764, .T. ) ;
#53824 = LINE ( 'NONE', #31213, #21208 ) ;
#53826 = LINE ( 'NONE', #6070, #38779 ) ;
#53825 = AXIS2_PLACEMENT_3D ( 'NONE', #29492, #24195, #45751 ) ;
#53827 = AXIS2_PLACEMENT_3D ( 'NONE', #34223, #66763, #12310 ) ;
#53828 = VECTOR ( 'NONE', #59419, 1000.000000000000000 ) ;
#53829 = DIRECTION ( 'NONE',  ( 1.000000000000000000, -0.000000000000000000, 0.000000000000000000 ) ) ;
#53830 = CARTESIAN_POINT ( 'NONE',  ( 7.250000000000005329, 7.250000000000000888, -15.00000000000000000 ) ) ;
#53831 = ORIENTED_EDGE ( 'NONE', *, *, #65655, .F. ) ;
#53832 = ORIENTED_EDGE ( 'NONE', *, *, #50732, .T. ) ;
#53834 = VERTEX_POINT ( 'NONE', #58832 ) ;
#53833 = DIRECTION ( 'NONE',  ( 0.000000000000000000, 0.000000000000000000, 1.000000000000000000 ) ) ;
#53835 = ORIENTED_EDGE ( 'NONE', *, *, #20253, .F. ) ;
#53836 = VECTOR ( 'NONE', #14289, 1000.000000000000000 ) ;
#53837 = CARTESIAN_POINT ( 'NONE',  ( 9.912023737882815766, -6.832023737882813919, 26.00000000000000000 ) ) ;
#53838 = CARTESIAN_POINT ( 'NONE',  ( 2.544523737882817382, 9.547976262117206403, 54.00000000000000711 ) ) ;
#53839 = CARTESIAN_POINT ( 'NONE',  ( 23.90000000000000213, -0.1999999999911430404, -8.864436962241481021E-12 ) ) ;
#53840 = CARTESIAN_POINT ( 'NONE',  ( 5.257023737882801306, 5.242976262117200470, 54.00000000000000711 ) ) ;
#53842 = DIRECTION ( 'NONE',  ( -0.000000000000000000, 3.673940397442059868E-16, -1.000000000000000000 ) ) ;
#53841 = DIRECTION ( 'NONE',  ( 1.000000000000000000, -0.000000000000000000, -0.000000000000000000 ) ) ;
#53843 = ORIENTED_EDGE ( 'NONE', *, *, #65547, .F. ) ;
#53845 = ORIENTED_EDGE ( 'NONE', *, *, #68744, .T. ) ;
#53844 = CARTESIAN_POINT ( 'NONE',  ( 7.000000000000000000, -21.00000000000000000, -7.799999999999999822 ) ) ;
#53846 = ORIENTED_EDGE ( 'NONE', *, *, #16379, .F. ) ;
#53847 = ORIENTED_EDGE ( 'NONE', *, *, #18490, .F. ) ;
#53848 = DIRECTION ( 'NONE',  ( 0.000000000000000000, 0.000000000000000000, -1.000000000000000000 ) ) ;
#53849 = CYLINDRICAL_SURFACE ( 'NONE', #10647, 0.1749999999999989342 ) ;
#53850 = EDGE_CURVE ( 'NONE', #46878, #37678, #48223, .T. ) ;
#53851 = DIRECTION ( 'NONE',  ( 0.000000000000000000, 0.000000000000000000, 1.000000000000000000 ) ) ;
#53852 = FACE_OUTER_BOUND ( 'NONE', #9801, .T. ) ;
#53853 = EDGE_CURVE ( 'NONE', #42177, #20434, #42560, .T. ) ;
#53854 = ORIENTED_EDGE ( 'NONE', *, *, #63433, .F. ) ;
#53855 = ORIENTED_EDGE ( 'NONE', *, *, #33129, .T. ) ;
#53856 = EDGE_CURVE ( 'NONE', #5174, #37532, #31956, .T. ) ;
#53857 = AXIS2_PLACEMENT_3D ( 'NONE', #1767, #13062, #12017 ) ;
#53858 = ORIENTED_EDGE ( 'NONE', *, *, #29105, .T. ) ;
#53859 = DIRECTION ( 'NONE',  ( 0.000000000000000000, 0.000000000000000000, 1.000000000000000000 ) ) ;
#53860 = DIRECTION ( 'NONE',  ( -1.836970198721029934E-16, 1.836970198721036344E-16, -1.000000000000000000 ) ) ;
#53861 = ADVANCED_FACE ( 'NONE', ( #20633 ), #21344, .F. ) ;
#53862 = AXIS2_PLACEMENT_3D ( 'NONE', #39824, #51143, #29213 ) ;
#53863 = FACE_OUTER_BOUND ( 'NONE', #25899, .T. ) ;
#53864 = ORIENTED_EDGE ( 'NONE', *, *, #28864, .F. ) ;
#53865 = VERTEX_POINT ( 'NONE', #42904 ) ;
#53866 = AXIS2_PLACEMENT_3D ( 'NONE', #50545, #22971, #38555 ) ;
#53868 = CYLINDRICAL_SURFACE ( 'NONE', #18098, 1.399999999999999245 ) ;
#53867 = CIRCLE ( 'NONE', #24517, 4.500000000000191847 ) ;
#53869 = ADVANCED_FACE ( 'NONE', ( #37613 ), #59863, .T. ) ;
#53870 = CARTESIAN_POINT ( 'NONE',  ( -13.00000000000000178, -15.50000000000000000, 20.05051025721700242 ) ) ;
#53872 = ORIENTED_EDGE ( 'NONE', *, *, #9372, .T. ) ;
#53871 = EDGE_CURVE ( 'NONE', #8765, #59076, #51949, .T. ) ;
#53873 = VECTOR ( 'NONE', #60298, 1000.000000000000000 ) ;
#53874 = CIRCLE ( 'NONE', #15448, 0.2000000000000005107 ) ;
#53875 = DIRECTION ( 'NONE',  ( -1.000000000000000000, 0.000000000000000000, 0.000000000000000000 ) ) ;
#53877 = ORIENTED_EDGE ( 'NONE', *, *, #50653, .F. ) ;
#53876 = DIRECTION ( 'NONE',  ( -0.000000000000000000, -0.000000000000000000, -1.000000000000000000 ) ) ;
#53878 = ORIENTED_EDGE ( 'NONE', *, *, #43052, .T. ) ;
#53879 = DIRECTION ( 'NONE',  ( -0.000000000000000000, 1.000000000000000000, -0.000000000000000000 ) ) ;
#53880 = VECTOR ( 'NONE', #14546, 1000.000000000000000 ) ;
#53881 = DIRECTION ( 'NONE',  ( 0.000000000000000000, 0.000000000000000000, -1.000000000000000000 ) ) ;
#53882 = AXIS2_PLACEMENT_3D ( 'NONE', #14068, #51913, #58620 ) ;
#53883 = CARTESIAN_POINT ( 'NONE',  ( 11.34648345035334671, 1.077516549646521327, 455.0000000000000568 ) ) ;
#53884 = DIRECTION ( 'NONE',  ( 0.3479852726768751237, 0.000000000000000000, -0.9375000000000004441 ) ) ;
#53885 = CARTESIAN_POINT ( 'NONE',  ( 9.750000000000001776, 9.690000000000001279, -4.250000000000000000 ) ) ;
#53886 = CIRCLE ( 'NONE', #25497, 0.2000000000000005107 ) ;
#53887 = ORIENTED_EDGE ( 'NONE', *, *, #59527, .F. ) ;
#53888 = DIRECTION ( 'NONE',  ( 0.000000000000000000, 1.000000000000000000, 0.000000000000000000 ) ) ;
#53889 = ORIENTED_EDGE ( 'NONE', *, *, #29573, .T. ) ;
#53890 = CARTESIAN_POINT ( 'NONE',  ( 7.250000000000005329, 7.250000000000000888, -13.00000000000000178 ) ) ;
#53891 = DIRECTION ( 'NONE',  ( 1.836970198721029934E-16, 1.836970198721010706E-16, -1.000000000000000000 ) ) ;
#53892 = CARTESIAN_POINT ( 'NONE',  ( -7.394232575409614761, 6.775514141871308738, 54.00000000000000711 ) ) ;
#53893 = DIRECTION ( 'NONE',  ( 1.836970198721029934E-16, 1.836970198721010706E-16, -1.000000000000000000 ) ) ;
#53894 = DIRECTION ( 'NONE',  ( 0.000000000000000000, 0.000000000000000000, 1.000000000000000000 ) ) ;
#53896 = ORIENTED_EDGE ( 'NONE', *, *, #64407, .F. ) ;
#53895 = ADVANCED_FACE ( 'NONE', ( #53191 ), #10386, .T. ) ;
#53897 = CARTESIAN_POINT ( 'NONE',  ( 21.90000000000000213, -14.06939075806902117, -20.80000000000000426 ) ) ;
#53898 = PLANE ( 'NONE',  #32225 ) ;
#53899 = VERTEX_POINT ( 'NONE', #16042 ) ;
#53900 = CARTESIAN_POINT ( 'NONE',  ( -9.897976262117259338, 6.642976262117183950, 26.00000000000000711 ) ) ;
#53901 = CARTESIAN_POINT ( 'NONE',  ( -5.242976262117259978, 5.242976262117182706, 26.00000000000000711 ) ) ;
#53902 = ORIENTED_EDGE ( 'NONE', *, *, #36287, .F. ) ;
#53903 = CARTESIAN_POINT ( 'NONE',  ( 0.000000000000000000, -8.249999999999998224, -11.00000000000000000 ) ) ;
#53904 = DIRECTION ( 'NONE',  ( 1.000000000000000000, 0.000000000000000000, 0.000000000000000000 ) ) ;
#53906 = ORIENTED_EDGE ( 'NONE', *, *, #3469, .T. ) ;
#53905 = EDGE_CURVE ( 'NONE', #54243, #18078, #10727, .T. ) ;
#53907 = DIRECTION ( 'NONE',  ( 1.000000000000000000, -5.981805089575194965E-17, 0.000000000000000000 ) ) ;
#53908 = DIRECTION ( 'NONE',  ( -1.000000000000000000, 0.000000000000000000, 0.000000000000000000 ) ) ;
#53909 = CIRCLE ( 'NONE', #35869, 0.4000000000000600298 ) ;
#53910 = AXIS2_PLACEMENT_3D ( 'NONE', #22208, #38796, #23225 ) ;
#53911 = DIRECTION ( 'NONE',  ( 0.000000000000000000, 1.000000000000000000, 0.000000000000000000 ) ) ;
#53912 = EDGE_CURVE ( 'NONE', #2504, #64281, #48564, .T. ) ;
#53913 = DIRECTION ( 'NONE',  ( 0.000000000000000000, 0.000000000000000000, 1.000000000000000000 ) ) ;
#53914 = ORIENTED_EDGE ( 'NONE', *, *, #11468, .T. ) ;
#53916 = ORIENTED_EDGE ( 'NONE', *, *, #43843, .F. ) ;
#53915 = LINE ( 'NONE', #59892, #53228 ) ;
#53917 = VECTOR ( 'NONE', #42928, 1000.000000000000000 ) ;
#53918 = CIRCLE ( 'NONE', #1952, 0.1999999999999996503 ) ;
#53919 = PLANE ( 'NONE',  #5650 ) ;
#53920 = EDGE_LOOP ( 'NONE', ( #47030, #27123, #45699, #66674 ) ) ;
#53921 = DIRECTION ( 'NONE',  ( 0.000000000000000000, -0.7071067811865474617, -0.7071067811865474617 ) ) ;
#53922 = CARTESIAN_POINT ( 'NONE',  ( 8.612468434717241550, -2.005523737882815460, 26.00000000000000711 ) ) ;
#53923 = ORIENTED_EDGE ( 'NONE', *, *, #6514, .F. ) ;
#53924 = CIRCLE ( 'NONE', #1957, 0.3499999999999996447 ) ;
#53926 = PLANE ( 'NONE',  #6260 ) ;
#53925 = AXIS2_PLACEMENT_3D ( 'NONE', #15912, #21230, #36791 ) ;
#53927 = CARTESIAN_POINT ( 'NONE',  ( 9.955011587777235604, -2.765062094116182312, 455.0000000000000568 ) ) ;
#53928 = ORIENTED_EDGE ( 'NONE', *, *, #13366, .F. ) ;
#53929 = ORIENTED_EDGE ( 'NONE', *, *, #31439, .F. ) ;
#53930 = EDGE_CURVE ( 'NONE', #40969, #9904, #30490, .T. ) ;
#53931 = EDGE_LOOP ( 'NONE', ( #27974, #18327, #6879, #17097 ) ) ;
#53932 = DIRECTION ( 'NONE',  ( 0.000000000000000000, 0.000000000000000000, 1.000000000000000000 ) ) ;
#53933 = LINE ( 'NONE', #65239, #54106 ) ;
#53934 = DIRECTION ( 'NONE',  ( 0.000000000000000000, 0.000000000000000000, 1.000000000000000000 ) ) ;
#53935 = CIRCLE ( 'NONE', #23427, 0.5000000000000000000 ) ;
#53936 = EDGE_CURVE ( 'NONE', #57134, #53130, #38424, .T. ) ;
#53937 = ORIENTED_EDGE ( 'NONE', *, *, #48178, .T. ) ;
#53938 = ORIENTED_EDGE ( 'NONE', *, *, #68959, .F. ) ;
#53939 = CARTESIAN_POINT ( 'NONE',  ( -10.73351654964669599, -1.690483450353341910, 455.0000000000000568 ) ) ;
#53940 = ORIENTED_EDGE ( 'NONE', *, *, #30204, .T. ) ;
#53941 = ORIENTED_EDGE ( 'NONE', *, *, #50977, .F. ) ;
#53942 = VERTEX_POINT ( 'NONE', #50281 ) ;
#53943 = ORIENTED_EDGE ( 'NONE', *, *, #64061, .T. ) ;
#53944 = CARTESIAN_POINT ( 'NONE',  ( 41.09999999999999432, 20.60000000000000142, -13.86939075806900057 ) ) ;
#53945 = EDGE_CURVE ( 'NONE', #58511, #40726, #1494, .T. ) ;
#53947 = ORIENTED_EDGE ( 'NONE', *, *, #36264, .F. ) ;
#53946 = DIRECTION ( 'NONE',  ( -1.000000000000000000, 0.000000000000000000, 0.000000000000000000 ) ) ;
#53948 = EDGE_CURVE ( 'NONE', #47752, #19062, #44277, .T. ) ;
#53949 = CARTESIAN_POINT ( 'NONE',  ( 283.0000000000000568, -25.93000000000544958, -9.412893218815410634 ) ) ;
#53950 = CARTESIAN_POINT ( 'NONE',  ( -8.250000000000001776, -7.249999999999998224, -26.00000000000001066 ) ) ;
#53951 = CARTESIAN_POINT ( 'NONE',  ( -9.547976262117222390, -2.369523737882729186, 54.00000000000000711 ) ) ;
#53952 = AXIS2_PLACEMENT_3D ( 'NONE', #43955, #65534, #38660 ) ;
#53953 = ORIENTED_EDGE ( 'NONE', *, *, #17685, .T. ) ;
#53954 = CARTESIAN_POINT ( 'NONE',  ( 0.000000000000000000, -7.449999999999998401, -17.50000000000000000 ) ) ;
#53955 = AXIS2_PLACEMENT_3D ( 'NONE', #9496, #68554, #37082 ) ;
#53956 = VECTOR ( 'NONE', #25330, 1000.000000000000000 ) ;
#53957 = CARTESIAN_POINT ( 'NONE',  ( 11.78648345035340661, 7.593516549646560421, 455.0000000000000568 ) ) ;
#53958 = EDGE_LOOP ( 'NONE', ( #32937, #30272, #24775, #35067 ) ) ;
#53959 = AXIS2_PLACEMENT_3D ( 'NONE', #5391, #64766, #43884 ) ;
#53960 = CIRCLE ( 'NONE', #62817, 1.000000000000000000 ) ;
#53961 = CARTESIAN_POINT ( 'NONE',  ( -4.706725378239216440, 6.344366288193329595, 26.00000000000000711 ) ) ;
#53962 = DIRECTION ( 'NONE',  ( 0.000000000000000000, 0.000000000000000000, 1.000000000000000000 ) ) ;
#53963 = VECTOR ( 'NONE', #55847, 1000.000000000000114 ) ;
#53964 = ORIENTED_EDGE ( 'NONE', *, *, #31063, .T. ) ;
#53965 = FACE_OUTER_BOUND ( 'NONE', #32526, .T. ) ;
#53966 = VECTOR ( 'NONE', #56645, 1000.000000000000000 ) ;
#53967 = CIRCLE ( 'NONE', #62990, 0.5000000000079362072 ) ;
#53968 = CYLINDRICAL_SURFACE ( 'NONE', #9366, 0.1999999999999987899 ) ;
#53969 = CARTESIAN_POINT ( 'NONE',  ( 289.5000000000000000, -42.00000000000000000, 27.00000000000000000 ) ) ;
#53970 = EDGE_CURVE ( 'NONE', #53516, #7467, #43938, .T. ) ;
#53971 = APPLICATION_CONTEXT ( 'automotive_design' ) ;
#53972 = DIRECTION ( 'NONE',  ( -0.000000000000000000, 1.000000000000000000, 3.673940397442059868E-16 ) ) ;
#53973 = FACE_BOUND ( 'NONE', #61226, .T. ) ;
#53974 = LINE ( 'NONE', #33083, #42945 ) ;
#53975 = ADVANCED_FACE ( 'NONE', ( #55939 ), #38981, .F. ) ;
#53976 = DIRECTION ( 'NONE',  ( 0.000000000000000000, 1.000000000000000000, 0.000000000000000000 ) ) ;
#53977 = VECTOR ( 'NONE', #49686, 1000.000000000000000 ) ;
#53978 = ORIENTED_EDGE ( 'NONE', *, *, #6413, .T. ) ;
#53979 = CYLINDRICAL_SURFACE ( 'NONE', #67683, 0.1749999999999998224 ) ;
#53980 = FACE_OUTER_BOUND ( 'NONE', #41925, .T. ) ;
#53981 = EDGE_CURVE ( 'NONE', #56310, #67044, #2193, .T. ) ;
#53982 = PLANE ( 'NONE',  #26749 ) ;
#53983 = CARTESIAN_POINT ( 'NONE',  ( -7.955476262117326947, -9.737023737882770646, 54.00000000000000711 ) ) ;
#53984 = ORIENTED_EDGE ( 'NONE', *, *, #43723, .T. ) ;
#53985 = PLANE ( 'NONE',  #24214 ) ;
#53986 = EDGE_CURVE ( 'NONE', #26187, #62567, #28034, .T. ) ;
#53987 = DIRECTION ( 'NONE',  ( 0.000000000000000000, 1.000000000000000000, 0.000000000000000000 ) ) ;
#53988 = DIRECTION ( 'NONE',  ( -1.836970198721029934E-16, 1.836970198721036344E-16, -1.000000000000000000 ) ) ;
#53989 = DIRECTION ( 'NONE',  ( 0.000000000000000000, 0.000000000000000000, 1.000000000000000000 ) ) ;
#53990 = DIRECTION ( 'NONE',  ( 0.4999999999989371835, 0.000000000000000000, -0.8660254037850523279 ) ) ;
#53991 = EDGE_CURVE ( 'NONE', #13299, #29909, #49933, .T. ) ;
#53992 = CARTESIAN_POINT ( 'NONE',  ( 9.955011587777235604, -2.765062094116182312, 455.0000000000000568 ) ) ;
#53993 = ORIENTED_EDGE ( 'NONE', *, *, #25405, .T. ) ;
#53994 = VERTEX_POINT ( 'NONE', #7135 ) ;
#53995 = CYLINDRICAL_SURFACE ( 'NONE', #39440, 0.5999999999999998668 ) ;
#53996 = CARTESIAN_POINT ( 'NONE',  ( 7.250000000000005329, -8.249999999999998224, -26.00000000000001066 ) ) ;
#53997 = AXIS2_PLACEMENT_3D ( 'NONE', #58426, #47790, #31548 ) ;
#53999 = ORIENTED_EDGE ( 'NONE', *, *, #6473, .T. ) ;
#53998 = EDGE_CURVE ( 'NONE', #12276, #5787, #1844, .T. ) ;
#54000 = CARTESIAN_POINT ( 'NONE',  ( 3.857023737882779635, -10.31452373788281029, 54.00000000000000711 ) ) ;
#54001 = EDGE_CURVE ( 'NONE', #25655, #23009, #66202, .T. ) ;
#54002 = CARTESIAN_POINT ( 'NONE',  ( 24.90000000000000213, -21.00000000000001421, -13.86939075806900945 ) ) ;
#54003 = ADVANCED_FACE ( 'NONE', ( #17409, #60545 ), #65852, .F. ) ;
#54004 = ORIENTED_EDGE ( 'NONE', *, *, #65634, .T. ) ;
#54005 = ADVANCED_FACE ( 'NONE', ( #13142, #12435 ), #38644, .T. ) ;
#54006 = ADVANCED_FACE ( 'NONE', ( #44974 ), #66545, .T. ) ;
#54007 = DIRECTION ( 'NONE',  ( -0.000000000000000000, 3.673940397442059868E-16, -1.000000000000000000 ) ) ;
#54008 = ORIENTED_EDGE ( 'NONE', *, *, #62092, .T. ) ;
#54009 = ORIENTED_EDGE ( 'NONE', *, *, #44932, .F. ) ;
#54010 = LINE ( 'NONE', #48345, #9184 ) ;
#54011 = ORIENTED_EDGE ( 'NONE', *, *, #40317, .F. ) ;
#54012 = FACE_OUTER_BOUND ( 'NONE', #35383, .T. ) ;
#54013 = EDGE_CURVE ( 'NONE', #23929, #28003, #49595, .T. ) ;
#54014 = VECTOR ( 'NONE', #15570, 999.9999999999998863 ) ;
#54015 = DIRECTION ( 'NONE',  ( -1.000000000000000000, 0.000000000000000000, 0.000000000000000000 ) ) ;
#54016 = CARTESIAN_POINT ( 'NONE',  ( -4.383466043307859827, 8.393516549646589553, 455.0000000000000568 ) ) ;
#54017 = EDGE_CURVE ( 'NONE', #57464, #17601, #53133, .T. ) ;
#54018 = ORIENTED_EDGE ( 'NONE', *, *, #33066, .F. ) ;
#54019 = ORIENTED_EDGE ( 'NONE', *, *, #36272, .F. ) ;
#54020 = CARTESIAN_POINT ( 'NONE',  ( 6.006483450353379716, -6.006483450353490738, 455.0000000000000568 ) ) ;
#54021 = EDGE_CURVE ( 'NONE', #26524, #69579, #50633, .T. ) ;
#54022 = AXIS2_PLACEMENT_3D ( 'NONE', #14084, #18328, #40952 ) ;
#54024 = CARTESIAN_POINT ( 'NONE',  ( -7.450000000000001954, 7.250000000000000000, -7.000000000000000000 ) ) ;
#54023 = CARTESIAN_POINT ( 'NONE',  ( -8.593516549646697200, -4.396432944014498467, 195.0000000000000284 ) ) ;
#54025 = EDGE_LOOP ( 'NONE', ( #40860, #30117, #14362, #29006, #32095, #48457, #59012, #35282, #67555, #42712, #61525, #16274, #58197, #64024, #37399, #53953, #61719, #63231, #46731, #32435 ) ) ;
#54026 = VERTEX_POINT ( 'NONE', #45312 ) ;
#54028 = VERTEX_POINT ( 'NONE', #66880 ) ;
#54027 = PRODUCT_CONTEXT ( 'NONE', #28643, 'mechanical' ) ;
#54029 = LINE ( 'NONE', #69923, #60445 ) ;
#54030 = EDGE_CURVE ( 'NONE', #7633, #56088, #11307, .T. ) ;
#54032 = EDGE_LOOP ( 'NONE', ( #6489, #37249, #51492, #54776 ) ) ;
#54031 = DIRECTION ( 'NONE',  ( -1.000000000000000000, 0.000000000000000000, 0.000000000000000000 ) ) ;
#54033 = EDGE_CURVE ( 'NONE', #32512, #62786, #837, .T. ) ;
#54034 = VECTOR ( 'NONE', #48310, 1000.000000000000000 ) ;
#54035 = CARTESIAN_POINT ( 'NONE',  ( -10.30047626211725742, 3.650476262117184234, 54.00000000000000711 ) ) ;
#54036 = LINE ( 'NONE', #5243, #62182 ) ;
#54037 = ORIENTED_EDGE ( 'NONE', *, *, #55732, .F. ) ;
#54038 = EDGE_LOOP ( 'NONE', ( #8474, #30820, #10367, #11287 ) ) ;
#54039 = CYLINDRICAL_SURFACE ( 'NONE', #60607, 25.39999999999999858 ) ;
#54040 = EDGE_LOOP ( 'NONE', ( #25867, #10692, #25245, #32756 ) ) ;
#54041 = DIRECTION ( 'NONE',  ( 0.000000000000000000, 0.000000000000000000, 1.000000000000000000 ) ) ;
#54042 = DIRECTION ( 'NONE',  ( -0.000000000000000000, 3.673940397442059868E-16, -1.000000000000000000 ) ) ;
#54043 = EDGE_LOOP ( 'NONE', ( #20228, #54740, #9040, #4458 ) ) ;
#54044 = FACE_OUTER_BOUND ( 'NONE', #8611, .T. ) ;
#54045 = DIRECTION ( 'NONE',  ( 1.000000000000000000, 0.000000000000000000, 0.000000000000000000 ) ) ;
#54046 = ORIENTED_EDGE ( 'NONE', *, *, #23920, .F. ) ;
#54047 = ORIENTED_EDGE ( 'NONE', *, *, #30517, .T. ) ;
#54048 = LINE ( 'NONE', #27168, #33981 ) ;
#54049 = LINE ( 'NONE', #16566, #11520 ) ;
#54050 = DIRECTION ( 'NONE',  ( 0.000000000000000000, 0.000000000000000000, -1.000000000000000000 ) ) ;
#54051 = DIRECTION ( 'NONE',  ( -0.000000000000000000, -1.000000000000000000, 0.000000000000000000 ) ) ;
#54052 = CARTESIAN_POINT ( 'NONE',  ( 41.09999999999999432, -14.06939075806900163, 20.80000000000000426 ) ) ;
#54053 = ORIENTED_EDGE ( 'NONE', *, *, #407, .F. ) ;
#54054 = DIRECTION ( 'NONE',  ( 0.7071067811865411334, -0.7071067811865539010, -2.597868168706484541E-16 ) ) ;
#54055 = LINE ( 'NONE', #52672, #48555 ) ;
#54056 = LINE ( 'NONE', #33167, #5231 ) ;
#54057 = AXIS2_PLACEMENT_3D ( 'NONE', #63560, #31737, #3457 ) ;
#54058 = EDGE_CURVE ( 'NONE', #25620, #17134, #20350, .T. ) ;
#54060 = ORIENTED_EDGE ( 'NONE', *, *, #59543, .F. ) ;
#54059 = CARTESIAN_POINT ( 'NONE',  ( 8.250000000000005329, 7.250000000000000888, -26.00000000000001066 ) ) ;
#54061 = LINE ( 'NONE', #5956, #55057 ) ;
#54062 = CYLINDRICAL_SURFACE ( 'NONE', #52969, 1.000000000000000000 ) ;
#54063 = DIRECTION ( 'NONE',  ( 1.836970198721029934E-16, 1.836970198721010706E-16, -1.000000000000000000 ) ) ;
#54064 = EDGE_CURVE ( 'NONE', #31930, #44295, #57335, .T. ) ;
#54065 = AXIS2_PLACEMENT_3D ( 'NONE', #44354, #44018, #23845 ) ;
#54066 = CARTESIAN_POINT ( 'NONE',  ( -15.50000000000000000, -1.037157890325000054, 26.00000000000000000 ) ) ;
#54067 = ORIENTED_EDGE ( 'NONE', *, *, #38041, .T. ) ;
#54068 = DIRECTION ( 'NONE',  ( -0.4999999999999755196, 0.8660254037844526964, 2.509347957447861534E-16 ) ) ;
#54069 = ADVANCED_FACE ( 'NONE', ( #62630 ), #40722, .F. ) ;
#54070 = DIRECTION ( 'NONE',  ( 0.000000000000000000, 0.000000000000000000, 1.000000000000000000 ) ) ;
#54071 = ORIENTED_EDGE ( 'NONE', *, *, #14255, .T. ) ;
#54072 = LINE ( 'NONE', #32146, #32272 ) ;
#54073 = DIRECTION ( 'NONE',  ( 0.000000000000000000, 0.000000000000000000, -1.000000000000000000 ) ) ;
#54074 = CARTESIAN_POINT ( 'NONE',  ( 8.250000000000005329, 7.250000000000000888, -18.00000000000000000 ) ) ;
#54075 = EDGE_CURVE ( 'NONE', #51462, #28725, #22672, .T. ) ;
#54076 = DIRECTION ( 'NONE',  ( -1.836970198721029934E-16, -1.836970198721010706E-16, 1.000000000000000000 ) ) ;
#54077 = VECTOR ( 'NONE', #11765, 1000.000000000000000 ) ;
#54078 = DIRECTION ( 'NONE',  ( -0.7071067811865474617, 0.7071067811865474617, 0.000000000000000000 ) ) ;
#54079 = VERTEX_POINT ( 'NONE', #8184 ) ;
#54080 = VERTEX_POINT ( 'NONE', #56972 ) ;
#54081 = CARTESIAN_POINT ( 'NONE',  ( -4.727349090213463612, 7.798499376343949407, 455.0000000000000568 ) ) ;
#54082 = ORIENTED_EDGE ( 'NONE', *, *, #54841, .T. ) ;
#54083 = DIRECTION ( 'NONE',  ( 3.614007241618349165E-15, 1.000000000000000000, 0.000000000000000000 ) ) ;
#54084 = VERTEX_POINT ( 'NONE', #63348 ) ;
#54085 = LINE ( 'NONE', #65039, #43845 ) ;
#54086 = EDGE_CURVE ( 'NONE', #35382, #26427, #25522, .T. ) ;
#54087 = DIRECTION ( 'NONE',  ( 0.000000000000000000, 0.000000000000000000, 1.000000000000000000 ) ) ;
#54088 = DIRECTION ( 'NONE',  ( 1.000000000000000000, 0.000000000000000000, 0.000000000000000000 ) ) ;
#54089 = VERTEX_POINT ( 'NONE', #40376 ) ;
#54090 = VERTEX_POINT ( 'NONE', #67949 ) ;
#54091 = CARTESIAN_POINT ( 'NONE',  ( -8.393516549646712122, 5.655420232009161552, 455.0000000000000568 ) ) ;
#54092 = VERTEX_POINT ( 'NONE', #19150 ) ;
#54093 = ORIENTED_EDGE ( 'NONE', *, *, #16355, .F. ) ;
#54094 = DIRECTION ( 'NONE',  ( 0.7071067811865474617, 0.7071067811865474617, 2.597868168706479611E-16 ) ) ;
#54095 = PLANE ( 'NONE',  #42603 ) ;
#54096 = DIRECTION ( 'NONE',  ( 1.000000000000000000, 0.000000000000000000, 0.000000000000000000 ) ) ;
#54097 = ORIENTED_EDGE ( 'NONE', *, *, #60291, .T. ) ;
#54098 = DIRECTION ( 'NONE',  ( 1.000000000000000000, -3.491481338843133750E-15, -1.836970198721036590E-16 ) ) ;
#54100 = DIRECTION ( 'NONE',  ( 0.000000000000000000, 0.000000000000000000, 1.000000000000000000 ) ) ;
#54099 = CARTESIAN_POINT ( 'NONE',  ( 10.31889768521803141, -25.34729925119248151, 17.15270074880751494 ) ) ;
#54101 = EDGE_LOOP ( 'NONE', ( #42791, #28092, #67822, #50060 ) ) ;
#54102 = VERTEX_POINT ( 'NONE', #46370 ) ;
#54104 = ORIENTED_EDGE ( 'NONE', *, *, #20622, .T. ) ;
#54103 = CARTESIAN_POINT ( 'NONE',  ( -5.242976262117259978, 5.242976262117182706, 26.00000000000000711 ) ) ;
#54105 = ORIENTED_EDGE ( 'NONE', *, *, #63649, .T. ) ;
#54106 = VECTOR ( 'NONE', #43990, 1000.000000000000000 ) ;
#54107 = DIRECTION ( 'NONE',  ( 1.000000000000000000, 0.000000000000000000, 0.000000000000000000 ) ) ;
#54108 = EDGE_CURVE ( 'NONE', #28277, #56701, #51693, .T. ) ;
#54109 = CIRCLE ( 'NONE', #31549, 3.499999999999855227 ) ;
#54110 = EDGE_CURVE ( 'NONE', #57928, #2646, #57684, .T. ) ;
#54111 = PLANE ( 'NONE',  #6768 ) ;
#54112 = ORIENTED_EDGE ( 'NONE', *, *, #57467, .F. ) ;
#54114 = VERTEX_POINT ( 'NONE', #8891 ) ;
#54113 = EDGE_CURVE ( 'NONE', #28873, #17252, #68657, .T. ) ;
#54115 = VECTOR ( 'NONE', #69794, 1000.000000000000000 ) ;
#54116 = CARTESIAN_POINT ( 'NONE',  ( 4.961189459950046121, 7.342976262117201003, 54.00000000000000711 ) ) ;
#54117 = DIRECTION ( 'NONE',  ( 0.000000000000000000, 0.000000000000000000, -1.000000000000000000 ) ) ;
#54118 = ORIENTED_EDGE ( 'NONE', *, *, #44426, .F. ) ;
#54119 = VERTEX_POINT ( 'NONE', #30110 ) ;
#54120 = VECTOR ( 'NONE', #62805, 1000.000000000000000 ) ;
#54121 = CARTESIAN_POINT ( 'NONE',  ( 7.450000000000004619, -1.336933437520057563E-15, -21.50000000000000000 ) ) ;
#54122 = LINE ( 'NONE', #5682, #6420 ) ;
#54123 = CARTESIAN_POINT ( 'NONE',  ( 6.872275254348426010, -3.003254798005752235, 26.00000000000000711 ) ) ;
#54124 = VERTEX_POINT ( 'NONE', #62281 ) ;
#54126 = CIRCLE ( 'NONE', #27016, 4.000000000000000888 ) ;
#54125 = CIRCLE ( 'NONE', #69908, 2.204799999999997429 ) ;
#54127 = DIRECTION ( 'NONE',  ( 0.000000000000000000, 0.000000000000000000, -1.000000000000000000 ) ) ;
#54128 = DIRECTION ( 'NONE',  ( -0.000000000000000000, 0.000000000000000000, -1.000000000000000000 ) ) ;
#54130 = ORIENTED_EDGE ( 'NONE', *, *, #43617, .T. ) ;
#54129 = DIRECTION ( 'NONE',  ( 0.000000000000000000, 0.7071067811865474617, 0.7071067811865474617 ) ) ;
#54132 = EDGE_LOOP ( 'NONE', ( #53321, #62261, #3580, #39803 ) ) ;
#54131 = DIRECTION ( 'NONE',  ( -0.000000000000000000, 3.673940397442059868E-16, -1.000000000000000000 ) ) ;
#54133 = DIRECTION ( 'NONE',  ( 0.000000000000000000, -1.000000000000000000, 0.000000000000000000 ) ) ;
#54134 = AXIS2_PLACEMENT_3D ( 'NONE', #62632, #64068, #31879 ) ;
#54135 = CARTESIAN_POINT ( 'NONE',  ( -7.250000000000001776, -7.249999999999998224, -25.00000000000000000 ) ) ;
#54136 = CARTESIAN_POINT ( 'NONE',  ( 8.835729544836338434, -2.544523737882816050, 26.00000000000000711 ) ) ;
#54137 = CARTESIAN_POINT ( 'NONE',  ( -11.29351654964668583, 8.513516549646642062, 455.0000000000000568 ) ) ;
#54138 = CARTESIAN_POINT ( 'NONE',  ( 11.00000000000000000, -5.200000000000001066, 26.59999999999999432 ) ) ;
#54139 = CARTESIAN_POINT ( 'NONE',  ( 8.250000000000005329, -8.249999999999998224, -26.00000000000001066 ) ) ;
#54140 = ORIENTED_EDGE ( 'NONE', *, *, #61369, .T. ) ;
#54141 = DIRECTION ( 'NONE',  ( 1.000000000000000000, 0.000000000000000000, 0.000000000000000000 ) ) ;
#54143 = VERTEX_POINT ( 'NONE', #67246 ) ;
#54142 = DIRECTION ( 'NONE',  ( 0.000000000000000000, 0.000000000000000000, -1.000000000000000000 ) ) ;
#54144 = EDGE_CURVE ( 'NONE', #51803, #6097, #13624, .T. ) ;
#54146 = ORIENTED_EDGE ( 'NONE', *, *, #56429, .F. ) ;
#54145 = FACE_OUTER_BOUND ( 'NONE', #13289, .T. ) ;
#54147 = DIRECTION ( 'NONE',  ( -1.000000000000000000, 0.000000000000000000, 0.000000000000000000 ) ) ;
#54148 = VECTOR ( 'NONE', #24439, 1000.000000000000000 ) ;
#54149 = CARTESIAN_POINT ( 'NONE',  ( 14.25000000000000000, -0.2038245569916330158, -23.22168783648699986 ) ) ;
#54150 = ADVANCED_FACE ( 'NONE', ( #20202 ), #41763, .T. ) ;
#54151 = ORIENTED_EDGE ( 'NONE', *, *, #66098, .T. ) ;
#54152 = PLANE ( 'NONE',  #57991 ) ;
#54153 = EDGE_CURVE ( 'NONE', #66814, #57287, #30463, .T. ) ;
#54154 = CYLINDRICAL_SURFACE ( 'NONE', #39588, 3.499999999999055866 ) ;
#54155 = EDGE_CURVE ( 'NONE', #26887, #16332, #13495, .T. ) ;
#54156 = EDGE_LOOP ( 'NONE', ( #67760, #18404, #69711, #66430 ) ) ;
#54157 = AXIS2_PLACEMENT_3D ( 'NONE', #39806, #23557, #2344 ) ;
#54158 = DIRECTION ( 'NONE',  ( 0.000000000000000000, -1.000000000000000000, -0.000000000000000000 ) ) ;
#54159 = FACE_OUTER_BOUND ( 'NONE', #14721, .T. ) ;
#54160 = DIRECTION ( 'NONE',  ( 0.000000000000000000, 0.000000000000000000, -1.000000000000000000 ) ) ;
#54161 = EDGE_CURVE ( 'NONE', #28070, #31078, #29406, .T. ) ;
#54162 = EDGE_CURVE ( 'NONE', #32793, #35449, #19849, .T. ) ;
#54163 = VECTOR ( 'NONE', #44222, 1000.000000000000114 ) ;
#54164 = CIRCLE ( 'NONE', #8962, 1.000000000000000888 ) ;
#54165 = EDGE_CURVE ( 'NONE', #45304, #10852, #24465, .T. ) ;
#54166 = VERTEX_POINT ( 'NONE', #50980 ) ;
#54167 = CARTESIAN_POINT ( 'NONE',  ( 283.0000000000000568, -39.80000000000000426, 12.69999999999999929 ) ) ;
#54168 = ORIENTED_EDGE ( 'NONE', *, *, #35522, .F. ) ;
#54169 = VERTEX_POINT ( 'NONE', #2534 ) ;
#54170 = VECTOR ( 'NONE', #36841, 1000.000000000000000 ) ;
#54171 = CARTESIAN_POINT ( 'NONE',  ( 7.000000000000000000, -25.93000000000544958, -9.412893218815410634 ) ) ;
#54172 = LINE ( 'NONE', #32599, #43278 ) ;
#54173 = AXIS2_PLACEMENT_3D ( 'NONE', #11686, #27620, #59798 ) ;
#54174 = DIRECTION ( 'NONE',  ( 1.000000000000000000, 0.000000000000000000, 0.000000000000000000 ) ) ;
#54175 = LINE ( 'NONE', #54518, #20487 ) ;
#54176 = ORIENTED_EDGE ( 'NONE', *, *, #67595, .T. ) ;
#54177 = EDGE_LOOP ( 'NONE', ( #51407, #34236, #59160, #36160 ) ) ;
#54179 = ORIENTED_EDGE ( 'NONE', *, *, #3259, .F. ) ;
#54178 = DIRECTION ( 'NONE',  ( 0.000000000000000000, 0.000000000000000000, -1.000000000000000000 ) ) ;
#54180 = ORIENTED_EDGE ( 'NONE', *, *, #53602, .F. ) ;
#54181 = CIRCLE ( 'NONE', #34903, 0.1999999999999996503 ) ;
#54182 = DIRECTION ( 'NONE',  ( -1.000000000000000000, 0.000000000000000000, 0.000000000000000000 ) ) ;
#54183 = DIRECTION ( 'NONE',  ( -1.000000000000000000, 0.000000000000000000, 0.000000000000000000 ) ) ;
#54184 = CARTESIAN_POINT ( 'NONE',  ( -9.791916549646712653, 10.19191654964664018, 455.0000000000000568 ) ) ;
#54185 = FACE_BOUND ( 'NONE', #12921, .T. ) ;
#54186 = VECTOR ( 'NONE', #27135, 1000.000000000000000 ) ;
#54188 = DIRECTION ( 'NONE',  ( -0.000000000000000000, -0.000000000000000000, 1.000000000000000000 ) ) ;
#54187 = CARTESIAN_POINT ( 'NONE',  ( 11.18999999999999950, 11.25000000000000178, -5.000000000000000000 ) ) ;
#54189 = ORIENTED_EDGE ( 'NONE', *, *, #59944, .F. ) ;
#54191 = ORIENTED_EDGE ( 'NONE', *, *, #229, .T. ) ;
#54190 = CARTESIAN_POINT ( 'NONE',  ( 11.32648345035337734, -7.806483450353395526, 195.0000000000000284 ) ) ;
#54192 = EDGE_LOOP ( 'NONE', ( #25198, #55814, #15235, #63558 ) ) ;
#54193 = EDGE_LOOP ( 'NONE', ( #67500, #42196, #66676, #43399 ) ) ;
#54194 = CARTESIAN_POINT ( 'NONE',  ( -6.500000000000002665, 6.500000000000002665, 0.000000000000000000 ) ) ;
#54195 = PLANE ( 'NONE',  #28697 ) ;
#54196 = ADVANCED_FACE ( 'NONE', ( #4653 ), #36467, .F. ) ;
#54197 = CARTESIAN_POINT ( 'NONE',  ( 49.00000000000000000, 20.60000000000000142, -13.86939075806900057 ) ) ;
#54198 = CIRCLE ( 'NONE', #23675, 1.399999999999999245 ) ;
#54199 = ORIENTED_EDGE ( 'NONE', *, *, #57016, .T. ) ;
#54200 = ORIENTED_EDGE ( 'NONE', *, *, #15687, .T. ) ;
#54201 = ORIENTED_EDGE ( 'NONE', *, *, #51404, .T. ) ;
#54202 = ADVANCED_FACE ( 'NONE', ( #68995 ), #64063, .T. ) ;
#54203 = EDGE_CURVE ( 'NONE', #37838, #51193, #59436, .T. ) ;
#54204 = DIRECTION ( 'NONE',  ( -1.000000000000000000, 2.135044278125299371E-15, 0.000000000000000000 ) ) ;
#54205 = LINE ( 'NONE', #812, #423 ) ;
#54206 = CARTESIAN_POINT ( 'NONE',  ( -10.30047626211725742, 3.842976262117182351, 26.00000000000000711 ) ) ;
#54207 = EDGE_CURVE ( 'NONE', #28131, #53754, #37870, .T. ) ;
#54208 = ORIENTED_EDGE ( 'NONE', *, *, #14695, .T. ) ;
#54209 = ORIENTED_EDGE ( 'NONE', *, *, #41518, .T. ) ;
#54210 = DIRECTION ( 'NONE',  ( -0.4999999999999170108, 0.000000000000000000, 0.8660254037844865582 ) ) ;
#54211 = CARTESIAN_POINT ( 'NONE',  ( 283.0000000000000568, -42.50000000000000000, 15.10000000000000142 ) ) ;
#54212 = VECTOR ( 'NONE', #39782, 1000.000000000000000 ) ;
#54213 = ORIENTED_EDGE ( 'NONE', *, *, #36705, .T. ) ;
#54214 = VECTOR ( 'NONE', #34892, 1000.000000000000000 ) ;
#54215 = FACE_OUTER_BOUND ( 'NONE', #3841, .T. ) ;
#54217 = VERTEX_POINT ( 'NONE', #14908 ) ;
#54216 = DIRECTION ( 'NONE',  ( 0.000000000000000000, 0.7071067811865474617, -0.7071067811865474617 ) ) ;
#54218 = ORIENTED_EDGE ( 'NONE', *, *, #38870, .T. ) ;
#54219 = AXIS2_PLACEMENT_3D ( 'NONE', #66023, #650, #48741 ) ;
#54220 = CARTESIAN_POINT ( 'NONE',  ( -10.08346604330797369, -9.106483450353383802, 455.0000000000000568 ) ) ;
#54221 = LINE ( 'NONE', #21688, #51520 ) ;
#54222 = DIRECTION ( 'NONE',  ( 0.6414496315691565753, -0.7671651518153006499, -2.818519042764004597E-16 ) ) ;
#54223 = CARTESIAN_POINT ( 'NONE',  ( 7.532023737882817649, -3.848229544836346605, 54.00000000000000711 ) ) ;
#54224 = AXIS2_PLACEMENT_3D ( 'NONE', #34200, #61075, #22242 ) ;
#54225 = DIRECTION ( 'NONE',  ( -1.836970198721029934E-16, -1.836970198721010706E-16, 1.000000000000000000 ) ) ;
#54226 = AXIS2_PLACEMENT_3D ( 'NONE', #51757, #46097, #46787 ) ;
#54227 = EDGE_LOOP ( 'NONE', ( #54238, #42220, #36691, #54606 ) ) ;
#54228 = DIRECTION ( 'NONE',  ( 1.000000000000000000, -0.000000000000000000, -0.000000000000000000 ) ) ;
#54229 = AXIS2_PLACEMENT_3D ( 'NONE', #36488, #42140, #58062 ) ;
#54230 = VERTEX_POINT ( 'NONE', #26214 ) ;
#54231 = CARTESIAN_POINT ( 'NONE',  ( 1.000000000000000000, -21.00000000000000000, -5.000000000000000000 ) ) ;
#54232 = CARTESIAN_POINT ( 'NONE',  ( 10.50702373788280752, 6.835476262117182067, 54.00000000000000711 ) ) ;
#54233 = FACE_OUTER_BOUND ( 'NONE', #16492, .T. ) ;
#54234 = DIRECTION ( 'NONE',  ( -0.000000000000000000, -0.000000000000000000, 1.000000000000000000 ) ) ;
#54235 = VECTOR ( 'NONE', #39661, 1000.000000000000000 ) ;
#54236 = AXIS2_PLACEMENT_3D ( 'NONE', #50431, #46510, #29195 ) ;
#54237 = FACE_OUTER_BOUND ( 'NONE', #3260, .T. ) ;
#54238 = ORIENTED_EDGE ( 'NONE', *, *, #50221, .T. ) ;
#54239 = CARTESIAN_POINT ( 'NONE',  ( 25.90000000000000213, -0.1999999999911795112, 8.826273045769999343E-12 ) ) ;
#54240 = EDGE_CURVE ( 'NONE', #15827, #8176, #10303, .T. ) ;
#54241 = PLANE ( 'NONE',  #27725 ) ;
#54242 = EDGE_CURVE ( 'NONE', #39584, #38450, #53442, .T. ) ;
#54243 = VERTEX_POINT ( 'NONE', #36836 ) ;
#54244 = VECTOR ( 'NONE', #51579, 1000.000000000000114 ) ;
#54245 = DIRECTION ( 'NONE',  ( -0.000000000000000000, -0.000000000000000000, -1.000000000000000000 ) ) ;
#54246 = DIRECTION ( 'NONE',  ( -1.836970198721029934E-16, 1.836970198721036590E-16, -1.000000000000000000 ) ) ;
#54247 = ORIENTED_EDGE ( 'NONE', *, *, #36968, .T. ) ;
#54248 = LINE ( 'NONE', #33017, #55020 ) ;
#54249 = DIRECTION ( 'NONE',  ( -8.951101527228104953E-17, -1.000000000000000000, 0.000000000000000000 ) ) ;
#54250 = VERTEX_POINT ( 'NONE', #64738 ) ;
#54251 = DIRECTION ( 'NONE',  ( 0.5773502691896237327, 0.5773502691896237327, 0.5773502691896298389 ) ) ;
#54252 = CARTESIAN_POINT ( 'NONE',  ( 7.428221114745003462, -3.606483450353490827, 455.0000000000000568 ) ) ;
#54253 = DIRECTION ( 'NONE',  ( 0.000000000000000000, 0.000000000000000000, -1.000000000000000000 ) ) ;
#54254 = LINE ( 'NONE', #874, #41887 ) ;
#54255 = ORIENTED_EDGE ( 'NONE', *, *, #39808, .F. ) ;
#54256 = AXIS2_PLACEMENT_3D ( 'NONE', #10284, #53428, #4979 ) ;
#54258 = EDGE_LOOP ( 'NONE', ( #25197, #8694, #45483, #2892 ) ) ;
#54257 = DIRECTION ( 'NONE',  ( 1.000000000000000000, -8.951101527228104953E-17, 0.000000000000000000 ) ) ;
#54259 = ADVANCED_FACE ( 'NONE', ( #47773 ), #10637, .T. ) ;
#54260 = AXIS2_PLACEMENT_3D ( 'NONE', #45429, #41178, #18562 ) ;
#54261 = CARTESIAN_POINT ( 'NONE',  ( 275.0000000000000000, -20.40000000000000213, 12.40000000000000213 ) ) ;
#54262 = DIRECTION ( 'NONE',  ( -5.981805089575196197E-17, -1.000000000000000000, 0.000000000000000000 ) ) ;
#54263 = LINE ( 'NONE', #27037, #68036 ) ;
#54264 = EDGE_LOOP ( 'NONE', ( #14802, #59812, #40535, #38721, #13978, #9770, #67380, #5500, #17458, #1643, #62550, #26332, #8954, #28650, #61838, #7267, #37976, #43374, #65997, #56042 ) ) ;
#54265 = CIRCLE ( 'NONE', #21494, 3.500000000000003109 ) ;
#54266 = DIRECTION ( 'NONE',  ( 1.000000000000000000, 0.000000000000000000, 0.000000000000000000 ) ) ;
#54267 = DIRECTION ( 'NONE',  ( -2.135044278125299371E-15, 1.000000000000000000, -0.000000000000000000 ) ) ;
#54268 = ORIENTED_EDGE ( 'NONE', *, *, #45909, .F. ) ;
#54269 = ORIENTED_EDGE ( 'NONE', *, *, #27905, .F. ) ;
#54270 = CIRCLE ( 'NONE', #23701, 4.500000000000190958 ) ;
#54271 = ORIENTED_EDGE ( 'NONE', *, *, #41193, .F. ) ;
#54272 = AXIS2_PLACEMENT_3D ( 'NONE', #33662, #29047, #49919 ) ;
#54273 = DIRECTION ( 'NONE',  ( -9.912705577010336396E-15, -1.000000000000000000, 0.000000000000000000 ) ) ;
#54274 = DIRECTION ( 'NONE',  ( 0.000000000000000000, 0.000000000000000000, 1.000000000000000000 ) ) ;
#54275 = ORIENTED_EDGE ( 'NONE', *, *, #3314, .T. ) ;
#54276 = ORIENTED_EDGE ( 'NONE', *, *, #39420, .F. ) ;
#54277 = EDGE_LOOP ( 'NONE', ( #62273, #27991, #62923, #44067 ) ) ;
#54279 = DIRECTION ( 'NONE',  ( 1.000000000000000000, -0.000000000000000000, -0.000000000000000000 ) ) ;
#54278 = AXIS2_PLACEMENT_3D ( 'NONE', #61933, #13847, #19498 ) ;
#54280 = AXIS2_PLACEMENT_3D ( 'NONE', #57042, #24171, #17829 ) ;
#54281 = ORIENTED_EDGE ( 'NONE', *, *, #33560, .F. ) ;
#54282 = VERTEX_POINT ( 'NONE', #32215 ) ;
#54283 = ADVANCED_FACE ( 'NONE', ( #69342 ), #31183, .F. ) ;
#54284 = ORIENTED_EDGE ( 'NONE', *, *, #50787, .F. ) ;
#54285 = ORIENTED_EDGE ( 'NONE', *, *, #60026, .F. ) ;
#54286 = DIRECTION ( 'NONE',  ( -1.000000000000000000, 0.000000000000000000, 0.000000000000000000 ) ) ;
#54287 = UNCERTAINTY_MEASURE_WITH_UNIT (LENGTH_MEASURE( 1.000000000000000082E-05 ), #43281, 'distance_accuracy_value', 'NONE');
#54289 = ORIENTED_EDGE ( 'NONE', *, *, #27943, .F. ) ;
#54288 = DIRECTION ( 'NONE',  ( 0.000000000000000000, 0.6857142857142869419, -0.7278708115918273158 ) ) ;
#54290 = DIRECTION ( 'NONE',  ( 0.7671651518153065341, -0.6414496315691495809, 0.000000000000000000 ) ) ;
#54291 = CARTESIAN_POINT ( 'NONE',  ( 283.0000000000000568, -31.30000000000095284, 12.19999999999906315 ) ) ;
#54292 = AXIS2_PLACEMENT_3D ( 'NONE', #48019, #42362, #37418 ) ;
#54293 = CARTESIAN_POINT ( 'NONE',  ( 283.0000000000000568, -37.15000000000001279, -7.700000000000000178 ) ) ;
#54294 = ORIENTED_EDGE ( 'NONE', *, *, #36583, .T. ) ;
#54295 = EDGE_CURVE ( 'NONE', #47155, #63841, #15620, .T. ) ;
#54296 = DIRECTION ( 'NONE',  ( -5.981805089575196197E-17, -1.000000000000000000, 0.000000000000000000 ) ) ;
#54297 = EDGE_CURVE ( 'NONE', #41637, #53484, #37185, .T. ) ;
#54298 = VECTOR ( 'NONE', #27766, 1000.000000000000000 ) ;
#54299 = VERTEX_POINT ( 'NONE', #58745 ) ;
#54300 = CARTESIAN_POINT ( 'NONE',  ( 2.664535259100375697E-15, -20.50000000000000355, -17.79289321881343611 ) ) ;
#54301 = DIRECTION ( 'NONE',  ( -0.000000000000000000, 3.673940397442059868E-16, -1.000000000000000000 ) ) ;
#54302 = VECTOR ( 'NONE', #28275, 1000.000000000000000 ) ;
#54303 = DIRECTION ( 'NONE',  ( 0.000000000000000000, 0.000000000000000000, -1.000000000000000000 ) ) ;
#54304 = DIRECTION ( 'NONE',  ( 1.000000000000000000, 0.000000000000000000, 0.000000000000000000 ) ) ;
#54305 = ORIENTED_EDGE ( 'NONE', *, *, #33563, .F. ) ;
#54307 = CARTESIAN_POINT ( 'NONE',  ( 15.00000000000000000, -0.5000000000000000000, -27.00000000000000000 ) ) ;
#54306 = AXIS2_PLACEMENT_3D ( 'NONE', #44208, #23680, #66128 ) ;
#54308 = DIRECTION ( 'NONE',  ( 1.000000000000000000, -1.047444401652940164E-14, 0.000000000000000000 ) ) ;
#54309 = DIRECTION ( 'NONE',  ( 0.000000000000000000, 0.000000000000000000, -1.000000000000000000 ) ) ;
#54310 = AXIS2_PLACEMENT_3D ( 'NONE', #26768, #48331, #37038 ) ;
#54311 = AXIS2_PLACEMENT_3D ( 'NONE', #67812, #56839, #46938 ) ;
#54312 = PLANE ( 'NONE',  #46635 ) ;
#54313 = CYLINDRICAL_SURFACE ( 'NONE', #58456, 0.4999999999991868727 ) ;
#54314 = DIRECTION ( 'NONE',  ( -1.000000000000000000, 0.000000000000000000, 0.000000000000000000 ) ) ;
#54315 =( NAMED_UNIT ( * ) PLANE_ANGLE_UNIT ( ) SI_UNIT ( $, .RADIAN. ) );
#54316 = VECTOR ( 'NONE', #56321, 1000.000000000000000 ) ;
#54317 = LINE ( 'NONE', #11502, #56013 ) ;
#54318 = EDGE_CURVE ( 'NONE', #55467, #1208, #58404, .T. ) ;
#54319 = EDGE_CURVE ( 'NONE', #10593, #46953, #26563, .T. ) ;
#54320 = ORIENTED_EDGE ( 'NONE', *, *, #39086, .T. ) ;
#54321 = CARTESIAN_POINT ( 'NONE',  ( -10.49297626211729551, -6.849523737882748264, 54.00000000000000711 ) ) ;
#54322 = EDGE_CURVE ( 'NONE', #10926, #59069, #47421, .T. ) ;
#54323 = CARTESIAN_POINT ( 'NONE',  ( -3.650476262117223314, 10.30047626211716683, 26.00000000000000711 ) ) ;
#54324 = VECTOR ( 'NONE', #66019, 1000.000000000000000 ) ;
#54325 = CARTESIAN_POINT ( 'NONE',  ( -11.00000000000000000, -11.50000000000100009, 19.50000000000103739 ) ) ;
#54326 = LINE ( 'NONE', #48323, #33034 ) ;
#54327 = ORIENTED_EDGE ( 'NONE', *, *, #49962, .F. ) ;
#54328 = CYLINDRICAL_SURFACE ( 'NONE', #51312, 0.1999999999999992339 ) ;
#54329 = CARTESIAN_POINT ( 'NONE',  ( -6.651770455163783957, -7.532023737882790115, 54.00000000000000711 ) ) ;
#54330 = EDGE_CURVE ( 'NONE', #60107, #57546, #64400, .T. ) ;
#54331 = CARTESIAN_POINT ( 'NONE',  ( 8.250000000000005329, 0.000000000000000000, -13.50000000000000178 ) ) ;
#54332 = EDGE_CURVE ( 'NONE', #18330, #10391, #48480, .T. ) ;
#54333 = DIRECTION ( 'NONE',  ( 1.000000000000000000, 0.000000000000000000, 0.000000000000000000 ) ) ;
#54334 = CARTESIAN_POINT ( 'NONE',  ( 158.8349105750994568, -33.83962462487175316, 5.000000000000000000 ) ) ;
#54335 = EDGE_CURVE ( 'NONE', #8176, #20324, #7960, .T. ) ;
#54336 = FACE_OUTER_BOUND ( 'NONE', #20256, .T. ) ;
#54337 = VERTEX_POINT ( 'NONE', #10995 ) ;
#54338 = EDGE_CURVE ( 'NONE', #32551, #47033, #27269, .T. ) ;
#54339 = EDGE_LOOP ( 'NONE', ( #40619, #55275, #65095, #24804 ) ) ;
#54340 = CYLINDRICAL_SURFACE ( 'NONE', #69938, 0.1999999999999987899 ) ;
#54341 = DIRECTION ( 'NONE',  ( -0.000000000000000000, -0.000000000000000000, -1.000000000000000000 ) ) ;
#54342 = ORIENTED_EDGE ( 'NONE', *, *, #744, .T. ) ;
#54343 = CARTESIAN_POINT ( 'NONE',  ( 11.25000000000000178, 11.18999999999999950, -4.250000000000000000 ) ) ;
#54344 = VERTEX_POINT ( 'NONE', #6712 ) ;
#54345 = FACE_BOUND ( 'NONE', #25216, .T. ) ;
#54346 = EDGE_LOOP ( 'NONE', ( #14497, #63315, #58712, #51007 ) ) ;
#54347 = ORIENTED_EDGE ( 'NONE', *, *, #50942, .T. ) ;
#54348 = CARTESIAN_POINT ( 'NONE',  ( 8.835729544836325999, 8.130476262117191766, 26.00000000000000711 ) ) ;
#54349 = VECTOR ( 'NONE', #3329, 1000.000000000000000 ) ;
#54350 = ORIENTED_EDGE ( 'NONE', *, *, #27442, .T. ) ;
#54351 = DIRECTION ( 'NONE',  ( 0.000000000000000000, 1.000000000000000000, 0.000000000000000000 ) ) ;
#54352 = DIRECTION ( 'NONE',  ( 3.491481338843133355E-15, 1.000000000000000000, 0.000000000000000000 ) ) ;
#54353 = LINE ( 'NONE', #60684, #67486 ) ;
#54354 = AXIS2_PLACEMENT_3D ( 'NONE', #14540, #36824, #51682 ) ;
#54355 = ADVANCED_FACE ( 'NONE', ( #2110 ), #39241, .T. ) ;
#54356 = ORIENTED_EDGE ( 'NONE', *, *, #31816, .T. ) ;
#54357 = ORIENTED_EDGE ( 'NONE', *, *, #49480, .F. ) ;
#54358 = VECTOR ( 'NONE', #54070, 1000.000000000000000 ) ;
#54359 = DIRECTION ( 'NONE',  ( 0.000000000000000000, 0.000000000000000000, -1.000000000000000000 ) ) ;
#54360 = LINE ( 'NONE', #12236, #32764 ) ;
#54361 = VERTEX_POINT ( 'NONE', #23667 ) ;
#54362 = ORIENTED_EDGE ( 'NONE', *, *, #53384, .T. ) ;
#54363 = VECTOR ( 'NONE', #11446, 1000.000000000000000 ) ;
#54364 = AXIS2_PLACEMENT_3D ( 'NONE', #34485, #66338, #11534 ) ;
#54365 = ADVANCED_FACE ( 'NONE', ( #1756 ), #28284, .T. ) ;
#54367 = ORIENTED_EDGE ( 'NONE', *, *, #30128, .F. ) ;
#54366 = CONTEXT_DEPENDENT_SHAPE_REPRESENTATION ( #10181, #12619 ) ;
#54368 = CARTESIAN_POINT ( 'NONE',  ( 14.10805890929250062, -5.000000000000000000, 26.25000000000000000 ) ) ;
#54370 = ORIENTED_EDGE ( 'NONE', *, *, #54086, .T. ) ;
#54369 = DIRECTION ( 'NONE',  ( 0.6414496315691469164, -0.7671651518153088656, -2.587583378555128790E-16 ) ) ;
#54371 = CIRCLE ( 'NONE', #56622, 4.000000000000000000 ) ;
#54372 = CARTESIAN_POINT ( 'NONE',  ( 170.5922698879802226, -35.25383818724483831, 0.000000000000000000 ) ) ;
#54373 = CARTESIAN_POINT ( 'NONE',  ( -8.693516549646711056, 11.11351654964659730, 455.0000000000000568 ) ) ;
#54374 = EDGE_LOOP ( 'NONE', ( #64761, #8706, #45535, #68010 ) ) ;
#54375 = ORIENTED_EDGE ( 'NONE', *, *, #18200, .T. ) ;
#54376 = CIRCLE ( 'NONE', #63409, 1.000000000000000000 ) ;
#54377 = ORIENTED_EDGE ( 'NONE', *, *, #54207, .F. ) ;
#54378 = DIRECTION ( 'NONE',  ( 1.000000000000000000, 0.000000000000000000, 0.000000000000000000 ) ) ;
#54379 = LINE ( 'NONE', #22199, #64034 ) ;
#54380 = EDGE_CURVE ( 'NONE', #48238, #40825, #66460, .T. ) ;
#54381 = ORIENTED_EDGE ( 'NONE', *, *, #57084, .F. ) ;
#54382 = CARTESIAN_POINT ( 'NONE',  ( -6.344366288193410419, 4.706725378239148050, 26.00000000000000711 ) ) ;
#54383 = DIRECTION ( 'NONE',  ( -1.000000000000000000, 0.000000000000000000, 0.000000000000000000 ) ) ;
#54384 = EDGE_CURVE ( 'NONE', #42854, #27322, #23772, .T. ) ;
#54386 = EDGE_LOOP ( 'NONE', ( #66070, #42374, #5440, #59133 ) ) ;
#54385 = DIRECTION ( 'NONE',  ( 1.000000000000000000, -0.000000000000000000, 0.000000000000000000 ) ) ;
#54387 = VERTEX_POINT ( 'NONE', #49855 ) ;
#54388 = ADVANCED_FACE ( 'NONE', ( #50553 ), #27947, .F. ) ;
#54389 = DIRECTION ( 'NONE',  ( 0.000000000000000000, -0.7071067811865474617, 0.7071067811865474617 ) ) ;
#54390 = CARTESIAN_POINT ( 'NONE',  ( -11.29351654964668583, 8.513516549646642062, 195.0000000000000284 ) ) ;
#54391 = EDGE_CURVE ( 'NONE', #1029, #41033, #54488, .T. ) ;
#54392 = DIRECTION ( 'NONE',  ( 0.000000000000000000, -1.000000000000000000, 0.000000000000000000 ) ) ;
#54393 = EDGE_CURVE ( 'NONE', #4451, #45572, #44109, .T. ) ;
#54394 = ADVANCED_FACE ( 'NONE', ( #28626 ), #17678, .T. ) ;
#54395 = LINE ( 'NONE', #44112, #59960 ) ;
#54396 = PLANE ( 'NONE',  #19482 ) ;
#54397 = ORIENTED_EDGE ( 'NONE', *, *, #35120, .F. ) ;
#54398 = PLANE ( 'NONE',  #13196 ) ;
#54399 = DIRECTION ( 'NONE',  ( -1.000000000000000000, 0.000000000000000000, 0.000000000000000000 ) ) ;
#54400 = VECTOR ( 'NONE', #64733, 1000.000000000000114 ) ;
#54401 = EDGE_CURVE ( 'NONE', #54664, #24168, #1414, .T. ) ;
#54402 = DIRECTION ( 'NONE',  ( 0.000000000000000000, 0.000000000000000000, -1.000000000000000000 ) ) ;
#54404 = EDGE_LOOP ( 'NONE', ( #42878, #11893, #1864, #37728, #7170, #15271, #60317, #40291 ) ) ;
#54403 = CARTESIAN_POINT ( 'NONE',  ( 4.456444791733522252E-16, 7.450000000000002842, -11.00000000000000000 ) ) ;
#54405 = LINE ( 'NONE', #27185, #18901 ) ;
#54406 = ADVANCED_FACE ( 'NONE', ( #55514 ), #12010, .F. ) ;
#54407 = FACE_OUTER_BOUND ( 'NONE', #9840, .T. ) ;
#54408 = CARTESIAN_POINT ( 'NONE',  ( 36.90000000000000568, 0.000000000000000000, 0.000000000000000000 ) ) ;
#54409 = EDGE_CURVE ( 'NONE', #23962, #53126, #60115, .T. ) ;
#54410 = LINE ( 'NONE', #11935, #6042 ) ;
#54411 = ORIENTED_EDGE ( 'NONE', *, *, #62344, .T. ) ;
#54412 = PLANE ( 'NONE',  #64817 ) ;
#54413 = CARTESIAN_POINT ( 'NONE',  ( -11.00000000000000000, -8.959999999999999076, 12.95475478405700009 ) ) ;
#54414 = VERTEX_POINT ( 'NONE', #16657 ) ;
#54415 = CARTESIAN_POINT ( 'NONE',  ( 146.5599459900709860, 9.000000000000001776, 284.4801873289890182 ) ) ;
#54416 = CIRCLE ( 'NONE', #63444, 0.5000000000009320322 ) ;
#54417 = CLOSED_SHELL ( 'NONE', ( #31116, #30691, #11070, #32387, #35201, #6721, #39726, #5459, #17820, #55259 ) ) ;
#54418 = CARTESIAN_POINT ( 'NONE',  ( 4.186483450353337687, -11.78648345035347589, 455.0000000000000568 ) ) ;
#54419 = DIRECTION ( 'NONE',  ( 0.000000000000000000, -1.000000000000000000, 0.000000000000000000 ) ) ;
#54420 = EDGE_CURVE ( 'NONE', #40026, #61739, #38228, .T. ) ;
#54421 = DIRECTION ( 'NONE',  ( 0.000000000000000000, 0.000000000000000000, 1.000000000000000000 ) ) ;
#54422 = ADVANCED_FACE ( 'NONE', ( #33591 ), #23331, .F. ) ;
#54423 = PLANE ( 'NONE',  #57839 ) ;
#54424 = ORIENTED_EDGE ( 'NONE', *, *, #51813, .T. ) ;
#54425 = CARTESIAN_POINT ( 'NONE',  ( 7.500000000000000000, -25.50000000000000355, -16.00000000000000000 ) ) ;
#54426 = CYLINDRICAL_SURFACE ( 'NONE', #35594, 24.99999999998789946 ) ;
#54427 = ORIENTED_EDGE ( 'NONE', *, *, #9965, .F. ) ;
#54428 = CARTESIAN_POINT ( 'NONE',  ( 275.0000000000000000, -25.93000000000544958, -9.412893218815410634 ) ) ;
#54429 = AXIS2_PLACEMENT_3D ( 'NONE', #42482, #26930, #32585 ) ;
#54430 = EDGE_CURVE ( 'NONE', #69312, #56335, #61137, .T. ) ;
#54431 = LINE ( 'NONE', #41486, #23104 ) ;
#54432 = CARTESIAN_POINT ( 'NONE',  ( -8.393516549646722780, -5.668387132715892562, 195.0000000000000284 ) ) ;
#54433 = ORIENTED_EDGE ( 'NONE', *, *, #19391, .F. ) ;
#54434 = ORIENTED_EDGE ( 'NONE', *, *, #61304, .F. ) ;
#54435 = DIRECTION ( 'NONE',  ( -1.000000000000000000, 0.000000000000000000, 0.000000000000000000 ) ) ;
#54436 = VERTEX_POINT ( 'NONE', #27598 ) ;
#54437 = ORIENTED_EDGE ( 'NONE', *, *, #60023, .F. ) ;
#54438 = CARTESIAN_POINT ( 'NONE',  ( 9.955011587777235604, -2.765062094116086833, 195.0000000000000284 ) ) ;
#54439 = CARTESIAN_POINT ( 'NONE',  ( 7.000000000000000000, -26.79000000000000625, 0.000000000000000000 ) ) ;
#54440 = CYLINDRICAL_SURFACE ( 'NONE', #33219, 3.500000000000000000 ) ;
#54441 = AXIS2_PLACEMENT_3D ( 'NONE', #25240, #4723, #15330 ) ;
#54442 = VERTEX_POINT ( 'NONE', #49173 ) ;
#54443 = LINE ( 'NONE', #65054, #41383 ) ;
#54445 = CARTESIAN_POINT ( 'NONE',  ( 11.08848345035334404, -9.804883450353433005, 195.0000000000000284 ) ) ;
#54444 = DIRECTION ( 'NONE',  ( -1.000000000000000000, 0.000000000000000000, 0.000000000000000000 ) ) ;
#54446 = ORIENTED_EDGE ( 'NONE', *, *, #67187, .T. ) ;
#54447 = VERTEX_POINT ( 'NONE', #43859 ) ;
#54449 = ORIENTED_EDGE ( 'NONE', *, *, #27329, .T. ) ;
#54448 = CARTESIAN_POINT ( 'NONE',  ( 11.50000000000000000, -11.70000000000012008, -11.00000000000000000 ) ) ;
#54450 = AXIS2_PLACEMENT_3D ( 'NONE', #60041, #16919, #44121 ) ;
#54451 = ORIENTED_EDGE ( 'NONE', *, *, #50409, .T. ) ;
#54452 = ADVANCED_FACE ( 'NONE', ( #11667 ), #19067, .F. ) ;
#54453 = DIRECTION ( 'NONE',  ( -1.000000000000000000, 0.000000000000000000, 0.000000000000000000 ) ) ;
#54454 = AXIS2_PLACEMENT_3D ( 'NONE', #643, #22215, #48036 ) ;
#54455 = EDGE_CURVE ( 'NONE', #41475, #26457, #24891, .T. ) ;
#54456 = DIRECTION ( 'NONE',  ( 0.000000000000000000, 0.000000000000000000, 1.000000000000000000 ) ) ;
#54457 = ORIENTED_EDGE ( 'NONE', *, *, #50648, .T. ) ;
#54458 = ORIENTED_EDGE ( 'NONE', *, *, #21771, .T. ) ;
#54459 = EDGE_CURVE ( 'NONE', #47029, #50321, #40634, .T. ) ;
#54460 = AXIS2_PLACEMENT_3D ( 'NONE', #29720, #1810, #62246 ) ;
#54461 = CARTESIAN_POINT ( 'NONE',  ( 7.272650909786598561, -4.201500623656122535, 455.0000000000000568 ) ) ;
#54462 = ADVANCED_FACE ( 'NONE', ( #34969 ), #45941, .T. ) ;
#54463 = CARTESIAN_POINT ( 'NONE',  ( 283.0000000000000568, -53.81370849898476649, 17.35424868893542438 ) ) ;
#54464 = CIRCLE ( 'NONE', #249, 4.000000000000000000 ) ;
#54465 = ORIENTED_EDGE ( 'NONE', *, *, #6353, .F. ) ;
#54466 = DIRECTION ( 'NONE',  ( 0.000000000000000000, 0.000000000000000000, -1.000000000000000000 ) ) ;
#54467 = DIRECTION ( 'NONE',  ( 0.000000000000000000, 1.000000000000000000, 0.000000000000000000 ) ) ;
#54468 = EDGE_CURVE ( 'NONE', #31078, #58674, #40284, .T. ) ;
#54469 = DIRECTION ( 'NONE',  ( -0.000000000000000000, 3.673940397442059868E-16, -1.000000000000000000 ) ) ;
#54470 = ORIENTED_EDGE ( 'NONE', *, *, #34967, .F. ) ;
#54471 = CIRCLE ( 'NONE', #36385, 0.5000000000004236611 ) ;
#54472 = CIRCLE ( 'NONE', #47701, 1.929199999999997139 ) ;
#54473 = CARTESIAN_POINT ( 'NONE',  ( 280.0000000000000000, -25.60000000000000142, -20.00000000000000000 ) ) ;
#54474 = LINE ( 'NONE', #21936, #23800 ) ;
#54475 = EDGE_CURVE ( 'NONE', #23831, #52876, #57249, .T. ) ;
#54477 = ORIENTED_EDGE ( 'NONE', *, *, #32612, .T. ) ;
#54476 = DIRECTION ( 'NONE',  ( 1.000000000000000000, 0.000000000000000000, 0.000000000000000000 ) ) ;
#54479 = ORIENTED_EDGE ( 'NONE', *, *, #57962, .F. ) ;
#54478 = CARTESIAN_POINT ( 'NONE',  ( 47.00000000000000000, 0.000000000000000000, 0.000000000000000000 ) ) ;
#54480 = EDGE_CURVE ( 'NONE', #7568, #29126, #62196, .T. ) ;
#54482 = CARTESIAN_POINT ( 'NONE',  ( -11.19000000000000128, -12.00000000000000000, -5.000000000000000000 ) ) ;
#54481 = AXIS2_PLACEMENT_3D ( 'NONE', #53372, #26148, #63628 ) ;
#54483 = DIRECTION ( 'NONE',  ( 1.836970198721029934E-16, -1.836970198721036344E-16, 1.000000000000000000 ) ) ;
#54484 = CARTESIAN_POINT ( 'NONE',  ( 176.4833316329832940, 0.000000000000000000, 324.6739988703752715 ) ) ;
#54485 = DIRECTION ( 'NONE',  ( 0.000000000000000000, 0.000000000000000000, 1.000000000000000000 ) ) ;
#54486 = ADVANCED_FACE ( 'NONE', ( #68208 ), #29666, .F. ) ;
#54487 = ADVANCED_FACE ( 'NONE', ( #18350 ), #51953, .F. ) ;
#54488 = LINE ( 'NONE', #16993, #56523 ) ;
#54489 = LINE ( 'NONE', #21947, #39412 ) ;
#54490 = ORIENTED_EDGE ( 'NONE', *, *, #1712, .F. ) ;
#54491 = CARTESIAN_POINT ( 'NONE',  ( 289.5000000000000000, -42.00000000000000000, -27.00000000000000000 ) ) ;
#54492 = EDGE_CURVE ( 'NONE', #69773, #12080, #39554, .T. ) ;
#54494 = ORIENTED_EDGE ( 'NONE', *, *, #5143, .F. ) ;
#54493 = LINE ( 'NONE', #6046, #14191 ) ;
#54496 = VERTEX_POINT ( 'NONE', #62539 ) ;
#54495 = CARTESIAN_POINT ( 'NONE',  ( 8.250000000000005329, -8.249999999999998224, -26.00000000000001066 ) ) ;
#54497 = CARTESIAN_POINT ( 'NONE',  ( -8.250000000000001776, -7.249999999999998224, -8.500000000000000000 ) ) ;
#54498 = CARTESIAN_POINT ( 'NONE',  ( 14.25000000000000178, -0.2714405302574905421, -22.01253933645463690 ) ) ;
#54499 = VERTEX_POINT ( 'NONE', #67860 ) ;
#54500 = CARTESIAN_POINT ( 'NONE',  ( 10.20488345035345290, 9.791916549646566992, 455.0000000000000568 ) ) ;
#54501 = CARTESIAN_POINT ( 'NONE',  ( 11.12648345035337627, -9.106483450353492159, 455.0000000000000568 ) ) ;
#54502 = AXIS2_PLACEMENT_3D ( 'NONE', #15792, #36661, #31381 ) ;
#54503 = VERTEX_POINT ( 'NONE', #45227 ) ;
#54504 = CYLINDRICAL_SURFACE ( 'NONE', #31205, 0.2000000000000005107 ) ;
#54505 = CARTESIAN_POINT ( 'NONE',  ( 7.250000000000004441, 7.450000000000001954, -24.50000000000000000 ) ) ;
#54506 = LINE ( 'NONE', #38583, #40450 ) ;
#54507 = VECTOR ( 'NONE', #13673, 1000.000000000000000 ) ;
#54508 = EDGE_CURVE ( 'NONE', #60224, #24588, #8444, .T. ) ;
#54509 = LINE ( 'NONE', #6062, #19170 ) ;
#54510 = EDGE_CURVE ( 'NONE', #31847, #32441, #14108, .T. ) ;
#54511 = ORIENTED_EDGE ( 'NONE', *, *, #9387, .T. ) ;
#54512 = CARTESIAN_POINT ( 'NONE',  ( 30.00000000000000000, -11.50000000000000000, 15.00000000000000000 ) ) ;
#54513 = EDGE_LOOP ( 'NONE', ( #13278, #43532, #17208, #44561 ) ) ;
#54514 = VERTEX_POINT ( 'NONE', #51603 ) ;
#54515 = DIRECTION ( 'NONE',  ( 0.000000000000000000, 0.000000000000000000, 1.000000000000000000 ) ) ;
#54516 = DIRECTION ( 'NONE',  ( 1.000000000000000000, 0.000000000000000000, 0.000000000000000000 ) ) ;
#54517 = CARTESIAN_POINT ( 'NONE',  ( 29.89999999999999858, 13.66939075806899240, -20.79999999999999361 ) ) ;
#54518 = CARTESIAN_POINT ( 'NONE',  ( -4.031976262117261456, 3.142976262117183506, 54.00000000000000711 ) ) ;
#54519 = ORIENTED_EDGE ( 'NONE', *, *, #16069, .F. ) ;
#54520 = VERTEX_POINT ( 'NONE', #8813 ) ;
#54522 = VERTEX_POINT ( 'NONE', #3165 ) ;
#54521 = DIRECTION ( 'NONE',  ( 0.000000000000000000, -0.7071067811865474617, -0.7071067811865474617 ) ) ;
#54523 = ORIENTED_EDGE ( 'NONE', *, *, #1313, .F. ) ;
#54524 = DIRECTION ( 'NONE',  ( -0.000000000000000000, -0.000000000000000000, -1.000000000000000000 ) ) ;
#54525 = VECTOR ( 'NONE', #1532, 1000.000000000000000 ) ;
#54526 = DIRECTION ( 'NONE',  ( -0.000000000000000000, 3.673940397442059868E-16, -1.000000000000000000 ) ) ;
#54527 = CARTESIAN_POINT ( 'NONE',  ( -7.250000000000000888, -8.249999999999998224, -14.00000000000000000 ) ) ;
#54528 = AXIS2_PLACEMENT_3D ( 'NONE', #52943, #69185, #5188 ) ;
#54529 =( LENGTH_UNIT ( ) NAMED_UNIT ( * ) SI_UNIT ( .MILLI., .METRE. ) );
#54531 = DIRECTION ( 'NONE',  ( 0.000000000000000000, 0.000000000000000000, 1.000000000000000000 ) ) ;
#54530 = DIRECTION ( 'NONE',  ( -1.836970198721029934E-16, 1.836970198721036344E-16, -1.000000000000000000 ) ) ;
#54532 = VECTOR ( 'NONE', #3263, 1000.000000000000000 ) ;
#54533 = ORIENTED_EDGE ( 'NONE', *, *, #60009, .T. ) ;
#54535 = ORIENTED_EDGE ( 'NONE', *, *, #18194, .T. ) ;
#54534 = CARTESIAN_POINT ( 'NONE',  ( -30.00000000000000000, -11.50000000000000000, 11.00000000000000000 ) ) ;
#54536 = ORIENTED_EDGE ( 'NONE', *, *, #15903, .T. ) ;
#54537 = ORIENTED_EDGE ( 'NONE', *, *, #15712, .T. ) ;
#54538 = CARTESIAN_POINT ( 'NONE',  ( 7.250000000000005329, 7.250000000000000888, -10.50000000000000000 ) ) ;
#54539 = AXIS2_PLACEMENT_3D ( 'NONE', #3513, #25427, #40977 ) ;
#54540 = DIRECTION ( 'NONE',  ( 0.7671651518153006499, 0.6414496315691565753, 0.000000000000000000 ) ) ;
#54541 = EDGE_CURVE ( 'NONE', #40746, #13295, #24726, .T. ) ;
#54542 = CARTESIAN_POINT ( 'NONE',  ( 7.450000000000004619, -1.336933437520057563E-15, -13.50000000000000178 ) ) ;
#54543 = AXIS2_PLACEMENT_3D ( 'NONE', #31166, #9947, #53424 ) ;
#54544 = EDGE_LOOP ( 'NONE', ( #39758, #31438, #57300, #50516 ) ) ;
#54545 = ORIENTED_EDGE ( 'NONE', *, *, #38285, .T. ) ;
#54546 = ADVANCED_FACE ( 'NONE', ( #46634 ), #30380, .F. ) ;
#54547 = CARTESIAN_POINT ( 'NONE',  ( 23.90000000000000213, -21.00000000000000000, 13.86939075806900057 ) ) ;
#54548 = CARTESIAN_POINT ( 'NONE',  ( -11.99351654964679526, -7.826483450353362237, 455.0000000000000568 ) ) ;
#54549 = EDGE_CURVE ( 'NONE', #49129, #50581, #30732, .T. ) ;
#54550 = DIRECTION ( 'NONE',  ( -3.717264591378874374E-15, -1.000000000000000000, 0.000000000000000000 ) ) ;
#54551 = VECTOR ( 'NONE', #20580, 1000.000000000000000 ) ;
#54552 = EDGE_CURVE ( 'NONE', #52657, #34054, #40786, .T. ) ;
#54553 = ORIENTED_EDGE ( 'NONE', *, *, #40958, .F. ) ;
#54554 = EDGE_LOOP ( 'NONE', ( #46526, #10142, #58454, #25916 ) ) ;
#54555 = CARTESIAN_POINT ( 'NONE',  ( -7.250000000000000888, 7.250000000000001776, -14.00000000000000000 ) ) ;
#54556 = EDGE_CURVE ( 'NONE', #20722, #21068, #56204, .T. ) ;
#54557 = ADVANCED_FACE ( 'NONE', ( #20124 ), #16209, .T. ) ;
#54558 = VECTOR ( 'NONE', #1140, 1000.000000000000000 ) ;
#54559 = DIRECTION ( 'NONE',  ( -1.000000000000000000, 0.000000000000000000, 0.000000000000000000 ) ) ;
#54560 = VERTEX_POINT ( 'NONE', #57945 ) ;
#54561 = DIRECTION ( 'NONE',  ( 9.912705577010319041E-15, 1.000000000000000000, 0.000000000000000000 ) ) ;
#54562 = VECTOR ( 'NONE', #12660, 1000.000000000000000 ) ;
#54564 = ORIENTED_EDGE ( 'NONE', *, *, #37164, .F. ) ;
#54563 = FACE_OUTER_BOUND ( 'NONE', #36874, .T. ) ;
#54565 = ORIENTED_EDGE ( 'NONE', *, *, #24968, .T. ) ;
#54566 = DIRECTION ( 'NONE',  ( -1.836970198721029934E-16, 1.836970198721036590E-16, -1.000000000000000000 ) ) ;
#54567 = PLANE ( 'NONE',  #18755 ) ;
#54568 = CARTESIAN_POINT ( 'NONE',  ( -5.993516549646711766, 5.993516549646603409, 455.0000000000000568 ) ) ;
#54569 = CARTESIAN_POINT ( 'NONE',  ( 11.34648345035330053, 1.077516549646569066, 195.0000000000000284 ) ) ;
#54570 = DIRECTION ( 'NONE',  ( -0.000000000000000000, -0.000000000000000000, -1.000000000000000000 ) ) ;
#54571 = ORIENTED_EDGE ( 'NONE', *, *, #63078, .F. ) ;
#54572 = DIRECTION ( 'NONE',  ( 0.000000000000000000, -0.7046037717859445770, 0.7096009616573392131 ) ) ;
#54574 = ORIENTED_EDGE ( 'NONE', *, *, #46102, .F. ) ;
#54573 = CARTESIAN_POINT ( 'NONE',  ( 8.250000000000005329, 7.250000000000000888, -16.50000000000000000 ) ) ;
#54575 = DIRECTION ( 'NONE',  ( -4.956352788505168198E-15, -1.000000000000000000, 0.000000000000000000 ) ) ;
#54576 = VECTOR ( 'NONE', #65143, 1000.000000000000000 ) ;
#54577 = CARTESIAN_POINT ( 'NONE',  ( 283.0000000000000568, -23.70411739045900390, -12.50000000000000000 ) ) ;
#54578 = CARTESIAN_POINT ( 'NONE',  ( -4.173516549646837603, -11.78648345035344214, 455.0000000000000568 ) ) ;
#54580 = CARTESIAN_POINT ( 'NONE',  ( 9.417013320880721849, 1.853252480934663771, 195.0000000000000284 ) ) ;
#54579 = AXIS2_PLACEMENT_3D ( 'NONE', #47878, #63806, #63102 ) ;
#54581 = CIRCLE ( 'NONE', #63614, 0.7112000000000124889 ) ;
#54582 = CARTESIAN_POINT ( 'NONE',  ( 13.00000000000000178, -16.64230188589299786, 14.64519951917100116 ) ) ;
#54583 = ORIENTED_EDGE ( 'NONE', *, *, #21532, .F. ) ;
#54584 = VERTEX_POINT ( 'NONE', #31450 ) ;
#54585 = STYLED_ITEM ( 'NONE', ( #14466 ), #42921 ) ;
#54586 = CARTESIAN_POINT ( 'NONE',  ( -7.517976262117260333, 3.834182069070703580, 54.00000000000000711 ) ) ;
#54587 = CIRCLE ( 'NONE', #24075, 0.9999999999999991118 ) ;
#54588 = CARTESIAN_POINT ( 'NONE',  ( 4.961189459950046121, 7.342976262117201003, 54.00000000000000711 ) ) ;
#54589 = EDGE_CURVE ( 'NONE', #51166, #49441, #32870, .T. ) ;
#54590 = EDGE_LOOP ( 'NONE', ( #43244, #66769 ) ) ;
#54591 = CARTESIAN_POINT ( 'NONE',  ( 8.711985858128644011, 2.406732575409517239, 54.00000000000000711 ) ) ;
#54592 = DIRECTION ( 'NONE',  ( 0.000000000000000000, 0.2142857142857145514, 0.9767710236555243730 ) ) ;
#54593 = EDGE_CURVE ( 'NONE', #27508, #53596, #36740, .T. ) ;
#54594 = ORIENTED_EDGE ( 'NONE', *, *, #3862, .F. ) ;
#54595 = DIRECTION ( 'NONE',  ( 1.000000000000000000, 0.000000000000000000, 0.000000000000000000 ) ) ;
#54596 = DIRECTION ( 'NONE',  ( 0.000000000000000000, 0.000000000000000000, -1.000000000000000000 ) ) ;
#54597 = ORIENTED_EDGE ( 'NONE', *, *, #47365, .F. ) ;
#54598 = CARTESIAN_POINT ( 'NONE',  ( 11.12648345035340647, 7.793516549646564151, 455.0000000000000568 ) ) ;
#54599 = AXIS2_PLACEMENT_3D ( 'NONE', #57004, #8565, #53134 ) ;
#54600 = DIRECTION ( 'NONE',  ( 0.000000000000000000, 0.000000000000000000, -1.000000000000000000 ) ) ;
#54601 = ADVANCED_FACE ( 'NONE', ( #48039 ), #64479, .T. ) ;
#54602 = ADVANCED_FACE ( 'NONE', ( #25426 ), #32486, .T. ) ;
#54603 = LINE ( 'NONE', #27719, #65950 ) ;
#54604 = FACE_OUTER_BOUND ( 'NONE', #50338, .T. ) ;
#54605 = AXIS2_PLACEMENT_3D ( 'NONE', #2381, #62457, #34546 ) ;
#54606 = ORIENTED_EDGE ( 'NONE', *, *, #23266, .T. ) ;
#54608 = ORIENTED_EDGE ( 'NONE', *, *, #65195, .T. ) ;
#54607 = DIRECTION ( 'NONE',  ( 0.000000000000000000, 1.000000000000000000, 0.000000000000000000 ) ) ;
#54609 = DIRECTION ( 'NONE',  ( 0.000000000000000000, 1.000000000000000000, 0.000000000000000000 ) ) ;
#54610 = CARTESIAN_POINT ( 'NONE',  ( 14.25000000000000000, -0.2038245569916330158, -21.77831216351300014 ) ) ;
#54611 = LINE ( 'NONE', #31657, #22858 ) ;
#54612 = EDGE_LOOP ( 'NONE', ( #66766, #69831, #45630, #39703 ) ) ;
#54613 = VECTOR ( 'NONE', #34113, 1000.000000000000000 ) ;
#54614 = CARTESIAN_POINT ( 'NONE',  ( 29.50000000000000355, -11.50000000000100009, 10.50000000000065903 ) ) ;
#54615 = CARTESIAN_POINT ( 'NONE',  ( 6.836383711243005479, -6.364920264886905876, 54.00000000000000711 ) ) ;
#54616 = ORIENTED_EDGE ( 'NONE', *, *, #56804, .F. ) ;
#54617 = EDGE_LOOP ( 'NONE', ( #56096, #67504, #27785, #39212 ) ) ;
#54618 = VERTEX_POINT ( 'NONE', #48391 ) ;
#54619 = DIRECTION ( 'NONE',  ( -1.000000000000000000, 0.000000000000000000, 0.000000000000000000 ) ) ;
#54620 = DIRECTION ( 'NONE',  ( 0.000000000000000000, -0.000000000000000000, 1.000000000000000000 ) ) ;
#54621 = DIRECTION ( 'NONE',  ( 0.000000000000000000, 0.000000000000000000, 1.000000000000000000 ) ) ;
#54622 = EDGE_CURVE ( 'NONE', #35173, #40737, #27229, .T. ) ;
#54623 = VECTOR ( 'NONE', #5379, 1000.000000000000114 ) ;
#54624 = AXIS2_PLACEMENT_3D ( 'NONE', #35185, #8322, #29893 ) ;
#54625 = VERTEX_POINT ( 'NONE', #42732 ) ;
#54626 = ORIENTED_EDGE ( 'NONE', *, *, #8941, .F. ) ;
#54627 = VERTEX_POINT ( 'NONE', #47692 ) ;
#54628 = CIRCLE ( 'NONE', #2511, 0.1999999999999987899 ) ;
#54629 = DIRECTION ( 'NONE',  ( 0.000000000000000000, 0.000000000000000000, 1.000000000000000000 ) ) ;
#54630 = ORIENTED_EDGE ( 'NONE', *, *, #45198, .T. ) ;
#54631 = AXIS2_PLACEMENT_3D ( 'NONE', #9666, #31240, #52818 ) ;
#54632 = ORIENTED_EDGE ( 'NONE', *, *, #44149, .F. ) ;
#54633 = ORIENTED_EDGE ( 'NONE', *, *, #47934, .F. ) ;
#54634 = ORIENTED_EDGE ( 'NONE', *, *, #42056, .F. ) ;
#54635 = CYLINDRICAL_SURFACE ( 'NONE', #12388, 6.000000000000005329 ) ;
#54636 = CIRCLE ( 'NONE', #48983, 4.000000000000000888 ) ;
#54637 = VECTOR ( 'NONE', #17053, 1000.000000000000000 ) ;
#54638 = ADVANCED_FACE ( 'NONE', ( #9515 ), #47340, .F. ) ;
#54639 = EDGE_CURVE ( 'NONE', #28757, #55545, #15917, .T. ) ;
#54641 = ORIENTED_EDGE ( 'NONE', *, *, #22810, .T. ) ;
#54640 = DIRECTION ( 'NONE',  ( -1.000000000000000000, -0.000000000000000000, -0.000000000000000000 ) ) ;
#54642 = DIRECTION ( 'NONE',  ( -1.000000000000000000, 0.000000000000000000, 0.000000000000000000 ) ) ;
#54643 = CARTESIAN_POINT ( 'NONE',  ( 55.00000000000000000, -21.00000000000000000, 16.96999999999999886 ) ) ;
#54644 = EDGE_CURVE ( 'NONE', #7139, #21874, #22719, .T. ) ;
#54645 = DIRECTION ( 'NONE',  ( 3.491481338843133355E-15, 1.000000000000000000, 1.836970198721029934E-16 ) ) ;
#54646 = EDGE_LOOP ( 'NONE', ( #34034, #15037, #32768, #45885 ) ) ;
#54647 = DIRECTION ( 'NONE',  ( -1.000000000000000000, 0.000000000000000000, 0.000000000000000000 ) ) ;
#54648 = ORIENTED_EDGE ( 'NONE', *, *, #14551, .T. ) ;
#54649 = DIRECTION ( 'NONE',  ( -0.000000000000000000, -0.000000000000000000, -1.000000000000000000 ) ) ;
#54650 = CARTESIAN_POINT ( 'NONE',  ( 9.737023737882816832, -6.832023737882823688, 54.00000000000000711 ) ) ;
#54651 = CARTESIAN_POINT ( 'NONE',  ( 8.580623737882845603, 8.916576262117189344, 54.00000000000000711 ) ) ;
#54652 = FACE_OUTER_BOUND ( 'NONE', #37050, .T. ) ;
#54653 = ORIENTED_EDGE ( 'NONE', *, *, #34019, .F. ) ;
#54654 = CARTESIAN_POINT ( 'NONE',  ( 30.00000000000000000, -11.70000000000000284, 12.50000000000000000 ) ) ;
#54655 = DIRECTION ( 'NONE',  ( 0.000000000000000000, 0.000000000000000000, -1.000000000000000000 ) ) ;
#54656 = CARTESIAN_POINT ( 'NONE',  ( -9.249999999999998224, 8.250000000000001776, 0.000000000000000000 ) ) ;
#54657 = PLANE ( 'NONE',  #64775 ) ;
#54658 = CARTESIAN_POINT ( 'NONE',  ( -8.000000000000000000, 8.000000000000000000, 0.000000000000000000 ) ) ;
#54659 = CARTESIAN_POINT ( 'NONE',  ( 39.00000000000000000, 21.00000000000000000, -13.98999642601811999 ) ) ;
#54660 = CARTESIAN_POINT ( 'NONE',  ( 9.900000000000000355, 18.00000000000000355, 21.00000000000000000 ) ) ;
#54661 = CARTESIAN_POINT ( 'NONE',  ( 3.682023737882786918, -9.737023737882809726, 54.00000000000000711 ) ) ;
#54662 = CIRCLE ( 'NONE', #24165, 0.5999999999999998668 ) ;
#54663 = AXIS2_PLACEMENT_3D ( 'NONE', #17822, #13552, #18493 ) ;
#54664 = VERTEX_POINT ( 'NONE', #15535 ) ;
#54665 = CARTESIAN_POINT ( 'NONE',  ( 2.544523737882787184, -9.562023737882800134, 54.00000000000000711 ) ) ;
#54666 = DIRECTION ( 'NONE',  ( 1.000000000000000000, 0.000000000000000000, 0.000000000000000000 ) ) ;
#54667 = ADVANCED_FACE ( 'NONE', ( #68914 ), #52666, .T. ) ;
#54668 = EDGE_CURVE ( 'NONE', #21320, #62492, #26135, .T. ) ;
#54669 = EDGE_CURVE ( 'NONE', #13935, #1121, #67840, .T. ) ;
#54670 = DIRECTION ( 'NONE',  ( -0.000000000000000000, -0.000000000000000000, -1.000000000000000000 ) ) ;
#54671 = DIRECTION ( 'NONE',  ( -1.053224967557347660E-14, -1.000000000000000000, 0.000000000000000000 ) ) ;
#54672 = AXIS2_PLACEMENT_3D ( 'NONE', #41094, #62312, #35434 ) ;
#54673 = ORIENTED_EDGE ( 'NONE', *, *, #34412, .T. ) ;
#54674 = VECTOR ( 'NONE', #54301, 1000.000000000000000 ) ;
#54675 = CARTESIAN_POINT ( 'NONE',  ( 10.09643294401454661, -2.906483450353491094, 455.0000000000000568 ) ) ;
#54676 = CARTESIAN_POINT ( 'NONE',  ( 6.836383711243005479, -4.149127210878744698, 54.00000000000000711 ) ) ;
#54677 = DIRECTION ( 'NONE',  ( -1.836970198721029934E-16, 1.836970198721036344E-16, -1.000000000000000000 ) ) ;
#54678 = EDGE_CURVE ( 'NONE', #29937, #7966, #42380, .T. ) ;
#54679 = VECTOR ( 'NONE', #14512, 1000.000000000000000 ) ;
#54680 = CARTESIAN_POINT ( 'NONE',  ( 0.5000000000000000000, -18.00000000000000355, 21.00000000000000000 ) ) ;
#54681 = DIRECTION ( 'NONE',  ( 0.000000000000000000, 0.000000000000000000, 1.000000000000000000 ) ) ;
#54682 = EDGE_LOOP ( 'NONE', ( #15189, #30868, #15183, #60295, #58698, #68279, #46670, #1296 ) ) ;
#54683 = VECTOR ( 'NONE', #46189, 1000.000000000000000 ) ;
#54684 = ORIENTED_EDGE ( 'NONE', *, *, #46966, .F. ) ;
#54685 = DIRECTION ( 'NONE',  ( 0.000000000000000000, 0.000000000000000000, -1.000000000000000000 ) ) ;
#54686 = DIRECTION ( 'NONE',  ( -1.000000000000000000, 0.000000000000000000, -0.000000000000000000 ) ) ;
#54687 = VERTEX_POINT ( 'NONE', #25789 ) ;
#54688 = VECTOR ( 'NONE', #29455, 1000.000000000000000 ) ;
#54689 = LINE ( 'NONE', #49718, #36379 ) ;
#54690 = ORIENTED_EDGE ( 'NONE', *, *, #16461, .F. ) ;
#54691 = DIRECTION ( 'NONE',  ( 0.000000000000000000, 0.000000000000000000, 1.000000000000000000 ) ) ;
#54692 = ORIENTED_EDGE ( 'NONE', *, *, #29497, .F. ) ;
#54693 = ORIENTED_EDGE ( 'NONE', *, *, #48686, .F. ) ;
#54694 = PLANE ( 'NONE',  #54364 ) ;
#54695 = VERTEX_POINT ( 'NONE', #58998 ) ;
#54696 = DIRECTION ( 'NONE',  ( 0.000000000000000000, 1.000000000000000000, 0.000000000000000000 ) ) ;
#54697 = DIRECTION ( 'NONE',  ( -0.000000000000000000, -0.000000000000000000, -1.000000000000000000 ) ) ;
#54698 = DIRECTION ( 'NONE',  ( 0.000000000000000000, -0.7046037717806115097, -0.7096009616626348659 ) ) ;
#54699 = ORIENTED_EDGE ( 'NONE', *, *, #64485, .T. ) ;
#54700 = VERTEX_POINT ( 'NONE', #10555 ) ;
#54701 = LINE ( 'NONE', #27829, #21101 ) ;
#54702 = CARTESIAN_POINT ( 'NONE',  ( 11.19368345035340440, 11.18071654964654904, 455.0000000000000568 ) ) ;
#54703 = VERTEX_POINT ( 'NONE', #32128 ) ;
#54704 = VECTOR ( 'NONE', #29686, 1000.000000000000000 ) ;
#54705 = ORIENTED_EDGE ( 'NONE', *, *, #45179, .F. ) ;
#54707 = ORIENTED_EDGE ( 'NONE', *, *, #26871, .F. ) ;
#54706 = ITEM_DEFINED_TRANSFORMATION ( 'NONE', 'NONE', #24525,  #45918 ) ;
#54708 = DIRECTION ( 'NONE',  ( 0.000000000000000000, 1.000000000000000000, 0.000000000000000000 ) ) ;
#54710 = ORIENTED_EDGE ( 'NONE', *, *, #58978, .F. ) ;
#54709 = FACE_OUTER_BOUND ( 'NONE', #50961, .T. ) ;
#54711 = EDGE_CURVE ( 'NONE', #41932, #32778, #37367, .T. ) ;
#54712 = LINE ( 'NONE', #48714, #2870 ) ;
#54713 = VECTOR ( 'NONE', #37033, 1000.000000000000114 ) ;
#54714 = AXIS2_PLACEMENT_3D ( 'NONE', #33650, #45282, #23730 ) ;
#54715 = DIRECTION ( 'NONE',  ( -0.000000000000000000, 1.000000000000000000, -0.000000000000000000 ) ) ;
#54716 = EDGE_CURVE ( 'NONE', #29241, #5502, #44795, .T. ) ;
#54717 = ORIENTED_EDGE ( 'NONE', *, *, #9385, .F. ) ;
#54718 = EDGE_CURVE ( 'NONE', #29457, #60260, #1266, .T. ) ;
#54719 = ORIENTED_EDGE ( 'NONE', *, *, #21271, .F. ) ;
#54720 = VECTOR ( 'NONE', #31561, 1000.000000000000000 ) ;
#54721 = VECTOR ( 'NONE', #50639, 1000.000000000000000 ) ;
#54722 = EDGE_CURVE ( 'NONE', #63841, #8038, #50919, .T. ) ;
#54723 = ORIENTED_EDGE ( 'NONE', *, *, #58050, .F. ) ;
#54724 = DIRECTION ( 'NONE',  ( 0.000000000000000000, 0.000000000000000000, -1.000000000000000000 ) ) ;
#54725 = CARTESIAN_POINT ( 'NONE',  ( -11.11351654964669500, -4.206483450353289300, 195.0000000000000284 ) ) ;
#54726 = EDGE_CURVE ( 'NONE', #65820, #19320, #24938, .T. ) ;
#54727 = ORIENTED_EDGE ( 'NONE', *, *, #46551, .F. ) ;
#54728 = ADVANCED_FACE ( 'NONE', ( #39492 ), #12611, .F. ) ;
#54729 = DIRECTION ( 'NONE',  ( 0.000000000000000000, 0.000000000000000000, -1.000000000000000000 ) ) ;
#54730 = FACE_OUTER_BOUND ( 'NONE', #39272, .T. ) ;
#54732 = VERTEX_POINT ( 'NONE', #27864 ) ;
#54731 = SURFACE_STYLE_USAGE ( .BOTH. , #55758 ) ;
#54733 = ORIENTED_EDGE ( 'NONE', *, *, #24536, .F. ) ;
#54734 = AXIS2_PLACEMENT_3D ( 'NONE', #10266, #53752, #54444 ) ;
#54735 = CARTESIAN_POINT ( 'NONE',  ( 106.4257688009193430, 0.000000000000000000, 327.4830310981789694 ) ) ;
#54736 = CARTESIAN_POINT ( 'NONE',  ( 4.201500623656052369, 4.727349090213339267, 455.0000000000000568 ) ) ;
#54737 = DIRECTION ( 'NONE',  ( 0.000000000000000000, -1.000000000000000000, 0.000000000000000000 ) ) ;
#54738 = FACE_OUTER_BOUND ( 'NONE', #15624, .T. ) ;
#54739 = LINE ( 'NONE', #60365, #65824 ) ;
#54740 = ORIENTED_EDGE ( 'NONE', *, *, #39139, .F. ) ;
#54741 = CARTESIAN_POINT ( 'NONE',  ( 10.50702373788277910, 3.650476262117147375, 26.00000000000000711 ) ) ;
#54742 = CARTESIAN_POINT ( 'NONE',  ( 3.006483450353369502, -7.428221114745093168, 455.0000000000000568 ) ) ;
#54743 = DIRECTION ( 'NONE',  ( 1.000000000000000000, -8.540177112501197482E-15, 0.000000000000000000 ) ) ;
#54744 = DIRECTION ( 'NONE',  ( 0.000000000000000000, -3.673940397442059868E-16, 1.000000000000000000 ) ) ;
#54745 = DIRECTION ( 'NONE',  ( 0.000000000000000000, 1.000000000000000000, 0.000000000000000000 ) ) ;
#54746 = DIRECTION ( 'NONE',  ( 1.836970198721029934E-16, 1.836970198721010706E-16, -1.000000000000000000 ) ) ;
#54747 = DIRECTION ( 'NONE',  ( 0.000000000000000000, -0.000000000000000000, 1.000000000000000000 ) ) ;
#54748 = DIRECTION ( 'NONE',  ( 0.000000000000000000, 0.000000000000000000, 1.000000000000000000 ) ) ;
#54749 = ORIENTED_EDGE ( 'NONE', *, *, #46531, .T. ) ;
#54750 = DIRECTION ( 'NONE',  ( 0.000000000000000000, -1.000000000000000000, 0.000000000000000000 ) ) ;
#54751 = LINE ( 'NONE', #28900, #33829 ) ;
#54752 = VECTOR ( 'NONE', #69430, 1000.000000000000000 ) ;
#54753 = ORIENTED_EDGE ( 'NONE', *, *, #35159, .F. ) ;
#54754 = CARTESIAN_POINT ( 'NONE',  ( -7.250000000000000888, 7.450000000000003730, -24.00000000000000000 ) ) ;
#54755 = DIRECTION ( 'NONE',  ( 0.000000000000000000, 0.000000000000000000, 1.000000000000000000 ) ) ;
#54756 = CARTESIAN_POINT ( 'NONE',  ( -9.404046420174113408, -1.866219381641437636, 455.0000000000000568 ) ) ;
#54757 = CYLINDRICAL_SURFACE ( 'NONE', #2568, 0.1999999999999996503 ) ;
#54758 = DIRECTION ( 'NONE',  ( 0.000000000000000000, -1.000000000000000000, -3.673940397442059868E-16 ) ) ;
#54759 = DIRECTION ( 'NONE',  ( 0.000000000000000000, -1.000000000000000000, 0.000000000000000000 ) ) ;
#54760 = AXIS2_PLACEMENT_3D ( 'NONE', #25174, #4325, #57342 ) ;
#54761 = AXIS2_PLACEMENT_3D ( 'NONE', #53764, #26892, #26535 ) ;
#54762 = ORIENTED_EDGE ( 'NONE', *, *, #11581, .F. ) ;
#54763 = CARTESIAN_POINT ( 'NONE',  ( 39.00000000000000000, -21.00000000000000000, -14.57806571531351914 ) ) ;
#54764 = LINE ( 'NONE', #49796, #28828 ) ;
#54765 = ORIENTED_EDGE ( 'NONE', *, *, #21305, .T. ) ;
#54766 = LINE ( 'NONE', #28230, #37053 ) ;
#54767 = AXIS2_PLACEMENT_3D ( 'NONE', #48427, #42768, #43109 ) ;
#54768 = ADVANCED_FACE ( 'NONE', ( #54738 ), #34177, .F. ) ;
#54769 = CYLINDRICAL_SURFACE ( 'NONE', #50209, 24.99999999998784972 ) ;
#54770 = VECTOR ( 'NONE', #30869, 1000.000000000000000 ) ;
#54771 = EDGE_CURVE ( 'NONE', #45033, #17091, #22894, .T. ) ;
#54772 = CARTESIAN_POINT ( 'NONE',  ( -5.993516549646751734, -8.211283450353379365, 195.0000000000000284 ) ) ;
#54773 = ORIENTED_EDGE ( 'NONE', *, *, #51481, .F. ) ;
#54774 = ORIENTED_EDGE ( 'NONE', *, *, #15378, .F. ) ;
#54775 = DIRECTION ( 'NONE',  ( -7.457533623526253657E-15, -1.000000000000000000, -1.836970198721024757E-16 ) ) ;
#54776 = ORIENTED_EDGE ( 'NONE', *, *, #5978, .T. ) ;
#54777 = ORIENTED_EDGE ( 'NONE', *, *, #66110, .T. ) ;
#54778 = CARTESIAN_POINT ( 'NONE',  ( 8.689999999999999503, 8.750000000000000000, -7.000000000000000000 ) ) ;
#54779 = LINE ( 'NONE', #27910, #23417 ) ;
#54780 = AXIS2_PLACEMENT_3D ( 'NONE', #63879, #12881, #6574 ) ;
#54781 = CARTESIAN_POINT ( 'NONE',  ( 7.000000000000000000, -42.00000000000000000, 7.000000000000000000 ) ) ;
#54782 = EDGE_CURVE ( 'NONE', #11406, #67088, #16586, .T. ) ;
#54783 = ORIENTED_EDGE ( 'NONE', *, *, #17444, .F. ) ;
#54784 = MECHANICAL_DESIGN_GEOMETRIC_PRESENTATION_REPRESENTATION (  '', ( #5126 ), #10765 ) ;
#54785 = CARTESIAN_POINT ( 'NONE',  ( -7.798499376344157241, -7.272650909786626983, 455.0000000000000568 ) ) ;
#54787 = LINE ( 'NONE', #54445, #8407 ) ;
#54786 = CARTESIAN_POINT ( 'NONE',  ( 30.90000000000000213, 20.60000000000000142, -13.86939075806900057 ) ) ;
#54788 = ORIENTED_EDGE ( 'NONE', *, *, #63507, .T. ) ;
#54789 = ORIENTED_EDGE ( 'NONE', *, *, #44863, .T. ) ;
#54791 = ORIENTED_EDGE ( 'NONE', *, *, #34231, .T. ) ;
#54790 = CARTESIAN_POINT ( 'NONE',  ( 275.0000000000000000, -20.40000000000000213, -17.60000000000000142 ) ) ;
#54792 = ORIENTED_EDGE ( 'NONE', *, *, #16730, .F. ) ;
#54793 = EDGE_CURVE ( 'NONE', #38888, #66296, #2368, .T. ) ;
#54794 = LINE ( 'NONE', #44505, #62670 ) ;
#54795 = FACE_OUTER_BOUND ( 'NONE', #25944, .T. ) ;
#54796 = EDGE_CURVE ( 'NONE', #39018, #44299, #54395, .T. ) ;
#54797 = ORIENTED_EDGE ( 'NONE', *, *, #505, .F. ) ;
#54798 = ORIENTED_EDGE ( 'NONE', *, *, #24896, .F. ) ;
#54799 = LINE ( 'NONE', #54461, #39149 ) ;
#54800 = CARTESIAN_POINT ( 'NONE',  ( 11.00000000000000000, -11.50000000000100009, -19.50000000000103739 ) ) ;
#54801 = CIRCLE ( 'NONE', #17486, 0.1999999999999987899 ) ;
#54802 = EDGE_LOOP ( 'NONE', ( #26338, #49498, #67104, #32943 ) ) ;
#54803 = DIRECTION ( 'NONE',  ( -1.000000000000000000, 6.308085367188447236E-15, 0.000000000000000000 ) ) ;
#54804 = CARTESIAN_POINT ( 'NONE',  ( 50.83090410532631864, 63.65740854044500452, 2.000000000000000000 ) ) ;
#54805 = AXIS2_PLACEMENT_3D ( 'NONE', #57267, #25809, #8829 ) ;
#54806 = EDGE_CURVE ( 'NONE', #21069, #20434, #40735, .T. ) ;
#54807 = FACE_BOUND ( 'NONE', #37219, .T. ) ;
#54808 = ORIENTED_EDGE ( 'NONE', *, *, #47533, .T. ) ;
#54809 = EDGE_CURVE ( 'NONE', #56386, #3052, #65350, .T. ) ;
#54810 = AXIS2_PLACEMENT_3D ( 'NONE', #43675, #64208, #198 ) ;
#54811 = VECTOR ( 'NONE', #43785, 1000.000000000000114 ) ;
#54812 = AXIS2_PLACEMENT_3D ( 'NONE', #15500, #58627, #37411 ) ;
#54813 = DIRECTION ( 'NONE',  ( -0.6414496315691494699, -0.7671651518153064231, 0.000000000000000000 ) ) ;
#54814 = LINE ( 'NONE', #16647, #53208 ) ;
#54816 = ORIENTED_EDGE ( 'NONE', *, *, #55165, .F. ) ;
#54815 = CARTESIAN_POINT ( 'NONE',  ( 10.47821035407137558, -20.81978353999702236, 17.31978353999702236 ) ) ;
#54818 = ORIENTED_EDGE ( 'NONE', *, *, #63091, .F. ) ;
#54817 = DIRECTION ( 'NONE',  ( -0.7671651518153106419, -0.6414496315691445849, 0.000000000000000000 ) ) ;
#54819 = DIRECTION ( 'NONE',  ( 0.000000000000000000, 0.7071067811865475727, 0.7071067811865475727 ) ) ;
#54820 = AXIS2_PLACEMENT_3D ( 'NONE', #67116, #2072, #2761 ) ;
#54821 = AXIS2_PLACEMENT_3D ( 'NONE', #27039, #47899, #69474 ) ;
#54822 = LINE ( 'NONE', #50549, #36315 ) ;
#54823 = ADVANCED_FACE ( 'NONE', ( #645 ), #1002, .F. ) ;
#54824 = CARTESIAN_POINT ( 'NONE',  ( -16.74999999999999289, -0.3152037684892597946, -22.25410949791978510 ) ) ;
#54825 = CARTESIAN_POINT ( 'NONE',  ( 16.75000000000000000, -0.2038245569916320166, 21.77831216351300014 ) ) ;
#54826 = DIRECTION ( 'NONE',  ( 0.000000000000000000, 1.000000000000000000, 0.000000000000000000 ) ) ;
#54827 = VECTOR ( 'NONE', #68546, 1000.000000000000000 ) ;
#54828 = DIRECTION ( 'NONE',  ( -1.000000000000000000, 0.000000000000000000, -0.000000000000000000 ) ) ;
#54829 = VERTEX_POINT ( 'NONE', #11921 ) ;
#54830 = PLANE ( 'NONE',  #63177 ) ;
#54832 = VERTEX_POINT ( 'NONE', #48736 ) ;
#54831 = LINE ( 'NONE', #44199, #63869 ) ;
#54834 = ORIENTED_EDGE ( 'NONE', *, *, #68755, .T. ) ;
#54833 = CARTESIAN_POINT ( 'NONE',  ( 7.250000000000005329, 8.250000000000001776, -9.500000000000001776 ) ) ;
#54835 = CIRCLE ( 'NONE', #49181, 0.1749999999999998224 ) ;
#54836 = DIRECTION ( 'NONE',  ( 1.836970198721029934E-16, -1.836970198721036344E-16, 1.000000000000000000 ) ) ;
#54837 = ORIENTED_EDGE ( 'NONE', *, *, #916, .T. ) ;
#54838 = DIRECTION ( 'NONE',  ( 1.000000000000000000, 0.000000000000000000, 0.000000000000000000 ) ) ;
#54839 = DIRECTION ( 'NONE',  ( -0.000000000000000000, -0.000000000000000000, 1.000000000000000000 ) ) ;
#54840 = VERTEX_POINT ( 'NONE', #28202 ) ;
#54841 = EDGE_CURVE ( 'NONE', #4035, #58797, #5777, .T. ) ;
#54842 = CARTESIAN_POINT ( 'NONE',  ( -15.50000000000129852, -17.50000000000000000, -22.50000000000000000 ) ) ;
#54843 = LINE ( 'NONE', #6401, #17981 ) ;
#54844 = PLANE ( 'NONE',  #57360 ) ;
#54845 = LINE ( 'NONE', #2130, #25961 ) ;
#54846 = EDGE_CURVE ( 'NONE', #27049, #22852, #59692, .T. ) ;
#54847 = LINE ( 'NONE', #49538, #13926 ) ;
#54848 = ORIENTED_EDGE ( 'NONE', *, *, #10226, .T. ) ;
#54849 = PLANE ( 'NONE',  #44052 ) ;
#54850 = VERTEX_POINT ( 'NONE', #11239 ) ;
#54851 = AXIS2_PLACEMENT_3D ( 'NONE', #14007, #57150, #8718 ) ;
#54852 = ADVANCED_FACE ( 'NONE', ( #39160 ), #60721, .F. ) ;
#54853 = VERTEX_POINT ( 'NONE', #63088 ) ;
#54854 = CARTESIAN_POINT ( 'NONE',  ( -7.450000000000001954, 0.000000000000000000, -20.00000000000000000 ) ) ;
#54855 = FACE_OUTER_BOUND ( 'NONE', #53171, .T. ) ;
#54856 = EDGE_CURVE ( 'NONE', #27495, #67923, #3340, .T. ) ;
#54857 = VECTOR ( 'NONE', #31393, 1000.000000000000000 ) ;
#54858 = CARTESIAN_POINT ( 'NONE',  ( -4.188533722949370208, -4.740315990920148437, 195.0000000000000284 ) ) ;
#54859 = AXIS2_PLACEMENT_3D ( 'NONE', #69884, #21448, #27102 ) ;
#54860 = ADVANCED_FACE ( 'NONE', ( #8641 ), #35495, .F. ) ;
#54861 = PLANE ( 'NONE',  #65659 ) ;
#54862 = ORIENTED_EDGE ( 'NONE', *, *, #49275, .T. ) ;
#54863 = ORIENTED_EDGE ( 'NONE', *, *, #26, .F. ) ;
#54865 = VERTEX_POINT ( 'NONE', #52128 ) ;
#54864 = DIRECTION ( 'NONE',  ( 0.000000000000000000, -0.1249999999999996531, -0.9921567416492215186 ) ) ;
#54866 = ORIENTED_EDGE ( 'NONE', *, *, #60429, .F. ) ;
#54867 = AXIS2_PLACEMENT_3D ( 'NONE', #22791, #18169, #17835 ) ;
#54868 = VECTOR ( 'NONE', #1262, 1000.000000000000114 ) ;
#54869 = VECTOR ( 'NONE', #29041, 1000.000000000000000 ) ;
#54870 = DIRECTION ( 'NONE',  ( 0.000000000000000000, -1.000000000000000000, -3.673940397442059868E-16 ) ) ;
#54871 = DIRECTION ( 'NONE',  ( -1.000000000000000000, 0.000000000000000000, 0.000000000000000000 ) ) ;
#54872 = FACE_BOUND ( 'NONE', #15253, .T. ) ;
#54873 = ADVANCED_FACE ( 'NONE', ( #4407 ), #46121, .F. ) ;
#54874 = EDGE_CURVE ( 'NONE', #30798, #7476, #35863, .T. ) ;
#54875 = CARTESIAN_POINT ( 'NONE',  ( -2.530476262117233865, 8.821682069070682530, 26.00000000000000711 ) ) ;
#54876 = CIRCLE ( 'NONE', #16464, 0.3499999999998879008 ) ;
#54877 = AXIS2_PLACEMENT_3D ( 'NONE', #22685, #1126, #43555 ) ;
#54879 = LINE ( 'NONE', #1129, #19881 ) ;
#54878 = LINE ( 'NONE', #49559, #25308 ) ;
#54880 = EDGE_LOOP ( 'NONE', ( #34380, #2053, #648, #5726 ) ) ;
#54883 = EDGE_CURVE ( 'NONE', #13109, #17390, #36208, .T. ) ;
#54882 = ORIENTED_EDGE ( 'NONE', *, *, #20690, .T. ) ;
#54881 = DIRECTION ( 'NONE',  ( 1.000000000000000000, 0.000000000000000000, 0.000000000000000000 ) ) ;
#54884 = ORIENTED_EDGE ( 'NONE', *, *, #33756, .F. ) ;
#54885 = VERTEX_POINT ( 'NONE', #47524 ) ;
#54886 = ADVANCED_FACE ( 'NONE', ( #57076 ), #30913, .F. ) ;
#54887 = ADVANCED_FACE ( 'NONE', ( #63794 ), #41519, .T. ) ;
#54888 = AXIS2_PLACEMENT_3D ( 'NONE', #49339, #22107, #23130 ) ;
#54889 = CARTESIAN_POINT ( 'NONE',  ( -28.00000000000000000, -17.00000000000000000, -15.70499999999969809 ) ) ;
#54890 = DIRECTION ( 'NONE',  ( 1.000000000000000000, 0.000000000000000000, 0.000000000000000000 ) ) ;
#54891 = EDGE_CURVE ( 'NONE', #55138, #53577, #56577, .T. ) ;
#54892 = AXIS2_PLACEMENT_3D ( 'NONE', #55445, #33526, #50128 ) ;
#54893 = CARTESIAN_POINT ( 'NONE',  ( -7.250000000000000888, -8.249999999999998224, -13.50000000000000178 ) ) ;
#54894 = DIRECTION ( 'NONE',  ( 0.000000000000000000, 0.000000000000000000, 1.000000000000000000 ) ) ;
#54895 = ORIENTED_EDGE ( 'NONE', *, *, #9650, .F. ) ;
#54896 = ORIENTED_EDGE ( 'NONE', *, *, #2333, .F. ) ;
#54897 = VECTOR ( 'NONE', #66386, 1000.000000000000000 ) ;
#54898 = FACE_OUTER_BOUND ( 'NONE', #32581, .T. ) ;
#54899 = DIRECTION ( 'NONE',  ( 0.000000000000000000, 0.000000000000000000, -1.000000000000000000 ) ) ;
#54900 = EDGE_LOOP ( 'NONE', ( #34383, #6454, #48400, #36536 ) ) ;
#54901 = ORIENTED_EDGE ( 'NONE', *, *, #43811, .F. ) ;
#54902 = LINE ( 'NONE', #22022, #42952 ) ;
#54903 = APPLICATION_CONTEXT ( 'automotive_design' ) ;
#54904 = EDGE_CURVE ( 'NONE', #49129, #44568, #35736, .T. ) ;
#54905 = CARTESIAN_POINT ( 'NONE',  ( 48.83285635894858245, -0.7500000000000019984, -3.758896888126563862 ) ) ;
#54906 = ORIENTED_EDGE ( 'NONE', *, *, #45139, .T. ) ;
#54907 = EDGE_CURVE ( 'NONE', #66121, #53994, #41160, .T. ) ;
#54908 = DIRECTION ( 'NONE',  ( 1.836970198721029934E-16, 1.836970198721010706E-16, -1.000000000000000000 ) ) ;
#54909 = VECTOR ( 'NONE', #4047, 1000.000000000000000 ) ;
#54911 = ORIENTED_EDGE ( 'NONE', *, *, #14388, .T. ) ;
#54910 = LINE ( 'NONE', #28027, #12530 ) ;
#54912 = ORIENTED_EDGE ( 'NONE', *, *, #61110, .T. ) ;
#54913 = DIRECTION ( 'NONE',  ( -1.678252938371784572E-14, -1.000000000000000000, -1.836970198721041520E-16 ) ) ;
#54914 = DIRECTION ( 'NONE',  ( -1.000000000000000000, 0.000000000000000000, 0.000000000000000000 ) ) ;
#54915 = CIRCLE ( 'NONE', #2955, 8.000000000000000000 ) ;
#54916 = FACE_OUTER_BOUND ( 'NONE', #64081, .T. ) ;
#54917 = DIRECTION ( 'NONE',  ( 0.000000000000000000, 0.000000000000000000, 1.000000000000000000 ) ) ;
#54918 = CARTESIAN_POINT ( 'NONE',  ( 7.000000000000000000, -32.95000000000000284, 7.700000000000000178 ) ) ;
#54919 = CIRCLE ( 'NONE', #63949, 0.2000000000000005107 ) ;
#54920 = ORIENTED_EDGE ( 'NONE', *, *, #7672, .F. ) ;
#54921 = DIRECTION ( 'NONE',  ( 1.000000000000000000, 0.000000000000000000, 0.000000000000000000 ) ) ;
#54923 = ORIENTED_EDGE ( 'NONE', *, *, #46290, .T. ) ;
#54922 = CARTESIAN_POINT ( 'NONE',  ( 0.000000000000000000, -7.449999999999998401, -22.00000000000000000 ) ) ;
#54924 = AXIS2_PLACEMENT_3D ( 'NONE', #18373, #34284, #1776 ) ;
#54925 = VECTOR ( 'NONE', #47443, 1000.000000000000000 ) ;
#54927 = CARTESIAN_POINT ( 'NONE',  ( 25.90000000000000213, 20.60000000000000142, -13.86939075806900057 ) ) ;
#54926 = VECTOR ( 'NONE', #5678, 1000.000000000000000 ) ;
#54928 = FACE_OUTER_BOUND ( 'NONE', #35839, .T. ) ;
#54929 = CARTESIAN_POINT ( 'NONE',  ( 49.00000000000000000, -5.000000000000000000, 0.000000000000000000 ) ) ;
#54930 = DIRECTION ( 'NONE',  ( 1.000000000000000000, -0.000000000000000000, 0.000000000000000000 ) ) ;
#54931 = AXIS2_PLACEMENT_3D ( 'NONE', #30552, #36197, #52474 ) ;
#54932 = AXIS2_PLACEMENT_3D ( 'NONE', #61718, #62059, #47133 ) ;
#54933 = VECTOR ( 'NONE', #50156, 1000.000000000000000 ) ;
#54934 = DIRECTION ( 'NONE',  ( 1.000000000000000000, -0.000000000000000000, 0.000000000000000000 ) ) ;
#54935 = ORIENTED_EDGE ( 'NONE', *, *, #35931, .T. ) ;
#54936 = VERTEX_POINT ( 'NONE', #20644 ) ;
#54937 = VECTOR ( 'NONE', #22963, 1000.000000000000000 ) ;
#54938 = CARTESIAN_POINT ( 'NONE',  ( 8.250000000000005329, -7.249999999999998224, -26.00000000000001066 ) ) ;
#54939 = CARTESIAN_POINT ( 'NONE',  ( 29.89999999999999858, -21.00000000000001421, -13.86939075806900945 ) ) ;
#54940 = EDGE_CURVE ( 'NONE', #16599, #48981, #67688, .T. ) ;
#54941 = AXIS2_PLACEMENT_3D ( 'NONE', #52590, #36666, #8743 ) ;
#54942 = ORIENTED_EDGE ( 'NONE', *, *, #33238, .T. ) ;
#54943 = CARTESIAN_POINT ( 'NONE',  ( -4.135079735113208699, -3.677663764522613121, 54.00000000000000711 ) ) ;
#54944 = CARTESIAN_POINT ( 'NONE',  ( 8.900000000000005684, -0.2000000000089119934, 8.909539772616881237E-12 ) ) ;
#54945 = ADVANCED_FACE ( 'NONE', ( #14308 ), #57430, .T. ) ;
#54946 = ORIENTED_EDGE ( 'NONE', *, *, #6405, .F. ) ;
#54947 = DIRECTION ( 'NONE',  ( 0.000000000000000000, 0.000000000000000000, 1.000000000000000000 ) ) ;
#54948 = DIRECTION ( 'NONE',  ( 0.000000000000000000, 1.000000000000000000, 0.000000000000000000 ) ) ;
#54949 = ORIENTED_EDGE ( 'NONE', *, *, #16243, .F. ) ;
#54950 = CARTESIAN_POINT ( 'NONE',  ( 4.186483450353337687, -11.78648345035337996, 195.0000000000000284 ) ) ;
#54951 = EDGE_CURVE ( 'NONE', #48961, #53340, #25261, .T. ) ;
#54952 = LINE ( 'NONE', #32673, #711 ) ;
#54953 =( NAMED_UNIT ( * ) SI_UNIT ( $, .STERADIAN. ) SOLID_ANGLE_UNIT ( ) );
#54954 = EDGE_CURVE ( 'NONE', #12339, #27421, #68394, .T. ) ;
#54955 = DIRECTION ( 'NONE',  ( 0.000000000000000000, 0.000000000000000000, -1.000000000000000000 ) ) ;
#54956 = EDGE_LOOP ( 'NONE', ( #58813, #13861, #19565, #68009 ) ) ;
#54958 = ORIENTED_EDGE ( 'NONE', *, *, #39358, .F. ) ;
#54957 = DIRECTION ( 'NONE',  ( -0.000000000000000000, -0.000000000000000000, 1.000000000000000000 ) ) ;
#54959 = CYLINDRICAL_SURFACE ( 'NONE', #34990, 0.3499999999999996447 ) ;
#54960 = DIRECTION ( 'NONE',  ( -1.000000000000000000, 0.000000000000000000, 0.000000000000000000 ) ) ;
#54961 = CARTESIAN_POINT ( 'NONE',  ( 8.900000000000005684, -21.00000000000000000, 18.00000000000000355 ) ) ;
#54962 = ORIENTED_EDGE ( 'NONE', *, *, #38797, .F. ) ;
#54963 = VECTOR ( 'NONE', #12706, 1000.000000000000000 ) ;
#54964 = DIRECTION ( 'NONE',  ( -1.000000000000000000, 0.000000000000000000, 0.000000000000000000 ) ) ;
#54965 = CARTESIAN_POINT ( 'NONE',  ( 25.50000000000000355, -5.200000000000001066, -20.24999999999999645 ) ) ;
#54966 = VECTOR ( 'NONE', #57723, 1000.000000000000000 ) ;
#54967 = EDGE_LOOP ( 'NONE', ( #34640, #34733, #48234, #57580 ) ) ;
#54968 = VERTEX_POINT ( 'NONE', #20300 ) ;
#54969 = EDGE_CURVE ( 'NONE', #31578, #31212, #12548, .T. ) ;
#54970 = CIRCLE ( 'NONE', #51570, 5.000000000000000000 ) ;
#54971 = VECTOR ( 'NONE', #52026, 1000.000000000000000 ) ;
#54972 = ORIENTED_EDGE ( 'NONE', *, *, #41350, .T. ) ;
#54973 = DIRECTION ( 'NONE',  ( -1.000000000000000000, 0.000000000000000000, 0.000000000000000000 ) ) ;
#54974 = DIRECTION ( 'NONE',  ( 1.000000000000000000, 0.000000000000000000, -0.000000000000000000 ) ) ;
#54975 = CARTESIAN_POINT ( 'NONE',  ( -7.250000000000000000, -7.449999999999998401, -9.500000000000001776 ) ) ;
#54976 = VECTOR ( 'NONE', #28134, 1000.000000000000114 ) ;
#54977 = VECTOR ( 'NONE', #27532, 1000.000000000000000 ) ;
#54978 = AXIS2_PLACEMENT_3D ( 'NONE', #13025, #50530, #2087 ) ;
#54979 = EDGE_LOOP ( 'NONE', ( #31901, #5001, #11821, #68721 ) ) ;
#54980 = ORIENTED_EDGE ( 'NONE', *, *, #17616, .T. ) ;
#54981 = ORIENTED_EDGE ( 'NONE', *, *, #4113, .F. ) ;
#54982 = CARTESIAN_POINT ( 'NONE',  ( -22.14589803375000088, -15.50000000000000000, -21.50000000000000000 ) ) ;
#54983 = AXIS2_PLACEMENT_3D ( 'NONE', #4317, #42472, #36835 ) ;
#54984 = AXIS2_PLACEMENT_3D ( 'NONE', #58179, #46860, #20003 ) ;
#54985 = ORIENTED_EDGE ( 'NONE', *, *, #25708, .T. ) ;
#54986 = ORIENTED_EDGE ( 'NONE', *, *, #10969, .T. ) ;
#54987 = ORIENTED_EDGE ( 'NONE', *, *, #33563, .T. ) ;
#54988 = VERTEX_POINT ( 'NONE', #69091 ) ;
#54989 = CIRCLE ( 'NONE', #11994, 0.3499999999999996447 ) ;
#54990 = CARTESIAN_POINT ( 'NONE',  ( 15.50000000000000000, -1.037157890325000054, -22.50000000000000000 ) ) ;
#54991 = ADVANCED_FACE ( 'NONE', ( #9704 ), #42569, .T. ) ;
#54993 = EDGE_LOOP ( 'NONE', ( #44438, #12981, #57709, #45088 ) ) ;
#54992 = CARTESIAN_POINT ( 'NONE',  ( -7.250000000000001776, -7.249999999999998224, -20.00000000000000000 ) ) ;
#54994 = LINE ( 'NONE', #1235, #35670 ) ;
#54995 = EDGE_CURVE ( 'NONE', #16805, #15647, #44205, .T. ) ;
#54996 = VECTOR ( 'NONE', #47419, 1000.000000000000000 ) ;
#54997 = CARTESIAN_POINT ( 'NONE',  ( 28.90000000000000213, 20.60000000000000142, 13.86939075806900057 ) ) ;
#54998 = LINE ( 'NONE', #54293, #824 ) ;
#54999 = ADVANCED_FACE ( 'NONE', ( #11089 ), #64161, .F. ) ;
#55000 = ORIENTED_EDGE ( 'NONE', *, *, #674, .T. ) ;
#55001 = CARTESIAN_POINT ( 'NONE',  ( 29.25000000000000000, -5.000000000000000000, 11.75000000000000000 ) ) ;
#55002 = CARTESIAN_POINT ( 'NONE',  ( 10.00000000000000000, -14.48845687959340012, -21.00000000000000000 ) ) ;
#55003 = CARTESIAN_POINT ( 'NONE',  ( 7.000000000000000000, -26.42999999999999972, 9.412893218813501051 ) ) ;
#55004 = ORIENTED_EDGE ( 'NONE', *, *, #11393, .F. ) ;
#55005 = FACE_OUTER_BOUND ( 'NONE', #4151, .T. ) ;
#55006 = CARTESIAN_POINT ( 'NONE',  ( 10.70000000000000107, -25.60000000000000142, 17.60000000000000142 ) ) ;
#55007 = LINE ( 'NONE', #6558, #17574 ) ;
#55008 = ADVANCED_FACE ( 'NONE', ( #27359 ), #65197, .T. ) ;
#55009 = AXIS2_PLACEMENT_3D ( 'NONE', #66470, #19078, #61495 ) ;
#55010 = ORIENTED_EDGE ( 'NONE', *, *, #50558, .F. ) ;
#55011 = CARTESIAN_POINT ( 'NONE',  ( 283.0000000000000568, -42.50000000000000000, 10.20000000000000107 ) ) ;
#55012 = DIRECTION ( 'NONE',  ( -0.000000000000000000, -0.000000000000000000, -1.000000000000000000 ) ) ;
#55013 = DIRECTION ( 'NONE',  ( -1.000000000000000000, 0.000000000000000000, 0.000000000000000000 ) ) ;
#55014 = VECTOR ( 'NONE', #54054, 1000.000000000000000 ) ;
#55015 = VECTOR ( 'NONE', #44783, 1000.000000000000000 ) ;
#55016 = DIRECTION ( 'NONE',  ( -1.000000000000000000, 6.308085367188447236E-15, 0.000000000000000000 ) ) ;
#55017 = DIRECTION ( 'NONE',  ( -1.000000000000000000, 3.016910393003147986E-15, 1.108394896831706469E-30 ) ) ;
#55018 = CARTESIAN_POINT ( 'NONE',  ( 111.9257688011041836, 10.00000000000000000, 281.4830310981151911 ) ) ;
#55019 = DIRECTION ( 'NONE',  ( 0.000000000000000000, 0.000000000000000000, 1.000000000000000000 ) ) ;
#55020 = VECTOR ( 'NONE', #27372, 1000.000000000000000 ) ;
#55021 = EDGE_CURVE ( 'NONE', #39380, #47318, #24987, .T. ) ;
#55022 = AXIS2_PLACEMENT_3D ( 'NONE', #29647, #9769, #58196 ) ;
#55023 =( GEOMETRIC_REPRESENTATION_CONTEXT ( 3 ) GLOBAL_UNCERTAINTY_ASSIGNED_CONTEXT ( ( #6187 ) ) GLOBAL_UNIT_ASSIGNED_CONTEXT ( ( #12318, #50165, #44855 ) ) REPRESENTATION_CONTEXT ( 'NONE', 'WORKASPACE' ) );
#55024 = VERTEX_POINT ( 'NONE', #27695 ) ;
#55025 = CARTESIAN_POINT ( 'NONE',  ( -7.813516549646789322, -11.78648345035335865, 195.0000000000000284 ) ) ;
#55026 = DIRECTION ( 'NONE',  ( 7.665540703601096574E-15, 1.000000000000000000, -0.000000000000000000 ) ) ;
#55027 = AXIS2_PLACEMENT_3D ( 'NONE', #41595, #9073, #30640 ) ;
#55028 = DIRECTION ( 'NONE',  ( -1.000000000000000000, 0.000000000000000000, -0.000000000000000000 ) ) ;
#55029 = VECTOR ( 'NONE', #24421, 1000.000000000000000 ) ;
#55030 = DIRECTION ( 'NONE',  ( 0.000000000000000000, 0.000000000000000000, -1.000000000000000000 ) ) ;
#55031 = ORIENTED_EDGE ( 'NONE', *, *, #41107, .F. ) ;
#55032 = FACE_OUTER_BOUND ( 'NONE', #27382, .T. ) ;
#55033 = FACE_OUTER_BOUND ( 'NONE', #48186, .T. ) ;
#55034 = ADVANCED_FACE ( 'NONE', ( #42912 ), #52097, .F. ) ;
#55035 = EDGE_CURVE ( 'NONE', #15894, #10947, #1319, .T. ) ;
#55036 = FACE_OUTER_BOUND ( 'NONE', #68352, .T. ) ;
#55037 = CARTESIAN_POINT ( 'NONE',  ( -25.50000000000000355, 0.000000000000000000, -24.12099999999999866 ) ) ;
#55038 = EDGE_CURVE ( 'NONE', #31475, #7660, #5795, .T. ) ;
#55039 = CARTESIAN_POINT ( 'NONE',  ( -25.50000000000000355, -15.50000000000000000, 24.50000000000000000 ) ) ;
#55040 = EDGE_CURVE ( 'NONE', #61720, #40050, #21703, .T. ) ;
#55041 = ORIENTED_EDGE ( 'NONE', *, *, #285, .T. ) ;
#55042 = VECTOR ( 'NONE', #42034, 1000.000000000000000 ) ;
#55043 = EDGE_CURVE ( 'NONE', #27624, #35699, #15705, .T. ) ;
#55044 = DIRECTION ( 'NONE',  ( -1.836970198721029934E-16, 1.836970198721036344E-16, -1.000000000000000000 ) ) ;
#55045 = CARTESIAN_POINT ( 'NONE',  ( 4.406483450353335662, -11.78648345035347766, 455.0000000000000568 ) ) ;
#55046 = VERTEX_POINT ( 'NONE', #69440 ) ;
#55047 = CARTESIAN_POINT ( 'NONE',  ( -8.566576262117353124, -9.703773737882732675, 26.00000000000000000 ) ) ;
#55048 = ORIENTED_EDGE ( 'NONE', *, *, #25417, .F. ) ;
#55049 = CARTESIAN_POINT ( 'NONE',  ( -6.651770455163781293, -7.357023737882790293, 54.00000000000000711 ) ) ;
#55050 = ORIENTED_EDGE ( 'NONE', *, *, #7064, .F. ) ;
#55051 = ORIENTED_EDGE ( 'NONE', *, *, #30443, .T. ) ;
#55052 = DIRECTION ( 'NONE',  ( -0.000000000000000000, -0.000000000000000000, -1.000000000000000000 ) ) ;
#55053 = ORIENTED_EDGE ( 'NONE', *, *, #66110, .F. ) ;
#55054 = FACE_OUTER_BOUND ( 'NONE', #13504, .T. ) ;
#55055 = LINE ( 'NONE', #49399, #67711 ) ;
#55056 = DIRECTION ( 'NONE',  ( 0.000000000000000000, 1.000000000000000000, 0.000000000000000000 ) ) ;
#55057 = VECTOR ( 'NONE', #27523, 1000.000000000000000 ) ;
#55058 = ORIENTED_EDGE ( 'NONE', *, *, #63855, .T. ) ;
#55059 = ORIENTED_EDGE ( 'NONE', *, *, #5575, .T. ) ;
#55060 = CARTESIAN_POINT ( 'NONE',  ( 13.90000000000000036, 0.000000000000000000, 6.464807985006735683E-16 ) ) ;
#55061 = CARTESIAN_POINT ( 'NONE',  ( -1.677516549646676625, 10.73351654964656987, 455.0000000000000568 ) ) ;
#55062 = EDGE_LOOP ( 'NONE', ( #39312, #33661, #7900, #20072 ) ) ;
#55063 = VERTEX_POINT ( 'NONE', #37624 ) ;
#55064 = VERTEX_POINT ( 'NONE', #22047 ) ;
#55065 = VECTOR ( 'NONE', #55017, 1000.000000000000000 ) ;
#55066 = AXIS2_PLACEMENT_3D ( 'NONE', #35573, #20376, #13664 ) ;
#55067 = CARTESIAN_POINT ( 'NONE',  ( 7.616533956692244089, 8.393516549646575342, 455.0000000000000568 ) ) ;
#55069 = ORIENTED_EDGE ( 'NONE', *, *, #36771, .F. ) ;
#55068 = CARTESIAN_POINT ( 'NONE',  ( 36.90000000000000568, -21.00000000000000000, 13.86939075806900057 ) ) ;
#55070 = VECTOR ( 'NONE', #15287, 1000.000000000000000 ) ;
#55071 = VECTOR ( 'NONE', #53875, 1000.000000000000000 ) ;
#55072 = LINE ( 'NONE', #49058, #17556 ) ;
#55073 = CARTESIAN_POINT ( 'NONE',  ( -7.250000000000000888, 8.250000000000001776, -26.00000000000001066 ) ) ;
#55074 = FACE_OUTER_BOUND ( 'NONE', #51340, .T. ) ;
#55075 = ORIENTED_EDGE ( 'NONE', *, *, #67010, .T. ) ;
#55076 = EDGE_LOOP ( 'NONE', ( #61634, #60310, #31914, #31242, #44399, #65894 ) ) ;
#55077 = EDGE_CURVE ( 'NONE', #4323, #52471, #850, .T. ) ;
#55078 = EDGE_CURVE ( 'NONE', #63544, #167, #58840, .T. ) ;
#55079 = VECTOR ( 'NONE', #52972, 1000.000000000000000 ) ;
#55080 = EDGE_CURVE ( 'NONE', #24515, #18477, #64842, .T. ) ;
#55081 = FACE_OUTER_BOUND ( 'NONE', #68906, .T. ) ;
#55082 = DIRECTION ( 'NONE',  ( 0.000000000000000000, 0.000000000000000000, -1.000000000000000000 ) ) ;
#55083 = AXIS2_PLACEMENT_3D ( 'NONE', #65684, #64643, #24645 ) ;
#55084 = CARTESIAN_POINT ( 'NONE',  ( 7.450000000000003730, -7.249999999999997335, -25.50000000000000355 ) ) ;
#55085 = LINE ( 'NONE', #23925, #30222 ) ;
#55087 = VERTEX_POINT ( 'NONE', #47868 ) ;
#55086 =( NAMED_UNIT ( * ) SI_UNIT ( $, .STERADIAN. ) SOLID_ANGLE_UNIT ( ) );
#55088 = ORIENTED_EDGE ( 'NONE', *, *, #45725, .T. ) ;
#55089 = DIRECTION ( 'NONE',  ( -1.836970198721029934E-16, 1.836970198721036590E-16, -1.000000000000000000 ) ) ;
#55090 = FACE_OUTER_BOUND ( 'NONE', #34678, .T. ) ;
#55091 = CARTESIAN_POINT ( 'NONE',  ( -11.31351654964679021, -7.806483450353372433, 455.0000000000000568 ) ) ;
#55092 = DIRECTION ( 'NONE',  ( -1.836970198721029934E-16, 1.836970198721036344E-16, -1.000000000000000000 ) ) ;
#55093 = CARTESIAN_POINT ( 'NONE',  ( 7.250000000000004441, 7.450000000000001954, -9.500000000000001776 ) ) ;
#55094 = ORIENTED_EDGE ( 'NONE', *, *, #58327, .T. ) ;
#55095 = PLANE ( 'NONE',  #34643 ) ;
#55096 = CARTESIAN_POINT ( 'NONE',  ( 0.000000000000000000, -7.449999999999998401, -19.50000000000000000 ) ) ;
#55097 = FILL_AREA_STYLE_COLOUR ( '', #65038 ) ;
#55098 = CARTESIAN_POINT ( 'NONE',  ( 2.290483450353350658, -9.841277389592708147, 195.0000000000000284 ) ) ;
#55099 = DIRECTION ( 'NONE',  ( -1.000000000000000000, 0.000000000000000000, 0.000000000000000000 ) ) ;
#55100 = CARTESIAN_POINT ( 'NONE',  ( -8.750000000000001776, 0.000000000000000000, -30.00000000000001066 ) ) ;
#55101 = CARTESIAN_POINT ( 'NONE',  ( -7.250000000000000888, 7.250000000000001776, -9.000000000000001776 ) ) ;
#55102 = ORIENTED_EDGE ( 'NONE', *, *, #47143, .T. ) ;
#55103 = DIRECTION ( 'NONE',  ( 0.000000000000000000, 0.000000000000000000, 1.000000000000000000 ) ) ;
#55104 = PLANE ( 'NONE',  #3367 ) ;
#55105 = ORIENTED_EDGE ( 'NONE', *, *, #28916, .T. ) ;
#55106 = CARTESIAN_POINT ( 'NONE',  ( -6.642976262117260333, 9.897976262117179402, 54.00000000000000711 ) ) ;
#55107 = CARTESIAN_POINT ( 'NONE',  ( 20.90000000000000213, -0.2000000000089119934, 8.909539772616881237E-12 ) ) ;
#55108 = CARTESIAN_POINT ( 'NONE',  ( 38.90000000000000568, -14.06939075806900874, 20.80000000000001137 ) ) ;
#55109 = DIRECTION ( 'NONE',  ( -0.7671651518153087546, -0.6414496315691469164, 2.309356642089053889E-17 ) ) ;
#55110 = DIRECTION ( 'NONE',  ( 0.000000000000000000, 0.000000000000000000, 1.000000000000000000 ) ) ;
#55111 = EDGE_CURVE ( 'NONE', #19113, #62883, #3548, .T. ) ;
#55112 = DIRECTION ( 'NONE',  ( -0.000000000000000000, 3.673940397442059868E-16, -1.000000000000000000 ) ) ;
#55113 = ORIENTED_EDGE ( 'NONE', *, *, #27013, .T. ) ;
#55114 = EDGE_CURVE ( 'NONE', #22946, #8396, #33003, .T. ) ;
#55115 = LINE ( 'NONE', #5640, #18693 ) ;
#55116 = ADVANCED_FACE ( 'NONE', ( #4746 ), #49276, .T. ) ;
#55117 = ORIENTED_EDGE ( 'NONE', *, *, #14219, .T. ) ;
#55118 = CARTESIAN_POINT ( 'NONE',  ( 4.396432944014527777, -8.406483450353384512, 195.0000000000000284 ) ) ;
#55119 = AXIS2_PLACEMENT_3D ( 'NONE', #56536, #8086, #19745 ) ;
#55120 = AXIS2_PLACEMENT_3D ( 'NONE', #34489, #56080, #7630 ) ;
#55121 = LINE ( 'NONE', #37473, #14122 ) ;
#55122 = CARTESIAN_POINT ( 'NONE',  ( -9.547976262117227719, -2.544523737882729453, 54.00000000000000711 ) ) ;
#55123 = EDGE_LOOP ( 'NONE', ( #48160, #36532, #57749, #853 ) ) ;
#55124 = ORIENTED_EDGE ( 'NONE', *, *, #45019, .F. ) ;
#55125 = LINE ( 'NONE', #66753, #45401 ) ;
#55127 = ORIENTED_EDGE ( 'NONE', *, *, #28371, .F. ) ;
#55126 = ADVANCED_FACE ( 'NONE', ( #31624 ), #53201, .F. ) ;
#55128 = EDGE_LOOP ( 'NONE', ( #30340, #66811, #8047, #61 ) ) ;
#55129 = CIRCLE ( 'NONE', #28024, 0.5249999999999990230 ) ;
#55130 = PRODUCT_DEFINITION_CONTEXT ( 'detailed design', #41764, 'design' ) ;
#55131 = FACE_OUTER_BOUND ( 'NONE', #6752, .T. ) ;
#55132 = CARTESIAN_POINT ( 'NONE',  ( 11.00000000000000000, -9.487228132326899654, 12.50000000000000000 ) ) ;
#55133 = CARTESIAN_POINT ( 'NONE',  ( -8.250000000000001776, 7.250000000000000888, -26.00000000000001066 ) ) ;
#55134 = ORIENTED_EDGE ( 'NONE', *, *, #20105, .F. ) ;
#55135 = CARTESIAN_POINT ( 'NONE',  ( -11.00000000000000000, -11.70000000000000284, -12.50000000000000000 ) ) ;
#55137 = DIRECTION ( 'NONE',  ( -1.000000000000000000, 0.000000000000000000, 0.000000000000000000 ) ) ;
#55136 = CARTESIAN_POINT ( 'NONE',  ( -3.842976262117221875, 10.30047626211716860, 54.00000000000000711 ) ) ;
#55138 = VERTEX_POINT ( 'NONE', #65862 ) ;
#55140 = EDGE_LOOP ( 'NONE', ( #50265, #57289, #13024, #13831, #42363, #11311, #59385, #17897 ) ) ;
#55139 = LINE ( 'NONE', #13014, #48955 ) ;
#55141 = ORIENTED_EDGE ( 'NONE', *, *, #6936, .T. ) ;
#55142 = CARTESIAN_POINT ( 'NONE',  ( -164.0000000000000000, 9.833141174518347682, 455.0000000000000568 ) ) ;
#55143 = CARTESIAN_POINT ( 'NONE',  ( 30.90000000000000213, 0.000000000000000000, 2.458500000000000796 ) ) ;
#55144 = LINE ( 'NONE', #7373, #3179 ) ;
#55145 = ORIENTED_EDGE ( 'NONE', *, *, #59149, .T. ) ;
#55146 = ORIENTED_EDGE ( 'NONE', *, *, #65570, .T. ) ;
#55147 = PLANE ( 'NONE',  #54978 ) ;
#55148 = CYLINDRICAL_SURFACE ( 'NONE', #11981, 0.5000000000001357803 ) ;
#55149 = ORIENTED_EDGE ( 'NONE', *, *, #56407, .T. ) ;
#55150 = EDGE_CURVE ( 'NONE', #24019, #19038, #50989, .T. ) ;
#55151 = CARTESIAN_POINT ( 'NONE',  ( -8.250000000000001776, 7.250000000000000888, -26.00000000000001066 ) ) ;
#55152 = CYLINDRICAL_SURFACE ( 'NONE', #63971, 0.4999999999991850963 ) ;
#55153 = CARTESIAN_POINT ( 'NONE',  ( 7.250000000000005329, -7.449999999999998401, -19.00000000000000000 ) ) ;
#55154 = ORIENTED_EDGE ( 'NONE', *, *, #15016, .F. ) ;
#55155 = AXIS2_PLACEMENT_3D ( 'NONE', #39364, #55979, #55629 ) ;
#55156 =( BOUNDED_CURVE ( )  B_SPLINE_CURVE ( 3, ( #29567, #55419, #61040, #28189 ),
 .UNSPECIFIED., .F., .F. ) 
 B_SPLINE_CURVE_WITH_KNOTS ( ( 4, 4 ),
 ( 5.387520513321711668, 5.560451059366170234 ),
 .UNSPECIFIED. ) 
 CURVE ( )  GEOMETRIC_REPRESENTATION_ITEM ( )  RATIONAL_B_SPLINE_CURVE ( ( 1.000000000000000000, 0.9975094710839671475, 0.9975094710839671475, 1.000000000000000000 ) ) 
 REPRESENTATION_ITEM ( '' )  );
#55157 = DIRECTION ( 'NONE',  ( 0.000000000000000000, 0.000000000000000000, -1.000000000000000000 ) ) ;
#55158 = FACE_OUTER_BOUND ( 'NONE', #58538, .T. ) ;
#55160 = ORIENTED_EDGE ( 'NONE', *, *, #8296, .F. ) ;
#55159 = CARTESIAN_POINT ( 'NONE',  ( 4.396432944014526889, -8.606483450353382025, 195.0000000000000284 ) ) ;
#55162 = EDGE_LOOP ( 'NONE', ( #45314, #17734 ) ) ;
#55161 = DIRECTION ( 'NONE',  ( 1.000000000000000000, 0.000000000000000000, 0.000000000000000000 ) ) ;
#55163 = LINE ( 'NONE', #54482, #50565 ) ;
#55164 = CIRCLE ( 'NONE', #50655, 0.4999999999945519691 ) ;
#55165 = EDGE_CURVE ( 'NONE', #36190, #13533, #8055, .T. ) ;
#55166 = CARTESIAN_POINT ( 'NONE',  ( 15.50000000000000000, -5.000000000000000000, 22.50000000000000000 ) ) ;
#55167 = CARTESIAN_POINT ( 'NONE',  ( 7.826483450353421745, 11.77351654964657257, 455.0000000000000568 ) ) ;
#55168 = CARTESIAN_POINT ( 'NONE',  ( -7.450000000000001954, -7.249999999999998224, -7.500000000000000000 ) ) ;
#55169 = DIRECTION ( 'NONE',  ( 1.000000000000000000, 0.000000000000000000, 0.000000000000000000 ) ) ;
#55170 = ADVANCED_FACE ( 'NONE', ( #39674 ), #17777, .T. ) ;
#55171 = DIRECTION ( 'NONE',  ( 0.000000000000000000, -1.000000000000000000, 0.000000000000000000 ) ) ;
#55172 = VERTEX_POINT ( 'NONE', #18108 ) ;
#55173 = DIRECTION ( 'NONE',  ( -1.000000000000000000, 0.000000000000000000, 0.000000000000000000 ) ) ;
#55174 = DIRECTION ( 'NONE',  ( 0.000000000000000000, 0.000000000000000000, 1.000000000000000000 ) ) ;
#55175 = CIRCLE ( 'NONE', #15666, 24.99999999998794920 ) ;
#55177 = ORIENTED_EDGE ( 'NONE', *, *, #20290, .F. ) ;
#55176 = DIRECTION ( 'NONE',  ( 1.000000000000000000, -0.000000000000000000, 0.000000000000000000 ) ) ;
#55178 = CARTESIAN_POINT ( 'NONE',  ( 9.912023737882782015, 3.667976262117150998, 54.00000000000000711 ) ) ;
#55179 = CARTESIAN_POINT ( 'NONE',  ( 11.19000000000000128, -12.00000000000000000, -5.000000000000000000 ) ) ;
#55180 = ORIENTED_EDGE ( 'NONE', *, *, #61318, .F. ) ;
#55181 = DIRECTION ( 'NONE',  ( 1.000000000000000000, 0.000000000000000000, 0.000000000000000000 ) ) ;
#55182 = LINE ( 'NONE', #33271, #62210 ) ;
#55183 = ORIENTED_EDGE ( 'NONE', *, *, #12121, .F. ) ;
#55184 = CARTESIAN_POINT ( 'NONE',  ( 9.900000000000000355, 0.000000000000000000, 2.154935995002245639E-16 ) ) ;
#55185 = CYLINDRICAL_SURFACE ( 'NONE', #15740, 0.2000000000000005107 ) ;
#55186 = DIRECTION ( 'NONE',  ( 1.000000000000000000, 0.000000000000000000, 0.000000000000000000 ) ) ;
#55187 = FACE_OUTER_BOUND ( 'NONE', #68090, .T. ) ;
#55188 = EDGE_CURVE ( 'NONE', #1760, #51933, #29080, .T. ) ;
#55189 = CARTESIAN_POINT ( 'NONE',  ( 40.90000000000000568, 0.000000000000000000, 3.447897592003593022E-15 ) ) ;
#55190 = VERTEX_POINT ( 'NONE', #17423 ) ;
#55191 = ADVANCED_FACE ( 'NONE', ( #56298 ), #38989, .T. ) ;
#55192 = CARTESIAN_POINT ( 'NONE',  ( 46.39999999999999858, 21.00000000000000000, -0.7500000000000000000 ) ) ;
#55193 = VERTEX_POINT ( 'NONE', #11764 ) ;
#55194 = EDGE_CURVE ( 'NONE', #23202, #4292, #39655, .T. ) ;
#55195 = ORIENTED_EDGE ( 'NONE', *, *, #54322, .F. ) ;
#55196 = LINE ( 'NONE', #27980, #58460 ) ;
#55197 = CARTESIAN_POINT ( 'NONE',  ( 24.00000000000000000, -16.28999999999710369, -14.50000000000000000 ) ) ;
#55198 = ADVANCED_FACE ( 'NONE', ( #7146 ), #61581, .F. ) ;
#55199 = FACE_OUTER_BOUND ( 'NONE', #24513, .T. ) ;
#55200 = DIRECTION ( 'NONE',  ( 1.000000000000000000, -5.981805089575194965E-17, 0.000000000000000000 ) ) ;
#55201 = ORIENTED_EDGE ( 'NONE', *, *, #62265, .T. ) ;
#55202 = EDGE_CURVE ( 'NONE', #46144, #27925, #1861, .T. ) ;
#55203 = VERTEX_POINT ( 'NONE', #49942 ) ;
#55205 = VERTEX_POINT ( 'NONE', #44985 ) ;
#55204 = DIRECTION ( 'NONE',  ( 0.000000000000000000, -0.7096009616570518874, -0.7046037717862339012 ) ) ;
#55207 = ORIENTED_EDGE ( 'NONE', *, *, #7562, .T. ) ;
#55206 = EDGE_CURVE ( 'NONE', #47162, #29352, #66556, .T. ) ;
#55208 = AXIS2_PLACEMENT_3D ( 'NONE', #11373, #32610, #49554 ) ;
#55209 = CARTESIAN_POINT ( 'NONE',  ( 8.250000000000005329, -8.249999999999998224, -26.00000000000001066 ) ) ;
#55210 = CARTESIAN_POINT ( 'NONE',  ( 75.42576880091937142, 10.00000000000000000, 289.4830310981789125 ) ) ;
#55211 = LINE ( 'NONE', #23023, #15044 ) ;
#55212 = VECTOR ( 'NONE', #44280, 1000.000000000000000 ) ;
#55213 = DIRECTION ( 'NONE',  ( -0.000000000000000000, -0.000000000000000000, -1.000000000000000000 ) ) ;
#55215 = CARTESIAN_POINT ( 'NONE',  ( 9.737023737882815055, -7.969523737882825642, 54.00000000000000711 ) ) ;
#55214 = FACE_OUTER_BOUND ( 'NONE', #46791, .T. ) ;
#55216 = EDGE_LOOP ( 'NONE', ( #36082, #40342, #14709, #18005 ) ) ;
#55218 = VERTEX_POINT ( 'NONE', #34358 ) ;
#55217 = CYLINDRICAL_SURFACE ( 'NONE', #28483, 0.1999999999999987899 ) ;
#55219 = ORIENTED_EDGE ( 'NONE', *, *, #15237, .F. ) ;
#55220 = VERTEX_POINT ( 'NONE', #44287 ) ;
#55221 = VECTOR ( 'NONE', #43185, 999.9999999999998863 ) ;
#55222 = CARTESIAN_POINT ( 'NONE',  ( 7.250000000000005329, -7.449999999999998401, -7.000000000000000000 ) ) ;
#55224 = CIRCLE ( 'NONE', #50714, 0.1749999999999989342 ) ;
#55223 = VECTOR ( 'NONE', #33519, 1000.000000000000000 ) ;
#55225 = LINE ( 'NONE', #6767, #62460 ) ;
#55226 = DIRECTION ( 'NONE',  ( -1.000000000000000000, 0.000000000000000000, 0.000000000000000000 ) ) ;
#55227 = EDGE_CURVE ( 'NONE', #23509, #24837, #22733, .T. ) ;
#55228 = ORIENTED_EDGE ( 'NONE', *, *, #56051, .F. ) ;
#55229 = VERTEX_POINT ( 'NONE', #7503 ) ;
#55230 = VECTOR ( 'NONE', #48137, 1000.000000000000000 ) ;
#55231 = LINE ( 'NONE', #17743, #42207 ) ;
#55232 = DIRECTION ( 'NONE',  ( 1.000000000000000000, -2.309061475090597584E-14, 1.836970198720987533E-16 ) ) ;
#55233 = ORIENTED_EDGE ( 'NONE', *, *, #27239, .T. ) ;
#55234 = EDGE_CURVE ( 'NONE', #26006, #42528, #23771, .T. ) ;
#55235 = ORIENTED_EDGE ( 'NONE', *, *, #41014, .F. ) ;
#55236 = DIRECTION ( 'NONE',  ( 0.000000000000000000, 0.000000000000000000, 1.000000000000000000 ) ) ;
#55237 = CARTESIAN_POINT ( 'NONE',  ( 9.106483450353415776, 10.08346604330773744, 455.0000000000000568 ) ) ;
#55238 = ORIENTED_EDGE ( 'NONE', *, *, #10860, .F. ) ;
#55239 = EDGE_CURVE ( 'NONE', #2916, #12117, #45324, .T. ) ;
#55240 = CARTESIAN_POINT ( 'NONE',  ( -9.390476262117200434, -0.9555237378827314831, 54.00000000000000711 ) ) ;
#55242 = ORIENTED_EDGE ( 'NONE', *, *, #51590, .T. ) ;
#55241 = DIRECTION ( 'NONE',  ( -1.000000000000000000, 0.000000000000000000, 0.000000000000000000 ) ) ;
#55243 = ORIENTED_EDGE ( 'NONE', *, *, #24137, .F. ) ;
#55244 = CARTESIAN_POINT ( 'NONE',  ( 11.00000000000000000, -17.50000000000000000, -15.70500000000000007 ) ) ;
#55245 = DIRECTION ( 'NONE',  ( -0.000000000000000000, 3.673940397442059868E-16, -1.000000000000000000 ) ) ;
#55246 = CARTESIAN_POINT ( 'NONE',  ( 11.00000000000000000, -11.50000000000000000, -15.00000000000000000 ) ) ;
#55247 = FACE_OUTER_BOUND ( 'NONE', #44692, .T. ) ;
#55248 = DIRECTION ( 'NONE',  ( 0.000000000000000000, -3.673940397442059868E-16, 1.000000000000000000 ) ) ;
#55249 = AXIS2_PLACEMENT_3D ( 'NONE', #60133, #26939, #67 ) ;
#55250 = DIRECTION ( 'NONE',  ( 1.000000000000000000, 0.000000000000000000, 0.000000000000000000 ) ) ;
#55251 = EDGE_CURVE ( 'NONE', #34031, #68975, #53275, .T. ) ;
#55252 = VERTEX_POINT ( 'NONE', #7842 ) ;
#55253 = DIRECTION ( 'NONE',  ( 0.000000000000000000, 0.000000000000000000, 1.000000000000000000 ) ) ;
#55254 = VECTOR ( 'NONE', #46224, 1000.000000000000000 ) ;
#55255 = CIRCLE ( 'NONE', #31603, 0.1999999999999996503 ) ;
#55256 = ORIENTED_EDGE ( 'NONE', *, *, #58339, .F. ) ;
#55257 = DIRECTION ( 'NONE',  ( 0.000000000000000000, 0.000000000000000000, 1.000000000000000000 ) ) ;
#55258 = CARTESIAN_POINT ( 'NONE',  ( -5.242976262117259978, 5.242976262117182706, 54.00000000000000711 ) ) ;
#55259 = ADVANCED_FACE ( 'NONE', ( #24116 ), #29418, .T. ) ;
#55260 = DIRECTION ( 'NONE',  ( -0.000000000000000000, -0.000000000000000000, -1.000000000000000000 ) ) ;
#55261 = ADVANCED_FACE ( 'NONE', ( #28045 ), #49605, .F. ) ;
#55262 = DIRECTION ( 'NONE',  ( 1.000000000000000000, -0.000000000000000000, -0.000000000000000000 ) ) ;
#55263 = CIRCLE ( 'NONE', #45094, 0.4999999999991868727 ) ;
#55264 = FACE_OUTER_BOUND ( 'NONE', #41848, .T. ) ;
#55265 = EDGE_CURVE ( 'NONE', #52459, #48929, #56646, .T. ) ;
#55266 = ORIENTED_EDGE ( 'NONE', *, *, #53200, .T. ) ;
#55267 = EDGE_CURVE ( 'NONE', #38943, #59582, #45305, .T. ) ;
#55268 = EDGE_CURVE ( 'NONE', #58882, #1276, #13509, .T. ) ;
#55269 = ORIENTED_EDGE ( 'NONE', *, *, #10867, .F. ) ;
#55270 = AXIS2_PLACEMENT_3D ( 'NONE', #68050, #14315, #13948 ) ;
#55271 = CYLINDRICAL_SURFACE ( 'NONE', #18950, 4.000000000000000000 ) ;
#55272 = DIRECTION ( 'NONE',  ( 0.000000000000000000, 1.000000000000000000, 0.000000000000000000 ) ) ;
#55273 = EDGE_CURVE ( 'NONE', #47489, #18717, #54376, .T. ) ;
#55274 = VECTOR ( 'NONE', #19259, 1000.000000000000000 ) ;
#55275 = ORIENTED_EDGE ( 'NONE', *, *, #29548, .F. ) ;
#55276 = EDGE_CURVE ( 'NONE', #15671, #9143, #41075, .T. ) ;
#55277 = DIRECTION ( 'NONE',  ( 0.000000000000000000, 3.673940397442059868E-16, -1.000000000000000000 ) ) ;
#55278 = VERTEX_POINT ( 'NONE', #61943 ) ;
#55279 = ORIENTED_EDGE ( 'NONE', *, *, #20762, .F. ) ;
#55280 = EDGE_CURVE ( 'NONE', #4772, #29478, #35774, .T. ) ;
#55281 = DIRECTION ( 'NONE',  ( 0.000000000000000000, -0.1249999999999996531, -0.9921567416492215186 ) ) ;
#55282 = AXIS2_PLACEMENT_3D ( 'NONE', #9478, #67825, #62867 ) ;
#55283 = DIRECTION ( 'NONE',  ( 1.000000000000000000, 0.000000000000000000, 0.000000000000000000 ) ) ;
#55284 = ORIENTED_EDGE ( 'NONE', *, *, #25524, .F. ) ;
#55285 = CARTESIAN_POINT ( 'NONE',  ( -6.835476262117333057, -10.31452373788278543, 54.00000000000000711 ) ) ;
#55286 = LINE ( 'NONE', #38335, #60546 ) ;
#55287 = SURFACE_STYLE_FILL_AREA ( #43970 ) ;
#55288 = DIRECTION ( 'NONE',  ( 0.000000000000000000, 0.000000000000000000, -1.000000000000000000 ) ) ;
#55289 = EDGE_CURVE ( 'NONE', #39379, #20422, #2899, .T. ) ;
#55290 = ORIENTED_EDGE ( 'NONE', *, *, #6487, .T. ) ;
#55292 = ORIENTED_EDGE ( 'NONE', *, *, #34772, .F. ) ;
#55291 = LINE ( 'NONE', #34044, #4706 ) ;
#55293 = ADVANCED_FACE ( 'NONE', ( #41778 ), #36478, .F. ) ;
#55294 = CARTESIAN_POINT ( 'NONE',  ( 10.31452373788281562, -6.849523737882823760, 54.00000000000000711 ) ) ;
#55295 = CARTESIAN_POINT ( 'NONE',  ( -8.916576262117258622, 9.689726262117185129, 54.00000000000000711 ) ) ;
#55296 = CARTESIAN_POINT ( 'NONE',  ( 7.250000000000005329, 7.250000000000000888, -18.50000000000000000 ) ) ;
#55297 = AXIS2_PLACEMENT_3D ( 'NONE', #61736, #1308, #66690 ) ;
#55298 = LINE ( 'NONE', #50326, #66904 ) ;
#55299 = ORIENTED_EDGE ( 'NONE', *, *, #26051, .T. ) ;
#55300 = PLANE ( 'NONE',  #45767 ) ;
#55301 = DIRECTION ( 'NONE',  ( -1.000000000000000000, 1.185108578570163402E-14, 1.836970198721051628E-16 ) ) ;
#55302 = VERTEX_POINT ( 'NONE', #63007 ) ;
#55303 = EDGE_CURVE ( 'NONE', #47033, #8022, #56986, .T. ) ;
#55304 = ORIENTED_EDGE ( 'NONE', *, *, #17695, .F. ) ;
#55305 = ORIENTED_EDGE ( 'NONE', *, *, #4548, .T. ) ;
#55306 = DIRECTION ( 'NONE',  ( 1.000000000000000000, 0.000000000000000000, 0.000000000000000000 ) ) ;
#55307 = CARTESIAN_POINT ( 'NONE',  ( -9.293516549646779978, -10.92648345035333790, 195.0000000000000284 ) ) ;
#55308 = AXIS2_PLACEMENT_3D ( 'NONE', #38755, #49388, #21804 ) ;
#55309 = CIRCLE ( 'NONE', #46256, 0.3499999999999996447 ) ;
#55310 = CARTESIAN_POINT ( 'NONE',  ( -7.259684009079930611, 4.188533722949235205, 195.0000000000000284 ) ) ;
#55311 = CARTESIAN_POINT ( 'NONE',  ( 9.562023737882814345, -7.969523737882814984, 26.00000000000000000 ) ) ;
#55312 = ORIENTED_EDGE ( 'NONE', *, *, #30738, .F. ) ;
#55313 = ORIENTED_EDGE ( 'NONE', *, *, #35159, .T. ) ;
#55314 = VERTEX_POINT ( 'NONE', #4328 ) ;
#55315 = VECTOR ( 'NONE', #26838, 1000.000000000000000 ) ;
#55316 = LINE ( 'NONE', #530, #59921 ) ;
#55317 = ORIENTED_EDGE ( 'NONE', *, *, #49440, .F. ) ;
#55318 = VERTEX_POINT ( 'NONE', #68669 ) ;
#55319 = ORIENTED_EDGE ( 'NONE', *, *, #20762, .T. ) ;
#55320 = VECTOR ( 'NONE', #27970, 1000.000000000000227 ) ;
#55321 = EDGE_CURVE ( 'NONE', #64507, #40247, #48772, .T. ) ;
#55322 = VERTEX_POINT ( 'NONE', #24480 ) ;
#55323 = DIRECTION ( 'NONE',  ( 1.000000000000000000, -5.981805089575194965E-17, 0.000000000000000000 ) ) ;
#55324 = VECTOR ( 'NONE', #24179, 1000.000000000000000 ) ;
#55326 = ORIENTED_EDGE ( 'NONE', *, *, #68697, .T. ) ;
#55325 = CARTESIAN_POINT ( 'NONE',  ( 11.78648345035335865, 7.813516549646607245, 195.0000000000000284 ) ) ;
#55327 = CIRCLE ( 'NONE', #7907, 0.9999999999999991118 ) ;
#55328 = EDGE_CURVE ( 'NONE', #32653, #51904, #8544, .T. ) ;
#55329 = CARTESIAN_POINT ( 'NONE',  ( -9.690000000000001279, 10.50000000000000178, 0.000000000000000000 ) ) ;
#55330 = CARTESIAN_POINT ( 'NONE',  ( -10.30047626211725742, 6.835476262117182955, 54.00000000000000711 ) ) ;
#55331 = CARTESIAN_POINT ( 'NONE',  ( 10.31452373788280674, 6.835476262117182067, 54.00000000000000711 ) ) ;
#55332 = EDGE_CURVE ( 'NONE', #59233, #30962, #68309, .T. ) ;
#55333 = ORIENTED_EDGE ( 'NONE', *, *, #58802, .T. ) ;
#55334 = VECTOR ( 'NONE', #47514, 1000.000000000000000 ) ;
#55335 = EDGE_CURVE ( 'NONE', #2382, #13669, #30124, .T. ) ;
#55336 = DIRECTION ( 'NONE',  ( 0.000000000000000000, 0.000000000000000000, 1.000000000000000000 ) ) ;
#55337 = LINE ( 'NONE', #1571, #43556 ) ;
#55338 = FACE_OUTER_BOUND ( 'NONE', #64821, .T. ) ;
#55339 = EDGE_CURVE ( 'NONE', #4916, #43945, #43107, .T. ) ;
#55340 = VERTEX_POINT ( 'NONE', #14920 ) ;
#55341 = FACE_BOUND ( 'NONE', #57405, .T. ) ;
#55342 = LINE ( 'NONE', #18535, #32059 ) ;
#55343 = CARTESIAN_POINT ( 'NONE',  ( 14.89999999999999680, 13.66939075806899950, 20.80000000000000426 ) ) ;
#55344 = AXIS2_PLACEMENT_3D ( 'NONE', #60697, #18595, #55399 ) ;
#55345 = VERTEX_POINT ( 'NONE', #19508 ) ;
#55346 = DIRECTION ( 'NONE',  ( -1.000000000000000000, 0.000000000000000000, 0.000000000000000000 ) ) ;
#55347 = DIRECTION ( 'NONE',  ( 0.000000000000000000, 0.000000000000000000, 1.000000000000000000 ) ) ;
#55348 = DIRECTION ( 'NONE',  ( 1.156482317317870187E-14, 1.000000000000000000, 0.000000000000000000 ) ) ;
#55349 = EDGE_CURVE ( 'NONE', #24441, #611, #9619, .T. ) ;
#55350 = ORIENTED_EDGE ( 'NONE', *, *, #25166, .T. ) ;
#55351 = CARTESIAN_POINT ( 'NONE',  ( -15.50000000000000000, -0.2000000000000000111, 19.20000000000052509 ) ) ;
#55352 = CARTESIAN_POINT ( 'NONE',  ( 78.77321854994620765, 47.95351654967443977, 20.00000000000000000 ) ) ;
#55353 = VECTOR ( 'NONE', #20331, 999.9999999999998863 ) ;
#55354 = DIRECTION ( 'NONE',  ( -1.000000000000000000, 0.000000000000000000, 0.000000000000000000 ) ) ;
#55355 = DIRECTION ( 'NONE',  ( -9.973078850062113474E-15, -1.000000000000000000, 0.000000000000000000 ) ) ;
#55356 = VECTOR ( 'NONE', #1601, 1000.000000000000114 ) ;
#55357 = ORIENTED_EDGE ( 'NONE', *, *, #49293, .F. ) ;
#55358 = DIRECTION ( 'NONE',  ( -1.000000000000000000, 0.000000000000000000, 0.000000000000000000 ) ) ;
#55359 = LINE ( 'NONE', #12887, #453 ) ;
#55360 = DIRECTION ( 'NONE',  ( -1.000000000000000000, 0.000000000000000000, -0.000000000000000000 ) ) ;
#55361 = AXIS2_PLACEMENT_3D ( 'NONE', #8732, #13680, #61772 ) ;
#55362 = CARTESIAN_POINT ( 'NONE',  ( 282.7711612342632179, -20.61060115624107780, -17.11060115624107425 ) ) ;
#55363 = CARTESIAN_POINT ( 'NONE',  ( 7.000000000000000000, -31.30000000000095284, 12.19999999999906315 ) ) ;
#55364 = VERTEX_POINT ( 'NONE', #31193 ) ;
#55365 = DIRECTION ( 'NONE',  ( 1.000000000000000000, -5.981805089575194965E-17, 0.000000000000000000 ) ) ;
#55366 = DIRECTION ( 'NONE',  ( -0.000000000000000000, -0.000000000000000000, -1.000000000000000000 ) ) ;
#55367 = LINE ( 'NONE', #11176, #57113 ) ;
#55368 = VECTOR ( 'NONE', #15889, 1000.000000000000000 ) ;
#55369 = CARTESIAN_POINT ( 'NONE',  ( -11.00000000000000000, -5.599999999999999645, 9.400000000000000355 ) ) ;
#55370 = LINE ( 'NONE', #44733, #21548 ) ;
#55371 = AXIS2_PLACEMENT_3D ( 'NONE', #62347, #19225, #13916 ) ;
#55372 = EDGE_CURVE ( 'NONE', #38597, #37495, #58915, .T. ) ;
#55373 = ORIENTED_EDGE ( 'NONE', *, *, #12831, .F. ) ;
#55374 = VERTEX_POINT ( 'NONE', #36123 ) ;
#55375 = EDGE_CURVE ( 'NONE', #527, #23385, #57693, .T. ) ;
#55376 = CARTESIAN_POINT ( 'NONE',  ( -7.172176262117278434, -5.257023737882785319, 54.00000000000000711 ) ) ;
#55377 = CARTESIAN_POINT ( 'NONE',  ( -6.350872789121327244, 3.663616288756986084, 54.00000000000000711 ) ) ;
#55378 = ORIENTED_EDGE ( 'NONE', *, *, #52465, .T. ) ;
#55379 = VECTOR ( 'NONE', #66799, 1000.000000000000000 ) ;
#55380 = AXIS2_PLACEMENT_3D ( 'NONE', #54702, #27477, #65656 ) ;
#55381 = DIRECTION ( 'NONE',  ( -1.836970198721029934E-16, 1.836970198721036590E-16, -1.000000000000000000 ) ) ;
#55382 = VERTEX_POINT ( 'NONE', #69353 ) ;
#55383 = LINE ( 'NONE', #5557, #62783 ) ;
#55384 = ORIENTED_EDGE ( 'NONE', *, *, #63152, .T. ) ;
#55385 = VERTEX_POINT ( 'NONE', #64749 ) ;
#55386 = CARTESIAN_POINT ( 'NONE',  ( 158.8349105750994568, -33.83962462487175316, 0.000000000000000000 ) ) ;
#55387 = CARTESIAN_POINT ( 'NONE',  ( 9.562023737882812569, -8.144523737882824577, 54.00000000000000711 ) ) ;
#55388 = DIRECTION ( 'NONE',  ( 0.000000000000000000, 0.000000000000000000, 1.000000000000000000 ) ) ;
#55389 = PLANE ( 'NONE',  #65229 ) ;
#55390 = AXIS2_PLACEMENT_3D ( 'NONE', #43576, #39892, #37938 ) ;
#55391 = ORIENTED_EDGE ( 'NONE', *, *, #26573, .F. ) ;
#55392 = ORIENTED_EDGE ( 'NONE', *, *, #63085, .T. ) ;
#55393 = CARTESIAN_POINT ( 'NONE',  ( 0.5000000000000000000, 21.00000000000000000, -18.00000000000000355 ) ) ;
#55394 = CARTESIAN_POINT ( 'NONE',  ( 8.900000000000002132, 18.00000000000000355, 21.00000000000000000 ) ) ;
#55395 = ORIENTED_EDGE ( 'NONE', *, *, #9797, .F. ) ;
#55396 = ORIENTED_EDGE ( 'NONE', *, *, #45673, .T. ) ;
#55397 = ORIENTED_EDGE ( 'NONE', *, *, #12375, .F. ) ;
#55398 = AXIS2_PLACEMENT_3D ( 'NONE', #64057, #43158, #53096 ) ;
#55399 = DIRECTION ( 'NONE',  ( 0.000000000000000000, 0.000000000000000000, 1.000000000000000000 ) ) ;
#55400 = DIRECTION ( 'NONE',  ( -0.6414496315691645689, -0.7671651518152939886, -2.587583378555115478E-16 ) ) ;
#55401 = AXIS2_PLACEMENT_3D ( 'NONE', #17665, #60440, #27933 ) ;
#55403 = ORIENTED_EDGE ( 'NONE', *, *, #30303, .T. ) ;
#55402 = CARTESIAN_POINT ( 'NONE',  ( -1.677516549646676625, 10.73351654964656987, 455.0000000000000568 ) ) ;
#55404 = EDGE_CURVE ( 'NONE', #24235, #55546, #36849, .T. ) ;
#55405 = CARTESIAN_POINT ( 'NONE',  ( 290.0000000000000000, -21.00000000000000000, 5.000000000000000000 ) ) ;
#55406 = AXIS2_PLACEMENT_3D ( 'NONE', #31302, #31642, #63812 ) ;
#55407 = DIRECTION ( 'NONE',  ( 0.000000000000000000, 0.000000000000000000, -1.000000000000000000 ) ) ;
#55408 = ORIENTED_EDGE ( 'NONE', *, *, #53948, .F. ) ;
#55410 = EDGE_CURVE ( 'NONE', #5119, #37252, #53803, .T. ) ;
#55409 = CIRCLE ( 'NONE', #2303, 5.000000000000000000 ) ;
#55411 = ORIENTED_EDGE ( 'NONE', *, *, #41242, .F. ) ;
#55412 = ADVANCED_FACE ( 'NONE', ( #398 ), #31886, .T. ) ;
#55413 = ADVANCED_FACE ( 'NONE', ( #58754 ), #48844, .F. ) ;
#55414 = AXIS2_PLACEMENT_3D ( 'NONE', #63815, #57800, #52150 ) ;
#55415 = FACE_OUTER_BOUND ( 'NONE', #24079, .T. ) ;
#55416 = CARTESIAN_POINT ( 'NONE',  ( 7.250000000000005329, 7.250000000000000888, -25.50000000000000355 ) ) ;
#55417 = EDGE_CURVE ( 'NONE', #5044, #8876, #42127, .T. ) ;
#55418 = ADVANCED_FACE ( 'NONE', ( #31540 ), #21624, .F. ) ;
#55419 = CARTESIAN_POINT ( 'NONE',  ( 10.47821035407137025, -20.81978353999701170, -17.31978353999701170 ) ) ;
#55420 = EDGE_CURVE ( 'NONE', #3957, #20305, #48145, .T. ) ;
#55421 = CARTESIAN_POINT ( 'NONE',  ( -23.75054448485400016, -15.50000000000000000, 25.53140320652400064 ) ) ;
#55422 = CARTESIAN_POINT ( 'NONE',  ( 9.106483450353415776, 10.08346604330773744, 455.0000000000000568 ) ) ;
#55424 = VERTEX_POINT ( 'NONE', #10651 ) ;
#55423 = SURFACE_STYLE_FILL_AREA ( #6282 ) ;
#55425 = VERTEX_POINT ( 'NONE', #5006 ) ;
#55426 = CARTESIAN_POINT ( 'NONE',  ( -6.350872789121377870, -6.836383711242978833, 54.00000000000000711 ) ) ;
#55427 = AXIS2_PLACEMENT_3D ( 'NONE', #16906, #21858, #299 ) ;
#55428 = LINE ( 'NONE', #61049, #30771 ) ;
#55429 = DIRECTION ( 'NONE',  ( 0.000000000000000000, -3.673940397442059868E-16, 1.000000000000000000 ) ) ;
#55430 = DIRECTION ( 'NONE',  ( 0.000000000000000000, 3.673940397442059868E-16, -1.000000000000000000 ) ) ;
#55431 = CARTESIAN_POINT ( 'NONE',  ( 0.2499999999999893141, -0.2499999999999893141, -26.75000000000001421 ) ) ;
#55432 = ORIENTED_EDGE ( 'NONE', *, *, #36210, .T. ) ;
#55433 = DIRECTION ( 'NONE',  ( -1.000000000000000000, 0.000000000000000000, 0.000000000000000000 ) ) ;
#55434 = DIRECTION ( 'NONE',  ( 7.304098846218132892E-15, 1.000000000000000000, 3.673940397442059868E-16 ) ) ;
#55435 = CARTESIAN_POINT ( 'NONE',  ( 19.90000000000000213, -0.1999999999911430404, -8.864436962241481021E-12 ) ) ;
#55436 = CARTESIAN_POINT ( 'NONE',  ( -25.50000000000000355, -15.50000000000000000, 22.50000000000000000 ) ) ;
#55437 = AXIS2_PLACEMENT_3D ( 'NONE', #21837, #6949, #38459 ) ;
#55438 = DIRECTION ( 'NONE',  ( 1.062171939662868407E-14, 1.000000000000000000, 0.000000000000000000 ) ) ;
#55439 = CARTESIAN_POINT ( 'NONE',  ( 8.689999999999999503, -9.750000000000001776, -7.000000000000000000 ) ) ;
#55440 = DIRECTION ( 'NONE',  ( 0.000000000000000000, -1.000000000000000000, -6.036837696397607468E-13 ) ) ;
#55441 = ORIENTED_EDGE ( 'NONE', *, *, #62221, .F. ) ;
#55442 = DIRECTION ( 'NONE',  ( 0.6414496315691367023, -0.7671651518153173033, -2.309356642089295169E-17 ) ) ;
#55443 = LINE ( 'NONE', #32833, #63390 ) ;
#55444 = ORIENTED_EDGE ( 'NONE', *, *, #41811, .F. ) ;
#55445 = CARTESIAN_POINT ( 'NONE',  ( -5.993516549646711766, 5.993516549646603409, 455.0000000000000568 ) ) ;
#55446 = CARTESIAN_POINT ( 'NONE',  ( -23.75054448485400016, -15.50000000000000000, 25.53140320652400064 ) ) ;
#55447 = DIRECTION ( 'NONE',  ( 1.836970198721029934E-16, 1.836970198721010706E-16, -1.000000000000000000 ) ) ;
#55448 = DIRECTION ( 'NONE',  ( 0.000000000000000000, 0.000000000000000000, -1.000000000000000000 ) ) ;
#55449 = CARTESIAN_POINT ( 'NONE',  ( 8.750000000000005329, -7.249999999999997335, -30.00000000000001066 ) ) ;
#55450 = AXIS2_PLACEMENT_3D ( 'NONE', #25064, #14095, #35653 ) ;
#55451 = EDGE_LOOP ( 'NONE', ( #6849, #35642, #39738, #58805 ) ) ;
#55452 = LINE ( 'NONE', #27888, #9291 ) ;
#55453 = EDGE_CURVE ( 'NONE', #49797, #36712, #26225, .T. ) ;
#55454 = AXIS2_PLACEMENT_3D ( 'NONE', #62620, #62986, #41056 ) ;
#55455 = ORIENTED_EDGE ( 'NONE', *, *, #33888, .T. ) ;
#55456 = CARTESIAN_POINT ( 'NONE',  ( 283.0000000000000568, -32.94999999999885176, -8.199999999997979572 ) ) ;
#55457 = EDGE_LOOP ( 'NONE', ( #43905, #468, #49616, #48047 ) ) ;
#55458 = EDGE_CURVE ( 'NONE', #56196, #11718, #21957, .T. ) ;
#55459 = AXIS2_PLACEMENT_3D ( 'NONE', #22993, #28298, #39930 ) ;
#55460 = PLANE ( 'NONE',  #34796 ) ;
#55461 = ADVANCED_FACE ( 'NONE', ( #16306 ), #21279, .F. ) ;
#55462 = EDGE_CURVE ( 'NONE', #19358, #57153, #32226, .T. ) ;
#55463 = CIRCLE ( 'NONE', #35102, 1.399999999999998579 ) ;
#55464 = DIRECTION ( 'NONE',  ( 0.000000000000000000, 0.000000000000000000, 1.000000000000000000 ) ) ;
#55465 = DIRECTION ( 'NONE',  ( -1.000000000000000000, 0.000000000000000000, 0.000000000000000000 ) ) ;
#55466 = ORIENTED_EDGE ( 'NONE', *, *, #5792, .T. ) ;
#55467 = VERTEX_POINT ( 'NONE', #15270 ) ;
#55468 = CARTESIAN_POINT ( 'NONE',  ( 283.0000000000000568, -31.30000000000045191, -8.900000000000430234 ) ) ;
#55469 = ORIENTED_EDGE ( 'NONE', *, *, #345, .T. ) ;
#55470 = CIRCLE ( 'NONE', #19315, 1.224999999999998757 ) ;
#55471 = ORIENTED_EDGE ( 'NONE', *, *, #12040, .F. ) ;
#55472 = CARTESIAN_POINT ( 'NONE',  ( 7.357023737882797398, 5.538810540049960984, 26.00000000000000711 ) ) ;
#55473 = DIRECTION ( 'NONE',  ( -0.000000000000000000, -0.000000000000000000, -1.000000000000000000 ) ) ;
#55474 = DIRECTION ( 'NONE',  ( 1.000000000000000000, -0.000000000000000000, 0.000000000000000000 ) ) ;
#55475 = VECTOR ( 'NONE', #52295, 1000.000000000000000 ) ;
#55476 = EDGE_LOOP ( 'NONE', ( #28164, #7161, #43363, #25785 ) ) ;
#55477 = PLANE ( 'NONE',  #36869 ) ;
#55478 = VECTOR ( 'NONE', #40817, 1000.000000000000000 ) ;
#55480 = CARTESIAN_POINT ( 'NONE',  ( -8.697938382363135545, 8.079219948824830411, 54.00000000000000711 ) ) ;
#55479 = DIRECTION ( 'NONE',  ( -1.836970198721029934E-16, 1.836970198721036590E-16, -1.000000000000000000 ) ) ;
#55481 = ORIENTED_EDGE ( 'NONE', *, *, #43594, .T. ) ;
#55483 = ORIENTED_EDGE ( 'NONE', *, *, #66136, .F. ) ;
#55482 = DIRECTION ( 'NONE',  ( -1.836970198721029934E-16, 1.836970198721036344E-16, -1.000000000000000000 ) ) ;
#55484 = EDGE_LOOP ( 'NONE', ( #69336, #48973, #978, #42617 ) ) ;
#55485 = CARTESIAN_POINT ( 'NONE',  ( -3.142976262117251451, 6.486996718459839606, 54.00000000000000711 ) ) ;
#55486 = VERTEX_POINT ( 'NONE', #5375 ) ;
#55487 = EDGE_CURVE ( 'NONE', #28850, #3957, #27326, .T. ) ;
#55488 = LINE ( 'NONE', #65746, #48357 ) ;
#55489 = VECTOR ( 'NONE', #26029, 1000.000000000000000 ) ;
#55490 = ORIENTED_EDGE ( 'NONE', *, *, #13448, .T. ) ;
#55491 = ORIENTED_EDGE ( 'NONE', *, *, #30598, .T. ) ;
#55492 = DIRECTION ( 'NONE',  ( -0.000000000000000000, 3.673940397442059868E-16, -1.000000000000000000 ) ) ;
#55493 = CARTESIAN_POINT ( 'NONE',  ( 7.357023737882792069, 4.947141984184419528, 26.00000000000000711 ) ) ;
#55494 = ORIENTED_EDGE ( 'NONE', *, *, #53805, .T. ) ;
#55495 = DIRECTION ( 'NONE',  ( -4.268512490100335178E-15, -1.000000000000000000, 0.000000000000000000 ) ) ;
#55496 = DIRECTION ( 'NONE',  ( -1.000000000000000000, 0.000000000000000000, 0.000000000000000000 ) ) ;
#55497 = EDGE_CURVE ( 'NONE', #22621, #46607, #11340, .T. ) ;
#55498 = CARTESIAN_POINT ( 'NONE',  ( -7.450000000000001954, -7.249999999999998224, -14.00000000000000000 ) ) ;
#55499 = EDGE_CURVE ( 'NONE', #20779, #15964, #43519, .T. ) ;
#55500 = AXIS2_PLACEMENT_3D ( 'NONE', #41852, #36549, #57061 ) ;
#55501 = ORIENTED_EDGE ( 'NONE', *, *, #5575, .F. ) ;
#55502 = EDGE_CURVE ( 'NONE', #38480, #10983, #58658, .T. ) ;
#55503 = CYLINDRICAL_SURFACE ( 'NONE', #5307, 0.5000000000009406920 ) ;
#55504 = CARTESIAN_POINT ( 'NONE',  ( 41.09999999999999432, -21.00000000000000000, 13.86939075806900057 ) ) ;
#55506 = ORIENTED_EDGE ( 'NONE', *, *, #37945, .T. ) ;
#55505 = LINE ( 'NONE', #17314, #69086 ) ;
#55508 = ORIENTED_EDGE ( 'NONE', *, *, #51754, .T. ) ;
#55507 = DIRECTION ( 'NONE',  ( 0.7671651518153006499, 0.6414496315691565753, 0.000000000000000000 ) ) ;
#55509 = PLANE ( 'NONE',  #44905 ) ;
#55510 = CYLINDRICAL_SURFACE ( 'NONE', #67968, 1.000000000000001776 ) ;
#55511 = DIRECTION ( 'NONE',  ( -1.000000000000000000, 0.000000000000000000, 0.000000000000000000 ) ) ;
#55512 = VECTOR ( 'NONE', #32601, 1000.000000000000000 ) ;
#55513 = CLOSED_SHELL ( 'NONE', ( #35854, #60717, #24937, #45102, #46698, #40465, #38997, #57922, #39214, #65176, #8075, #42743, #37745, #33897, #4018, #27986, #9883, #26630, #6812, #28146, #61498, #25790, #27167, #65600, #8640, #31646, #18184, #52388, #39944, #43058, #52029, #35763, #53769, #55703, #47, #50207, #41239, #23387, #38733, #40149, #46656, #66360, #62659, #22694, #40319, #47056, #22816, #3318, #20346, #29735, #11738, #69556, #65611, #67384, #66118, #49650, #65160, #33391, #25969, #39192, #52739, #28764, #28143, #41770, #43833, #27408, #33936, #39671, #54006, #6168, #1297, #58560, #29775, #21916, #21192, #21604, #43883, #55595, #40894, #58105, #27716, #37693, #11122, #42227, #24556, #66836, #63962, #56192, #1976, #153, #50252, #36501, #57033, #13344, #49671, #45826, #38337, #119, #67411, #45490, #58822, #32288, #57694, #25022, #61328, #16938, #11164, #25660, #54999, #55170, #4751, #24359, #68436, #41706, #35109, #19380, #33086, #32119, #44311, #48915, #51430, #30395, #19962, #14528, #53676, #44026, #58461, #675, #21677, #49160, #64708, #44458, #64190, #18959, #39990, #24450, #43485, #36055, #29896, #16389, #8626, #61360, #15518, #2422, #32115, #5701, #22407, #32643, #1034, #49519, #12210, #51842, #64223, #7224, #62165, #23395, #28549, #42306, #69841, #25700, #59958, #43909, #63192, #59331, #58135, #37020, #50952, #67457, #50531, #59822, #54728, #8475, #57402, #45500, #28425, #30393, #56763, #39888, #52706, #41417, #66961, #29413, #46705, #45354, #11728, #51855, #45835, #25905, #8479, #50831, #50871, #44009, #23737, #56078, #50552, #17220, #49871, #51009, #14635, #10950, #11305, #62219, #48078, #63601, #9535, #3851, #44276, #280, #36259, #43682, #27761, #56615, #237, #69638, #33191, #61951, #1622, #39984, #5046, #62349, #17363, #55116, #17420, #22377, #8308, #22475, #16547, #26294, #62795, #18900, #29453, #45775, #37485, #32808, #31258, #19697, #47059, #26806, #7896, #48868, #33551, #35212, #27101, #20452, #14979, #41186, #20160, #52931, #4369, #15605, #18606, #17880, #2983, #6874, #64238, #3860, #50997, #24999, #10517, #39515, #59725, #26104, #22267, #63482, #53627, #10165, #17586, #62605, #68923, #28490, #64292, #69157, #68661, #67405, #12136, #17583, #20716, #15232, #590, #12750, #1305, #3447, #25176, #67712, #17821, #6057, #63095, #68526, #55588, #2329, #69716, #22614, #8877, #11195, #36975, #36668, #2895, #56154, #13285, #15941, #17370, #47523, #21652, #20630, #5786, #33686, #63087, #59064, #68827, #29258, #38421, #19257, #11854, #41377, #8559, #6418, #27237, #6080, #67692, #5738, #13535, #40008, #31118, #33649, #69355, #31947, #24271, #44611, #21085, #62683, #62886, #11257, #6268, #38013, #67247, #45323, #3087, #31909, #17452, #61051, #59578, #3035, #46827, #4300, #9516, #44443, #43934, #29687, #28050, #17069, #36097, #47205, #42840, #40248, #66187, #58293, #40724, #46577, #21770, #6419, #19075, #37397, #3796, #35893, #24635, #40492, #4745, #3618, #28499, #1691, #48880, #58732 ) ) ;
#55514 = FACE_OUTER_BOUND ( 'NONE', #30689, .T. ) ;
#55515 = CARTESIAN_POINT ( 'NONE',  ( 11.12648345035337982, -7.806483450353490561, 455.0000000000000568 ) ) ;
#55516 = ORIENTED_EDGE ( 'NONE', *, *, #16320, .T. ) ;
#55517 = DIRECTION ( 'NONE',  ( -1.000000000000000000, 0.000000000000000000, 0.000000000000000000 ) ) ;
#55518 = DIRECTION ( 'NONE',  ( -1.000000000000000000, 0.000000000000000000, 0.000000000000000000 ) ) ;
#55519 = DIRECTION ( 'NONE',  ( 1.836970198721029934E-16, 1.836970198721010706E-16, -1.000000000000000000 ) ) ;
#55521 = ORIENTED_EDGE ( 'NONE', *, *, #66172, .T. ) ;
#55520 = DIRECTION ( 'NONE',  ( 0.000000000000000000, 0.000000000000000000, -1.000000000000000000 ) ) ;
#55522 = LINE ( 'NONE', #67164, #58393 ) ;
#55523 = DIRECTION ( 'NONE',  ( 0.000000000000000000, 1.000000000000000000, 0.000000000000000000 ) ) ;
#55524 = AXIS2_PLACEMENT_3D ( 'NONE', #51613, #40988, #19427 ) ;
#55525 = ORIENTED_EDGE ( 'NONE', *, *, #44329, .T. ) ;
#55526 = DIRECTION ( 'NONE',  ( 1.836970198721029934E-16, -1.836970198721036344E-16, 1.000000000000000000 ) ) ;
#55527 = CARTESIAN_POINT ( 'NONE',  ( -10.19191654964685156, -9.804883450353383267, 455.0000000000000568 ) ) ;
#55528 = ORIENTED_EDGE ( 'NONE', *, *, #49592, .T. ) ;
#55529 = DIRECTION ( 'NONE',  ( 1.000000000000000000, -0.000000000000000000, -0.000000000000000000 ) ) ;
#55530 = CARTESIAN_POINT ( 'NONE',  ( -9.689726262117227762, 8.916576262117214213, 54.00000000000000711 ) ) ;
#55531 = CARTESIAN_POINT ( 'NONE',  ( 15.50000000000000000, -0.2000000000000000111, 22.50000000000000000 ) ) ;
#55532 = DIRECTION ( 'NONE',  ( 0.000000000000000000, 0.000000000000000000, 1.000000000000000000 ) ) ;
#55533 = DIRECTION ( 'NONE',  ( 0.000000000000000000, -1.000000000000000000, -3.673940397442059868E-16 ) ) ;
#55534 = ORIENTED_EDGE ( 'NONE', *, *, #44717, .T. ) ;
#55535 = VECTOR ( 'NONE', #52013, 1000.000000000000000 ) ;
#55536 = DIRECTION ( 'NONE',  ( 1.836970198721029934E-16, 1.836970198721010706E-16, -1.000000000000000000 ) ) ;
#55537 = ORIENTED_EDGE ( 'NONE', *, *, #19809, .T. ) ;
#55538 = ORIENTED_EDGE ( 'NONE', *, *, #4428, .T. ) ;
#55539 = EDGE_CURVE ( 'NONE', #53942, #43565, #69007, .T. ) ;
#55540 = DIRECTION ( 'NONE',  ( 0.000000000000000000, 1.000000000000000000, 0.000000000000000000 ) ) ;
#55541 = DIRECTION ( 'NONE',  ( 1.000000000000000000, -0.000000000000000000, 0.000000000000000000 ) ) ;
#55542 = EDGE_CURVE ( 'NONE', #21874, #7139, #61151, .T. ) ;
#55543 = PRESENTATION_STYLE_ASSIGNMENT (( #12383 ) ) ;
#55544 = DIRECTION ( 'NONE',  ( -1.000000000000000000, 3.491481338843133355E-15, 0.000000000000000000 ) ) ;
#55545 = VERTEX_POINT ( 'NONE', #45238 ) ;
#55546 = VERTEX_POINT ( 'NONE', #27609 ) ;
#55547 = AXIS2_PLACEMENT_3D ( 'NONE', #33921, #49850, #28624 ) ;
#55548 = CARTESIAN_POINT ( 'NONE',  ( 15.00000000000000000, -42.00000000000000000, 15.10000000000000142 ) ) ;
#55549 = ORIENTED_EDGE ( 'NONE', *, *, #15636, .T. ) ;
#55550 = PRODUCT_DEFINITION_SHAPE ( 'NONE', 'NONE',  #9788 ) ;
#55551 = DIRECTION ( 'NONE',  ( -1.000000000000000000, 0.000000000000000000, 0.000000000000000000 ) ) ;
#55552 = CARTESIAN_POINT ( 'NONE',  ( 283.0000000000000568, -30.80000000000000071, 12.20000000000000107 ) ) ;
#55553 = CARTESIAN_POINT ( 'NONE',  ( 7.000000000000000000, -38.64999999999999858, -12.69999999999999929 ) ) ;
#55554 =( NAMED_UNIT ( * ) SI_UNIT ( $, .STERADIAN. ) SOLID_ANGLE_UNIT ( ) );
#55556 = DIRECTION ( 'NONE',  ( -1.000000000000000000, 0.000000000000000000, 0.000000000000000000 ) ) ;
#55555 = DIRECTION ( 'NONE',  ( 0.000000000000000000, -1.000000000000000000, 0.000000000000000000 ) ) ;
#55557 = ORIENTED_EDGE ( 'NONE', *, *, #41007, .F. ) ;
#55559 = ORIENTED_EDGE ( 'NONE', *, *, #54593, .F. ) ;
#55558 = CARTESIAN_POINT ( 'NONE',  ( -15.50000000000000000, -5.000000000000000000, -19.00000000000000000 ) ) ;
#55560 = ORIENTED_EDGE ( 'NONE', *, *, #25933, .F. ) ;
#55561 = VERTEX_POINT ( 'NONE', #65445 ) ;
#55562 = AXIS2_PLACEMENT_3D ( 'NONE', #40845, #13276, #29535 ) ;
#55563 = AXIS2_PLACEMENT_3D ( 'NONE', #43103, #4598, #32513 ) ;
#55564 = EDGE_CURVE ( 'NONE', #17797, #1336, #2463, .T. ) ;
#55565 = DIRECTION ( 'NONE',  ( 1.000000000000000000, 0.000000000000000000, 0.000000000000000000 ) ) ;
#55566 = VECTOR ( 'NONE', #27549, 1000.000000000000000 ) ;
#55567 =( BOUNDED_CURVE ( )  B_SPLINE_CURVE ( 3, ( #9156, #52288, #27073, #21769 ),
 .UNSPECIFIED., .F., .F. ) 
 B_SPLINE_CURVE_WITH_KNOTS ( ( 4, 4 ),
 ( 3.864326901403209558, 3.989654732571277229 ),
 .UNSPECIFIED. ) 
 CURVE ( )  GEOMETRIC_REPRESENTATION_ITEM ( )  RATIONAL_B_SPLINE_CURVE ( ( 1.000000000000000000, 0.9986915061577686936, 0.9986915061577686936, 1.000000000000000000 ) ) 
 REPRESENTATION_ITEM ( '' )  );
#55568 = CARTESIAN_POINT ( 'NONE',  ( 283.0000000000000568, -25.50000000000000355, -17.00000000000000000 ) ) ;
#55569 = CARTESIAN_POINT ( 'NONE',  ( -1.466476262117230034, 9.390476262117152473, 54.00000000000000711 ) ) ;
#55570 = EDGE_LOOP ( 'NONE', ( #3394, #28309, #30214, #63056 ) ) ;
#55571 = ORIENTED_EDGE ( 'NONE', *, *, #56131, .T. ) ;
#55572 = AXIS2_PLACEMENT_3D ( 'NONE', #21871, #59009, #69968 ) ;
#55573 = FACE_OUTER_BOUND ( 'NONE', #54682, .T. ) ;
#55574 = LINE ( 'NONE', #18076, #10842 ) ;
#55575 = ORIENTED_EDGE ( 'NONE', *, *, #18507, .F. ) ;
#55576 = VERTEX_POINT ( 'NONE', #22321 ) ;
#55577 = CARTESIAN_POINT ( 'NONE',  ( 8.250000000000005329, -8.249999999999998224, -26.00000000000001066 ) ) ;
#55578 = CARTESIAN_POINT ( 'NONE',  ( -11.00000000000000000, -11.50000000000082068, -10.20500000000000007 ) ) ;
#55579 = VERTEX_POINT ( 'NONE', #1422 ) ;
#55580 = ADVANCED_FACE ( 'NONE', ( #6723 ), #18364, .T. ) ;
#55581 = EDGE_CURVE ( 'NONE', #41772, #61464, #41998, .T. ) ;
#55582 = DIRECTION ( 'NONE',  ( -0.000000000000000000, -0.000000000000000000, 1.000000000000000000 ) ) ;
#55583 = EDGE_CURVE ( 'NONE', #9544, #31253, #33605, .T. ) ;
#55584 = ORIENTED_EDGE ( 'NONE', *, *, #19483, .F. ) ;
#55585 = VERTEX_POINT ( 'NONE', #1093 ) ;
#55586 = DIRECTION ( 'NONE',  ( 1.000000000000000000, 0.000000000000000000, 0.000000000000000000 ) ) ;
#55587 = DIRECTION ( 'NONE',  ( -1.000000000000000000, 0.000000000000000000, 0.000000000000000000 ) ) ;
#55588 = ADVANCED_FACE ( 'NONE', ( #28294 ), #39253, .F. ) ;
#55589 = CARTESIAN_POINT ( 'NONE',  ( -25.50000000000000355, -5.200000000000001066, 22.50000000000000000 ) ) ;
#55590 = CIRCLE ( 'NONE', #25108, 1.620999999999997332 ) ;
#55591 = LINE ( 'NONE', #69857, #39449 ) ;
#55592 = CARTESIAN_POINT ( 'NONE',  ( 1.480523737882816881, 9.390476262117212869, 54.00000000000000711 ) ) ;
#55593 = EDGE_CURVE ( 'NONE', #22970, #63961, #60063, .T. ) ;
#55594 = DIRECTION ( 'NONE',  ( -1.000000000000000000, 0.000000000000000000, 0.000000000000000000 ) ) ;
#55595 = ADVANCED_FACE ( 'NONE', ( #12357 ), #33937, .T. ) ;
#55596 = EDGE_CURVE ( 'NONE', #38683, #54169, #8107, .T. ) ;
#55597 = VERTEX_POINT ( 'NONE', #22654 ) ;
#55598 = CARTESIAN_POINT ( 'NONE',  ( -11.47551654964667733, 11.07551654964660237, 455.0000000000000568 ) ) ;
#55599 = EDGE_CURVE ( 'NONE', #53330, #28620, #6952, .T. ) ;
#55601 = EDGE_LOOP ( 'NONE', ( #54981, #51700, #27030, #31397 ) ) ;
#55600 = PLANE ( 'NONE',  #43469 ) ;
#55602 = LINE ( 'NONE', #17774, #42292 ) ;
#55603 = CARTESIAN_POINT ( 'NONE',  ( 7.357023737882792069, 4.947141984184419528, 26.00000000000000711 ) ) ;
#55604 = CARTESIAN_POINT ( 'NONE',  ( 28.00000000000000000, -17.50000000000000000, -20.05051025721700242 ) ) ;
#55605 = DIRECTION ( 'NONE',  ( 0.000000000000000000, 0.000000000000000000, 1.000000000000000000 ) ) ;
#55606 = CARTESIAN_POINT ( 'NONE',  ( 30.00000000000000000, -17.00000000000000000, -15.70499999999969809 ) ) ;
#55607 = ORIENTED_EDGE ( 'NONE', *, *, #30709, .T. ) ;
#55608 = ORIENTED_EDGE ( 'NONE', *, *, #47923, .F. ) ;
#55609 = DIRECTION ( 'NONE',  ( 0.000000000000000000, 0.000000000000000000, 1.000000000000000000 ) ) ;
#55610 = CARTESIAN_POINT ( 'NONE',  ( 9.106483450353380249, -11.12648345035348640, 455.0000000000000568 ) ) ;
#55611 = LINE ( 'NONE', #1871, #61251 ) ;
#55612 = AXIS2_PLACEMENT_3D ( 'NONE', #22430, #65226, #58875 ) ;
#55613 = VERTEX_POINT ( 'NONE', #1769 ) ;
#55614 = DIRECTION ( 'NONE',  ( 1.000000000000000000, 0.000000000000000000, 0.000000000000000000 ) ) ;
#55615 = ORIENTED_EDGE ( 'NONE', *, *, #50694, .F. ) ;
#55616 = VERTEX_POINT ( 'NONE', #11678 ) ;
#55617 = AXIS2_PLACEMENT_3D ( 'NONE', #60988, #54666, #23167 ) ;
#55618 = LINE ( 'NONE', #17095, #21151 ) ;
#55619 = LINE ( 'NONE', #60913, #55638 ) ;
#55620 = ORIENTED_EDGE ( 'NONE', *, *, #12947, .T. ) ;
#55621 = DIRECTION ( 'NONE',  ( 0.7671651518153105309, 0.6414496315691445849, 2.356647714346206145E-16 ) ) ;
#55622 = AXIS2_PLACEMENT_3D ( 'NONE', #13167, #30139, #61593 ) ;
#55623 = DIRECTION ( 'NONE',  ( -1.000000000000000000, 0.000000000000000000, 0.000000000000000000 ) ) ;
#55624 = AXIS2_PLACEMENT_3D ( 'NONE', #37439, #10557, #26478 ) ;
#55625 = DIRECTION ( 'NONE',  ( -1.000000000000000000, 0.000000000000000000, 0.000000000000000000 ) ) ;
#55626 = VERTEX_POINT ( 'NONE', #23342 ) ;
#55628 = ORIENTED_EDGE ( 'NONE', *, *, #57121, .F. ) ;
#55627 = DIRECTION ( 'NONE',  ( 0.000000000000000000, 0.000000000000000000, 1.000000000000000000 ) ) ;
#55629 = DIRECTION ( 'NONE',  ( -4.336808689942043768E-15, -1.000000000000000000, 0.000000000000000000 ) ) ;
#55630 = VECTOR ( 'NONE', #61555, 1000.000000000000000 ) ;
#55631 = CYLINDRICAL_SURFACE ( 'NONE', #64405, 0.1999999999999987899 ) ;
#55632 = CARTESIAN_POINT ( 'NONE',  ( 7.250000000000005329, 8.250000000000001776, -22.50000000000000000 ) ) ;
#55633 = DIRECTION ( 'NONE',  ( -0.000000000000000000, -0.000000000000000000, -1.000000000000000000 ) ) ;
#55634 = ORIENTED_EDGE ( 'NONE', *, *, #57260, .T. ) ;
#55635 = CARTESIAN_POINT ( 'NONE',  ( -15.50000000000000000, -5.000000000000000000, 22.50000000000000000 ) ) ;
#55636 = EDGE_CURVE ( 'NONE', #67039, #65777, #44204, .T. ) ;
#55637 = CARTESIAN_POINT ( 'NONE',  ( -2.693516549646827851, -10.92648345035345692, 455.0000000000000568 ) ) ;
#55638 = VECTOR ( 'NONE', #55283, 1000.000000000000000 ) ;
#55639 = ORIENTED_EDGE ( 'NONE', *, *, #25097, .T. ) ;
#55640 = ORIENTED_EDGE ( 'NONE', *, *, #9308, .F. ) ;
#55641 = ORIENTED_EDGE ( 'NONE', *, *, #41838, .T. ) ;
#55642 = EDGE_CURVE ( 'NONE', #22061, #39495, #39709, .T. ) ;
#55643 = DIRECTION ( 'NONE',  ( 1.000000000000000000, 0.000000000000000000, -0.000000000000000000 ) ) ;
#55644 = VECTOR ( 'NONE', #21778, 1000.000000000000000 ) ;
#55645 = CARTESIAN_POINT ( 'NONE',  ( 25.50000000000000355, -5.200000000000001066, 24.75000000000000000 ) ) ;
#55646 = DIRECTION ( 'NONE',  ( 1.000000000000000000, -0.000000000000000000, -0.000000000000000000 ) ) ;
#55647 = VERTEX_POINT ( 'NONE', #17335 ) ;
#55649 = EDGE_CURVE ( 'NONE', #62514, #54442, #39587, .T. ) ;
#55648 = ORIENTED_EDGE ( 'NONE', *, *, #33808, .F. ) ;
#55650 = ORIENTED_EDGE ( 'NONE', *, *, #65325, .T. ) ;
#55651 = DIRECTION ( 'NONE',  ( -0.000000000000000000, -0.000000000000000000, 1.000000000000000000 ) ) ;
#55652 = ORIENTED_EDGE ( 'NONE', *, *, #29787, .F. ) ;
#55653 = ORIENTED_EDGE ( 'NONE', *, *, #35500, .F. ) ;
#55654 = EDGE_CURVE ( 'NONE', #10277, #16237, #34276, .T. ) ;
#55655 = ORIENTED_EDGE ( 'NONE', *, *, #43547, .T. ) ;
#55656 = ORIENTED_EDGE ( 'NONE', *, *, #54001, .F. ) ;
#55657 = B_SPLINE_CURVE_WITH_KNOTS ( 'NONE', 3,
 ( #33325, #54905, #6458, #6779 ),
 .UNSPECIFIED., .F., .F.,
 ( 4, 4 ),
 ( 0.0009978974790779693294, 0.7140570275647658560 ),
 .UNSPECIFIED. ) ;
#55658 = DIRECTION ( 'NONE',  ( 0.000000000000000000, 1.000000000000000000, 0.000000000000000000 ) ) ;
#55660 = ORIENTED_EDGE ( 'NONE', *, *, #28102, .F. ) ;
#55659 = CARTESIAN_POINT ( 'NONE',  ( 41.09999999999999432, -14.06939075806900163, 20.80000000000000426 ) ) ;
#55661 = DIRECTION ( 'NONE',  ( -0.000000000000000000, -0.000000000000000000, -1.000000000000000000 ) ) ;
#55663 = CARTESIAN_POINT ( 'NONE',  ( 78.77321854994620765, 47.95351654967443977, 0.000000000000000000 ) ) ;
#55662 = AXIS2_PLACEMENT_3D ( 'NONE', #18143, #24154, #39708 ) ;
#55664 = ADVANCED_FACE ( 'NONE', ( #55863 ), #7414, .F. ) ;
#55665 = DIRECTION ( 'NONE',  ( 0.000000000000000000, -0.000000000000000000, 1.000000000000000000 ) ) ;
#55667 = ORIENTED_EDGE ( 'NONE', *, *, #50383, .T. ) ;
#55666 = DIRECTION ( 'NONE',  ( 1.000000000000000000, -3.016910393003147986E-15, 0.000000000000000000 ) ) ;
#55668 = VECTOR ( 'NONE', #19779, 1000.000000000000000 ) ;
#55669 = CIRCLE ( 'NONE', #64714, 4.000000000000000888 ) ;
#55670 = DIRECTION ( 'NONE',  ( 1.836970198721029934E-16, -1.836970198721036344E-16, 1.000000000000000000 ) ) ;
#55671 = DIRECTION ( 'NONE',  ( 1.836970198721029934E-16, 1.836970198721010706E-16, -1.000000000000000000 ) ) ;
#55672 = CARTESIAN_POINT ( 'NONE',  ( 30.00000000000000000, -5.200000000000001066, 9.400000000000000355 ) ) ;
#55673 = VECTOR ( 'NONE', #34531, 1000.000000000000000 ) ;
#55674 = EDGE_CURVE ( 'NONE', #24680, #19296, #37472, .T. ) ;
#55675 = ORIENTED_EDGE ( 'NONE', *, *, #66489, .F. ) ;
#55676 = FACE_OUTER_BOUND ( 'NONE', #44607, .T. ) ;
#55677 = ADVANCED_FACE ( 'NONE', ( #68579 ), #30039, .F. ) ;
#55678 = CARTESIAN_POINT ( 'NONE',  ( -8.916576262117258622, 10.03972626211718477, 54.00000000000000711 ) ) ;
#55679 = AXIS2_PLACEMENT_3D ( 'NONE', #32887, #65419, #55495 ) ;
#55680 = LINE ( 'NONE', #62369, #31192 ) ;
#55681 = ORIENTED_EDGE ( 'NONE', *, *, #11737, .F. ) ;
#55682 = CARTESIAN_POINT ( 'NONE',  ( -8.821682069070780230, 7.955476262117183062, 54.00000000000000711 ) ) ;
#55683 = LINE ( 'NONE', #1943, #29640 ) ;
#55684 = CARTESIAN_POINT ( 'NONE',  ( -11.00000000000000000, -15.46862696659690073, 14.50000000000000000 ) ) ;
#55685 = VECTOR ( 'NONE', #4424, 1000.000000000000000 ) ;
#55686 = VERTEX_POINT ( 'NONE', #40294 ) ;
#55687 = DIRECTION ( 'NONE',  ( 0.000000000000000000, 0.2142857142857145514, 0.9767710236555243730 ) ) ;
#55688 = PLANE ( 'NONE',  #59902 ) ;
#55689 = VECTOR ( 'NONE', #14450, 1000.000000000000000 ) ;
#55690 = CARTESIAN_POINT ( 'NONE',  ( 7.250000000000005329, -7.249999999999998224, -19.50000000000000000 ) ) ;
#55691 = CYLINDRICAL_SURFACE ( 'NONE', #25542, 1.000000000000000000 ) ;
#55692 = VERTEX_POINT ( 'NONE', #7764 ) ;
#55693 = CARTESIAN_POINT ( 'NONE',  ( 12.00648345035338060, -4.186483450353492231, 455.0000000000000568 ) ) ;
#55694 = DIRECTION ( 'NONE',  ( 0.000000000000000000, 0.000000000000000000, -1.000000000000000000 ) ) ;
#55695 = DIRECTION ( 'NONE',  ( 0.000000000000000000, 1.000000000000000000, 0.000000000000000000 ) ) ;
#55696 = CIRCLE ( 'NONE', #4890, 5.000000000000004441 ) ;
#55697 = LINE ( 'NONE', #65618, #1906 ) ;
#55698 = CARTESIAN_POINT ( 'NONE',  ( -10.08346604330797369, -9.106483450353383802, 455.0000000000000568 ) ) ;
#55699 = ORIENTED_EDGE ( 'NONE', *, *, #49695, .F. ) ;
#55700 = PLANE ( 'NONE',  #38905 ) ;
#55701 = DIRECTION ( 'NONE',  ( -0.000000000000000000, 0.000000000000000000, 1.000000000000000000 ) ) ;
#55702 = CARTESIAN_POINT ( 'NONE',  ( -11.99351654964679526, -7.826483450353362237, 455.0000000000000568 ) ) ;
#55703 = ADVANCED_FACE ( 'NONE', ( #63270 ), #20133, .T. ) ;
#55704 = DIRECTION ( 'NONE',  ( 1.000000000000000000, 0.000000000000000000, 0.000000000000000000 ) ) ;
#55705 = CARTESIAN_POINT ( 'NONE',  ( 7.450000000000003730, -7.249999999999997335, -7.500000000000000000 ) ) ;
#55706 = ORIENTED_EDGE ( 'NONE', *, *, #47160, .F. ) ;
#55707 = VERTEX_POINT ( 'NONE', #35682 ) ;
#55708 = EDGE_CURVE ( 'NONE', #15805, #35336, #52312, .T. ) ;
#55709 = CIRCLE ( 'NONE', #51210, 1.000000000000000000 ) ;
#55710 = CIRCLE ( 'NONE', #46677, 24.99999999998789946 ) ;
#55711 = CARTESIAN_POINT ( 'NONE',  ( -3.142976262117267883, -4.046023737882828542, 54.00000000000000711 ) ) ;
#55712 = DIRECTION ( 'NONE',  ( 1.000000000000000000, -0.000000000000000000, -0.000000000000000000 ) ) ;
#55713 = ORIENTED_EDGE ( 'NONE', *, *, #53709, .T. ) ;
#55714 = ADVANCED_FACE ( 'NONE', ( #13425 ), #68219, .F. ) ;
#55715 = CIRCLE ( 'NONE', #2617, 0.4000000000000010214 ) ;
#55716 = AXIS2_PLACEMENT_3D ( 'NONE', #36956, #25990, #69114 ) ;
#55717 = FACE_OUTER_BOUND ( 'NONE', #21926, .T. ) ;
#55718 = TOROIDAL_SURFACE ( 'NONE', #41028, 5.000000000000003553, 1.000000000000000000 ) ;
#55719 = EDGE_CURVE ( 'NONE', #38741, #57915, #2462, .T. ) ;
#55720 = ORIENTED_EDGE ( 'NONE', *, *, #61731, .T. ) ;
#55721 = CARTESIAN_POINT ( 'NONE',  ( 7.357023737882806280, 6.651770455163672935, 54.00000000000000711 ) ) ;
#55723 = ORIENTED_EDGE ( 'NONE', *, *, #11685, .F. ) ;
#55722 = COLOUR_RGB ( '', 0.72549020, 0.75294118, 0.79215686) ;
#55724 = AXIS2_PLACEMENT_3D ( 'NONE', #39639, #7812, #2172 ) ;
#55725 = EDGE_CURVE ( 'NONE', #17940, #2806, #41695, .T. ) ;
#55726 = VERTEX_POINT ( 'NONE', #34980 ) ;
#55727 = CARTESIAN_POINT ( 'NONE',  ( 7.250000000000005329, -7.449999999999998401, -13.00000000000000178 ) ) ;
#55728 = CARTESIAN_POINT ( 'NONE',  ( -30.00000000000000000, -8.959999999999999076, -17.04524521594300523 ) ) ;
#55729 = CARTESIAN_POINT ( 'NONE',  ( -2.893516549646830249, -11.12648345035345621, 455.0000000000000568 ) ) ;
#55730 = DIRECTION ( 'NONE',  ( 0.7071067811865550112, 0.7071067811865401342, 2.597868168706466299E-16 ) ) ;
#55731 = ORIENTED_EDGE ( 'NONE', *, *, #2084, .F. ) ;
#55732 = EDGE_CURVE ( 'NONE', #69020, #61169, #45589, .T. ) ;
#55733 = EDGE_LOOP ( 'NONE', ( #25359, #22551, #55914, #57545 ) ) ;
#55734 = DIRECTION ( 'NONE',  ( 0.000000000000000000, 0.000000000000000000, -1.000000000000000000 ) ) ;
#55735 = ADVANCED_FACE ( 'NONE', ( #67165 ), #35320, .F. ) ;
#55736 = DIRECTION ( 'NONE',  ( -1.000000000000000000, 0.000000000000000000, 0.000000000000000000 ) ) ;
#55737 = VERTEX_POINT ( 'NONE', #3523 ) ;
#55738 = EDGE_LOOP ( 'NONE', ( #25313, #4077, #60754, #49019, #56755, #28807 ) ) ;
#55739 = EDGE_CURVE ( 'NONE', #2965, #35460, #36341, .T. ) ;
#55740 = EDGE_CURVE ( 'NONE', #42432, #60403, #40644, .T. ) ;
#55741 = VERTEX_POINT ( 'NONE', #29677 ) ;
#55742 = DIRECTION ( 'NONE',  ( -1.000000000000000000, 0.000000000000000000, 0.000000000000000000 ) ) ;
#55744 = ORIENTED_EDGE ( 'NONE', *, *, #3518, .F. ) ;
#55743 = DIRECTION ( 'NONE',  ( 0.000000000000000000, -1.000000000000000000, 0.000000000000000000 ) ) ;
#55745 = EDGE_CURVE ( 'NONE', #12180, #42535, #46647, .T. ) ;
#55746 = CARTESIAN_POINT ( 'NONE',  ( -5.538810540050023157, 7.342976262117183239, 54.00000000000000711 ) ) ;
#55747 = LINE ( 'NONE', #16885, #12516 ) ;
#55748 = VERTEX_POINT ( 'NONE', #19079 ) ;
#55749 = ORIENTED_EDGE ( 'NONE', *, *, #14152, .T. ) ;
#55750 = DIRECTION ( 'NONE',  ( 0.000000000000000000, 0.000000000000000000, 1.000000000000000000 ) ) ;
#55751 = CARTESIAN_POINT ( 'NONE',  ( -5.993516549646776603, -6.006483450353426790, 455.0000000000000568 ) ) ;
#55752 = ADVANCED_FACE ( 'NONE', ( #56896, #13771, #3177 ), #14485, .T. ) ;
#55753 = LINE ( 'NONE', #28867, #68800 ) ;
#55754 = ADVANCED_FACE ( 'NONE', ( #36040 ), #57611, .F. ) ;
#55755 = VECTOR ( 'NONE', #25303, 1000.000000000000000 ) ;
#55756 = FACE_OUTER_BOUND ( 'NONE', #15908, .T. ) ;
#55757 = DIRECTION ( 'NONE',  ( 0.000000000000000000, 1.000000000000000000, 0.000000000000000000 ) ) ;
#55759 = EDGE_LOOP ( 'NONE', ( #44178, #18500, #886, #33351 ) ) ;
#55758 = SURFACE_SIDE_STYLE ('',( #55423 ) ) ;
#55760 = ORIENTED_EDGE ( 'NONE', *, *, #10008, .F. ) ;
#55761 = DIRECTION ( 'NONE',  ( 0.000000000000000000, 1.000000000000000000, 0.000000000000000000 ) ) ;
#55762 = VECTOR ( 'NONE', #17101, 1000.000000000000000 ) ;
#55764 = AXIS2_PLACEMENT_3D ( 'NONE', #45222, #61478, #35662 ) ;
#55763 = DIRECTION ( 'NONE',  ( 0.000000000000000000, -1.000000000000000000, 0.000000000000000000 ) ) ;
#55765 = FACE_OUTER_BOUND ( 'NONE', #68000, .T. ) ;
#55766 = DIRECTION ( 'NONE',  ( 1.000000000000000000, 0.000000000000000000, 0.000000000000000000 ) ) ;
#55767 = VECTOR ( 'NONE', #9648, 1000.000000000000000 ) ;
#55768 = VECTOR ( 'NONE', #51712, 1000.000000000000000 ) ;
#55769 = DIRECTION ( 'NONE',  ( -0.000000000000000000, -0.000000000000000000, 1.000000000000000000 ) ) ;
#55770 = ORIENTED_EDGE ( 'NONE', *, *, #54391, .F. ) ;
#55771 = LINE ( 'NONE', #33513, #51620 ) ;
#55772 = DIRECTION ( 'NONE',  ( 0.000000000000000000, 0.000000000000000000, 1.000000000000000000 ) ) ;
#55773 = DIRECTION ( 'NONE',  ( 0.000000000000000000, -0.7046037717859445770, 0.7096009616573392131 ) ) ;
#55774 = LINE ( 'NONE', #6974, #22056 ) ;
#55775 = CARTESIAN_POINT ( 'NONE',  ( 49.00000000000000000, -0.2000000000089119934, -8.913009219568841313E-12 ) ) ;
#55776 = LINE ( 'NONE', #33853, #8163 ) ;
#55777 = AXIS2_PLACEMENT_3D ( 'NONE', #19543, #9298, #20948 ) ;
#55778 = CARTESIAN_POINT ( 'NONE',  ( 29.50000000000000355, -12.00000000000000000, -11.03137303340310282 ) ) ;
#55779 = ORIENTED_EDGE ( 'NONE', *, *, #10655, .T. ) ;
#55780 = CARTESIAN_POINT ( 'NONE',  ( 39.00000000000000000, -16.96999999999999886, 21.00000000000000000 ) ) ;
#55781 = DIRECTION ( 'NONE',  ( -0.000000000000000000, -0.000000000000000000, -1.000000000000000000 ) ) ;
#55782 = ORIENTED_EDGE ( 'NONE', *, *, #33375, .T. ) ;
#55783 = LINE ( 'NONE', #40209, #63922 ) ;
#55784 = DIRECTION ( 'NONE',  ( 1.000000000000000000, -0.000000000000000000, 0.000000000000000000 ) ) ;
#55785 = CARTESIAN_POINT ( 'NONE',  ( -10.19191654964671301, 10.19191654964664018, 455.0000000000000568 ) ) ;
#55786 = LINE ( 'NONE', #33530, #44348 ) ;
#55787 = CARTESIAN_POINT ( 'NONE',  ( -8.250000000000001776, -8.249999999999998224, -26.00000000000001066 ) ) ;
#55788 = VERTEX_POINT ( 'NONE', #32496 ) ;
#55789 = ADVANCED_FACE ( 'NONE', ( #65017, #10921 ), #52679, .F. ) ;
#55790 = LINE ( 'NONE', #18295, #67016 ) ;
#55791 = EDGE_LOOP ( 'NONE', ( #62068, #13220, #9453, #23369 ) ) ;
#55792 = LINE ( 'NONE', #51545, #68379 ) ;
#55793 = ORIENTED_EDGE ( 'NONE', *, *, #463, .T. ) ;
#55794 = AXIS2_PLACEMENT_3D ( 'NONE', #54944, #16759, #60220 ) ;
#55795 = EDGE_CURVE ( 'NONE', #26023, #43043, #58671, .T. ) ;
#55796 = DIRECTION ( 'NONE',  ( -1.000000000000000000, 6.308085367188448025E-15, 0.000000000000000000 ) ) ;
#55797 = EDGE_CURVE ( 'NONE', #19307, #14977, #47351, .T. ) ;
#55798 = AXIS2_PLACEMENT_3D ( 'NONE', #68933, #9538, #57269 ) ;
#55799 = EDGE_CURVE ( 'NONE', #20779, #24327, #47703, .T. ) ;
#55800 = CARTESIAN_POINT ( 'NONE',  ( -8.566576262117353124, -9.703773737882732675, 26.00000000000000000 ) ) ;
#55801 = PLANE ( 'NONE',  #68396 ) ;
#55802 = ORIENTED_EDGE ( 'NONE', *, *, #11639, .T. ) ;
#55803 = EDGE_CURVE ( 'NONE', #65821, #15450, #9527, .T. ) ;
#55804 = ORIENTED_EDGE ( 'NONE', *, *, #43537, .T. ) ;
#55805 = EDGE_CURVE ( 'NONE', #9113, #27438, #10454, .T. ) ;
#55806 = LINE ( 'NONE', #60755, #21709 ) ;
#55807 = EDGE_LOOP ( 'NONE', ( #49795, #7305, #19144, #11631 ) ) ;
#55808 = ORIENTED_EDGE ( 'NONE', *, *, #27451, .T. ) ;
#55809 = DIRECTION ( 'NONE',  ( -1.836970198721029934E-16, -1.836970198721010706E-16, 1.000000000000000000 ) ) ;
#55810 = DIRECTION ( 'NONE',  ( 0.8660254037844482555, 0.000000000000000000, 0.4999999999999831801 ) ) ;
#55811 = VECTOR ( 'NONE', #69190, 1000.000000000000000 ) ;
#55812 = AXIS2_PLACEMENT_3D ( 'NONE', #1815, #6766, #29375 ) ;
#55813 = DIRECTION ( 'NONE',  ( -0.000000000000000000, -0.000000000000000000, 1.000000000000000000 ) ) ;
#55814 = ORIENTED_EDGE ( 'NONE', *, *, #64453, .F. ) ;
#55815 = DIRECTION ( 'NONE',  ( 0.000000000000000000, 0.000000000000000000, 1.000000000000000000 ) ) ;
#55817 = CYLINDRICAL_SURFACE ( 'NONE', #62624, 0.1750000000000002387 ) ;
#55816 = FACE_OUTER_BOUND ( 'NONE', #9181, .T. ) ;
#55819 = ORIENTED_EDGE ( 'NONE', *, *, #50125, .F. ) ;
#55818 = AXIS2_PLACEMENT_3D ( 'NONE', #21699, #32654, #64490 ) ;
#55821 = ORIENTED_EDGE ( 'NONE', *, *, #29506, .T. ) ;
#55820 = CARTESIAN_POINT ( 'NONE',  ( 46.39999999999999858, 33.00000000000000000, -0.7500000000000000000 ) ) ;
#55822 = ORIENTED_EDGE ( 'NONE', *, *, #34361, .F. ) ;
#55823 = DIRECTION ( 'NONE',  ( 0.000000000000000000, 0.000000000000000000, 1.000000000000000000 ) ) ;
#55824 = VECTOR ( 'NONE', #67906, 1000.000000000000000 ) ;
#55825 = CARTESIAN_POINT ( 'NONE',  ( -7.813516549646711162, 11.77351654964660277, 195.0000000000000284 ) ) ;
#55826 = ORIENTED_EDGE ( 'NONE', *, *, #54722, .T. ) ;
#55827 = FACE_OUTER_BOUND ( 'NONE', #50163, .T. ) ;
#55828 = DIRECTION ( 'NONE',  ( 1.000000000000000000, -0.000000000000000000, -0.000000000000000000 ) ) ;
#55829 = VERTEX_POINT ( 'NONE', #310 ) ;
#55830 = ORIENTED_EDGE ( 'NONE', *, *, #21979, .T. ) ;
#55831 = CARTESIAN_POINT ( 'NONE',  ( 75.42576880091937142, 0.000000000000000000, 285.9830310981789125 ) ) ;
#55832 = DIRECTION ( 'NONE',  ( 0.000000000000000000, -1.000000000000000000, 0.000000000000000000 ) ) ;
#55833 = ORIENTED_EDGE ( 'NONE', *, *, #2811, .F. ) ;
#55834 = DIRECTION ( 'NONE',  ( 0.000000000000000000, -0.000000000000000000, 1.000000000000000000 ) ) ;
#55835 = CARTESIAN_POINT ( 'NONE',  ( 47.00000000000000000, 6.123233995736766282E-16, -5.000000000000000000 ) ) ;
#55836 = CARTESIAN_POINT ( 'NONE',  ( 17.89999999999999858, -0.1999999999911795112, 8.826273045769999343E-12 ) ) ;
#55837 = ORIENTED_EDGE ( 'NONE', *, *, #65570, .F. ) ;
#55838 = ADVANCED_FACE ( 'NONE', ( #31103 ), #32139, .F. ) ;
#55839 = CARTESIAN_POINT ( 'NONE',  ( 12.00648345035337883, -11.19368345035347900, 455.0000000000000568 ) ) ;
#55840 = CARTESIAN_POINT ( 'NONE',  ( -30.00000000000000000, -10.85999999999999943, 9.000000000000001776 ) ) ;
#55841 = VECTOR ( 'NONE', #13444, 1000.000000000000000 ) ;
#55844 = VERTEX_POINT ( 'NONE', #15186 ) ;
#55843 = ADVANCED_FACE ( 'NONE', ( #4237 ), #58329, .F. ) ;
#55842 = CARTESIAN_POINT ( 'NONE',  ( 7.408280051175138325, 3.710438382363051790, 54.00000000000000711 ) ) ;
#55846 = ORIENTED_EDGE ( 'NONE', *, *, #16410, .F. ) ;
#55845 = CARTESIAN_POINT ( 'NONE',  ( 29.50000000000000355, -11.50000000000000000, -15.00000000000000000 ) ) ;
#55847 = DIRECTION ( 'NONE',  ( 0.000000000000000000, 0.7071067811865474617, -0.7071067811865474617 ) ) ;
#55848 = DIRECTION ( 'NONE',  ( 0.000000000000000000, 1.000000000000000000, 0.000000000000000000 ) ) ;
#55849 = VECTOR ( 'NONE', #14409, 999.9999999999998863 ) ;
#55850 = LINE ( 'NONE', #36028, #44859 ) ;
#55851 = CARTESIAN_POINT ( 'NONE',  ( -7.605476262117258024, 9.722976262117178692, 25.99999580000000421 ) ) ;
#55852 = CARTESIAN_POINT ( 'NONE',  ( -6.651770455163739548, 7.517976262117183062, 26.00000000000000711 ) ) ;
#55853 = ORIENTED_EDGE ( 'NONE', *, *, #59283, .F. ) ;
#55854 = CARTESIAN_POINT ( 'NONE',  ( -7.250000000000001776, -7.249999999999998224, -10.50000000000000000 ) ) ;
#55855 = FACE_OUTER_BOUND ( 'NONE', #24641, .T. ) ;
#55856 = CARTESIAN_POINT ( 'NONE',  ( -9.897976262117293089, -6.832023737882757075, 54.00000000000000711 ) ) ;
#55858 = ORIENTED_EDGE ( 'NONE', *, *, #37854, .F. ) ;
#55857 = CARTESIAN_POINT ( 'NONE',  ( 275.0000000000000000, 0.000000000000000000, 0.000000000000000000 ) ) ;
#55859 = AXIS2_PLACEMENT_3D ( 'NONE', #2893, #41428, #24477 ) ;
#55860 = AXIS2_PLACEMENT_3D ( 'NONE', #14880, #47397, #36437 ) ;
#55861 = DIRECTION ( 'NONE',  ( 0.000000000000000000, 0.000000000000000000, 1.000000000000000000 ) ) ;
#55862 = ADVANCED_FACE ( 'NONE', ( #53026 ), #9889, .T. ) ;
#55863 = FACE_OUTER_BOUND ( 'NONE', #39739, .T. ) ;
#55864 = VECTOR ( 'NONE', #65040, 1000.000000000000000 ) ;
#55865 = VERTEX_POINT ( 'NONE', #42047 ) ;
#55866 = CARTESIAN_POINT ( 'NONE',  ( 49.00000000000000000, -0.1999999999911430404, -8.864436962241481021E-12 ) ) ;
#55867 = FACE_OUTER_BOUND ( 'NONE', #46061, .T. ) ;
#55868 = ORIENTED_EDGE ( 'NONE', *, *, #54874, .F. ) ;
#55869 = LINE ( 'NONE', #33273, #39102 ) ;
#55870 = LINE ( 'NONE', #24034, #59456 ) ;
#55871 = VECTOR ( 'NONE', #1903, 1000.000000000000000 ) ;
#55872 = LINE ( 'NONE', #33617, #53072 ) ;
#55873 = EDGE_CURVE ( 'NONE', #69741, #9508, #4581, .T. ) ;
#55874 = DIRECTION ( 'NONE',  ( -1.000000000000000000, 1.794541526872559352E-16, 0.000000000000000000 ) ) ;
#55875 = CIRCLE ( 'NONE', #23114, 0.5000000000001386669 ) ;
#55876 = EDGE_LOOP ( 'NONE', ( #60091, #17964, #66086, #33746 ) ) ;
#55877 = CARTESIAN_POINT ( 'NONE',  ( -1.077516549646825750, -10.74648345035347852, 455.0000000000000568 ) ) ;
#55878 = ORIENTED_EDGE ( 'NONE', *, *, #39294, .F. ) ;
#55879 = VERTEX_POINT ( 'NONE', #37451 ) ;
#55880 = PRESENTATION_LAYER_ASSIGNMENT (  '', '', ( #5126 ) ) ;
#55881 = CARTESIAN_POINT ( 'NONE',  ( -12.00000000000000000, -11.18999999999999950, -5.000000000000000000 ) ) ;
#55882 = EDGE_CURVE ( 'NONE', #43142, #20701, #16064, .T. ) ;
#55883 = EDGE_CURVE ( 'NONE', #63858, #49163, #53716, .T. ) ;
#55885 = CARTESIAN_POINT ( 'NONE',  ( 7.000000000000000000, -20.40000000000000213, 17.60000000000000142 ) ) ;
#55884 = CARTESIAN_POINT ( 'NONE',  ( -7.450000000000001954, 7.250000000000000000, -23.50000000000000000 ) ) ;
#55886 = VERTEX_POINT ( 'NONE', #42395 ) ;
#55887 = EDGE_CURVE ( 'NONE', #40613, #14714, #21527, .T. ) ;
#55888 = ORIENTED_EDGE ( 'NONE', *, *, #8156, .T. ) ;
#55889 = EDGE_CURVE ( 'NONE', #7056, #67901, #44300, .T. ) ;
#55890 = FACE_OUTER_BOUND ( 'NONE', #55123, .T. ) ;
#55891 = VECTOR ( 'NONE', #9782, 1000.000000000000000 ) ;
#55892 = ORIENTED_EDGE ( 'NONE', *, *, #8290, .T. ) ;
#55893 = CARTESIAN_POINT ( 'NONE',  ( 10.14575131106459160, -20.49999999999999645, -17.00000000000000000 ) ) ;
#55894 = CARTESIAN_POINT ( 'NONE',  ( 7.272650909786598561, -7.811466277050860718, 455.0000000000000568 ) ) ;
#55895 = EDGE_CURVE ( 'NONE', #8859, #68245, #43088, .T. ) ;
#55896 = DIRECTION ( 'NONE',  ( -0.000000000000000000, 3.673940397442059868E-16, -1.000000000000000000 ) ) ;
#55897 = CARTESIAN_POINT ( 'NONE',  ( 7.450000000000003730, -7.249999999999997335, -17.00000000000000000 ) ) ;
#55899 = CARTESIAN_POINT ( 'NONE',  ( 55.00000000000000000, 0.000000000000000000, 5.250000000000000000 ) ) ;
#55898 = DIRECTION ( 'NONE',  ( 1.000000000000000000, 0.000000000000000000, 0.000000000000000000 ) ) ;
#55900 = ORIENTED_EDGE ( 'NONE', *, *, #2864, .T. ) ;
#55902 = VERTEX_POINT ( 'NONE', #59357 ) ;
#55901 = CARTESIAN_POINT ( 'NONE',  ( 30.00000000000000000, -11.50000000000000000, 19.00000000000000000 ) ) ;
#55903 = VECTOR ( 'NONE', #68687, 1000.000000000000000 ) ;
#55904 = ORIENTED_EDGE ( 'NONE', *, *, #18023, .F. ) ;
#55905 = EDGE_LOOP ( 'NONE', ( #54446, #50306, #10759, #50273 ) ) ;
#55906 = LINE ( 'NONE', #66515, #29862 ) ;
#55907 = VECTOR ( 'NONE', #21405, 1000.000000000000000 ) ;
#55908 = VECTOR ( 'NONE', #41338, 1000.000000000000000 ) ;
#55910 = PLANE ( 'NONE',  #34922 ) ;
#55909 = AXIS2_PLACEMENT_3D ( 'NONE', #57750, #36176, #52457 ) ;
#55911 = AXIS2_PLACEMENT_3D ( 'NONE', #24067, #67912, #3564 ) ;
#55912 = DIRECTION ( 'NONE',  ( 3.614007241618349165E-15, 1.000000000000000000, 0.000000000000000000 ) ) ;
#55913 = ORIENTED_EDGE ( 'NONE', *, *, #9376, .T. ) ;
#55914 = ORIENTED_EDGE ( 'NONE', *, *, #420, .T. ) ;
#55915 = AXIS2_PLACEMENT_3D ( 'NONE', #42698, #4530, #58270 ) ;
#55916 = VECTOR ( 'NONE', #56332, 1000.000000000000000 ) ;
#55917 = FACE_OUTER_BOUND ( 'NONE', #69893, .T. ) ;
#55918 = CARTESIAN_POINT ( 'NONE',  ( 2.706483450353343478, -10.92648345035346225, 455.0000000000000568 ) ) ;
#55919 = VERTEX_POINT ( 'NONE', #5619 ) ;
#55920 = ORIENTED_EDGE ( 'NONE', *, *, #3298, .T. ) ;
#55921 = FACE_OUTER_BOUND ( 'NONE', #23439, .T. ) ;
#55922 = AXIS2_PLACEMENT_3D ( 'NONE', #46768, #69760, #63402 ) ;
#55923 = PLANE ( 'NONE',  #10840 ) ;
#55924 = ORIENTED_EDGE ( 'NONE', *, *, #47210, .F. ) ;
#55925 = VECTOR ( 'NONE', #46126, 1000.000000000000000 ) ;
#55926 = DIRECTION ( 'NONE',  ( 8.659560562354951347E-17, -0.7071067811865460184, 0.7071067811865489050 ) ) ;
#55929 = EDGE_LOOP ( 'NONE', ( #57960, #41494, #63008, #24790, #48623, #25798, #26951, #63052 ) ) ;
#55928 = ADVANCED_FACE ( 'NONE', ( #43429 ), #27371, .F. ) ;
#55927 = FACE_OUTER_BOUND ( 'NONE', #53958, .T. ) ;
#55930 = VECTOR ( 'NONE', #13853, 1000.000000000000000 ) ;
#55931 = ORIENTED_EDGE ( 'NONE', *, *, #53082, .T. ) ;
#55932 = EDGE_CURVE ( 'NONE', #40401, #10374, #7319, .T. ) ;
#55933 = CARTESIAN_POINT ( 'NONE',  ( -30.00000000000000000, -14.04000000000000092, -14.80000000000000071 ) ) ;
#55934 = CARTESIAN_POINT ( 'NONE',  ( 0.000000000000000000, -8.249999999999998224, -24.50000000000000000 ) ) ;
#55935 = DIRECTION ( 'NONE',  ( 0.000000000000000000, -0.9921567416492215186, 0.1249999999999996531 ) ) ;
#55936 = CARTESIAN_POINT ( 'NONE',  ( -28.00000000000000000, -15.50000000000000000, 20.05051025721700242 ) ) ;
#55937 = CARTESIAN_POINT ( 'NONE',  ( 41.09999999999999432, 20.60000000000000142, 13.86939075806900057 ) ) ;
#55938 = EDGE_CURVE ( 'NONE', #48072, #34099, #55776, .T. ) ;
#55939 = FACE_OUTER_BOUND ( 'NONE', #59646, .T. ) ;
#55940 = CARTESIAN_POINT ( 'NONE',  ( -9.404046420174067222, -1.866219381641389674, 195.0000000000000284 ) ) ;
#55941 = ORIENTED_EDGE ( 'NONE', *, *, #12348, .T. ) ;
#55942 = CARTESIAN_POINT ( 'NONE',  ( -7.250000000000000888, -8.249999999999998224, -11.00000000000000000 ) ) ;
#55944 = ORIENTED_EDGE ( 'NONE', *, *, #4214, .F. ) ;
#55943 = LINE ( 'NONE', #50637, #7306 ) ;
#55945 = CARTESIAN_POINT ( 'NONE',  ( 7.969523737882818537, -8.835729544836345539, 54.00000000000000711 ) ) ;
#55946 = PLANE ( 'NONE',  #13129 ) ;
#55947 = CARTESIAN_POINT ( 'NONE',  ( 0.4999999999999982792, -42.00000000000000000, -27.00000000000000000 ) ) ;
#55948 = DIRECTION ( 'NONE',  ( -1.000000000000000000, 0.000000000000000000, 0.000000000000000000 ) ) ;
#55949 = CARTESIAN_POINT ( 'NONE',  ( 34.89999999999999858, -0.1999999999911795112, 8.826273045769999343E-12 ) ) ;
#55950 = VECTOR ( 'NONE', #12293, 1000.000000000000000 ) ;
#55951 = ORIENTED_EDGE ( 'NONE', *, *, #31426, .F. ) ;
#55952 = EDGE_LOOP ( 'NONE', ( #42855, #8403, #64964, #16374, #32192, #62144, #34494, #45241, #11617, #54191, #55920, #43835, #57199, #53984, #53937, #60473, #46262 ) ) ;
#55953 = VECTOR ( 'NONE', #19342, 1000.000000000000114 ) ;
#55954 = PLANE ( 'NONE',  #58501 ) ;
#55955 = LINE ( 'NONE', #22740, #5121 ) ;
#55956 = AXIS2_PLACEMENT_3D ( 'NONE', #60620, #34781, #7904 ) ;
#55957 = CIRCLE ( 'NONE', #25491, 0.1749999999999998224 ) ;
#55958 = DIRECTION ( 'NONE',  ( -0.000000000000000000, 3.673940397442059868E-16, -1.000000000000000000 ) ) ;
#55959 = ORIENTED_EDGE ( 'NONE', *, *, #22789, .T. ) ;
#55960 = FACE_BOUND ( 'NONE', #22931, .T. ) ;
#55961 = ORIENTED_EDGE ( 'NONE', *, *, #30576, .T. ) ;
#55962 = ORIENTED_EDGE ( 'NONE', *, *, #16936, .T. ) ;
#55963 = CARTESIAN_POINT ( 'NONE',  ( -4.173516549646666185, 11.99351654964658920, 455.0000000000000568 ) ) ;
#55964 = DIRECTION ( 'NONE',  ( 1.000000000000000000, -5.981805089575194965E-17, 0.000000000000000000 ) ) ;
#55965 = VECTOR ( 'NONE', #2744, 1000.000000000000000 ) ;
#55966 = CIRCLE ( 'NONE', #32316, 7.999999999999998224 ) ;
#55967 = ORIENTED_EDGE ( 'NONE', *, *, #21821, .T. ) ;
#55968 = CARTESIAN_POINT ( 'NONE',  ( 11.00000000000000000, -11.70000000000000284, -12.50000000000000000 ) ) ;
#55969 = CIRCLE ( 'NONE', #22117, 0.7499999999999997780 ) ;
#55970 = CARTESIAN_POINT ( 'NONE',  ( 152.0064834503532722, 2.160375375128253950, 0.000000000000000000 ) ) ;
#55971 = CARTESIAN_POINT ( 'NONE',  ( 7.757955312929505354, 8.452095193409313367, 195.0000000000000284 ) ) ;
#55972 = ORIENTED_EDGE ( 'NONE', *, *, #49823, .F. ) ;
#55973 = VERTEX_POINT ( 'NONE', #11251 ) ;
#55975 = ORIENTED_EDGE ( 'NONE', *, *, #45013, .F. ) ;
#55974 = CARTESIAN_POINT ( 'NONE',  ( 8.250000000000005329, 0.000000000000000000, -18.00000000000000000 ) ) ;
#55976 = ADVANCED_FACE ( 'NONE', ( #33520 ), #38488, .F. ) ;
#55977 = ORIENTED_EDGE ( 'NONE', *, *, #51853, .T. ) ;
#55978 = AXIS2_PLACEMENT_3D ( 'NONE', #5627, #1020, #16587 ) ;
#55979 = DIRECTION ( 'NONE',  ( 1.836970198721029934E-16, -1.836970198721036344E-16, 1.000000000000000000 ) ) ;
#55980 = LINE ( 'NONE', #66928, #63677 ) ;
#55981 = EDGE_CURVE ( 'NONE', #1978, #4035, #17248, .T. ) ;
#55982 = CARTESIAN_POINT ( 'NONE',  ( 10.74648345035330443, 1.677516549646577371, 195.0000000000000284 ) ) ;
#55983 = DIRECTION ( 'NONE',  ( 0.000000000000000000, 0.000000000000000000, 1.000000000000000000 ) ) ;
#55984 = EDGE_CURVE ( 'NONE', #41462, #1475, #1674, .T. ) ;
#55985 = AXIS2_PLACEMENT_3D ( 'NONE', #55435, #17590, #23585 ) ;
#55986 = DIRECTION ( 'NONE',  ( 0.000000000000000000, 0.000000000000000000, 1.000000000000000000 ) ) ;
#55987 = CARTESIAN_POINT ( 'NONE',  ( 30.00000000000000000, -11.10796162543699950, -9.102987789146602893 ) ) ;
#55988 = ADVANCED_FACE ( 'NONE', ( #49450 ), #39171, .F. ) ;
#55989 = ORIENTED_EDGE ( 'NONE', *, *, #13035, .T. ) ;
#55990 = ORIENTED_EDGE ( 'NONE', *, *, #46302, .T. ) ;
#55991 = VERTEX_POINT ( 'NONE', #28892 ) ;
#55992 = DIRECTION ( 'NONE',  ( 0.000000000000000000, 0.000000000000000000, -1.000000000000000000 ) ) ;
#55993 = EDGE_CURVE ( 'NONE', #18999, #10507, #38154, .T. ) ;
#55994 = DIRECTION ( 'NONE',  ( 0.000000000000000000, -0.9921567416492215186, 0.1249999999999996531 ) ) ;
#55995 = EDGE_CURVE ( 'NONE', #63788, #28850, #22904, .T. ) ;
#55996 = LINE ( 'NONE', #66257, #14615 ) ;
#55997 =( LENGTH_UNIT ( ) NAMED_UNIT ( * ) SI_UNIT ( .MILLI., .METRE. ) );
#55998 = ORIENTED_EDGE ( 'NONE', *, *, #18434, .T. ) ;
#55999 = ORIENTED_EDGE ( 'NONE', *, *, #49754, .F. ) ;
#56000 = AXIS2_PLACEMENT_3D ( 'NONE', #58570, #10118, #25329 ) ;
#56001 = EDGE_LOOP ( 'NONE', ( #21544, #2588, #24315, #69944 ) ) ;
#56002 = CARTESIAN_POINT ( 'NONE',  ( 21.90000000000000213, 20.60000000000000142, -13.86939075806900057 ) ) ;
#56003 = VERTEX_POINT ( 'NONE', #12273 ) ;
#56004 = ORIENTED_EDGE ( 'NONE', *, *, #43284, .F. ) ;
#56005 = ORIENTED_EDGE ( 'NONE', *, *, #34029, .T. ) ;
#56006 = ORIENTED_EDGE ( 'NONE', *, *, #37315, .F. ) ;
#56007 = VECTOR ( 'NONE', #68414, 1000.000000000000000 ) ;
#56008 = CARTESIAN_POINT ( 'NONE',  ( 7.250000000000005329, 7.250000000000000888, -17.50000000000000000 ) ) ;
#56010 = ORIENTED_EDGE ( 'NONE', *, *, #31068, .F. ) ;
#56009 = DIRECTION ( 'NONE',  ( 0.000000000000000000, -1.000000000000000000, 0.000000000000000000 ) ) ;
#56011 = DIRECTION ( 'NONE',  ( 0.000000000000000000, -1.000000000000000000, 0.000000000000000000 ) ) ;
#56012 = VECTOR ( 'NONE', #2520, 1000.000000000000000 ) ;
#56013 = VECTOR ( 'NONE', #55019, 1000.000000000000000 ) ;
#56014 = AXIS2_PLACEMENT_3D ( 'NONE', #13738, #63235, #14805 ) ;
#56015 = DIRECTION ( 'NONE',  ( 0.000000000000000000, 0.000000000000000000, 1.000000000000000000 ) ) ;
#56016 = DIRECTION ( 'NONE',  ( 1.000000000000000000, 0.000000000000000000, 0.000000000000000000 ) ) ;
#56018 = ORIENTED_EDGE ( 'NONE', *, *, #20163, .F. ) ;
#56017 = DIRECTION ( 'NONE',  ( 0.000000000000000000, 0.000000000000000000, -1.000000000000000000 ) ) ;
#56019 = ORIENTED_EDGE ( 'NONE', *, *, #63931, .F. ) ;
#56020 = CIRCLE ( 'NONE', #69560, 0.3999999999999993006 ) ;
#56021 = VECTOR ( 'NONE', #66335, 1000.000000000000114 ) ;
#56022 = VECTOR ( 'NONE', #9835, 1000.000000000000000 ) ;
#56023 = DIRECTION ( 'NONE',  ( 3.717264591378874374E-15, 1.000000000000000000, 0.000000000000000000 ) ) ;
#56024 = CARTESIAN_POINT ( 'NONE',  ( -5.779227145995285753, -4.155633711806640207, 54.00000000000000711 ) ) ;
#56025 = EDGE_CURVE ( 'NONE', #17228, #61430, #57843, .T. ) ;
#56026 = FACE_OUTER_BOUND ( 'NONE', #7963, .T. ) ;
#56027 = CIRCLE ( 'NONE', #31219, 4.500000000000190958 ) ;
#56028 = VERTEX_POINT ( 'NONE', #1345 ) ;
#56029 = CARTESIAN_POINT ( 'NONE',  ( -6.835476262117260227, 10.49297626211718359, 54.00000000000000711 ) ) ;
#56030 = AXIS2_PLACEMENT_3D ( 'NONE', #20400, #68501, #25008 ) ;
#56031 = DIRECTION ( 'NONE',  ( -1.000000000000000000, 0.000000000000000000, 0.000000000000000000 ) ) ;
#56032 = DIRECTION ( 'NONE',  ( 0.000000000000000000, 0.000000000000000000, -1.000000000000000000 ) ) ;
#56033 = EDGE_LOOP ( 'NONE', ( #37633, #968, #15579, #20936 ) ) ;
#56034 = DIRECTION ( 'NONE',  ( -0.7071067811865500152, -0.7071067811865451302, 0.000000000000000000 ) ) ;
#56035 = EDGE_CURVE ( 'NONE', #2764, #62836, #2514, .T. ) ;
#56036 = DIRECTION ( 'NONE',  ( 1.000000000000000000, -0.000000000000000000, -0.000000000000000000 ) ) ;
#56037 = FACE_OUTER_BOUND ( 'NONE', #69571, .T. ) ;
#56038 = EDGE_LOOP ( 'NONE', ( #53740, #61735, #5764, #17350 ) ) ;
#56039 = EDGE_CURVE ( 'NONE', #56183, #15490, #39754, .T. ) ;
#56040 = DIRECTION ( 'NONE',  ( 1.000000000000000000, -0.000000000000000000, -0.000000000000000000 ) ) ;
#56041 = CARTESIAN_POINT ( 'NONE',  ( 36.90000000000000568, -14.06939075806900874, 20.80000000000001137 ) ) ;
#56042 = ORIENTED_EDGE ( 'NONE', *, *, #5917, .F. ) ;
#56043 = LINE ( 'NONE', #39764, #15759 ) ;
#56044 = LINE ( 'NONE', #12546, #54613 ) ;
#56045 = PLANE ( 'NONE',  #45458 ) ;
#56046 = CARTESIAN_POINT ( 'NONE',  ( 181.4833316329832940, 9.000000000000001776, 280.7801873289890295 ) ) ;
#56047 = LINE ( 'NONE', #62037, #37596 ) ;
#56048 = EDGE_LOOP ( 'NONE', ( #61092, #40777, #23474, #34483 ) ) ;
#56049 = DIRECTION ( 'NONE',  ( 0.000000000000000000, -1.000000000000000000, -0.000000000000000000 ) ) ;
#56050 = DIRECTION ( 'NONE',  ( 0.000000000000000000, 0.000000000000000000, -1.000000000000000000 ) ) ;
#56051 = EDGE_CURVE ( 'NONE', #32857, #278, #1013, .T. ) ;
#56052 = CARTESIAN_POINT ( 'NONE',  ( 25.50000000000000355, -15.50000000000000000, -20.49999999999999645 ) ) ;
#56053 = VECTOR ( 'NONE', #41335, 1000.000000000000000 ) ;
#56054 = AXIS2_PLACEMENT_3D ( 'NONE', #54473, #37859, #59426 ) ;
#56055 = DIRECTION ( 'NONE',  ( -0.7071067811865475727, 0.7071067811865475727, 2.597868168706480597E-16 ) ) ;
#56056 = CARTESIAN_POINT ( 'NONE',  ( 39.00000000000000000, 16.96999999999999886, -21.00000000000000000 ) ) ;
#56057 = VERTEX_POINT ( 'NONE', #55439 ) ;
#56059 = ORIENTED_EDGE ( 'NONE', *, *, #35073, .T. ) ;
#56058 = CARTESIAN_POINT ( 'NONE',  ( 15.50000000000000000, -0.2038245569916610489, -23.94337567297399971 ) ) ;
#56060 = CIRCLE ( 'NONE', #2967, 2.215251240775983899 ) ;
#56061 = AXIS2_PLACEMENT_3D ( 'NONE', #9858, #69241, #37766 ) ;
#56062 = PLANE ( 'NONE',  #23636 ) ;
#56063 = ADVANCED_FACE ( 'NONE', ( #6979 ), #28545, .F. ) ;
#56064 = CARTESIAN_POINT ( 'NONE',  ( 105.8309041053263257, 63.65740854044500452, 10.00000000000000000 ) ) ;
#56065 = ORIENTED_EDGE ( 'NONE', *, *, #25802, .F. ) ;
#56066 = VECTOR ( 'NONE', #68381, 1000.000000000000114 ) ;
#56067 = CIRCLE ( 'NONE', #53882, 0.5000000000009459100 ) ;
#56068 = CARTESIAN_POINT ( 'NONE',  ( 8.250000000000005329, -7.249999999999998224, -25.00000000000000000 ) ) ;
#56069 = EDGE_CURVE ( 'NONE', #5667, #62784, #59703, .T. ) ;
#56070 = EDGE_LOOP ( 'NONE', ( #2103, #50519, #68997, #68289 ) ) ;
#56071 = AXIS2_PLACEMENT_3D ( 'NONE', #20885, #54467, #46446 ) ;
#56072 = CARTESIAN_POINT ( 'NONE',  ( 169.1780563256071446, -35.83962462487175316, 5.000000000000000000 ) ) ;
#56073 = ORIENTED_EDGE ( 'NONE', *, *, #5862, .T. ) ;
#56074 = EDGE_LOOP ( 'NONE', ( #31333, #22328, #30563 ) ) ;
#56076 = EDGE_CURVE ( 'NONE', #27235, #27455, #12643, .T. ) ;
#56075 = FACE_OUTER_BOUND ( 'NONE', #47317, .T. ) ;
#56077 = CARTESIAN_POINT ( 'NONE',  ( -7.250000000000000000, -7.449999999999998401, -7.500000000000000000 ) ) ;
#56078 = ADVANCED_FACE ( 'NONE', ( #65364 ), #22570, .F. ) ;
#56079 = DIRECTION ( 'NONE',  ( -0.000000000000000000, -0.000000000000000000, -1.000000000000000000 ) ) ;
#56080 = DIRECTION ( 'NONE',  ( 0.000000000000000000, 1.000000000000000000, 0.000000000000000000 ) ) ;
#56081 = VECTOR ( 'NONE', #30108, 1000.000000000000000 ) ;
#56082 = ORIENTED_EDGE ( 'NONE', *, *, #59513, .T. ) ;
#56083 = ORIENTED_EDGE ( 'NONE', *, *, #23486, .F. ) ;
#56084 = DIRECTION ( 'NONE',  ( -0.000000000000000000, 1.000000000000000000, -0.000000000000000000 ) ) ;
#56085 = DIRECTION ( 'NONE',  ( -0.000000000000000000, -0.000000000000000000, -1.000000000000000000 ) ) ;
#56086 = VERTEX_POINT ( 'NONE', #52216 ) ;
#56087 = ORIENTED_EDGE ( 'NONE', *, *, #30931, .F. ) ;
#56088 = VERTEX_POINT ( 'NONE', #39840 ) ;
#56089 = CARTESIAN_POINT ( 'NONE',  ( 174.0064834503533575, -29.01119750012555443, 0.000000000000000000 ) ) ;
#56091 = EDGE_LOOP ( 'NONE', ( #69485, #56319, #9311, #33127 ) ) ;
#56090 = DIRECTION ( 'NONE',  ( -0.000000000000000000, -0.000000000000000000, -1.000000000000000000 ) ) ;
#56092 = DIRECTION ( 'NONE',  ( -1.836970198721029934E-16, 1.836970198721036590E-16, -1.000000000000000000 ) ) ;
#56093 = CARTESIAN_POINT ( 'NONE',  ( 11.50000000000000000, -11.50000000000000000, -11.00000000000000000 ) ) ;
#56094 = EDGE_CURVE ( 'NONE', #2486, #7598, #2380, .T. ) ;
#56095 = ORIENTED_EDGE ( 'NONE', *, *, #21775, .F. ) ;
#56096 = ORIENTED_EDGE ( 'NONE', *, *, #12876, .T. ) ;
#56097 = MECHANICAL_DESIGN_GEOMETRIC_PRESENTATION_REPRESENTATION (  '', ( #50445 ), #65162 ) ;
#56098 = EDGE_CURVE ( 'NONE', #8072, #32931, #62455, .T. ) ;
#56099 = DIRECTION ( 'NONE',  ( -0.000000000000000000, -0.000000000000000000, -1.000000000000000000 ) ) ;
#56100 = LINE ( 'NONE', #51140, #13217 ) ;
#56101 = VECTOR ( 'NONE', #51956, 1000.000000000000000 ) ;
#56102 = CIRCLE ( 'NONE', #57268, 0.3499999999999285905 ) ;
#56103 = CARTESIAN_POINT ( 'NONE',  ( -11.07551654964682086, -10.20488345035337296, 455.0000000000000568 ) ) ;
#56104 = EDGE_CURVE ( 'NONE', #21736, #5314, #18992, .T. ) ;
#56105 = AXIS2_PLACEMENT_3D ( 'NONE', #30655, #23350, #50907 ) ;
#56106 = CIRCLE ( 'NONE', #25695, 1.000000000000000000 ) ;
#56107 = DIRECTION ( 'NONE',  ( -1.836970198721029934E-16, 1.836970198721036590E-16, -1.000000000000000000 ) ) ;
#56108 = CARTESIAN_POINT ( 'NONE',  ( -7.250000000000000888, 7.250000000000001776, -9.500000000000001776 ) ) ;
#56110 = ORIENTED_EDGE ( 'NONE', *, *, #28509, .T. ) ;
#56109 = PLANE ( 'NONE',  #64774 ) ;
#56111 = VERTEX_POINT ( 'NONE', #23942 ) ;
#56112 = EDGE_CURVE ( 'NONE', #18830, #35523, #56812, .T. ) ;
#56113 = CARTESIAN_POINT ( 'NONE',  ( 3.157023737882809655, -6.501044194225480410, 54.00000000000000711 ) ) ;
#56114 = CIRCLE ( 'NONE', #67382, 0.1999999999999996503 ) ;
#56115 = VECTOR ( 'NONE', #11963, 1000.000000000000000 ) ;
#56116 = CARTESIAN_POINT ( 'NONE',  ( 8.144523737882817471, -9.562023737882817898, 54.00000000000000711 ) ) ;
#56117 = EDGE_CURVE ( 'NONE', #60377, #60100, #26260, .T. ) ;
#56118 = DIRECTION ( 'NONE',  ( -1.000000000000000000, 0.000000000000000000, 0.000000000000000000 ) ) ;
#56119 = AXIS2_PLACEMENT_3D ( 'NONE', #38791, #34165, #28523 ) ;
#56120 = EDGE_CURVE ( 'NONE', #44833, #24433, #53373, .T. ) ;
#56121 = DIRECTION ( 'NONE',  ( 1.836970198721029934E-16, 1.836970198721010706E-16, -1.000000000000000000 ) ) ;
#56122 = ORIENTED_EDGE ( 'NONE', *, *, #14652, .T. ) ;
#56123 = CARTESIAN_POINT ( 'NONE',  ( 10.20488345035338007, -11.48848345035339769, 195.0000000000000284 ) ) ;
#56124 = CARTESIAN_POINT ( 'NONE',  ( -7.250000000000001776, -7.249999999999998224, -11.50000000000000000 ) ) ;
#56125 = LINE ( 'NONE', #1669, #54897 ) ;
#56126 = CARTESIAN_POINT ( 'NONE',  ( 29.50000000000000355, -11.50000000000000000, -19.00000000000000000 ) ) ;
#56127 = PRODUCT_DEFINITION_SHAPE ( 'NONE', 'NONE',  #69991 ) ;
#56128 = VECTOR ( 'NONE', #12008, 1000.000000000000000 ) ;
#56129 = EDGE_CURVE ( 'NONE', #24615, #5610, #47704, .T. ) ;
#56130 = CARTESIAN_POINT ( 'NONE',  ( 4.186483450353376767, 11.99351654964663716, 195.0000000000000284 ) ) ;
#56131 = EDGE_CURVE ( 'NONE', #6538, #47930, #61408, .T. ) ;
#56132 = DIRECTION ( 'NONE',  ( -1.000000000000000000, 0.000000000000000000, 0.000000000000000000 ) ) ;
#56133 = ORIENTED_EDGE ( 'NONE', *, *, #49354, .T. ) ;
#56134 = CARTESIAN_POINT ( 'NONE',  ( 6.836383711243005479, -4.149127210878744698, 54.00000000000000711 ) ) ;
#56135 = DIRECTION ( 'NONE',  ( 1.000000000000000000, -0.000000000000000000, -0.000000000000000000 ) ) ;
#56136 = EDGE_CURVE ( 'NONE', #41307, #21951, #18632, .T. ) ;
#56137 = ORIENTED_EDGE ( 'NONE', *, *, #48642, .F. ) ;
#56138 = FACE_OUTER_BOUND ( 'NONE', #5452, .T. ) ;
#56139 = EDGE_CURVE ( 'NONE', #60418, #37432, #14030, .T. ) ;
#56140 = EDGE_CURVE ( 'NONE', #749, #66609, #50809, .T. ) ;
#56141 = DIRECTION ( 'NONE',  ( 0.7671651518152985405, 0.6414496315691592399, -2.309356642088639737E-17 ) ) ;
#56142 = CARTESIAN_POINT ( 'NONE',  ( -4.734785091273957747, 5.380658396643156038, 195.0000000000000284 ) ) ;
#56143 = DIRECTION ( 'NONE',  ( -1.000000000000000000, 0.000000000000000000, 0.000000000000000000 ) ) ;
#56144 = CARTESIAN_POINT ( 'NONE',  ( 24.00000000000000000, -17.35230188589299871, 15.35019951917099945 ) ) ;
#56145 = ORIENTED_EDGE ( 'NONE', *, *, #11909, .T. ) ;
#56146 = EDGE_CURVE ( 'NONE', #31391, #19920, #12968, .T. ) ;
#56147 = DIRECTION ( 'NONE',  ( 0.000000000000000000, 0.000000000000000000, -1.000000000000000000 ) ) ;
#56148 = VERTEX_POINT ( 'NONE', #56130 ) ;
#56149 = EDGE_CURVE ( 'NONE', #65251, #36248, #43208, .T. ) ;
#56150 = DIRECTION ( 'NONE',  ( 0.7071067811865446862, 0.7071067811865503483, 0.000000000000000000 ) ) ;
#56151 = AXIS2_PLACEMENT_3D ( 'NONE', #24211, #60373, #57083 ) ;
#56152 = ORIENTED_EDGE ( 'NONE', *, *, #9011, .F. ) ;
#56153 = DIRECTION ( 'NONE',  ( 0.000000000000000000, 0.000000000000000000, -1.000000000000000000 ) ) ;
#56154 = ADVANCED_FACE ( 'NONE', ( #3091 ), #30308, .F. ) ;
#56155 = CARTESIAN_POINT ( 'NONE',  ( 39.00000000000000000, 16.96999999999999886, 21.00000000000000000 ) ) ;
#56156 = AXIS2_PLACEMENT_3D ( 'NONE', #12256, #22549, #56445 ) ;
#56157 = CARTESIAN_POINT ( 'NONE',  ( 29.50000000000000355, -11.50000000000000000, -15.00000000000000000 ) ) ;
#56158 = ORIENTED_EDGE ( 'NONE', *, *, #10347, .T. ) ;
#56159 = ORIENTED_EDGE ( 'NONE', *, *, #61747, .F. ) ;
#56161 = ADVANCED_FACE ( 'NONE', ( #57519 ), #19335, .F. ) ;
#56160 = CARTESIAN_POINT ( 'NONE',  ( -17.24945551514599984, -17.50000000000000000, 25.53140320652400064 ) ) ;
#56162 = ORIENTED_EDGE ( 'NONE', *, *, #32864, .T. ) ;
#56163 = ORIENTED_EDGE ( 'NONE', *, *, #22703, .T. ) ;
#56164 = EDGE_CURVE ( 'NONE', #55385, #62302, #45861, .T. ) ;
#56165 = AXIS2_PLACEMENT_3D ( 'NONE', #15371, #59197, #43273 ) ;
#56166 = PLANE ( 'NONE',  #32698 ) ;
#56167 = CARTESIAN_POINT ( 'NONE',  ( 7.450000000000004619, -1.336933437520057563E-15, -8.000000000000000000 ) ) ;
#56168 = CARTESIAN_POINT ( 'NONE',  ( 25.49999999999869971, -17.50000000000000000, -22.50000000000000000 ) ) ;
#56169 = PRODUCT_DEFINITION_FORMATION_WITH_SPECIFIED_SOURCE ( 'ANY', '', #49892, .NOT_KNOWN. ) ;
#56170 = VERTEX_POINT ( 'NONE', #67445 ) ;
#56171 = DIRECTION ( 'NONE',  ( 1.000000000000000000, -0.000000000000000000, 0.000000000000000000 ) ) ;
#56173 = CARTESIAN_POINT ( 'NONE',  ( 0.000000000000000000, 0.000000000000000000, -7.000000000000000000 ) ) ;
#56172 = DIRECTION ( 'NONE',  ( 9.050731179009442381E-15, 1.000000000000000000, 0.000000000000000000 ) ) ;
#56174 = ORIENTED_EDGE ( 'NONE', *, *, #52923, .F. ) ;
#56176 = ORIENTED_EDGE ( 'NONE', *, *, #5620, .F. ) ;
#56175 = DIRECTION ( 'NONE',  ( -0.000000000000000000, -1.000000000000000000, 0.000000000000000000 ) ) ;
#56177 = ORIENTED_EDGE ( 'NONE', *, *, #57209, .T. ) ;
#56178 = CARTESIAN_POINT ( 'NONE',  ( 0.000000000000000000, 0.000000000000000000, 0.000000000000000000 ) ) ;
#56179 = DIRECTION ( 'NONE',  ( -0.000000000000000000, 1.000000000000000000, -0.000000000000000000 ) ) ;
#56180 = ORIENTED_EDGE ( 'NONE', *, *, #66361, .F. ) ;
#56181 = CARTESIAN_POINT ( 'NONE',  ( -11.77351654964679106, -7.606483450353366038, 455.0000000000000568 ) ) ;
#56182 = DIRECTION ( 'NONE',  ( 0.000000000000000000, 0.000000000000000000, 1.000000000000000000 ) ) ;
#56183 = VERTEX_POINT ( 'NONE', #67779 ) ;
#56184 = ORIENTED_EDGE ( 'NONE', *, *, #1572, .F. ) ;
#56185 = DIRECTION ( 'NONE',  ( -0.000000000000000000, -0.000000000000000000, -1.000000000000000000 ) ) ;
#56186 = DIRECTION ( 'NONE',  ( -1.000000000000000000, 0.000000000000000000, 0.000000000000000000 ) ) ;
#56187 = ORIENTED_EDGE ( 'NONE', *, *, #54409, .F. ) ;
#56188 = DIRECTION ( 'NONE',  ( 0.000000000000000000, 0.000000000000000000, -1.000000000000000000 ) ) ;
#56189 = FACE_OUTER_BOUND ( 'NONE', #65261, .T. ) ;
#56190 = DIRECTION ( 'NONE',  ( 0.000000000000000000, 0.000000000000000000, -1.000000000000000000 ) ) ;
#56191 = ORIENTED_EDGE ( 'NONE', *, *, #52239, .F. ) ;
#56192 = ADVANCED_FACE ( 'NONE', ( #3433 ), #9084, .T. ) ;
#56193 = CARTESIAN_POINT ( 'NONE',  ( -7.252248008019509307, -5.393625297349935011, 455.0000000000000568 ) ) ;
#56194 = VECTOR ( 'NONE', #37629, 1000.000000000000000 ) ;
#56196 = VERTEX_POINT ( 'NONE', #30653 ) ;
#56195 = CARTESIAN_POINT ( 'NONE',  ( 10.90000000000000036, -0.1999999999911795112, 8.826273045769999343E-12 ) ) ;
#56198 = ORIENTED_EDGE ( 'NONE', *, *, #5868, .T. ) ;
#56197 = CARTESIAN_POINT ( 'NONE',  ( -15.50000000000000000, -0.2038245569916614930, 21.05662432702600029 ) ) ;
#56199 = ADVANCED_FACE ( 'NONE', ( #53980 ), #10483, .T. ) ;
#56200 = LINE ( 'NONE', #2793, #55475 ) ;
#56201 = CARTESIAN_POINT ( 'NONE',  ( -7.250000000000001776, -7.249999999999998224, -26.00000000000001066 ) ) ;
#56202 = EDGE_CURVE ( 'NONE', #32122, #53390, #31717, .T. ) ;
#56203 = CARTESIAN_POINT ( 'NONE',  ( 9.703773737882785966, -8.930623737882855906, 54.00000000000000711 ) ) ;
#56204 = LINE ( 'NONE', #20470, #10265 ) ;
#56205 = AXIS2_PLACEMENT_3D ( 'NONE', #15158, #26463, #30718 ) ;
#56206 = EDGE_CURVE ( 'NONE', #57523, #17475, #26753, .T. ) ;
#56207 = DIRECTION ( 'NONE',  ( 1.836970198721029934E-16, 1.836970198721010706E-16, -1.000000000000000000 ) ) ;
#56208 = ORIENTED_EDGE ( 'NONE', *, *, #64318, .F. ) ;
#56209 = FACE_OUTER_BOUND ( 'NONE', #56001, .T. ) ;
#56210 = CARTESIAN_POINT ( 'NONE',  ( -30.00000000000000000, -17.50000000000000000, -15.70500000000000007 ) ) ;
#56211 = SURFACE_SIDE_STYLE ('',( #60807 ) ) ;
#56212 = VECTOR ( 'NONE', #53132, 1000.000000000000000 ) ;
#56215 = ORIENTED_EDGE ( 'NONE', *, *, #53136, .T. ) ;
#56214 = LINE ( 'NONE', #30389, #55908 ) ;
#56213 = VECTOR ( 'NONE', #25953, 1000.000000000000000 ) ;
#56216 = CARTESIAN_POINT ( 'NONE',  ( 30.00000000000000000, -17.50000000000000000, 26.64999999999999858 ) ) ;
#56217 = AXIS2_PLACEMENT_3D ( 'NONE', #12005, #17319, #38223 ) ;
#56218 = DIRECTION ( 'NONE',  ( 0.000000000000000000, -1.000000000000000000, 0.000000000000000000 ) ) ;
#56219 = VECTOR ( 'NONE', #10734, 1000.000000000000000 ) ;
#56220 = ORIENTED_EDGE ( 'NONE', *, *, #67508, .F. ) ;
#56221 = CARTESIAN_POINT ( 'NONE',  ( 86.07321854994620480, 47.95351654967443977, 39.00000000000000000 ) ) ;
#56222 = DIRECTION ( 'NONE',  ( 0.000000000000000000, -1.000000000000000000, 0.000000000000000000 ) ) ;
#56223 = VERTEX_POINT ( 'NONE', #48321 ) ;
#56224 = EDGE_CURVE ( 'NONE', #68694, #7560, #43001, .T. ) ;
#56225 = CARTESIAN_POINT ( 'NONE',  ( 9.900000000000000355, 21.00000000000000000, -18.00000000000000355 ) ) ;
#56226 = CARTESIAN_POINT ( 'NONE',  ( 7.000000000000000000, -21.00000000000000000, 12.50000000000000000 ) ) ;
#56227 = APPLICATION_CONTEXT ( 'automotive_design' ) ;
#56228 = CARTESIAN_POINT ( 'NONE',  ( 283.0000000000000568, -42.00000000000000000, -7.000000000000000000 ) ) ;
#56229 = VECTOR ( 'NONE', #62374, 1000.000000000000000 ) ;
#56230 = DIRECTION ( 'NONE',  ( 0.000000000000000000, -1.000000000000000000, 0.000000000000000000 ) ) ;
#56231 = ORIENTED_EDGE ( 'NONE', *, *, #34464, .F. ) ;
#56232 = DIRECTION ( 'NONE',  ( -0.9375000000000004441, 0.000000000000000000, -0.3479852726768752902 ) ) ;
#56233 = ORIENTED_EDGE ( 'NONE', *, *, #68521, .F. ) ;
#56234 = EDGE_LOOP ( 'NONE', ( #3405, #38631, #64778, #51279 ) ) ;
#56235 = CARTESIAN_POINT ( 'NONE',  ( 29.25000000000000000, -5.200000000000001066, 11.75000000000000000 ) ) ;
#56236 = CARTESIAN_POINT ( 'NONE',  ( 4.456444791733522252E-16, 7.450000000000002842, -23.50000000000000000 ) ) ;
#56238 = PLANE ( 'NONE',  #10684 ) ;
#56237 = DIRECTION ( 'NONE',  ( 1.836970198721029934E-16, 1.836970198721010706E-16, -1.000000000000000000 ) ) ;
#56239 = VERTEX_POINT ( 'NONE', #4494 ) ;
#56240 = ORIENTED_EDGE ( 'NONE', *, *, #8918, .F. ) ;
#56242 = EDGE_CURVE ( 'NONE', #46696, #62134, #16135, .T. ) ;
#56241 = DIRECTION ( 'NONE',  ( 0.000000000000000000, 0.000000000000000000, 1.000000000000000000 ) ) ;
#56243 = EDGE_LOOP ( 'NONE', ( #45804, #30044, #7715, #56059 ) ) ;
#56244 = EDGE_CURVE ( 'NONE', #41347, #60663, #9803, .T. ) ;
#56245 = CARTESIAN_POINT ( 'NONE',  ( 6.006483450353379716, -4.606483450353492159, 455.0000000000000568 ) ) ;
#56246 = CARTESIAN_POINT ( 'NONE',  ( 36.90000000000000568, -0.2000000000089119934, -8.913009219568841313E-12 ) ) ;
#56247 = FACE_OUTER_BOUND ( 'NONE', #61624, .T. ) ;
#56248 = VECTOR ( 'NONE', #54160, 1000.000000000000000 ) ;
#56249 = EDGE_CURVE ( 'NONE', #27468, #21827, #25139, .T. ) ;
#56250 = CARTESIAN_POINT ( 'NONE',  ( 0.000000000000000000, 0.000000000000000000, -8.500000000000000000 ) ) ;
#56252 = CARTESIAN_POINT ( 'NONE',  ( 10.31452373788281562, -3.664523737882816157, 26.00000000000000711 ) ) ;
#56251 = PLANE ( 'NONE',  #67133 ) ;
#56253 = ORIENTED_EDGE ( 'NONE', *, *, #22874, .F. ) ;
#56255 = ORIENTED_EDGE ( 'NONE', *, *, #37787, .F. ) ;
#56254 = FACE_OUTER_BOUND ( 'NONE', #15940, .T. ) ;
#56256 = ORIENTED_EDGE ( 'NONE', *, *, #68874, .F. ) ;
#56257 = ORIENTED_EDGE ( 'NONE', *, *, #34088, .T. ) ;
#56258 = PLANE ( 'NONE',  #11789 ) ;
#56259 = VECTOR ( 'NONE', #8389, 1000.000000000000000 ) ;
#56260 = CARTESIAN_POINT ( 'NONE',  ( 7.000000000000000000, -37.15000000000001279, 7.700000000000000178 ) ) ;
#56261 = VERTEX_POINT ( 'NONE', #37366 ) ;
#56262 = ORIENTED_EDGE ( 'NONE', *, *, #56206, .T. ) ;
#56263 = VECTOR ( 'NONE', #18342, 1000.000000000000000 ) ;
#56264 = PLANE ( 'NONE',  #63678 ) ;
#56265 = DIRECTION ( 'NONE',  ( 1.000000000000000000, 0.000000000000000000, 0.000000000000000000 ) ) ;
#56266 = VERTEX_POINT ( 'NONE', #4147 ) ;
#56267 = ORIENTED_EDGE ( 'NONE', *, *, #3089, .F. ) ;
#56268 = LINE ( 'NONE', #50962, #4817 ) ;
#56269 = CARTESIAN_POINT ( 'NONE',  ( 5.393625297349938563, 7.252248008019325454, 455.0000000000000568 ) ) ;
#56270 = ORIENTED_EDGE ( 'NONE', *, *, #36325, .T. ) ;
#56271 = AXIS2_PLACEMENT_3D ( 'NONE', #55606, #39675, #29081 ) ;
#56272 = EDGE_CURVE ( 'NONE', #5559, #33795, #63540, .T. ) ;
#56273 = CARTESIAN_POINT ( 'NONE',  ( 40.90000000000000568, 21.00000000000000000, 13.98999642601811999 ) ) ;
#56274 = DIRECTION ( 'NONE',  ( -1.000000000000000000, 0.000000000000000000, 0.000000000000000000 ) ) ;
#56276 = EDGE_LOOP ( 'NONE', ( #17016, #10659, #60081, #66169 ) ) ;
#56275 = LINE ( 'NONE', #24093, #64502 ) ;
#56277 = ORIENTED_EDGE ( 'NONE', *, *, #7745, .F. ) ;
#56278 = EDGE_CURVE ( 'NONE', #31600, #69380, #48874, .T. ) ;
#56279 = DIRECTION ( 'NONE',  ( -0.000000000000000000, 0.000000000000000000, 1.000000000000000000 ) ) ;
#56280 = DIRECTION ( 'NONE',  ( 0.000000000000000000, 1.000000000000000000, 0.000000000000000000 ) ) ;
#56281 = LINE ( 'NONE', #67242, #44177 ) ;
#56282 = EDGE_CURVE ( 'NONE', #10769, #39380, #59270, .T. ) ;
#56283 = DIRECTION ( 'NONE',  ( 1.000000000000000000, -0.000000000000000000, 0.000000000000000000 ) ) ;
#56284 = EDGE_CURVE ( 'NONE', #38291, #50590, #58927, .T. ) ;
#56285 = CARTESIAN_POINT ( 'NONE',  ( 7.450000000000004619, -1.336933437520057563E-15, -21.50000000000000000 ) ) ;
#56286 = DIRECTION ( 'NONE',  ( 1.261617073437657735E-14, 1.000000000000000000, 3.673940397442059868E-16 ) ) ;
#56287 = EDGE_CURVE ( 'NONE', #43516, #41912, #52244, .T. ) ;
#56288 = EDGE_CURVE ( 'NONE', #33465, #14877, #46575, .T. ) ;
#56289 = DIRECTION ( 'NONE',  ( 0.000000000000000000, 1.000000000000000000, 0.000000000000000000 ) ) ;
#56290 = ORIENTED_EDGE ( 'NONE', *, *, #60842, .F. ) ;
#56291 = CARTESIAN_POINT ( 'NONE',  ( -9.093516549646782465, -11.12648345035334252, 195.0000000000000284 ) ) ;
#56293 = ORIENTED_EDGE ( 'NONE', *, *, #42722, .T. ) ;
#56292 = LINE ( 'NONE', #50984, #66066 ) ;
#56294 = DIRECTION ( 'NONE',  ( -1.000000000000000000, 0.000000000000000000, 0.000000000000000000 ) ) ;
#56295 = CARTESIAN_POINT ( 'NONE',  ( 8.250000000000005329, -7.249999999999998224, -10.50000000000000000 ) ) ;
#56296 = ADVANCED_FACE ( 'NONE', ( #37029, #26402 ), #9435, .F. ) ;
#56297 = FACE_OUTER_BOUND ( 'NONE', #28773, .T. ) ;
#56298 = FACE_OUTER_BOUND ( 'NONE', #19851, .T. ) ;
#56299 = DIRECTION ( 'NONE',  ( 0.000000000000000000, 0.000000000000000000, -1.000000000000000000 ) ) ;
#56300 = ORIENTED_EDGE ( 'NONE', *, *, #50299, .F. ) ;
#56301 = DIRECTION ( 'NONE',  ( -1.000000000000000000, 0.000000000000000000, 0.000000000000000000 ) ) ;
#56302 = ORIENTED_EDGE ( 'NONE', *, *, #3793, .F. ) ;
#56303 = AXIS2_PLACEMENT_3D ( 'NONE', #33803, #50071, #45808 ) ;
#56304 = DIRECTION ( 'NONE',  ( -1.000000000000000000, 0.000000000000000000, 0.000000000000000000 ) ) ;
#56305 = LINE ( 'NONE', #50996, #27771 ) ;
#56306 = AXIS2_PLACEMENT_3D ( 'NONE', #53648, #66241, #45009 ) ;
#56307 = CARTESIAN_POINT ( 'NONE',  ( 7.250000000000005329, 8.250000000000001776, -15.00000000000000000 ) ) ;
#56308 = VERTEX_POINT ( 'NONE', #15095 ) ;
#56309 = DIRECTION ( 'NONE',  ( -1.000000000000000000, 0.000000000000000000, 0.000000000000000000 ) ) ;
#56310 = VERTEX_POINT ( 'NONE', #36657 ) ;
#56311 = ORIENTED_EDGE ( 'NONE', *, *, #65856, .T. ) ;
#56312 = CIRCLE ( 'NONE', #25851, 0.2000000000000005107 ) ;
#56313 = CARTESIAN_POINT ( 'NONE',  ( 41.09999999999999432, 13.66939075806899950, 20.80000000000000426 ) ) ;
#56314 = DIRECTION ( 'NONE',  ( -1.047444401652940007E-14, -1.000000000000000000, -1.836970198721029934E-16 ) ) ;
#56315 = VERTEX_POINT ( 'NONE', #20739 ) ;
#56316 = DIRECTION ( 'NONE',  ( -1.836970198721029934E-16, 1.836970198721036344E-16, -1.000000000000000000 ) ) ;
#56317 = PLANE ( 'NONE',  #7195 ) ;
#56318 = LINE ( 'NONE', #40033, #27266 ) ;
#56319 = ORIENTED_EDGE ( 'NONE', *, *, #67947, .T. ) ;
#56320 = VERTEX_POINT ( 'NONE', #25717 ) ;
#56322 = VERTEX_POINT ( 'NONE', #47270 ) ;
#56321 = DIRECTION ( 'NONE',  ( 0.000000000000000000, 1.000000000000000000, 3.673940397442059868E-16 ) ) ;
#56323 = ORIENTED_EDGE ( 'NONE', *, *, #47844, .T. ) ;
#56324 = CIRCLE ( 'NONE', #1026, 24.99999999998794920 ) ;
#56325 = EDGE_CURVE ( 'NONE', #56650, #29848, #31378, .T. ) ;
#56326 = CARTESIAN_POINT ( 'NONE',  ( 4.201500623656039934, 7.259684009079806266, 455.0000000000000568 ) ) ;
#56327 = LINE ( 'NONE', #51022, #67022 ) ;
#56328 = DIRECTION ( 'NONE',  ( -1.000000000000000000, 0.000000000000000000, 0.000000000000000000 ) ) ;
#56329 = CARTESIAN_POINT ( 'NONE',  ( -16.75000000000000000, -2.500000000000000000, -21.77831216351300014 ) ) ;
#56330 = ADVANCED_FACE ( 'NONE', ( #69534, #63884 ), #53631, .T. ) ;
#56331 = EDGE_CURVE ( 'NONE', #40323, #63752, #65289, .T. ) ;
#56332 = DIRECTION ( 'NONE',  ( -1.836970198721029934E-16, 1.836970198721036344E-16, -1.000000000000000000 ) ) ;
#56333 = LINE ( 'NONE', #39711, #60095 ) ;
#56334 = VERTEX_POINT ( 'NONE', #33090 ) ;
#56335 = VERTEX_POINT ( 'NONE', #17170 ) ;
#56336 = EDGE_CURVE ( 'NONE', #66645, #47996, #21790, .T. ) ;
#56337 = ORIENTED_EDGE ( 'NONE', *, *, #10610, .F. ) ;
#56338 = ORIENTED_EDGE ( 'NONE', *, *, #4775, .T. ) ;
#56339 = CARTESIAN_POINT ( 'NONE',  ( -11.77351654964670935, 7.813516549646603693, 455.0000000000000568 ) ) ;
#56340 = CARTESIAN_POINT ( 'NONE',  ( 14.50000000000000000, -42.00000000000000000, -27.00000000000000000 ) ) ;
#56341 = DIRECTION ( 'NONE',  ( -0.000000000000000000, -0.000000000000000000, -1.000000000000000000 ) ) ;
#56342 =( NAMED_UNIT ( * ) SI_UNIT ( $, .STERADIAN. ) SOLID_ANGLE_UNIT ( ) );
#56343 = DIRECTION ( 'NONE',  ( 0.000000000000000000, 0.000000000000000000, -1.000000000000000000 ) ) ;
#56344 = ORIENTED_EDGE ( 'NONE', *, *, #9643, .F. ) ;
#56345 = EDGE_LOOP ( 'NONE', ( #29275, #37581, #35752, #16715 ) ) ;
#56346 = ORIENTED_EDGE ( 'NONE', *, *, #48155, .F. ) ;
#56347 = DIRECTION ( 'NONE',  ( 0.000000000000000000, 1.000000000000000000, -0.000000000000000000 ) ) ;
#56348 = ORIENTED_EDGE ( 'NONE', *, *, #26449, .T. ) ;
#56349 = ORIENTED_EDGE ( 'NONE', *, *, #54322, .T. ) ;
#56350 = EDGE_LOOP ( 'NONE', ( #43324, #55951, #55575, #40442 ) ) ;
#56351 = VECTOR ( 'NONE', #10661, 1000.000000000000000 ) ;
#56352 = ORIENTED_EDGE ( 'NONE', *, *, #993, .T. ) ;
#56353 = FACE_OUTER_BOUND ( 'NONE', #63505, .T. ) ;
#56355 = ORIENTED_EDGE ( 'NONE', *, *, #37842, .T. ) ;
#56354 = LINE ( 'NONE', #61288, #13036 ) ;
#56356 = ORIENTED_EDGE ( 'NONE', *, *, #60498, .T. ) ;
#56357 = AXIS2_PLACEMENT_3D ( 'NONE', #20940, #10000, #69382 ) ;
#56358 = DIRECTION ( 'NONE',  ( -1.000000000000000000, 0.000000000000000000, 0.000000000000000000 ) ) ;
#56359 = CYLINDRICAL_SURFACE ( 'NONE', #37484, 24.99999999998784972 ) ;
#56360 = DIRECTION ( 'NONE',  ( -1.794541526872559352E-16, -1.000000000000000000, 0.000000000000000000 ) ) ;
#56362 = VERTEX_POINT ( 'NONE', #7241 ) ;
#56361 = CARTESIAN_POINT ( 'NONE',  ( 39.90000000000000568, 0.000000000000000000, 0.000000000000000000 ) ) ;
#56363 = EDGE_LOOP ( 'NONE', ( #8772, #9348, #55235, #33007 ) ) ;
#56364 = VECTOR ( 'NONE', #29411, 1000.000000000000000 ) ;
#56365 = DIRECTION ( 'NONE',  ( 1.000000000000000000, -0.000000000000000000, -0.000000000000000000 ) ) ;
#56366 = DIRECTION ( 'NONE',  ( 1.000000000000000000, -2.135044278125299371E-15, -7.844025423732057781E-31 ) ) ;
#56367 = AXIS2_PLACEMENT_3D ( 'NONE', #14373, #51502, #63863 ) ;
#56368 = FACE_OUTER_BOUND ( 'NONE', #26736, .T. ) ;
#56369 = ADVANCED_FACE ( 'NONE', ( #50037 ), #940, .F. ) ;
#56370 = ORIENTED_EDGE ( 'NONE', *, *, #16469, .T. ) ;
#56371 = DIRECTION ( 'NONE',  ( -0.4999999999999786282, 0.8660254037844510311, 3.181725716174766844E-16 ) ) ;
#56372 = AXIS2_PLACEMENT_3D ( 'NONE', #29864, #56388, #23164 ) ;
#56373 = LINE ( 'NONE', #45760, #3838 ) ;
#56374 = DIRECTION ( 'NONE',  ( -1.000000000000000000, 0.000000000000000000, 0.000000000000000000 ) ) ;
#56375 = ADVANCED_FACE ( 'NONE', ( #49699 ), #49015, .T. ) ;
#56376 = ORIENTED_EDGE ( 'NONE', *, *, #4333, .F. ) ;
#56377 = CARTESIAN_POINT ( 'NONE',  ( -8.566576262117260754, 8.916576262117214213, 26.00000000000000711 ) ) ;
#56378 = AXIS2_PLACEMENT_3D ( 'NONE', #41765, #63350, #69343 ) ;
#56379 = DIRECTION ( 'NONE',  ( -1.000000000000000000, 0.000000000000000000, 0.000000000000000000 ) ) ;
#56380 = LINE ( 'NONE', #34103, #6576 ) ;
#56381 = VERTEX_POINT ( 'NONE', #60658 ) ;
#56382 = PLANE ( 'NONE',  #56151 ) ;
#56383 = CARTESIAN_POINT ( 'NONE',  ( 15.50000000000000000, -1.037157890325000054, 22.50000000000000000 ) ) ;
#56384 = FACE_OUTER_BOUND ( 'NONE', #36917, .T. ) ;
#56385 = EDGE_CURVE ( 'NONE', #3293, #41058, #3689, .T. ) ;
#56386 = VERTEX_POINT ( 'NONE', #34114 ) ;
#56387 = AXIS2_PLACEMENT_3D ( 'NONE', #39972, #13117, #19470 ) ;
#56388 = DIRECTION ( 'NONE',  ( 0.000000000000000000, 0.000000000000000000, 1.000000000000000000 ) ) ;
#56389 = DIRECTION ( 'NONE',  ( -1.000000000000000000, 5.120954910632640039E-15, 0.000000000000000000 ) ) ;
#56390 = LINE ( 'NONE', #29866, #35303 ) ;
#56391 = CARTESIAN_POINT ( 'NONE',  ( -10.30047626211725742, 3.650476262117184234, 26.00000000000000711 ) ) ;
#56392 = CARTESIAN_POINT ( 'NONE',  ( 16.89999999999999858, 20.60000000000000142, -13.86939075806900057 ) ) ;
#56393 = ORIENTED_EDGE ( 'NONE', *, *, #17169, .F. ) ;
#56394 = DIRECTION ( 'NONE',  ( 0.7071067811865530128, 0.7071067811865421326, 0.000000000000000000 ) ) ;
#56395 = CARTESIAN_POINT ( 'NONE',  ( 69.92576880110368620, 0.000000000000000000, 281.4830310981151911 ) ) ;
#56396 = DIRECTION ( 'NONE',  ( 8.659560562354951347E-17, -0.7071067811865460184, 0.7071067811865489050 ) ) ;
#56397 = CARTESIAN_POINT ( 'NONE',  ( -8.250000000000001776, -7.249999999999998224, -24.50000000000000000 ) ) ;
#56398 = CARTESIAN_POINT ( 'NONE',  ( 13.00000000000000178, -17.50000000000000000, 20.05051025721700242 ) ) ;
#56399 = ORIENTED_EDGE ( 'NONE', *, *, #38736, .F. ) ;
#56400 = VECTOR ( 'NONE', #58943, 1000.000000000000000 ) ;
#56402 = ORIENTED_EDGE ( 'NONE', *, *, #49090, .F. ) ;
#56401 = FACE_OUTER_BOUND ( 'NONE', #31824, .T. ) ;
#56403 = CIRCLE ( 'NONE', #25950, 4.000000000000000888 ) ;
#56404 = DIRECTION ( 'NONE',  ( 1.000000000000000000, -5.981805089575194965E-17, 0.000000000000000000 ) ) ;
#56405 = CARTESIAN_POINT ( 'NONE',  ( 10.92648345035337520, -9.106483450353492159, 455.0000000000000568 ) ) ;
#56406 = VERTEX_POINT ( 'NONE', #64931 ) ;
#56407 = EDGE_CURVE ( 'NONE', #11123, #15298, #11853, .T. ) ;
#56408 = AXIS2_PLACEMENT_3D ( 'NONE', #26567, #48139, #5705 ) ;
#56409 = DIRECTION ( 'NONE',  ( 0.000000000000000000, 0.000000000000000000, -1.000000000000000000 ) ) ;
#56410 = ORIENTED_EDGE ( 'NONE', *, *, #4333, .T. ) ;
#56411 = EDGE_CURVE ( 'NONE', #24688, #31770, #226, .T. ) ;
#56412 = AXIS2_PLACEMENT_3D ( 'NONE', #21969, #46821, #63449 ) ;
#56413 = CARTESIAN_POINT ( 'NONE',  ( 41.09999999999999432, -21.00000000000000000, -13.86939075806900057 ) ) ;
#56414 = ORIENTED_EDGE ( 'NONE', *, *, #59381, .F. ) ;
#56415 = ORIENTED_EDGE ( 'NONE', *, *, #5312, .T. ) ;
#56416 = CARTESIAN_POINT ( 'NONE',  ( 0.000000000000000000, 8.250000000000001776, -18.00000000000000000 ) ) ;
#56417 = DIRECTION ( 'NONE',  ( -1.794541526872559352E-16, -1.000000000000000000, 0.000000000000000000 ) ) ;
#56418 = VECTOR ( 'NONE', #63018, 1000.000000000000000 ) ;
#56419 = DIRECTION ( 'NONE',  ( -0.000000000000000000, -0.000000000000000000, -1.000000000000000000 ) ) ;
#56420 = CARTESIAN_POINT ( 'NONE',  ( -7.342976262117288933, -6.665817930929258672, 26.00000000000000000 ) ) ;
#56421 = ORIENTED_EDGE ( 'NONE', *, *, #31102, .T. ) ;
#56422 = EDGE_LOOP ( 'NONE', ( #68621, #61963, #67572, #57526 ) ) ;
#56423 = CARTESIAN_POINT ( 'NONE',  ( 0.000000000000000000, 0.000000000000000000, -17.50000000000000000 ) ) ;
#56425 = DIRECTION ( 'NONE',  ( -1.836970198721029934E-16, -1.836970198721010706E-16, 1.000000000000000000 ) ) ;
#56424 = AXIS2_PLACEMENT_3D ( 'NONE', #54023, #5572, #37062 ) ;
#56426 = ORIENTED_EDGE ( 'NONE', *, *, #51090, .T. ) ;
#56427 = ORIENTED_EDGE ( 'NONE', *, *, #14313, .T. ) ;
#56428 = EDGE_LOOP ( 'NONE', ( #38251, #1039, #50927, #7119, #69175, #65134, #60090, #7553 ) ) ;
#56429 = EDGE_CURVE ( 'NONE', #36185, #48836, #50010, .T. ) ;
#56430 = DIRECTION ( 'NONE',  ( -0.7071067811865474617, 0.7071067811865474617, -0.000000000000000000 ) ) ;
#56432 = ORIENTED_EDGE ( 'NONE', *, *, #22534, .T. ) ;
#56431 = DIRECTION ( 'NONE',  ( 1.836970198721029934E-16, 1.836970198721010706E-16, -1.000000000000000000 ) ) ;
#56433 = DIRECTION ( 'NONE',  ( 0.000000000000000000, 0.000000000000000000, -1.000000000000000000 ) ) ;
#56434 = CARTESIAN_POINT ( 'NONE',  ( 30.00000000000000000, -17.00000000000000000, -15.70499999999969809 ) ) ;
#56435 = VECTOR ( 'NONE', #68802, 1000.000000000000000 ) ;
#56436 = ORIENTED_EDGE ( 'NONE', *, *, #38511, .T. ) ;
#56437 = VERTEX_POINT ( 'NONE', #65615 ) ;
#56438 = CYLINDRICAL_SURFACE ( 'NONE', #2166, 0.3999999999999993006 ) ;
#56439 = DIRECTION ( 'NONE',  ( 0.000000000000000000, 0.000000000000000000, -1.000000000000000000 ) ) ;
#56440 = CARTESIAN_POINT ( 'NONE',  ( -7.450000000000001954, 7.250000000000000000, -19.50000000000000000 ) ) ;
#56441 = CIRCLE ( 'NONE', #1151, 0.1749999999999998224 ) ;
#56442 = EDGE_CURVE ( 'NONE', #14977, #41272, #33442, .T. ) ;
#56443 = VECTOR ( 'NONE', #49094, 1000.000000000000000 ) ;
#56444 = LINE ( 'NONE', #3071, #15332 ) ;
#56445 = DIRECTION ( 'NONE',  ( 0.000000000000000000, 0.000000000000000000, -1.000000000000000000 ) ) ;
#56446 = EDGE_CURVE ( 'NONE', #9593, #4203, #38403, .T. ) ;
#56447 = EDGE_CURVE ( 'NONE', #38888, #60780, #6903, .T. ) ;
#56449 = ORIENTED_EDGE ( 'NONE', *, *, #7910, .F. ) ;
#56448 = CARTESIAN_POINT ( 'NONE',  ( -8.821682069070828192, -7.969523737882767911, 54.00000000000000711 ) ) ;
#56450 = ORIENTED_EDGE ( 'NONE', *, *, #12049, .F. ) ;
#56451 = LINE ( 'NONE', #18978, #54683 ) ;
#56453 = DIRECTION ( 'NONE',  ( -0.000000000000000000, -0.000000000000000000, 1.000000000000000000 ) ) ;
#56452 = VECTOR ( 'NONE', #21865, 1000.000000000000000 ) ;
#56454 = DIRECTION ( 'NONE',  ( 0.000000000000000000, 0.000000000000000000, -1.000000000000000000 ) ) ;
#56455 = EDGE_CURVE ( 'NONE', #51358, #19035, #44373, .T. ) ;
#56456 = CARTESIAN_POINT ( 'NONE',  ( 4.186483450353335023, -12.00648345035347830, 455.0000000000000568 ) ) ;
#56457 = EDGE_CURVE ( 'NONE', #69443, #49539, #26306, .T. ) ;
#56458 = AXIS2_PLACEMENT_3D ( 'NONE', #32840, #54421, #50821 ) ;
#56459 = DIRECTION ( 'NONE',  ( 1.000000000000000000, -0.000000000000000000, -0.000000000000000000 ) ) ;
#56460 = EDGE_CURVE ( 'NONE', #20566, #58112, #32742, .T. ) ;
#56461 = ORIENTED_EDGE ( 'NONE', *, *, #24193, .F. ) ;
#56462 = CARTESIAN_POINT ( 'NONE',  ( -25.50000000000000355, -5.200000000000001066, -22.50000000000000000 ) ) ;
#56463 = LINE ( 'NONE', #30302, #68895 ) ;
#56465 = EDGE_CURVE ( 'NONE', #49178, #55278, #51120, .T. ) ;
#56464 = DIRECTION ( 'NONE',  ( -1.000000000000000000, 0.000000000000000000, 0.000000000000000000 ) ) ;
#56466 = DIRECTION ( 'NONE',  ( 0.000000000000000000, 0.000000000000000000, 1.000000000000000000 ) ) ;
#56467 = CYLINDRICAL_SURFACE ( 'NONE', #15711, 24.99999999998784972 ) ;
#56468 = CARTESIAN_POINT ( 'NONE',  ( 5.257023737882795977, 5.242976262117205799, 26.00000000000000711 ) ) ;
#56469 = VECTOR ( 'NONE', #11417, 1000.000000000000000 ) ;
#56470 = VECTOR ( 'NONE', #48702, 1000.000000000000000 ) ;
#56471 = CARTESIAN_POINT ( 'NONE',  ( -9.547976262117256141, 2.530476262117183683, 26.00000000000000711 ) ) ;
#56472 = VERTEX_POINT ( 'NONE', #6579 ) ;
#56473 = LINE ( 'NONE', #12971, #11741 ) ;
#56474 = CARTESIAN_POINT ( 'NONE',  ( 7.450000000000003730, -7.249999999999997335, -24.50000000000000000 ) ) ;
#56475 = VERTEX_POINT ( 'NONE', #6222 ) ;
#56476 = CARTESIAN_POINT ( 'NONE',  ( 275.0000000000000000, -20.40000000000000213, -12.40000000000000213 ) ) ;
#56477 = FACE_OUTER_BOUND ( 'NONE', #1240, .T. ) ;
#56478 = DIRECTION ( 'NONE',  ( 0.000000000000000000, 0.000000000000000000, 1.000000000000000000 ) ) ;
#56479 = DIRECTION ( 'NONE',  ( -0.000000000000000000, 3.673940397442059868E-16, -1.000000000000000000 ) ) ;
#56480 = CARTESIAN_POINT ( 'NONE',  ( -11.77351654964670935, 4.173516549646604901, 195.0000000000000284 ) ) ;
#56481 = ORIENTED_EDGE ( 'NONE', *, *, #10877, .T. ) ;
#56482 = DIRECTION ( 'NONE',  ( 0.000000000000000000, 0.000000000000000000, 1.000000000000000000 ) ) ;
#56483 = EDGE_LOOP ( 'NONE', ( #62541, #24750, #64395, #57803, #36888, #67518 ) ) ;
#56484 = CIRCLE ( 'NONE', #55390, 0.2000000000000005107 ) ;
#56485 = CARTESIAN_POINT ( 'NONE',  ( -7.415254214038336400, 3.593516549646603497, 455.0000000000000568 ) ) ;
#56486 = EDGE_CURVE ( 'NONE', #20807, #42575, #22143, .T. ) ;
#56487 = VERTEX_POINT ( 'NONE', #43708 ) ;
#56488 = FACE_OUTER_BOUND ( 'NONE', #64547, .T. ) ;
#56489 = ORIENTED_EDGE ( 'NONE', *, *, #22999, .T. ) ;
#56490 = EDGE_CURVE ( 'NONE', #65734, #8948, #11508, .T. ) ;
#56491 = CARTESIAN_POINT ( 'NONE',  ( 20.90000000000000213, -21.00000000000001421, -13.86939075806900945 ) ) ;
#56492 = CIRCLE ( 'NONE', #46354, 3.233000000000000096 ) ;
#56493 = CYLINDRICAL_SURFACE ( 'NONE', #52605, 25.39999999999999858 ) ;
#56494 = ORIENTED_EDGE ( 'NONE', *, *, #12865, .T. ) ;
#56495 = ORIENTED_EDGE ( 'NONE', *, *, #10964, .T. ) ;
#56496 = CARTESIAN_POINT ( 'NONE',  ( 1.090483450353338268, -11.34648345035345329, 455.0000000000000568 ) ) ;
#56497 = VECTOR ( 'NONE', #4301, 1000.000000000000000 ) ;
#56498 = ORIENTED_EDGE ( 'NONE', *, *, #41030, .F. ) ;
#56499 = VERTEX_POINT ( 'NONE', #34455 ) ;
#56500 = DIRECTION ( 'NONE',  ( 0.7671651518153131954, 0.6414496315691415873, 2.587583378555109562E-16 ) ) ;
#56501 = LINE ( 'NONE', #25039, #45974 ) ;
#56503 = DIRECTION ( 'NONE',  ( -0.000000000000000000, 3.673940397442059868E-16, -1.000000000000000000 ) ) ;
#56502 = AXIS2_PLACEMENT_3D ( 'NONE', #41541, #37291, #69460 ) ;
#56504 = ORIENTED_EDGE ( 'NONE', *, *, #9944, .T. ) ;
#56505 = AXIS2_PLACEMENT_3D ( 'NONE', #42996, #47610, #69177 ) ;
#56506 = CARTESIAN_POINT ( 'NONE',  ( -3.834182069070824816, -7.532023737882819425, 54.00000000000000711 ) ) ;
#56508 = FACE_OUTER_BOUND ( 'NONE', #40136, .T. ) ;
#56507 = FACE_OUTER_BOUND ( 'NONE', #19653, .T. ) ;
#56509 = VERTEX_POINT ( 'NONE', #66997 ) ;
#56511 = EDGE_LOOP ( 'NONE', ( #35919, #47835, #33207, #18977 ) ) ;
#56510 = CARTESIAN_POINT ( 'NONE',  ( 10.05377373788278739, -9.703773737882823269, 54.00000000000000711 ) ) ;
#56512 = ORIENTED_EDGE ( 'NONE', *, *, #12467, .F. ) ;
#56513 = VECTOR ( 'NONE', #63189, 1000.000000000000000 ) ;
#56514 = APPLICATION_PROTOCOL_DEFINITION ( 'draft international standard', 'automotive_design', 1998, #62502 ) ;
#56515 = EDGE_CURVE ( 'NONE', #40339, #43425, #51083, .T. ) ;
#56516 = PLANE ( 'NONE',  #15247 ) ;
#56517 = VERTEX_POINT ( 'NONE', #24219 ) ;
#56518 = CARTESIAN_POINT ( 'NONE',  ( 30.00000000000000000, -12.00000000000000000, -11.03137303340310282 ) ) ;
#56519 = CARTESIAN_POINT ( 'NONE',  ( -28.00000000000000000, -15.50000000000000000, -20.05051025721700242 ) ) ;
#56520 = ORIENTED_EDGE ( 'NONE', *, *, #59986, .T. ) ;
#56521 = EDGE_CURVE ( 'NONE', #25535, #1031, #3351, .T. ) ;
#56522 = ORIENTED_EDGE ( 'NONE', *, *, #27163, .F. ) ;
#56523 = VECTOR ( 'NONE', #49515, 1000.000000000000000 ) ;
#56524 = VECTOR ( 'NONE', #13910, 1000.000000000000000 ) ;
#56525 = CARTESIAN_POINT ( 'NONE',  ( -7.450000000000001954, 0.000000000000000000, -11.00000000000000000 ) ) ;
#56526 = LINE ( 'NONE', #17994, #24419 ) ;
#56527 = EDGE_CURVE ( 'NONE', #29684, #4835, #67358, .T. ) ;
#56528 = ADVANCED_FACE ( 'NONE', ( #68054 ), #56045, .F. ) ;
#56529 = ORIENTED_EDGE ( 'NONE', *, *, #44796, .F. ) ;
#56530 = DIRECTION ( 'NONE',  ( 0.000000000000000000, 1.000000000000000000, 0.000000000000000000 ) ) ;
#56531 = LINE ( 'NONE', #24709, #59468 ) ;
#56532 = CARTESIAN_POINT ( 'NONE',  ( 7.811466277050774565, 7.259684009079793832, 455.0000000000000568 ) ) ;
#56533 = EDGE_LOOP ( 'NONE', ( #46227, #60753, #52200, #44621, #46511, #25456 ) ) ;
#56534 = DIRECTION ( 'NONE',  ( 0.000000000000000000, 0.000000000000000000, 1.000000000000000000 ) ) ;
#56535 = EDGE_CURVE ( 'NONE', #36733, #39553, #40475, .T. ) ;
#56536 = CARTESIAN_POINT ( 'NONE',  ( 6.832023737882815695, 9.897976262117191837, 54.00000000000000711 ) ) ;
#56538 = ORIENTED_EDGE ( 'NONE', *, *, #18779, .F. ) ;
#56537 = CYLINDRICAL_SURFACE ( 'NONE', #62300, 0.1999999999999996503 ) ;
#56540 = ORIENTED_EDGE ( 'NONE', *, *, #1758, .F. ) ;
#56539 = DIRECTION ( 'NONE',  ( 0.000000000000000000, 0.000000000000000000, 1.000000000000000000 ) ) ;
#56541 = EDGE_CURVE ( 'NONE', #46508, #21984, #14320, .T. ) ;
#56542 = CARTESIAN_POINT ( 'NONE',  ( -11.00000000000000000, -11.50000000000082068, 10.20500000000000007 ) ) ;
#56543 = DIRECTION ( 'NONE',  ( -1.000000000000000000, 0.000000000000000000, 0.000000000000000000 ) ) ;
#56544 = CARTESIAN_POINT ( 'NONE',  ( 3.664523737882814824, 10.30047626211720768, 26.00000000000000711 ) ) ;
#56545 = DIRECTION ( 'NONE',  ( -7.808916176531286882E-15, -1.000000000000000000, 0.000000000000000000 ) ) ;
#56546 = DIRECTION ( 'NONE',  ( 0.5773502691896257311, 0.5773502691896257311, 0.5773502691896257311 ) ) ;
#56547 = EDGE_CURVE ( 'NONE', #54114, #2916, #67698, .T. ) ;
#56548 = ORIENTED_EDGE ( 'NONE', *, *, #22999, .F. ) ;
#56549 = CARTESIAN_POINT ( 'NONE',  ( -15.50000000000000000, -5.000000000000000000, -22.50000000000000000 ) ) ;
#56550 = DIRECTION ( 'NONE',  ( 1.836970198721029934E-16, -1.836970198721036344E-16, 1.000000000000000000 ) ) ;
#56551 = VECTOR ( 'NONE', #6873, 1000.000000000000000 ) ;
#56553 = EDGE_CURVE ( 'NONE', #50555, #12586, #8654, .T. ) ;
#56552 = CYLINDRICAL_SURFACE ( 'NONE', #50327, 0.1749999999999998224 ) ;
#56555 = ORIENTED_EDGE ( 'NONE', *, *, #5490, .T. ) ;
#56554 = DIRECTION ( 'NONE',  ( 1.000000000000000000, 0.000000000000000000, 0.000000000000000000 ) ) ;
#56556 = PRODUCT ( 'BR-Y-111', 'BR-Y-111', '', ( #8782 ) ) ;
#56557 = CIRCLE ( 'NONE', #45236, 0.5000000000079362072 ) ;
#56558 = CARTESIAN_POINT ( 'NONE',  ( -5.242976262117280406, -5.257023737882805747, 54.00000000000000711 ) ) ;
#56559 = DIRECTION ( 'NONE',  ( -1.000000000000000000, 0.000000000000000000, 0.000000000000000000 ) ) ;
#56560 = CIRCLE ( 'NONE', #54306, 0.1999999999999996503 ) ;
#56561 = VERTEX_POINT ( 'NONE', #29518 ) ;
#56562 = ORIENTED_EDGE ( 'NONE', *, *, #54064, .T. ) ;
#56563 = LINE ( 'NONE', #29681, #69349 ) ;
#56564 = LINE ( 'NONE', #29329, #49798 ) ;
#56565 = EDGE_CURVE ( 'NONE', #63123, #43741, #34814, .T. ) ;
#56566 = EDGE_LOOP ( 'NONE', ( #25675, #30597, #57152, #54762, #34826, #53095 ) ) ;
#56567 = VECTOR ( 'NONE', #1881, 1000.000000000000000 ) ;
#56568 = VECTOR ( 'NONE', #62062, 1000.000000000000000 ) ;
#56569 = CARTESIAN_POINT ( 'NONE',  ( 30.00000000000000000, -16.28999999999710369, -15.00000000000794920 ) ) ;
#56570 = CARTESIAN_POINT ( 'NONE',  ( 47.00000000000000000, -0.7500000000000000000, 4.943429983321300014 ) ) ;
#56571 = DIRECTION ( 'NONE',  ( 0.1289152302546202611, 0.000000000000000000, 0.9916556173432378163 ) ) ;
#56572 = VERTEX_POINT ( 'NONE', #23865 ) ;
#56573 = CARTESIAN_POINT ( 'NONE',  ( -7.342976262117259623, 6.651770455163663165, 54.00000000000000711 ) ) ;
#56574 = ORIENTED_EDGE ( 'NONE', *, *, #13313, .F. ) ;
#56575 = ORIENTED_EDGE ( 'NONE', *, *, #46161, .T. ) ;
#56576 = DIRECTION ( 'NONE',  ( 1.000000000000000000, -0.000000000000000000, -0.000000000000000000 ) ) ;
#56577 = CIRCLE ( 'NONE', #4664, 24.99999999998784972 ) ;
#56578 = EDGE_CURVE ( 'NONE', #122, #52042, #46479, .T. ) ;
#56579 = CARTESIAN_POINT ( 'NONE',  ( 48.50000000000000000, -0.7500000000000000000, -3.418698582794335028 ) ) ;
#56580 = DIRECTION ( 'NONE',  ( 1.000000000000000000, 0.000000000000000000, 0.000000000000000000 ) ) ;
#56581 = EDGE_LOOP ( 'NONE', ( #55913, #58205 ) ) ;
#56582 = ORIENTED_EDGE ( 'NONE', *, *, #53190, .T. ) ;
#56583 = LINE ( 'NONE', #8132, #62318 ) ;
#56584 = ORIENTED_EDGE ( 'NONE', *, *, #23791, .F. ) ;
#56585 = ADVANCED_FACE ( 'NONE', ( #57443 ), #41172, .T. ) ;
#56586 = DIRECTION ( 'NONE',  ( 0.000000000000000000, 1.000000000000000000, -0.000000000000000000 ) ) ;
#56587 = LINE ( 'NONE', #51648, #11011 ) ;
#56588 = CARTESIAN_POINT ( 'NONE',  ( 8.406483450353359643, 7.603567055985454459, 195.0000000000000284 ) ) ;
#56589 = VECTOR ( 'NONE', #65588, 1000.000000000000000 ) ;
#56590 = CARTESIAN_POINT ( 'NONE',  ( 7.500000000000000000, -20.49999999999999645, -20.00000000000000000 ) ) ;
#56591 = ORIENTED_EDGE ( 'NONE', *, *, #31518, .T. ) ;
#56592 = EDGE_CURVE ( 'NONE', #45555, #24615, #56390, .T. ) ;
#56593 = DIRECTION ( 'NONE',  ( -0.000000000000000000, -0.000000000000000000, -1.000000000000000000 ) ) ;
#56595 = DIRECTION ( 'NONE',  ( -1.000000000000000000, 0.000000000000000000, 0.000000000000000000 ) ) ;
#56594 = CARTESIAN_POINT ( 'NONE',  ( 7.450000000000004619, -1.336933437520057563E-15, -18.50000000000000000 ) ) ;
#56596 = ORIENTED_EDGE ( 'NONE', *, *, #55887, .T. ) ;
#56597 = EDGE_CURVE ( 'NONE', #10503, #69064, #19262, .T. ) ;
#56599 = ORIENTED_EDGE ( 'NONE', *, *, #13432, .F. ) ;
#56598 = DIRECTION ( 'NONE',  ( 1.000000000000000000, -0.000000000000000000, -0.000000000000000000 ) ) ;
#56600 = ORIENTED_EDGE ( 'NONE', *, *, #2650, .T. ) ;
#56601 = ORIENTED_EDGE ( 'NONE', *, *, #46210, .T. ) ;
#56602 = EDGE_CURVE ( 'NONE', #42657, #2683, #39766, .T. ) ;
#56603 = CARTESIAN_POINT ( 'NONE',  ( -7.250000000000000888, -8.249999999999998224, -26.00000000000001066 ) ) ;
#56604 = AXIS2_PLACEMENT_3D ( 'NONE', #43247, #48559, #132 ) ;
#56605 = DIRECTION ( 'NONE',  ( 0.000000000000000000, 0.000000000000000000, -1.000000000000000000 ) ) ;
#56606 = AXIS2_PLACEMENT_3D ( 'NONE', #64820, #16733, #26991 ) ;
#56607 = VERTEX_POINT ( 'NONE', #62381 ) ;
#56608 = VERTEX_POINT ( 'NONE', #13952 ) ;
#56609 = EDGE_CURVE ( 'NONE', #16704, #26653, #18396, .T. ) ;
#56610 = ADVANCED_FACE ( 'NONE', ( #35507 ), #66648, .F. ) ;
#56611 = DIRECTION ( 'NONE',  ( 1.000000000000000000, 0.000000000000000000, 0.000000000000000000 ) ) ;
#56612 = LINE ( 'NONE', #24443, #8556 ) ;
#56613 = ORIENTED_EDGE ( 'NONE', *, *, #39135, .T. ) ;
#56615 = ADVANCED_FACE ( 'NONE', ( #12888 ), #41879, .F. ) ;
#56614 = VECTOR ( 'NONE', #45263, 1000.000000000000000 ) ;
#56616 = EDGE_CURVE ( 'NONE', #40050, #54625, #38758, .T. ) ;
#56617 = CLOSED_SHELL ( 'NONE', ( #30438, #25744, #46431, #21346, #35935, #32, #63242, #61717, #47511, #56296, #18631, #27755 ) ) ;
#56618 = ORIENTED_EDGE ( 'NONE', *, *, #56104, .T. ) ;
#56619 = LINE ( 'NONE', #40354, #68049 ) ;
#56620 = FACE_OUTER_BOUND ( 'NONE', #50569, .T. ) ;
#56621 = EDGE_LOOP ( 'NONE', ( #16008, #20627, #35393, #1076 ) ) ;
#56622 = AXIS2_PLACEMENT_3D ( 'NONE', #47808, #25560, #13882 ) ;
#56623 = EDGE_CURVE ( 'NONE', #36081, #5045, #30572, .T. ) ;
#56624 = CARTESIAN_POINT ( 'NONE',  ( 1.690483450353370998, 10.73351654964664270, 195.0000000000000284 ) ) ;
#56625 = CARTESIAN_POINT ( 'NONE',  ( -30.00000000000000000, -12.00000000000000000, 11.03137303340310282 ) ) ;
#56626 = ORIENTED_EDGE ( 'NONE', *, *, #64151, .T. ) ;
#56627 = ORIENTED_EDGE ( 'NONE', *, *, #12422, .T. ) ;
#56629 = CARTESIAN_POINT ( 'NONE',  ( 41.09999999999999432, 20.60000000000000142, -13.86939075806900057 ) ) ;
#56628 = VECTOR ( 'NONE', #3608, 1000.000000000000000 ) ;
#56630 = LINE ( 'NONE', #29401, #62824 ) ;
#56631 = CARTESIAN_POINT ( 'NONE',  ( 5.793274621760814647, 4.141586236041038482, 54.00000000000000711 ) ) ;
#56632 = CARTESIAN_POINT ( 'NONE',  ( -24.00000000000000000, -17.50000000000000000, 15.70499999999969809 ) ) ;
#56633 = DIRECTION ( 'NONE',  ( 1.836970198721029934E-16, 1.836970198721010706E-16, -1.000000000000000000 ) ) ;
#56634 = CARTESIAN_POINT ( 'NONE',  ( 4.456444791733522252E-16, 7.450000000000002842, -14.00000000000000000 ) ) ;
#56635 = DIRECTION ( 'NONE',  ( -1.000000000000000000, 1.349135440953254490E-14, -1.836970198721005282E-16 ) ) ;
#56636 = EDGE_CURVE ( 'NONE', #40609, #13055, #770, .T. ) ;
#56637 = VERTEX_POINT ( 'NONE', #4761 ) ;
#56638 = DIRECTION ( 'NONE',  ( 1.047444401652940007E-14, 1.000000000000000000, 1.836970198721029934E-16 ) ) ;
#56641 = ORIENTED_EDGE ( 'NONE', *, *, #8467, .F. ) ;
#56640 = EDGE_CURVE ( 'NONE', #55340, #32467, #9357, .T. ) ;
#56639 = CARTESIAN_POINT ( 'NONE',  ( 7.852485183456931139, -3.430747519065322937, 195.0000000000000284 ) ) ;
#56642 = PLANE ( 'NONE',  #60303 ) ;
#56643 = LINE ( 'NONE', #8192, #68527 ) ;
#56644 = CIRCLE ( 'NONE', #32929, 2.458500000000000796 ) ;
#56645 = DIRECTION ( 'NONE',  ( -1.794541526872559352E-16, -1.000000000000000000, 0.000000000000000000 ) ) ;
#56646 = LINE ( 'NONE', #67611, #5825 ) ;
#56647 = CARTESIAN_POINT ( 'NONE',  ( -11.00000000000000000, -13.54524521594299991, -17.53999999999999915 ) ) ;
#56648 = ORIENTED_EDGE ( 'NONE', *, *, #31347, .T. ) ;
#56649 = CARTESIAN_POINT ( 'NONE',  ( 11.50000000000000000, -11.50000000000100009, -19.50000000000103739 ) ) ;
#56650 = VERTEX_POINT ( 'NONE', #68407 ) ;
#56651 = PLANE ( 'NONE',  #43788 ) ;
#56652 = CIRCLE ( 'NONE', #45331, 0.1999999999999996503 ) ;
#56653 = DIRECTION ( 'NONE',  ( 0.000000000000000000, 0.000000000000000000, -1.000000000000000000 ) ) ;
#56654 = VECTOR ( 'NONE', #66099, 1000.000000000000000 ) ;
#56655 = CARTESIAN_POINT ( 'NONE',  ( 8.750000000000000000, -7.348062532928000934, -5.000000000000000000 ) ) ;
#56656 = ORIENTED_EDGE ( 'NONE', *, *, #39762, .F. ) ;
#56657 = DIRECTION ( 'NONE',  ( -0.000000000000000000, 1.000000000000000000, -0.000000000000000000 ) ) ;
#56658 = ORIENTED_EDGE ( 'NONE', *, *, #55649, .F. ) ;
#56659 = ORIENTED_EDGE ( 'NONE', *, *, #53853, .T. ) ;
#56660 = DIRECTION ( 'NONE',  ( -1.000000000000000000, 0.000000000000000000, 0.000000000000000000 ) ) ;
#56661 = FACE_BOUND ( 'NONE', #15607, .T. ) ;
#56662 = ORIENTED_EDGE ( 'NONE', *, *, #334, .T. ) ;
#56663 = CYLINDRICAL_SURFACE ( 'NONE', #16446, 1.000000000000000000 ) ;
#56664 = VECTOR ( 'NONE', #69829, 1000.000000000000000 ) ;
#56665 = CYLINDRICAL_SURFACE ( 'NONE', #27563, 1.000000000000000000 ) ;
#56666 = CARTESIAN_POINT ( 'NONE',  ( 49.00000000000000000, 20.60000000000000142, -13.86939075806900057 ) ) ;
#56667 = ORIENTED_EDGE ( 'NONE', *, *, #54430, .F. ) ;
#56668 = ORIENTED_EDGE ( 'NONE', *, *, #19345, .F. ) ;
#56670 = ORIENTED_EDGE ( 'NONE', *, *, #36602, .T. ) ;
#56669 = CARTESIAN_POINT ( 'NONE',  ( 8.406483450353379183, -4.396432944014657451, 455.0000000000000568 ) ) ;
#56671 = VECTOR ( 'NONE', #57986, 1000.000000000000000 ) ;
#56672 = ORIENTED_EDGE ( 'NONE', *, *, #33081, .T. ) ;
#56673 = ADVANCED_FACE ( 'NONE', ( #4064 ), #42223, .T. ) ;
#56674 = DIRECTION ( 'NONE',  ( 1.280238727658158432E-15, 1.000000000000000000, -0.000000000000000000 ) ) ;
#56675 = DIRECTION ( 'NONE',  ( 0.7071067811865475727, 0.7071067811865475727, 2.597868168706480597E-16 ) ) ;
#56676 = CARTESIAN_POINT ( 'NONE',  ( -7.250000000000000888, 7.250000000000001776, -7.500000000000000000 ) ) ;
#56677 = PLANE ( 'NONE',  #34186 ) ;
#56678 = EDGE_CURVE ( 'NONE', #43920, #55991, #58146, .T. ) ;
#56679 = AXIS2_PLACEMENT_3D ( 'NONE', #28988, #51249, #47003 ) ;
#56680 = PRESENTATION_STYLE_ASSIGNMENT (( #51026 ) ) ;
#56681 = DIRECTION ( 'NONE',  ( 0.000000000000000000, 0.000000000000000000, 1.000000000000000000 ) ) ;
#56682 = EDGE_CURVE ( 'NONE', #60969, #14935, #25189, .T. ) ;
#56683 = EDGE_LOOP ( 'NONE', ( #52748, #9192, #24072, #12663 ) ) ;
#56684 = ORIENTED_EDGE ( 'NONE', *, *, #1661, .T. ) ;
#56685 = ADVANCED_FACE ( 'NONE', ( #57789 ), #30925, .T. ) ;
#56686 = EDGE_LOOP ( 'NONE', ( #4122, #59297 ) ) ;
#56687 = ORIENTED_EDGE ( 'NONE', *, *, #16372, .F. ) ;
#56688 = CARTESIAN_POINT ( 'NONE',  ( 15.50000000000000000, -5.000000000000000000, 19.00000000000000000 ) ) ;
#56689 = EDGE_CURVE ( 'NONE', #43025, #58272, #52497, .T. ) ;
#56690 = ADVANCED_FACE ( 'NONE', ( #52865 ), #68762, .F. ) ;
#56691 = FACE_OUTER_BOUND ( 'NONE', #65150, .T. ) ;
#56692 = CARTESIAN_POINT ( 'NONE',  ( -16.75000000000000000, -0.2038245569916330158, 23.22168783648699986 ) ) ;
#56693 = ORIENTED_EDGE ( 'NONE', *, *, #7316, .F. ) ;
#56694 = ORIENTED_EDGE ( 'NONE', *, *, #21821, .F. ) ;
#56695 = ORIENTED_EDGE ( 'NONE', *, *, #10331, .F. ) ;
#56696 = LINE ( 'NONE', #44676, #11365 ) ;
#56697 = ORIENTED_EDGE ( 'NONE', *, *, #12452, .T. ) ;
#56698 = ORIENTED_EDGE ( 'NONE', *, *, #10275, .T. ) ;
#56699 = LINE ( 'NONE', #6944, #51418 ) ;
#56700 = AXIS2_PLACEMENT_3D ( 'NONE', #29237, #34889, #34191 ) ;
#56701 = VERTEX_POINT ( 'NONE', #63454 ) ;
#56702 = VERTEX_POINT ( 'NONE', #15013 ) ;
#56703 = CARTESIAN_POINT ( 'NONE',  ( 7.000000000000000000, -42.50000000000000000, -15.10000000000000142 ) ) ;
#56704 = VECTOR ( 'NONE', #46990, 1000.000000000000114 ) ;
#56706 = ORIENTED_EDGE ( 'NONE', *, *, #66098, .F. ) ;
#56705 = DIRECTION ( 'NONE',  ( -0.4999999999999913958, 0.8660254037844435926, 6.723777587268537869E-17 ) ) ;
#56707 = EDGE_LOOP ( 'NONE', ( #3159, #16536, #59893, #20971 ) ) ;
#56708 = CARTESIAN_POINT ( 'NONE',  ( -11.11351654964674118, -4.206483450353336373, 455.0000000000000568 ) ) ;
#56709 = CARTESIAN_POINT ( 'NONE',  ( 11.19368345035340440, 11.18071654964654904, 455.0000000000000568 ) ) ;
#56710 = CARTESIAN_POINT ( 'NONE',  ( -7.250000000000000888, 7.450000000000003730, -13.00000000000000178 ) ) ;
#56711 = VECTOR ( 'NONE', #13981, 1000.000000000000000 ) ;
#56713 = ORIENTED_EDGE ( 'NONE', *, *, #29288, .T. ) ;
#56712 = PLANE ( 'NONE',  #42514 ) ;
#56714 = VERTEX_POINT ( 'NONE', #58514 ) ;
#56715 = CARTESIAN_POINT ( 'NONE',  ( -9.791916549646819234, -11.08848345035330496, 195.0000000000000284 ) ) ;
#56716 = VECTOR ( 'NONE', #17116, 1000.000000000000000 ) ;
#56717 = CARTESIAN_POINT ( 'NONE',  ( 7.969523737882816761, 9.722976262117187574, 54.00000000000000711 ) ) ;
#56718 = LINE ( 'NONE', #46456, #66625 ) ;
#56719 = ORIENTED_EDGE ( 'NONE', *, *, #67903, .F. ) ;
#56720 = LINE ( 'NONE', #24899, #32614 ) ;
#56721 = EDGE_CURVE ( 'NONE', #19077, #31121, #66964, .T. ) ;
#56722 = DIRECTION ( 'NONE',  ( 0.7671651518153087546, 0.6414496315691469164, 0.000000000000000000 ) ) ;
#56723 = CIRCLE ( 'NONE', #35296, 4.500000000000191847 ) ;
#56724 = CARTESIAN_POINT ( 'NONE',  ( 8.249999999999996447, 8.250000000000001776, 5.000000000000000000 ) ) ;
#56725 = ORIENTED_EDGE ( 'NONE', *, *, #56984, .T. ) ;
#56726 = ADVANCED_FACE ( 'NONE', ( #17015 ), #46825, .F. ) ;
#56727 = CARTESIAN_POINT ( 'NONE',  ( -10.19191654964671301, 11.47551654964660450, 455.0000000000000568 ) ) ;
#56728 = AXIS2_PLACEMENT_3D ( 'NONE', #54408, #50474, #44457 ) ;
#56729 = LINE ( 'NONE', #45768, #33084 ) ;
#56730 = CARTESIAN_POINT ( 'NONE',  ( 15.00000000000000000, -25.60000000000000142, -17.60000000000000142 ) ) ;
#56731 = EDGE_LOOP ( 'NONE', ( #42346, #52809, #56432, #17061 ) ) ;
#56732 = DIRECTION ( 'NONE',  ( -1.000000000000000000, 0.000000000000000000, 0.000000000000000000 ) ) ;
#56733 = FACE_OUTER_BOUND ( 'NONE', #45017, .T. ) ;
#56734 = CIRCLE ( 'NONE', #5974, 5.250000000000000000 ) ;
#56735 = EDGE_LOOP ( 'NONE', ( #56520, #22680, #41723, #63065 ) ) ;
#56736 = DIRECTION ( 'NONE',  ( 0.000000000000000000, -0.9921567416492215186, 0.1249999999999996531 ) ) ;
#56737 = CARTESIAN_POINT ( 'NONE',  ( 11.00000000000000000, -9.199999999999999289, 12.69999999999986073 ) ) ;
#56738 = CARTESIAN_POINT ( 'NONE',  ( -10.50000000000000178, 9.690000000000001279, 0.000000000000000000 ) ) ;
#56739 = DIRECTION ( 'NONE',  ( -1.828336019306068695E-14, -1.000000000000000000, -1.836970198721044232E-16 ) ) ;
#56740 = CYLINDRICAL_SURFACE ( 'NONE', #7070, 0.2000000000000005107 ) ;
#56741 = VERTEX_POINT ( 'NONE', #41534 ) ;
#56742 = CARTESIAN_POINT ( 'NONE',  ( -30.00000000000000000, -17.14999999999900027, -26.64999999999900027 ) ) ;
#56743 = DIRECTION ( 'NONE',  ( -1.000000000000000000, 0.000000000000000000, 0.000000000000000000 ) ) ;
#56744 = VECTOR ( 'NONE', #61334, 1000.000000000000000 ) ;
#56745 = CARTESIAN_POINT ( 'NONE',  ( 7.272650909786598561, -4.201500623656122535, 455.0000000000000568 ) ) ;
#56746 = LINE ( 'NONE', #61697, #43310 ) ;
#56747 = CARTESIAN_POINT ( 'NONE',  ( 49.00000000000000000, -0.7500000000000000000, 4.943429983321300014 ) ) ;
#56748 = AXIS2_PLACEMENT_3D ( 'NONE', #23931, #7308, #18265 ) ;
#56749 = ORIENTED_EDGE ( 'NONE', *, *, #52733, .T. ) ;
#56751 = ORIENTED_EDGE ( 'NONE', *, *, #63498, .F. ) ;
#56750 = FACE_OUTER_BOUND ( 'NONE', #20737, .T. ) ;
#56752 = EDGE_CURVE ( 'NONE', #22939, #64180, #9394, .T. ) ;
#56753 = LINE ( 'NONE', #62053, #14670 ) ;
#56754 = DIRECTION ( 'NONE',  ( -0.000000000000000000, 3.673940397442059868E-16, -1.000000000000000000 ) ) ;
#56755 = ORIENTED_EDGE ( 'NONE', *, *, #47840, .F. ) ;
#56756 = AXIS2_PLACEMENT_3D ( 'NONE', #41031, #24781, #58373 ) ;
#56757 = DIRECTION ( 'NONE',  ( 1.000000000000000000, 0.000000000000000000, 0.000000000000000000 ) ) ;
#56758 = VERTEX_POINT ( 'NONE', #64169 ) ;
#56759 = ORIENTED_EDGE ( 'NONE', *, *, #23652, .T. ) ;
#56760 = EDGE_LOOP ( 'NONE', ( #69368, #55559, #69012, #53339 ) ) ;
#56761 = CARTESIAN_POINT ( 'NONE',  ( 49.00000000000000000, 13.66939075806899950, 20.80000000000000426 ) ) ;
#56762 = EDGE_CURVE ( 'NONE', #31998, #66792, #15370, .T. ) ;
#56763 = ADVANCED_FACE ( 'NONE', ( #10408 ), #5104, .F. ) ;
#56764 = CARTESIAN_POINT ( 'NONE',  ( -7.450000000000001954, 0.000000000000000000, -13.00000000000000178 ) ) ;
#56765 = DIRECTION ( 'NONE',  ( -1.000000000000000000, 0.000000000000000000, 0.000000000000000000 ) ) ;
#56766 = DIRECTION ( 'NONE',  ( -0.7671651518153105309, -0.6414496315691445849, 0.000000000000000000 ) ) ;
#56767 = AXIS2_PLACEMENT_3D ( 'NONE', #15031, #14677, #36239 ) ;
#56768 = EDGE_CURVE ( 'NONE', #43371, #2424, #54847, .T. ) ;
#56769 = ORIENTED_EDGE ( 'NONE', *, *, #41295, .T. ) ;
#56770 = VERTEX_POINT ( 'NONE', #44215 ) ;
#56771 = CARTESIAN_POINT ( 'NONE',  ( 14.25000000000000000, -2.500000000000000000, 23.22168783648699986 ) ) ;
#56772 = VECTOR ( 'NONE', #29165, 1000.000000000000000 ) ;
#56773 = CARTESIAN_POINT ( 'NONE',  ( 46.39999999999999858, 21.00000000000000000, 2.750000000000000444 ) ) ;
#56774 = ORIENTED_EDGE ( 'NONE', *, *, #47494, .F. ) ;
#56775 = VECTOR ( 'NONE', #41971, 1000.000000000000000 ) ;
#56776 = EDGE_LOOP ( 'NONE', ( #33463, #4871, #36088, #31701 ) ) ;
#56777 = ORIENTED_EDGE ( 'NONE', *, *, #22005, .F. ) ;
#56778 = FACE_OUTER_BOUND ( 'NONE', #37282, .T. ) ;
#56779 = AXIS2_PLACEMENT_3D ( 'NONE', #44113, #58999, #16211 ) ;
#56781 = ORIENTED_EDGE ( 'NONE', *, *, #68623, .F. ) ;
#56780 = LINE ( 'NONE', #17906, #34432 ) ;
#56782 = DIRECTION ( 'NONE',  ( 9.912705577010361640E-15, 1.000000000000000000, 0.000000000000000000 ) ) ;
#56783 = VECTOR ( 'NONE', #5681, 1000.000000000000000 ) ;
#56784 = DIRECTION ( 'NONE',  ( 1.000000000000000000, 0.000000000000000000, 0.000000000000000000 ) ) ;
#56785 = VERTEX_POINT ( 'NONE', #61164 ) ;
#56786 = ORIENTED_EDGE ( 'NONE', *, *, #4275, .T. ) ;
#56787 = VECTOR ( 'NONE', #23446, 1000.000000000000000 ) ;
#56788 = DIRECTION ( 'NONE',  ( 0.000000000000000000, 0.000000000000000000, 1.000000000000000000 ) ) ;
#56789 = CARTESIAN_POINT ( 'NONE',  ( -6.642976262117260333, 10.30047626211718104, 26.00000000000000711 ) ) ;
#56790 = VECTOR ( 'NONE', #15269, 1000.000000000000000 ) ;
#56791 = FACE_OUTER_BOUND ( 'NONE', #38119, .T. ) ;
#56792 = LINE ( 'NONE', #66708, #25474 ) ;
#56793 = DIRECTION ( 'NONE',  ( -1.836970198721029934E-16, -1.836970198721010706E-16, 1.000000000000000000 ) ) ;
#56795 = ORIENTED_EDGE ( 'NONE', *, *, #15059, .F. ) ;
#56794 = LINE ( 'NONE', #62093, #62693 ) ;
#56796 = EDGE_LOOP ( 'NONE', ( #17443, #26416, #34267, #6931 ) ) ;
#56797 = ADVANCED_FACE ( 'NONE', ( #2131 ), #6408, .F. ) ;
#56798 = DIRECTION ( 'NONE',  ( -1.000000000000000000, 0.000000000000000000, 0.000000000000000000 ) ) ;
#56799 = CARTESIAN_POINT ( 'NONE',  ( 13.90000000000000036, -0.000000000000000000, -20.80000000000000426 ) ) ;
#56800 = EDGE_CURVE ( 'NONE', #53367, #35322, #28306, .T. ) ;
#56801 = EDGE_CURVE ( 'NONE', #20952, #8722, #32016, .T. ) ;
#56802 = DIRECTION ( 'NONE',  ( 0.000000000000000000, 0.000000000000000000, -1.000000000000000000 ) ) ;
#56803 = DIRECTION ( 'NONE',  ( -1.000000000000000000, 0.000000000000000000, 0.000000000000000000 ) ) ;
#56804 = EDGE_CURVE ( 'NONE', #58634, #53797, #17299, .T. ) ;
#56805 = CARTESIAN_POINT ( 'NONE',  ( 31.89999999999999858, 20.60000000000000142, -13.86939075806900057 ) ) ;
#56806 = ORIENTED_EDGE ( 'NONE', *, *, #64567, .T. ) ;
#56807 = DIRECTION ( 'NONE',  ( -0.7071067811865474617, 0.7071067811865474617, 0.000000000000000000 ) ) ;
#56808 = DIRECTION ( 'NONE',  ( -0.000000000000000000, -0.000000000000000000, 1.000000000000000000 ) ) ;
#56809 = CARTESIAN_POINT ( 'NONE',  ( 55.00000000000000000, 16.96999999999999886, 21.00000000000000000 ) ) ;
#56810 = AXIS2_PLACEMENT_3D ( 'NONE', #60587, #18483, #13189 ) ;
#56811 = LINE ( 'NONE', #67777, #67637 ) ;
#56812 = LINE ( 'NONE', #35231, #62372 ) ;
#56813 = VECTOR ( 'NONE', #56907, 1000.000000000000000 ) ;
#56814 = DIRECTION ( 'NONE',  ( 1.079558018506126625E-14, 1.000000000000000000, 1.836970198721016622E-16 ) ) ;
#56815 = AXIS2_PLACEMENT_3D ( 'NONE', #6230, #17525, #28473 ) ;
#56816 = ORIENTED_EDGE ( 'NONE', *, *, #53594, .F. ) ;
#56817 = VECTOR ( 'NONE', #39302, 1000.000000000000000 ) ;
#56818 = DIRECTION ( 'NONE',  ( 0.000000000000000000, 1.000000000000000000, 0.000000000000000000 ) ) ;
#56819 = DIRECTION ( 'NONE',  ( 0.000000000000000000, 0.000000000000000000, -1.000000000000000000 ) ) ;
#56820 = VERTEX_POINT ( 'NONE', #1434 ) ;
#56821 = CARTESIAN_POINT ( 'NONE',  ( 4.456444791733522252E-16, 7.450000000000002842, -12.50000000000000000 ) ) ;
#56822 = DIRECTION ( 'NONE',  ( 1.000000000000000000, 0.000000000000000000, 0.000000000000000000 ) ) ;
#56823 = CARTESIAN_POINT ( 'NONE',  ( 12.00000000000000000, 11.18999999999999950, 0.000000000000000000 ) ) ;
#56824 = PRESENTATION_LAYER_ASSIGNMENT (  '', '', ( #11648 ) ) ;
#56825 = LINE ( 'NONE', #24662, #18400 ) ;
#56826 = CARTESIAN_POINT ( 'NONE',  ( 7.000000000000000000, -42.50000000000000000, 15.10000000000000142 ) ) ;
#56827 = ORIENTED_EDGE ( 'NONE', *, *, #64530, .F. ) ;
#56828 = CARTESIAN_POINT ( 'NONE',  ( 283.0000000000000568, -25.14575131106457917, 17.35424868893542438 ) ) ;
#56829 = ORIENTED_EDGE ( 'NONE', *, *, #44463, .F. ) ;
#56830 = DIRECTION ( 'NONE',  ( -8.339399738404099512E-15, -1.000000000000000000, 0.000000000000000000 ) ) ;
#56831 = LINE ( 'NONE', #56485, #5141 ) ;
#56832 = ORIENTED_EDGE ( 'NONE', *, *, #12381, .F. ) ;
#56833 = CARTESIAN_POINT ( 'NONE',  ( 4.406483450353420928, 11.77351654964658501, 455.0000000000000568 ) ) ;
#56834 = AXIS2_PLACEMENT_3D ( 'NONE', #48508, #20927, #27629 ) ;
#56835 = ORIENTED_EDGE ( 'NONE', *, *, #32679, .T. ) ;
#56836 = DIRECTION ( 'NONE',  ( 0.000000000000000000, 0.000000000000000000, 1.000000000000000000 ) ) ;
#56837 = VERTEX_POINT ( 'NONE', #18379 ) ;
#56838 = ORIENTED_EDGE ( 'NONE', *, *, #58222, .T. ) ;
#56839 = DIRECTION ( 'NONE',  ( 0.000000000000000000, 0.7071067811865470176, 0.7071067811865480168 ) ) ;
#56840 = ORIENTED_EDGE ( 'NONE', *, *, #39147, .F. ) ;
#56841 = ORIENTED_EDGE ( 'NONE', *, *, #15119, .T. ) ;
#56842 = ADVANCED_FACE ( 'NONE', ( #45253 ), #60137, .T. ) ;
#56843 = DIRECTION ( 'NONE',  ( -1.000000000000000000, 0.000000000000000000, 0.000000000000000000 ) ) ;
#56844 = DIRECTION ( 'NONE',  ( 1.047444401652940007E-14, 1.000000000000000000, 0.000000000000000000 ) ) ;
#56845 = DIRECTION ( 'NONE',  ( -1.000000000000000000, 0.000000000000000000, 0.000000000000000000 ) ) ;
#56846 = ADVANCED_FACE ( 'NONE', ( #33619, #23002 ), #33278, .F. ) ;
#56847 = EDGE_CURVE ( 'NONE', #67044, #44995, #12369, .T. ) ;
#56848 = ORIENTED_EDGE ( 'NONE', *, *, #64705, .F. ) ;
#56849 = DIRECTION ( 'NONE',  ( -4.121462285523435444E-16, -1.000000000000000000, 0.000000000000000000 ) ) ;
#56851 = CARTESIAN_POINT ( 'NONE',  ( 24.00000000000000000, -17.00000000000000000, 15.70499999999969809 ) ) ;
#56850 = PLANE ( 'NONE',  #47402 ) ;
#56852 = ORIENTED_EDGE ( 'NONE', *, *, #9734, .T. ) ;
#56855 = ORIENTED_EDGE ( 'NONE', *, *, #15503, .T. ) ;
#56854 = EDGE_CURVE ( 'NONE', #37495, #20667, #38921, .T. ) ;
#56853 = CARTESIAN_POINT ( 'NONE',  ( 17.89999999999999858, -14.06939075806900874, 20.80000000000001137 ) ) ;
#56856 = VERTEX_POINT ( 'NONE', #33952 ) ;
#56857 = PRODUCT_CONTEXT ( 'NONE', #46719, 'mechanical' ) ;
#56858 = EDGE_CURVE ( 'NONE', #14886, #50762, #61510, .T. ) ;
#56859 = DIRECTION ( 'NONE',  ( 0.000000000000000000, 1.000000000000000000, 0.000000000000000000 ) ) ;
#56860 = EDGE_CURVE ( 'NONE', #39038, #25974, #60481, .T. ) ;
#56861 = VERTEX_POINT ( 'NONE', #39267 ) ;
#56862 = CARTESIAN_POINT ( 'NONE',  ( -4.188533722949417282, -4.740315990920195510, 455.0000000000000568 ) ) ;
#56863 = VECTOR ( 'NONE', #18025, 1000.000000000000000 ) ;
#56864 = AXIS2_PLACEMENT_3D ( 'NONE', #34840, #40143, #62407 ) ;
#56865 = LINE ( 'NONE', #68547, #45218 ) ;
#56866 = VERTEX_POINT ( 'NONE', #60823 ) ;
#56867 = VERTEX_POINT ( 'NONE', #7078 ) ;
#56869 = DIRECTION ( 'NONE',  ( -1.836970198721029934E-16, -1.836970198721010706E-16, 1.000000000000000000 ) ) ;
#56868 = AXIS2_PLACEMENT_3D ( 'NONE', #20664, #41544, #63463 ) ;
#56870 = VECTOR ( 'NONE', #53007, 1000.000000000000000 ) ;
#56871 = LINE ( 'NONE', #57927, #57225 ) ;
#56872 = ORIENTED_EDGE ( 'NONE', *, *, #4847, .F. ) ;
#56873 = CARTESIAN_POINT ( 'NONE',  ( 30.00000000000000000, -5.000000000000000000, -11.75000000000000000 ) ) ;
#56874 = CARTESIAN_POINT ( 'NONE',  ( 11.00000000000000000, -14.33999999999999986, 14.50000000000000000 ) ) ;
#56875 = VECTOR ( 'NONE', #13120, 1000.000000000000000 ) ;
#56876 = DIRECTION ( 'NONE',  ( 0.7071067811865503483, 0.7071067811865446862, 0.000000000000000000 ) ) ;
#56877 = EDGE_LOOP ( 'NONE', ( #20181, #15640, #65472, #38365 ) ) ;
#56878 = CARTESIAN_POINT ( 'NONE',  ( -30.00000000000000000, -9.200000000000120082, 17.30000000000000071 ) ) ;
#56879 = CARTESIAN_POINT ( 'NONE',  ( 283.0000000000000568, -26.79000000000000625, 0.000000000000000000 ) ) ;
#56881 = ORIENTED_EDGE ( 'NONE', *, *, #4156, .F. ) ;
#56880 = CARTESIAN_POINT ( 'NONE',  ( -4.135079735113214916, -6.836383711243002814, 54.00000000000000711 ) ) ;
#56883 = ORIENTED_EDGE ( 'NONE', *, *, #61779, .T. ) ;
#56882 = DIRECTION ( 'NONE',  ( -1.000000000000000000, 0.000000000000000000, 0.000000000000000000 ) ) ;
#56884 = DIRECTION ( 'NONE',  ( 0.000000000000000000, 1.000000000000000000, 0.000000000000000000 ) ) ;
#56885 = CARTESIAN_POINT ( 'NONE',  ( -4.706725378239217328, 4.141586236041038482, 54.00000000000000711 ) ) ;
#56886 = LINE ( 'NONE', #8443, #5384 ) ;
#56887 = DIRECTION ( 'NONE',  ( 1.000000000000000000, -0.000000000000000000, -0.000000000000000000 ) ) ;
#56888 = CARTESIAN_POINT ( 'NONE',  ( 2.906483450353342324, -11.12648345035336916, 195.0000000000000284 ) ) ;
#56889 = ORIENTED_EDGE ( 'NONE', *, *, #62803, .F. ) ;
#56890 = LINE ( 'NONE', #18354, #57220 ) ;
#56891 = CARTESIAN_POINT ( 'NONE',  ( 40.90000000000000568, -21.00000000000000000, 13.86939075806900057 ) ) ;
#56892 = DIRECTION ( 'NONE',  ( 0.000000000000000000, 0.000000000000000000, 1.000000000000000000 ) ) ;
#56894 = ORIENTED_EDGE ( 'NONE', *, *, #24866, .T. ) ;
#56893 = CARTESIAN_POINT ( 'NONE',  ( 7.969523737882816761, 9.722976262117187574, 54.00000000000000711 ) ) ;
#56895 = PLANE ( 'NONE',  #3060 ) ;
#56896 = FACE_BOUND ( 'NONE', #20007, .T. ) ;
#56897 = ORIENTED_EDGE ( 'NONE', *, *, #60194, .T. ) ;
#56898 = ADVANCED_FACE ( 'NONE', ( #1779 ), #23357, .F. ) ;
#56899 = VERTEX_POINT ( 'NONE', #50912 ) ;
#56900 = DIRECTION ( 'NONE',  ( 4.336808689942043768E-15, 1.000000000000000000, 0.000000000000000000 ) ) ;
#56901 = CARTESIAN_POINT ( 'NONE',  ( 275.0000000000000000, -32.45000000000000995, 12.69999999999999929 ) ) ;
#56902 = ORIENTED_EDGE ( 'NONE', *, *, #69231, .F. ) ;
#56903 = PLANE ( 'NONE',  #64019 ) ;
#56904 = CARTESIAN_POINT ( 'NONE',  ( 283.0000000000000568, -26.50000000000000000, -9.080000000000000071 ) ) ;
#56905 = ADVANCED_FACE ( 'NONE', ( #66482 ), #39601, .F. ) ;
#56906 = DIRECTION ( 'NONE',  ( -0.000000000000000000, -0.000000000000000000, -1.000000000000000000 ) ) ;
#56907 = DIRECTION ( 'NONE',  ( 0.000000000000000000, 1.000000000000000000, 0.000000000000000000 ) ) ;
#56908 = AXIS2_PLACEMENT_3D ( 'NONE', #47355, #68928, #42401 ) ;
#56909 = VECTOR ( 'NONE', #51744, 1000.000000000000000 ) ;
#56910 = ORIENTED_EDGE ( 'NONE', *, *, #9244, .F. ) ;
#56911 = LINE ( 'NONE', #35335, #65522 ) ;
#56912 = ORIENTED_EDGE ( 'NONE', *, *, #48999, .T. ) ;
#56913 = CARTESIAN_POINT ( 'NONE',  ( 28.90000000000000213, 20.60000000000000142, -13.86939075806900057 ) ) ;
#56914 = EDGE_CURVE ( 'NONE', #55902, #39228, #55715, .T. ) ;
#56915 = ORIENTED_EDGE ( 'NONE', *, *, #9792, .T. ) ;
#56916 = CARTESIAN_POINT ( 'NONE',  ( 9.703773737882785966, -8.580623737882856261, 54.00000000000000711 ) ) ;
#56917 = AXIS2_PLACEMENT_3D ( 'NONE', #15291, #42849, #52064 ) ;
#56918 = AXIS2_PLACEMENT_3D ( 'NONE', #481, #37272, #22043 ) ;
#56919 = EDGE_CURVE ( 'NONE', #31900, #67199, #57274, .T. ) ;
#56920 = DIRECTION ( 'NONE',  ( -0.000000000000000000, -0.000000000000000000, -1.000000000000000000 ) ) ;
#56921 = AXIS2_PLACEMENT_3D ( 'NONE', #18055, #39621, #40332 ) ;
#56922 = CARTESIAN_POINT ( 'NONE',  ( 7.826483450353374671, 11.77351654964661876, 195.0000000000000284 ) ) ;
#56923 = ORIENTED_EDGE ( 'NONE', *, *, #29068, .F. ) ;
#56924 = VERTEX_POINT ( 'NONE', #4251 ) ;
#56925 = CARTESIAN_POINT ( 'NONE',  ( 176.4833316329832940, 9.000000000000001776, 278.4149360882130395 ) ) ;
#56926 = ORIENTED_EDGE ( 'NONE', *, *, #62437, .T. ) ;
#56927 = VERTEX_POINT ( 'NONE', #61883 ) ;
#56928 = DIRECTION ( 'NONE',  ( 0.7071067811865530128, 0.7071067811865421326, 0.000000000000000000 ) ) ;
#56929 = CARTESIAN_POINT ( 'NONE',  ( -6.817976262117261044, 9.722976262117182245, 54.00000000000000711 ) ) ;
#56930 = DIRECTION ( 'NONE',  ( 0.000000000000000000, 1.000000000000000000, 3.673940397442059868E-16 ) ) ;
#56931 = VECTOR ( 'NONE', #27859, 1000.000000000000000 ) ;
#56932 = EDGE_CURVE ( 'NONE', #53516, #12410, #46681, .T. ) ;
#56933 = CARTESIAN_POINT ( 'NONE',  ( 8.900000000000002132, 0.000000000000000000, 0.000000000000000000 ) ) ;
#56934 = VERTEX_POINT ( 'NONE', #62933 ) ;
#56935 = CIRCLE ( 'NONE', #9510, 3.500000000000000000 ) ;
#56936 = DIRECTION ( 'NONE',  ( 0.000000000000000000, 0.000000000000000000, 1.000000000000000000 ) ) ;
#56938 = CARTESIAN_POINT ( 'NONE',  ( -16.75000000000000000, -0.2038245569916330158, 23.22168783648699986 ) ) ;
#56937 = CYLINDRICAL_SURFACE ( 'NONE', #66014, 0.5249999999999990230 ) ;
#56939 = VERTEX_POINT ( 'NONE', #67543 ) ;
#56941 = VERTEX_POINT ( 'NONE', #25452 ) ;
#56940 = LINE ( 'NONE', #41733, #4838 ) ;
#56942 = ORIENTED_EDGE ( 'NONE', *, *, #53986, .F. ) ;
#56943 = ORIENTED_EDGE ( 'NONE', *, *, #5782, .T. ) ;
#56944 = EDGE_CURVE ( 'NONE', #68720, #50148, #68937, .T. ) ;
#56945 = CYLINDRICAL_SURFACE ( 'NONE', #33264, 4.500000000000188294 ) ;
#56946 = ADVANCED_FACE ( 'NONE', ( #2825 ), #52327, .F. ) ;
#56947 = CARTESIAN_POINT ( 'NONE',  ( 283.0000000000000568, -42.00000000000000000, -15.00000000000000000 ) ) ;
#56948 = ORIENTED_EDGE ( 'NONE', *, *, #4342, .T. ) ;
#56949 = ORIENTED_EDGE ( 'NONE', *, *, #60038, .T. ) ;
#56950 = CARTESIAN_POINT ( 'NONE',  ( -11.18999999999999950, -11.18999999999999950, -5.000000000000000000 ) ) ;
#56951 = DIRECTION ( 'NONE',  ( -0.7671651518153043137, 0.6414496315691521344, 2.587583378555129776E-16 ) ) ;
#56952 = EDGE_CURVE ( 'NONE', #62860, #16525, #57623, .T. ) ;
#56953 = VECTOR ( 'NONE', #62467, 1000.000000000000000 ) ;
#56954 = VERTEX_POINT ( 'NONE', #35333 ) ;
#56955 = ORIENTED_EDGE ( 'NONE', *, *, #28965, .F. ) ;
#56956 = LINE ( 'NONE', #8874, #7063 ) ;
#56957 = PLANE ( 'NONE',  #5706 ) ;
#56958 = ORIENTED_EDGE ( 'NONE', *, *, #13885, .T. ) ;
#56959 = VECTOR ( 'NONE', #36575, 1000.000000000000000 ) ;
#56960 = DIRECTION ( 'NONE',  ( 0.000000000000000000, 0.000000000000000000, -1.000000000000000000 ) ) ;
#56961 = CARTESIAN_POINT ( 'NONE',  ( -9.404046420174124066, 1.853252480934674651, 455.0000000000000568 ) ) ;
#56963 = VERTEX_POINT ( 'NONE', #67887 ) ;
#56962 = SURFACE_STYLE_USAGE ( .BOTH. , #63692 ) ;
#56964 = ORIENTED_EDGE ( 'NONE', *, *, #67563, .T. ) ;
#56965 = CARTESIAN_POINT ( 'NONE',  ( 41.09999999999999432, -14.48845687959340012, -21.00000000000000000 ) ) ;
#56966 = DIRECTION ( 'NONE',  ( 1.000000000000000000, -1.047444401652940007E-14, 0.000000000000000000 ) ) ;
#56967 = PRESENTATION_LAYER_ASSIGNMENT (  '', '', ( #5057 ) ) ;
#56968 = CARTESIAN_POINT ( 'NONE',  ( 9.562023737882764607, 2.355476262117153663, 54.00000000000000711 ) ) ;
#56969 = LINE ( 'NONE', #8182, #61726 ) ;
#56970 = CARTESIAN_POINT ( 'NONE',  ( 10.20488345035338185, -10.20488345035352928, 455.0000000000000568 ) ) ;
#56971 = EDGE_CURVE ( 'NONE', #47849, #20965, #60207, .T. ) ;
#56972 = CARTESIAN_POINT ( 'NONE',  ( 7.250000000000004441, 7.450000000000001954, -20.00000000000000000 ) ) ;
#56973 = VECTOR ( 'NONE', #48001, 1000.000000000000000 ) ;
#56974 = DIRECTION ( 'NONE',  ( 0.000000000000000000, 0.000000000000000000, 1.000000000000000000 ) ) ;
#56975 = EDGE_LOOP ( 'NONE', ( #63142, #59195, #55292, #39154 ) ) ;
#56976 = CARTESIAN_POINT ( 'NONE',  ( -9.390476262117259054, 1.466476262117183182, 54.00000000000000711 ) ) ;
#56977 = EDGE_CURVE ( 'NONE', #9070, #69553, #52689, .T. ) ;
#56979 = ORIENTED_EDGE ( 'NONE', *, *, #63702, .T. ) ;
#56978 = FACE_OUTER_BOUND ( 'NONE', #3299, .T. ) ;
#56980 = CARTESIAN_POINT ( 'NONE',  ( 275.0000000000000000, -20.40000000000000213, 17.60000000000000142 ) ) ;
#56981 = VECTOR ( 'NONE', #222, 1000.000000000000000 ) ;
#56982 = CARTESIAN_POINT ( 'NONE',  ( -9.897976262117259338, 6.642976262117183950, 54.00000000000000711 ) ) ;
#56984 = EDGE_CURVE ( 'NONE', #17866, #13194, #47363, .T. ) ;
#56983 = CARTESIAN_POINT ( 'NONE',  ( 29.25000000000000000, -5.200000000000001066, -26.25000000000000000 ) ) ;
#56985 = AXIS2_PLACEMENT_3D ( 'NONE', #53065, #14515, #36431 ) ;
#56986 = LINE ( 'NONE', #18814, #3593 ) ;
#56987 = DIRECTION ( 'NONE',  ( -1.000000000000000000, 0.000000000000000000, 0.000000000000000000 ) ) ;
#56988 = EDGE_CURVE ( 'NONE', #13299, #43994, #64713, .T. ) ;
#56989 = ORIENTED_EDGE ( 'NONE', *, *, #57099, .F. ) ;
#56990 = CARTESIAN_POINT ( 'NONE',  ( 283.0000000000000568, -32.44999999999905071, 12.69999999999999929 ) ) ;
#56991 = CARTESIAN_POINT ( 'NONE',  ( 10.00000000000000000, -21.00000000000000000, -18.00000000000000355 ) ) ;
#56992 = ORIENTED_EDGE ( 'NONE', *, *, #41468, .F. ) ;
#56993 = DIRECTION ( 'NONE',  ( -1.000000000000000000, 0.000000000000000000, 0.000000000000000000 ) ) ;
#56994 = EDGE_CURVE ( 'NONE', #65332, #53236, #62222, .T. ) ;
#56995 = CYLINDRICAL_SURFACE ( 'NONE', #46576, 1.929199999999998028 ) ;
#56996 = VERTEX_POINT ( 'NONE', #40308 ) ;
#56997 = CARTESIAN_POINT ( 'NONE',  ( 30.00000000000000000, -13.54524521594299991, 17.53999999999999915 ) ) ;
#56998 = ORIENTED_EDGE ( 'NONE', *, *, #22071, .F. ) ;
#56999 = EDGE_CURVE ( 'NONE', #22725, #19628, #12740, .T. ) ;
#57000 = AXIS2_PLACEMENT_3D ( 'NONE', #15213, #27217, #33874 ) ;
#57001 = ORIENTED_EDGE ( 'NONE', *, *, #15594, .F. ) ;
#57002 = EDGE_CURVE ( 'NONE', #63059, #59074, #30843, .T. ) ;
#57003 = CARTESIAN_POINT ( 'NONE',  ( 30.00000000000000000, -17.14999999999900027, -26.64999999999900027 ) ) ;
#57004 = CARTESIAN_POINT ( 'NONE',  ( 6.832023737882815695, 9.897976262117191837, 54.00000000000000711 ) ) ;
#57005 = CARTESIAN_POINT ( 'NONE',  ( 7.250000000000005329, -7.449999999999998401, -15.00000000000000000 ) ) ;
#57006 = EDGE_CURVE ( 'NONE', #65979, #69122, #8263, .T. ) ;
#57007 = AXIS2_PLACEMENT_3D ( 'NONE', #6822, #28392, #39355 ) ;
#57008 = EDGE_CURVE ( 'NONE', #5664, #57882, #30759, .T. ) ;
#57009 = EDGE_CURVE ( 'NONE', #53333, #62865, #51260, .T. ) ;
#57010 = CARTESIAN_POINT ( 'NONE',  ( 13.90000000000000213, -21.00000000000000000, 13.86939075806900057 ) ) ;
#57011 = CARTESIAN_POINT ( 'NONE',  ( -7.955476262117317177, -8.835729544836295801, 54.00000000000000711 ) ) ;
#57012 = ORIENTED_EDGE ( 'NONE', *, *, #57933, .F. ) ;
#57013 = ORIENTED_EDGE ( 'NONE', *, *, #67945, .T. ) ;
#57015 = ORIENTED_EDGE ( 'NONE', *, *, #31873, .T. ) ;
#57014 = CARTESIAN_POINT ( 'NONE',  ( 30.00000000000000000, -5.200000000000001066, 26.59999999999999787 ) ) ;
#57016 = EDGE_CURVE ( 'NONE', #30915, #34406, #41707, .T. ) ;
#57017 = ORIENTED_EDGE ( 'NONE', *, *, #7426, .F. ) ;
#57018 = CIRCLE ( 'NONE', #50253, 0.1749999999999998224 ) ;
#57019 = CYLINDRICAL_SURFACE ( 'NONE', #68743, 2.204799999999997873 ) ;
#57020 = CARTESIAN_POINT ( 'NONE',  ( 7.250000000000005329, -7.249999999999998224, -25.50000000000000355 ) ) ;
#57021 = LINE ( 'NONE', #8582, #54966 ) ;
#57022 = AXIS2_PLACEMENT_3D ( 'NONE', #29716, #52354, #67202 ) ;
#57023 = EDGE_CURVE ( 'NONE', #41828, #35896, #54628, .T. ) ;
#57024 = CARTESIAN_POINT ( 'NONE',  ( -9.828310488886053520, 1.677516549646603794, 455.0000000000000568 ) ) ;
#57025 = LINE ( 'NONE', #8585, #67220 ) ;
#57026 = STYLED_ITEM ( 'NONE', ( #42245 ), #67347 ) ;
#57027 = CARTESIAN_POINT ( 'NONE',  ( -7.250000000000000000, -7.449999999999998401, -19.00000000000000000 ) ) ;
#57028 = ORIENTED_EDGE ( 'NONE', *, *, #2650, .F. ) ;
#57029 = EDGE_LOOP ( 'NONE', ( #69363, #45029, #69081, #9466 ) ) ;
#57030 = ORIENTED_EDGE ( 'NONE', *, *, #38282, .F. ) ;
#57031 = ORIENTED_EDGE ( 'NONE', *, *, #51847, .F. ) ;
#57032 = DIRECTION ( 'NONE',  ( 0.7071067811865446862, 0.7071067811865503483, 0.000000000000000000 ) ) ;
#57033 = ADVANCED_FACE ( 'NONE', ( #57973 ), #9541, .F. ) ;
#57034 = LINE ( 'NONE', #15310, #50153 ) ;
#57035 = ADVANCED_FACE ( 'NONE', ( #63640 ), #69283, .F. ) ;
#57036 = VECTOR ( 'NONE', #566, 1000.000000000000000 ) ;
#57037 = DIRECTION ( 'NONE',  ( -1.000000000000000000, 0.000000000000000000, 0.000000000000000000 ) ) ;
#57038 = ORIENTED_EDGE ( 'NONE', *, *, #44879, .F. ) ;
#57039 = ORIENTED_EDGE ( 'NONE', *, *, #44412, .F. ) ;
#57040 = ORIENTED_EDGE ( 'NONE', *, *, #53604, .T. ) ;
#57041 =( GEOMETRIC_REPRESENTATION_CONTEXT ( 3 ) GLOBAL_UNCERTAINTY_ASSIGNED_CONTEXT ( ( #31681 ) ) GLOBAL_UNIT_ASSIGNED_CONTEXT ( ( #38648, #11757, #44281 ) ) REPRESENTATION_CONTEXT ( 'NONE', 'WORKASPACE' ) );
#57042 = CARTESIAN_POINT ( 'NONE',  ( -30.00000000000000000, -16.28999999999710369, -15.00000000000794920 ) ) ;
#57043 = ORIENTED_EDGE ( 'NONE', *, *, #58635, .F. ) ;
#57044 = ORIENTED_EDGE ( 'NONE', *, *, #35860, .F. ) ;
#57045 = DIRECTION ( 'NONE',  ( 9.912705577010336396E-15, 1.000000000000000000, 0.000000000000000000 ) ) ;
#57046 = ORIENTED_EDGE ( 'NONE', *, *, #32561, .F. ) ;
#57047 = VERTEX_POINT ( 'NONE', #43441 ) ;
#57048 = CARTESIAN_POINT ( 'NONE',  ( 71.47321854994621049, 47.95351654967443977, 39.00000000000000000 ) ) ;
#57050 = ORIENTED_EDGE ( 'NONE', *, *, #69088, .T. ) ;
#57049 = DIRECTION ( 'NONE',  ( -0.000000000000000000, 1.000000000000000000, -0.000000000000000000 ) ) ;
#57051 = ORIENTED_EDGE ( 'NONE', *, *, #24205, .F. ) ;
#57052 = FACE_OUTER_BOUND ( 'NONE', #53510, .T. ) ;
#57053 = EDGE_CURVE ( 'NONE', #61584, #64098, #4936, .T. ) ;
#57054 = LINE ( 'NONE', #24544, #20514 ) ;
#57055 = CARTESIAN_POINT ( 'NONE',  ( -17.00000000000000000, -16.28999999999710369, -15.00000000000794920 ) ) ;
#57057 = ORIENTED_EDGE ( 'NONE', *, *, #47921, .F. ) ;
#57056 = CARTESIAN_POINT ( 'NONE',  ( 7.000000000000000000, -23.70411739045900390, -12.50000000000000000 ) ) ;
#57058 = ORIENTED_EDGE ( 'NONE', *, *, #5996, .F. ) ;
#57059 = LINE ( 'NONE', #24892, #47940 ) ;
#57060 = VECTOR ( 'NONE', #61081, 1000.000000000000000 ) ;
#57061 = DIRECTION ( 'NONE',  ( -1.062171939662868407E-14, -1.000000000000000000, 0.000000000000000000 ) ) ;
#57062 = CARTESIAN_POINT ( 'NONE',  ( 0.5000000000000000000, -21.00000000000000000, 18.00000000000000355 ) ) ;
#57063 = CARTESIAN_POINT ( 'NONE',  ( 11.00000000000000000, -5.200000000000001066, 9.400000000000000355 ) ) ;
#57064 = VECTOR ( 'NONE', #61072, 1000.000000000000000 ) ;
#57065 = VERTEX_POINT ( 'NONE', #58682 ) ;
#57066 = CARTESIAN_POINT ( 'NONE',  ( -4.393516549646835578, -11.78648345035344214, 455.0000000000000568 ) ) ;
#57067 = EDGE_CURVE ( 'NONE', #22518, #43019, #24115, .T. ) ;
#57068 = VECTOR ( 'NONE', #51840, 1000.000000000000000 ) ;
#57069 = CIRCLE ( 'NONE', #36806, 1.000000000000003553 ) ;
#57071 = CARTESIAN_POINT ( 'NONE',  ( 6.006483450353401921, 5.993516549646582092, 455.0000000000000568 ) ) ;
#57070 = VECTOR ( 'NONE', #46783, 1000.000000000000000 ) ;
#57072 = DIRECTION ( 'NONE',  ( -0.000000000000000000, -0.000000000000000000, -1.000000000000000000 ) ) ;
#57073 = ORIENTED_EDGE ( 'NONE', *, *, #20460, .F. ) ;
#57075 = EDGE_CURVE ( 'NONE', #39920, #18785, #34244, .T. ) ;
#57074 = DIRECTION ( 'NONE',  ( 0.000000000000000000, 0.000000000000000000, -1.000000000000000000 ) ) ;
#57076 = FACE_OUTER_BOUND ( 'NONE', #61129, .T. ) ;
#57077 = VECTOR ( 'NONE', #9112, 1000.000000000000000 ) ;
#57078 = CIRCLE ( 'NONE', #7345, 1.929199999999998028 ) ;
#57079 = CARTESIAN_POINT ( 'NONE',  ( 275.0000000000000000, -23.65000000000000568, -12.40000000000000213 ) ) ;
#57080 = EDGE_CURVE ( 'NONE', #40165, #32104, #69646, .T. ) ;
#57081 = ORIENTED_EDGE ( 'NONE', *, *, #20920, .F. ) ;
#57082 = VECTOR ( 'NONE', #32790, 1000.000000000000000 ) ;
#57083 = DIRECTION ( 'NONE',  ( 8.903847840905249551E-15, 1.000000000000000000, 0.000000000000000000 ) ) ;
#57084 = EDGE_CURVE ( 'NONE', #41334, #27705, #23958, .T. ) ;
#57085 = CARTESIAN_POINT ( 'NONE',  ( 14.50000000000000000, -42.00000000000000000, -27.00000000000000000 ) ) ;
#57086 = PRESENTATION_LAYER_ASSIGNMENT (  '', '', ( #67230 ) ) ;
#57087 = CARTESIAN_POINT ( 'NONE',  ( 7.250000000000004441, 7.450000000000001954, -23.50000000000000000 ) ) ;
#57088 = ORIENTED_EDGE ( 'NONE', *, *, #13240, .T. ) ;
#57089 = CARTESIAN_POINT ( 'NONE',  ( 7.250000000000004441, 7.450000000000001954, -20.50000000000000000 ) ) ;
#57090 = CARTESIAN_POINT ( 'NONE',  ( -29.50000000000000355, -11.50000000000000000, -15.00000000000000000 ) ) ;
#57091 = CARTESIAN_POINT ( 'NONE',  ( -7.250000000000000888, 8.250000000000001776, -26.00000000000001066 ) ) ;
#57092 =( GEOMETRIC_REPRESENTATION_CONTEXT ( 3 ) GLOBAL_UNCERTAINTY_ASSIGNED_CONTEXT ( ( #32374 ) ) GLOBAL_UNIT_ASSIGNED_CONTEXT ( ( #37190, #42823, #22647 ) ) REPRESENTATION_CONTEXT ( 'NONE', 'WORKASPACE' ) );
#57093 = LINE ( 'NONE', #46480, #35820 ) ;
#57094 = CARTESIAN_POINT ( 'NONE',  ( 7.250000000000005329, 7.250000000000000888, -19.50000000000000000 ) ) ;
#57095 = VERTEX_POINT ( 'NONE', #64334 ) ;
#57096 = DIRECTION ( 'NONE',  ( 1.000000000000000000, -0.000000000000000000, -0.000000000000000000 ) ) ;
#57097 = CARTESIAN_POINT ( 'NONE',  ( 2.500000000000000000, 3.061616997868383141E-16, -29.90000000000000924 ) ) ;
#57098 = CARTESIAN_POINT ( 'NONE',  ( 29.50000000000000355, -11.50000000000000000, -19.00000000000000000 ) ) ;
#57099 = EDGE_CURVE ( 'NONE', #13987, #9996, #21539, .T. ) ;
#57100 = FILL_AREA_STYLE ('',( #7612 ) ) ;
#57101 = CARTESIAN_POINT ( 'NONE',  ( -29.50000000000000355, -11.50000000000100009, 15.00000000000084910 ) ) ;
#57102 = ORIENTED_EDGE ( 'NONE', *, *, #65886, .T. ) ;
#57104 = EDGE_LOOP ( 'NONE', ( #16893, #56489, #11437, #11322 ) ) ;
#57103 = CARTESIAN_POINT ( 'NONE',  ( -8.079219948824906794, 8.697938382363059162, 54.00000000000000711 ) ) ;
#57105 = CARTESIAN_POINT ( 'NONE',  ( 7.000000000000000000, -20.50000000000000000, 13.00000000000000178 ) ) ;
#57106 = CARTESIAN_POINT ( 'NONE',  ( 283.0000000000000568, -38.64999999999999858, -12.69999999999999929 ) ) ;
#57107 = DIRECTION ( 'NONE',  ( 0.000000000000000000, 1.000000000000000000, 0.000000000000000000 ) ) ;
#57108 = ORIENTED_EDGE ( 'NONE', *, *, #59586, .T. ) ;
#57109 = VECTOR ( 'NONE', #24201, 1000.000000000000000 ) ;
#57110 = DIRECTION ( 'NONE',  ( -1.000000000000000000, 0.000000000000000000, 0.000000000000000000 ) ) ;
#57111 = VECTOR ( 'NONE', #49389, 1000.000000000000000 ) ;
#57112 = VERTEX_POINT ( 'NONE', #53038 ) ;
#57113 = VECTOR ( 'NONE', #34121, 1000.000000000000000 ) ;
#57114 = ORIENTED_EDGE ( 'NONE', *, *, #39815, .F. ) ;
#57115 = EDGE_LOOP ( 'NONE', ( #31870, #50250, #49139, #32618 ) ) ;
#57116 = FACE_BOUND ( 'NONE', #32514, .T. ) ;
#57117 = ADVANCED_FACE ( 'NONE', ( #32150 ), #10931, .F. ) ;
#57118 = CARTESIAN_POINT ( 'NONE',  ( 6.849523737882818430, 10.49297626211719603, 54.00000000000000711 ) ) ;
#57119 = DIRECTION ( 'NONE',  ( -0.000000000000000000, -0.000000000000000000, 1.000000000000000000 ) ) ;
#57121 = EDGE_CURVE ( 'NONE', #36500, #38962, #18448, .T. ) ;
#57120 = CYLINDRICAL_SURFACE ( 'NONE', #21094, 0.1999999999999987899 ) ;
#57122 = CIRCLE ( 'NONE', #4043, 24.99999999998789946 ) ;
#57123 = AXIS2_PLACEMENT_3D ( 'NONE', #22138, #44034, #16485 ) ;
#57124 = EDGE_LOOP ( 'NONE', ( #64047, #17076, #37146, #28144 ) ) ;
#57126 = EDGE_CURVE ( 'NONE', #56856, #54703, #59022, .T. ) ;
#57125 = VERTEX_POINT ( 'NONE', #20837 ) ;
#57127 = PLANE ( 'NONE',  #42557 ) ;
#57128 = CYLINDRICAL_SURFACE ( 'NONE', #5676, 0.5000000000001374456 ) ;
#57129 = AXIS2_PLACEMENT_3D ( 'NONE', #14718, #57845, #59247 ) ;
#57130 = CIRCLE ( 'NONE', #43557, 2.458500000000000796 ) ;
#57131 = ORIENTED_EDGE ( 'NONE', *, *, #41069, .T. ) ;
#57132 = ORIENTED_EDGE ( 'NONE', *, *, #42496, .T. ) ;
#57133 = ORIENTED_EDGE ( 'NONE', *, *, #17825, .F. ) ;
#57134 = VERTEX_POINT ( 'NONE', #32510 ) ;
#57135 = CIRCLE ( 'NONE', #53778, 1.000000000000000888 ) ;
#57136 = CARTESIAN_POINT ( 'NONE',  ( 30.00000000000000000, -8.959999999999999076, 17.04524521594300523 ) ) ;
#57138 = ORIENTED_EDGE ( 'NONE', *, *, #45135, .T. ) ;
#57137 = CARTESIAN_POINT ( 'NONE',  ( 7.000000000000000000, -27.13000000000000611, 13.50000000000000000 ) ) ;
#57139 = CARTESIAN_POINT ( 'NONE',  ( -8.249999999999996447, 8.250000000000001776, -5.000000000000000000 ) ) ;
#57140 = PRODUCT ( 'Part3', 'Part3', '', ( #35636 ) ) ;
#57141 =( GEOMETRIC_REPRESENTATION_CONTEXT ( 3 ) GLOBAL_UNCERTAINTY_ASSIGNED_CONTEXT ( ( #3396 ) ) GLOBAL_UNIT_ASSIGNED_CONTEXT ( ( #31112, #4243, #58336 ) ) REPRESENTATION_CONTEXT ( 'NONE', 'WORKASPACE' ) );
#57142 = DIRECTION ( 'NONE',  ( -1.000000000000000000, 0.000000000000000000, 0.000000000000000000 ) ) ;
#57143 = ORIENTED_EDGE ( 'NONE', *, *, #38427, .T. ) ;
#57144 = AXIS2_PLACEMENT_3D ( 'NONE', #43784, #16574, #32821 ) ;
#57145 = EDGE_LOOP ( 'NONE', ( #62769, #47984, #60179, #31593 ) ) ;
#57146 = DIRECTION ( 'NONE',  ( -1.000000000000000000, 0.000000000000000000, 0.000000000000000000 ) ) ;
#57147 = CARTESIAN_POINT ( 'NONE',  ( -15.50000000000129852, -15.50000000000000000, -22.50000000000000000 ) ) ;
#57148 = DIRECTION ( 'NONE',  ( -1.000000000000000000, 0.000000000000000000, 0.000000000000000000 ) ) ;
#57149 = ADVANCED_FACE ( 'NONE', ( #63998 ), #4593, .T. ) ;
#57150 = DIRECTION ( 'NONE',  ( -0.000000000000000000, 1.000000000000000000, -0.000000000000000000 ) ) ;
#57151 = DIRECTION ( 'NONE',  ( 1.000000000000000000, 3.016910393003147986E-15, 1.108394896831706469E-30 ) ) ;
#57152 = ORIENTED_EDGE ( 'NONE', *, *, #27796, .T. ) ;
#57153 = VERTEX_POINT ( 'NONE', #10578 ) ;
#57154 = DIRECTION ( 'NONE',  ( 1.000000000000000000, 0.000000000000000000, 0.000000000000000000 ) ) ;
#57155 = LINE ( 'NONE', #14014, #13256 ) ;
#57156 = CARTESIAN_POINT ( 'NONE',  ( -6.606374702650169795, 7.252248008019353875, 455.0000000000000568 ) ) ;
#57157 = AXIS2_PLACEMENT_3D ( 'NONE', #1889, #34388, #67293 ) ;
#57158 = LINE ( 'NONE', #63165, #15580 ) ;
#57159 = ADVANCED_FACE ( 'NONE', ( #26861 ), #54423, .F. ) ;
#57160 = ADVANCED_FACE ( 'NONE', ( #59370 ), #48420, .F. ) ;
#57161 = VECTOR ( 'NONE', #3358, 1000.000000000000000 ) ;
#57162 = LINE ( 'NONE', #3083, #63619 ) ;
#57164 = ORIENTED_EDGE ( 'NONE', *, *, #22784, .T. ) ;
#57163 = EDGE_CURVE ( 'NONE', #341, #13015, #36544, .T. ) ;
#57165 = DIRECTION ( 'NONE',  ( -1.836970198721029934E-16, 1.836970198721036344E-16, -1.000000000000000000 ) ) ;
#57166 = EDGE_CURVE ( 'NONE', #54732, #27591, #59716, .T. ) ;
#57167 = CYLINDRICAL_SURFACE ( 'NONE', #30475, 4.000000000000000000 ) ;
#57168 = LINE ( 'NONE', #58220, #37827 ) ;
#57169 = CARTESIAN_POINT ( 'NONE',  ( 151.5599459900709860, -10.00000000000000178, 278.4149360882130395 ) ) ;
#57170 = VECTOR ( 'NONE', #61929, 1000.000000000000000 ) ;
#57171 = AXIS2_PLACEMENT_3D ( 'NONE', #6059, #54158, #10660 ) ;
#57172 = AXIS2_PLACEMENT_3D ( 'NONE', #32885, #37848, #59415 ) ;
#57173 = ADVANCED_FACE ( 'NONE', ( #22243 ), #43801, .T. ) ;
#57174 = CARTESIAN_POINT ( 'NONE',  ( -7.342976262117259623, 3.834182069070703580, 54.00000000000000711 ) ) ;
#57175 = DIRECTION ( 'NONE',  ( 0.000000000000000000, 0.000000000000000000, -1.000000000000000000 ) ) ;
#57176 = VECTOR ( 'NONE', #40374, 1000.000000000000000 ) ;
#57177 = VECTOR ( 'NONE', #46682, 1000.000000000000000 ) ;
#57178 = CARTESIAN_POINT ( 'NONE',  ( -7.250000000000000888, -8.249999999999998224, -26.00000000000001066 ) ) ;
#57179 = EDGE_LOOP ( 'NONE', ( #54882, #48909, #66779, #22464 ) ) ;
#57180 = CARTESIAN_POINT ( 'NONE',  ( 3.848229544836329730, 7.342976262117204556, 54.00000000000000711 ) ) ;
#57181 = CARTESIAN_POINT ( 'NONE',  ( 10.09643294401457858, 9.093516549646567526, 455.0000000000000568 ) ) ;
#57182 = ORIENTED_EDGE ( 'NONE', *, *, #42243, .F. ) ;
#57183 = DIRECTION ( 'NONE',  ( 8.673617379884087537E-15, 1.000000000000000000, 0.000000000000000000 ) ) ;
#57184 = DIRECTION ( 'NONE',  ( -0.000000000000000000, 3.673940397442059868E-16, -1.000000000000000000 ) ) ;
#57185 = AXIS2_PLACEMENT_3D ( 'NONE', #35841, #43144, #64720 ) ;
#57186 = CARTESIAN_POINT ( 'NONE',  ( -17.00000000000000000, -17.00000000000000000, -15.70499999999969809 ) ) ;
#57187 = DIRECTION ( 'NONE',  ( -0.000000000000000000, -0.000000000000000000, -1.000000000000000000 ) ) ;
#57188 = FACE_OUTER_BOUND ( 'NONE', #18839, .T. ) ;
#57189 = VERTEX_POINT ( 'NONE', #22582 ) ;
#57190 = CARTESIAN_POINT ( 'NONE',  ( 31.89999999999999858, 0.000000000000000000, 2.458500000000000796 ) ) ;
#57191 = VECTOR ( 'NONE', #34552, 1000.000000000000000 ) ;
#57192 = VERTEX_POINT ( 'NONE', #12635 ) ;
#57193 = CARTESIAN_POINT ( 'NONE',  ( 40.90000000000000568, -21.00000000000000000, -16.96999999999999886 ) ) ;
#57194 = DIRECTION ( 'NONE',  ( 0.000000000000000000, 0.000000000000000000, 1.000000000000000000 ) ) ;
#57195 = ORIENTED_EDGE ( 'NONE', *, *, #67993, .F. ) ;
#57196 = DIRECTION ( 'NONE',  ( 0.000000000000000000, 1.000000000000000000, 0.000000000000000000 ) ) ;
#57197 = EDGE_LOOP ( 'NONE', ( #5424, #22202, #7642, #23390, #44279, #66914, #5639 ) ) ;
#57198 = CARTESIAN_POINT ( 'NONE',  ( -6.606374702650211539, -7.265214908726115972, 195.0000000000000284 ) ) ;
#57199 = ORIENTED_EDGE ( 'NONE', *, *, #19604, .T. ) ;
#57200 = ORIENTED_EDGE ( 'NONE', *, *, #18591, .T. ) ;
#57201 = DIRECTION ( 'NONE',  ( 1.000000000000000000, -5.120954910632640039E-15, 0.000000000000000000 ) ) ;
#57202 = ORIENTED_EDGE ( 'NONE', *, *, #55542, .T. ) ;
#57203 = ORIENTED_EDGE ( 'NONE', *, *, #47635, .T. ) ;
#57204 = DIRECTION ( 'NONE',  ( 0.000000000000000000, 3.673940397442059868E-16, -1.000000000000000000 ) ) ;
#57205 = LINE ( 'NONE', #18310, #22323 ) ;
#57206 = FACE_OUTER_BOUND ( 'NONE', #35607, .T. ) ;
#57207 = CIRCLE ( 'NONE', #41408, 9.300000000000002487 ) ;
#57208 = ORIENTED_EDGE ( 'NONE', *, *, #7653, .F. ) ;
#57209 = EDGE_CURVE ( 'NONE', #43309, #17252, #52351, .T. ) ;
#57210 = CARTESIAN_POINT ( 'NONE',  ( 9.900000000000000355, 14.08845687959340331, 21.00000000000000000 ) ) ;
#57211 = EDGE_CURVE ( 'NONE', #28902, #21463, #51216, .T. ) ;
#57213 = FACE_OUTER_BOUND ( 'NONE', #66250, .T. ) ;
#57212 = DIRECTION ( 'NONE',  ( 0.000000000000000000, 0.000000000000000000, 1.000000000000000000 ) ) ;
#57214 = ORIENTED_EDGE ( 'NONE', *, *, #58859, .F. ) ;
#57216 = VERTEX_POINT ( 'NONE', #39183 ) ;
#57215 = CARTESIAN_POINT ( 'NONE',  ( 0.000000000000000000, 0.000000000000000000, -30.00000000000001066 ) ) ;
#57217 = VECTOR ( 'NONE', #28750, 1000.000000000000000 ) ;
#57218 = ORIENTED_EDGE ( 'NONE', *, *, #58852, .F. ) ;
#57219 = EDGE_CURVE ( 'NONE', #44331, #361, #61195, .T. ) ;
#57220 = VECTOR ( 'NONE', #17682, 1000.000000000000000 ) ;
#57221 = CARTESIAN_POINT ( 'NONE',  ( 39.00000000000000000, 16.96999999999999886, 21.00000000000000000 ) ) ;
#57223 = ORIENTED_EDGE ( 'NONE', *, *, #57692, .F. ) ;
#57222 = DIRECTION ( 'NONE',  ( 0.000000000000000000, 1.000000000000000000, 0.000000000000000000 ) ) ;
#57224 = VECTOR ( 'NONE', #32055, 1000.000000000000000 ) ;
#57225 = VECTOR ( 'NONE', #9493, 1000.000000000000000 ) ;
#57226 = LINE ( 'NONE', #25054, #68705 ) ;
#57227 = FACE_OUTER_BOUND ( 'NONE', #56483, .T. ) ;
#57228 = VERTEX_POINT ( 'NONE', #60057 ) ;
#57229 = ORIENTED_EDGE ( 'NONE', *, *, #51079, .F. ) ;
#57230 = VECTOR ( 'NONE', #742, 1000.000000000000000 ) ;
#57231 = AXIS2_PLACEMENT_3D ( 'NONE', #40331, #7789, #2840 ) ;
#57232 = CARTESIAN_POINT ( 'NONE',  ( 0.000000000000000000, 0.000000000000000000, -18.50000000000000000 ) ) ;
#57233 = VERTEX_POINT ( 'NONE', #65378 ) ;
#57234 = DIRECTION ( 'NONE',  ( -1.000000000000000000, 0.000000000000000000, 0.000000000000000000 ) ) ;
#57236 = DIRECTION ( 'NONE',  ( -0.000000000000000000, -0.000000000000000000, -1.000000000000000000 ) ) ;
#57235 = VECTOR ( 'NONE', #38131, 1000.000000000000000 ) ;
#57237 = LINE ( 'NONE', #46270, #7981 ) ;
#57238 = ORIENTED_EDGE ( 'NONE', *, *, #69160, .F. ) ;
#57239 = CIRCLE ( 'NONE', #23317, 3.500000000000003109 ) ;
#57240 = CARTESIAN_POINT ( 'NONE',  ( 275.0000000000000000, -25.50000000000000355, -17.00000000000000000 ) ) ;
#57241 = CARTESIAN_POINT ( 'NONE',  ( -25.50000000000000355, -5.578999999999999737, -20.87899999999999778 ) ) ;
#57243 = EDGE_LOOP ( 'NONE', ( #35364, #60678, #51849, #17747 ) ) ;
#57242 = FILL_AREA_STYLE ('',( #40624 ) ) ;
#57245 = EDGE_LOOP ( 'NONE', ( #69229, #53732, #19285, #7702, #7540, #61296, #11117, #43728, #63749, #44202, #34071 ) ) ;
#57244 = CARTESIAN_POINT ( 'NONE',  ( -2.617976262117293285, -6.501044194225502615, 54.00000000000000711 ) ) ;
#57246 = DIRECTION ( 'NONE',  ( 0.000000000000000000, 0.000000000000000000, 1.000000000000000000 ) ) ;
#57247 = CARTESIAN_POINT ( 'NONE',  ( 41.09999999999999432, -21.00000000000000000, -13.86939075806900057 ) ) ;
#57248 = DIRECTION ( 'NONE',  ( -0.000000000000000000, -0.000000000000000000, 1.000000000000000000 ) ) ;
#57249 = LINE ( 'NONE', #3512, #33905 ) ;
#57250 = DIRECTION ( 'NONE',  ( 0.000000000000000000, 0.000000000000000000, 1.000000000000000000 ) ) ;
#57251 = EDGE_LOOP ( 'NONE', ( #37814, #28498, #56187, #1770, #306 ) ) ;
#57252 = LINE ( 'NONE', #36745, #52757 ) ;
#57253 = EDGE_CURVE ( 'NONE', #31525, #28725, #66403, .T. ) ;
#57254 = CARTESIAN_POINT ( 'NONE',  ( -7.250000000000000000, -7.449999999999998401, -8.500000000000000000 ) ) ;
#57255 = CARTESIAN_POINT ( 'NONE',  ( -11.07551654964667520, 10.19191654964664018, 455.0000000000000568 ) ) ;
#57257 = EDGE_LOOP ( 'NONE', ( #53501, #6424, #56262, #48972 ) ) ;
#57256 = DIRECTION ( 'NONE',  ( 0.000000000000000000, -1.000000000000000000, 0.000000000000000000 ) ) ;
#57258 = DIRECTION ( 'NONE',  ( 1.836970198721029934E-16, -1.836970198721036344E-16, 1.000000000000000000 ) ) ;
#57259 = EDGE_CURVE ( 'NONE', #38565, #48363, #60388, .T. ) ;
#57260 = EDGE_CURVE ( 'NONE', #55613, #40627, #6657, .T. ) ;
#57261 = VECTOR ( 'NONE', #40986, 1000.000000000000000 ) ;
#57262 = CARTESIAN_POINT ( 'NONE',  ( -4.188533722949374649, -7.272650909786617213, 195.0000000000000284 ) ) ;
#57263 = ORIENTED_EDGE ( 'NONE', *, *, #35365, .F. ) ;
#57264 = DIRECTION ( 'NONE',  ( 0.000000000000000000, 1.000000000000000000, 0.000000000000000000 ) ) ;
#57265 = DIRECTION ( 'NONE',  ( 0.000000000000000000, 1.000000000000000000, 0.000000000000000000 ) ) ;
#57266 = VERTEX_POINT ( 'NONE', #33532 ) ;
#57267 = CARTESIAN_POINT ( 'NONE',  ( 8.250000000000005329, 8.250000000000001776, -26.00000000000001066 ) ) ;
#57268 = AXIS2_PLACEMENT_3D ( 'NONE', #56878, #58300, #9503 ) ;
#57269 = DIRECTION ( 'NONE',  ( 0.000000000000000000, -0.7046037717806115097, -0.7096009616626348659 ) ) ;
#57270 = DIRECTION ( 'NONE',  ( 1.000000000000000000, 0.000000000000000000, 0.000000000000000000 ) ) ;
#57271 = EDGE_CURVE ( 'NONE', #44739, #37577, #11946, .T. ) ;
#57272 = AXIS2_PLACEMENT_3D ( 'NONE', #57003, #52061, #18126 ) ;
#57274 = LINE ( 'NONE', #24749, #50056 ) ;
#57273 = AXIS2_PLACEMENT_3D ( 'NONE', #44010, #32716, #39057 ) ;
#57275 = VERTEX_POINT ( 'NONE', #44821 ) ;
#57276 = ORIENTED_EDGE ( 'NONE', *, *, #156, .F. ) ;
#57277 = DIRECTION ( 'NONE',  ( 1.836970198721029934E-16, 1.836970198721010706E-16, -1.000000000000000000 ) ) ;
#57278 = ORIENTED_EDGE ( 'NONE', *, *, #2478, .T. ) ;
#57279 = DIRECTION ( 'NONE',  ( 0.000000000000000000, 0.7084617869628681008, 0.7057491738665939707 ) ) ;
#57280 = EDGE_LOOP ( 'NONE', ( #8807, #57341, #17907, #64965 ) ) ;
#57281 = CARTESIAN_POINT ( 'NONE',  ( 176.0064834503533575, 2.160375375128253950, 0.000000000000000000 ) ) ;
#57282 = AXIS2_PLACEMENT_3D ( 'NONE', #6560, #17854, #55346 ) ;
#57283 = CIRCLE ( 'NONE', #53925, 4.500000000000190958 ) ;
#57284 = CARTESIAN_POINT ( 'NONE',  ( 4.456444791733522252E-16, 7.450000000000002842, -12.50000000000000000 ) ) ;
#57285 = DIRECTION ( 'NONE',  ( 0.000000000000000000, 0.000000000000000000, -1.000000000000000000 ) ) ;
#57286 = ORIENTED_EDGE ( 'NONE', *, *, #33032, .T. ) ;
#57287 = VERTEX_POINT ( 'NONE', #66043 ) ;
#57288 = CARTESIAN_POINT ( 'NONE',  ( 29.50000000000000355, -11.50000000000000000, 15.00000000000000000 ) ) ;
#57289 = ORIENTED_EDGE ( 'NONE', *, *, #23700, .T. ) ;
#57290 = EDGE_LOOP ( 'NONE', ( #32350, #28419, #58739, #16260 ) ) ;
#57291 = AXIS2_PLACEMENT_3D ( 'NONE', #44889, #62193, #13756 ) ;
#57292 = DIRECTION ( 'NONE',  ( 0.000000000000000000, -1.000000000000000000, 0.000000000000000000 ) ) ;
#57293 = CARTESIAN_POINT ( 'NONE',  ( -7.450000000000001954, -7.249999999999998224, -18.50000000000000000 ) ) ;
#57294 = CARTESIAN_POINT ( 'NONE',  ( 39.00000000000000000, 0.000000000000000000, 0.000000000000000000 ) ) ;
#57295 = DIRECTION ( 'NONE',  ( 0.000000000000000000, -1.000000000000000000, 0.000000000000000000 ) ) ;
#57296 = ORIENTED_EDGE ( 'NONE', *, *, #19656, .F. ) ;
#57297 = CARTESIAN_POINT ( 'NONE',  ( -30.00000000000000000, -16.64230188589299786, 14.64519951917100116 ) ) ;
#57299 = CARTESIAN_POINT ( 'NONE',  ( 11.00000000000000000, -9.454754784057099570, -17.53999999999999915 ) ) ;
#57298 = PLANE ( 'NONE',  #21975 ) ;
#57300 = ORIENTED_EDGE ( 'NONE', *, *, #58023, .T. ) ;
#57302 = ORIENTED_EDGE ( 'NONE', *, *, #32268, .T. ) ;
#57301 = LINE ( 'NONE', #47048, #63541 ) ;
#57303 = ORIENTED_EDGE ( 'NONE', *, *, #501, .T. ) ;
#57304 = ORIENTED_EDGE ( 'NONE', *, *, #28406, .F. ) ;
#57305 = EDGE_CURVE ( 'NONE', #16845, #68516, #55790, .T. ) ;
#57306 = LINE ( 'NONE', #20523, #24215 ) ;
#57307 = DIRECTION ( 'NONE',  ( -1.000000000000000000, 0.000000000000000000, 0.000000000000000000 ) ) ;
#57308 = ORIENTED_EDGE ( 'NONE', *, *, #12776, .F. ) ;
#57309 = VECTOR ( 'NONE', #31975, 1000.000000000000000 ) ;
#57310 = ORIENTED_EDGE ( 'NONE', *, *, #69494, .F. ) ;
#57311 = EDGE_CURVE ( 'NONE', #18617, #52439, #17954, .T. ) ;
#57312 = DIRECTION ( 'NONE',  ( 1.836970198721029934E-16, 1.836970198721010706E-16, -1.000000000000000000 ) ) ;
#57313 = FACE_OUTER_BOUND ( 'NONE', #63238, .T. ) ;
#57314 = ORIENTED_EDGE ( 'NONE', *, *, #31555, .F. ) ;
#57315 = ORIENTED_EDGE ( 'NONE', *, *, #52170, .F. ) ;
#57316 = CIRCLE ( 'NONE', #49411, 3.499999999999855227 ) ;
#57318 = CARTESIAN_POINT ( 'NONE',  ( -3.142976262117261221, 4.031976262117183296, 54.00000000000000711 ) ) ;
#57317 = AXIS2_PLACEMENT_3D ( 'NONE', #10811, #69166, #43691 ) ;
#57319 = EDGE_CURVE ( 'NONE', #40613, #9508, #11604, .T. ) ;
#57320 = LINE ( 'NONE', #51673, #57622 ) ;
#57321 = ORIENTED_EDGE ( 'NONE', *, *, #66315, .T. ) ;
#57322 = AXIS2_PLACEMENT_3D ( 'NONE', #54171, #27295, #48859 ) ;
#57323 = CIRCLE ( 'NONE', #52817, 5.250000000000000000 ) ;
#57324 = LINE ( 'NONE', #58391, #30111 ) ;
#57325 = DIRECTION ( 'NONE',  ( 0.000000000000000000, 0.000000000000000000, 1.000000000000000000 ) ) ;
#57327 = VERTEX_POINT ( 'NONE', #12290 ) ;
#57326 = CARTESIAN_POINT ( 'NONE',  ( -4.031976262117261456, 3.142976262117183506, 26.00000000000000711 ) ) ;
#57328 = ORIENTED_EDGE ( 'NONE', *, *, #14844, .F. ) ;
#57329 = DIRECTION ( 'NONE',  ( -3.491481338843133355E-15, -1.000000000000000000, -1.836970198721029934E-16 ) ) ;
#57330 = VECTOR ( 'NONE', #27006, 1000.000000000000000 ) ;
#57331 = VECTOR ( 'NONE', #55730, 1000.000000000000114 ) ;
#57332 = PLANE ( 'NONE',  #1339 ) ;
#57333 = CARTESIAN_POINT ( 'NONE',  ( 0.000000000000000000, -8.249999999999998224, -15.00000000000000000 ) ) ;
#57334 = CARTESIAN_POINT ( 'NONE',  ( 7.532023737882817649, -6.665817930929303969, 54.00000000000000711 ) ) ;
#57335 = LINE ( 'NONE', #56634, #68910 ) ;
#57336 = DIRECTION ( 'NONE',  ( -0.000000000000000000, 3.673940397442059868E-16, -1.000000000000000000 ) ) ;
#57337 = ORIENTED_EDGE ( 'NONE', *, *, #52217, .F. ) ;
#57338 = FACE_OUTER_BOUND ( 'NONE', #8884, .T. ) ;
#57339 = EDGE_CURVE ( 'NONE', #19122, #33105, #39517, .T. ) ;
#57341 = ORIENTED_EDGE ( 'NONE', *, *, #45108, .F. ) ;
#57340 = DIRECTION ( 'NONE',  ( -0.000000000000000000, -0.000000000000000000, 1.000000000000000000 ) ) ;
#57342 = DIRECTION ( 'NONE',  ( 0.000000000000000000, 0.000000000000000000, -1.000000000000000000 ) ) ;
#57343 = DIRECTION ( 'NONE',  ( -1.000000000000000000, 0.000000000000000000, 0.000000000000000000 ) ) ;
#57344 = EDGE_CURVE ( 'NONE', #40439, #12122, #60744, .T. ) ;
#57345 = EDGE_CURVE ( 'NONE', #41911, #27132, #61421, .T. ) ;
#57346 = DIRECTION ( 'NONE',  ( 0.000000000000000000, 0.000000000000000000, -1.000000000000000000 ) ) ;
#57347 = EDGE_CURVE ( 'NONE', #33281, #62698, #49462, .T. ) ;
#57348 = VERTEX_POINT ( 'NONE', #65715 ) ;
#57349 = CARTESIAN_POINT ( 'NONE',  ( -25.50000000000000355, -15.50000000000000000, 22.50000000000000000 ) ) ;
#57350 = DIRECTION ( 'NONE',  ( 1.000000000000000000, -0.000000000000000000, 0.000000000000000000 ) ) ;
#57351 = ORIENTED_EDGE ( 'NONE', *, *, #14800, .F. ) ;
#57352 = EDGE_CURVE ( 'NONE', #9744, #33676, #55452, .T. ) ;
#57353 = DIRECTION ( 'NONE',  ( 0.000000000000000000, 0.000000000000000000, -1.000000000000000000 ) ) ;
#57354 = ADVANCED_FACE ( 'NONE', ( #1027 ), #50488, .F. ) ;
#57355 = EDGE_CURVE ( 'NONE', #34574, #3676, #18645, .T. ) ;
#57356 = CARTESIAN_POINT ( 'NONE',  ( 4.456444791733522252E-16, 7.450000000000002842, -25.50000000000000355 ) ) ;
#57357 = ORIENTED_EDGE ( 'NONE', *, *, #30829, .F. ) ;
#57358 = CARTESIAN_POINT ( 'NONE',  ( -11.50000000000000000, -11.70000000000000284, -11.00000000000000000 ) ) ;
#57359 = VERTEX_POINT ( 'NONE', #56828 ) ;
#57360 = AXIS2_PLACEMENT_3D ( 'NONE', #6404, #23685, #22998 ) ;
#57361 = EDGE_LOOP ( 'NONE', ( #10294, #32245, #51004, #2020 ) ) ;
#57362 = CARTESIAN_POINT ( 'NONE',  ( 7.826483450353421745, 11.99351654964657499, 455.0000000000000568 ) ) ;
#57363 = CYLINDRICAL_SURFACE ( 'NONE', #45522, 0.5000000000009302559 ) ;
#57364 = CARTESIAN_POINT ( 'NONE',  ( 7.250000000000005329, 8.250000000000001776, -15.50000000000000000 ) ) ;
#57365 = DIRECTION ( 'NONE',  ( 0.000000000000000000, 0.000000000000000000, 1.000000000000000000 ) ) ;
#57366 = LINE ( 'NONE', #47805, #32906 ) ;
#57367 = ORIENTED_EDGE ( 'NONE', *, *, #10025, .T. ) ;
#57368 = VERTEX_POINT ( 'NONE', #34904 ) ;
#57370 = EDGE_LOOP ( 'NONE', ( #32027, #56087, #26131, #47395 ) ) ;
#57369 = FACE_OUTER_BOUND ( 'NONE', #33717, .T. ) ;
#57371 = EDGE_LOOP ( 'NONE', ( #593, #34532, #28090, #11815 ) ) ;
#57372 = VECTOR ( 'NONE', #21547, 1000.000000000000000 ) ;
#57373 = DIRECTION ( 'NONE',  ( 0.000000000000000000, -0.000000000000000000, 1.000000000000000000 ) ) ;
#57374 = CARTESIAN_POINT ( 'NONE',  ( -11.50000000000000000, -15.46862696659690073, -14.50000000000000000 ) ) ;
#57375 = DIRECTION ( 'NONE',  ( 0.9583148474998870459, 0.000000000000000000, -0.2857142857143623593 ) ) ;
#57376 = EDGE_CURVE ( 'NONE', #39010, #32501, #67797, .T. ) ;
#57377 = CARTESIAN_POINT ( 'NONE',  ( -6.467976262117258734, 5.242976262117182706, 54.00000000000000711 ) ) ;
#57378 = AXIS2_PLACEMENT_3D ( 'NONE', #49145, #7029, #17648 ) ;
#57380 = DIRECTION ( 'NONE',  ( 0.000000000000000000, 0.000000000000000000, -1.000000000000000000 ) ) ;
#57379 = AXIS2_PLACEMENT_3D ( 'NONE', #42611, #26014, #63486 ) ;
#57381 = DIRECTION ( 'NONE',  ( -1.000000000000000000, 0.000000000000000000, 0.000000000000000000 ) ) ;
#57382 = ORIENTED_EDGE ( 'NONE', *, *, #42837, .T. ) ;
#57383 = ORIENTED_EDGE ( 'NONE', *, *, #59855, .F. ) ;
#57384 = VERTEX_POINT ( 'NONE', #50823 ) ;
#57385 = EDGE_CURVE ( 'NONE', #17547, #59678, #38663, .T. ) ;
#57386 = ORIENTED_EDGE ( 'NONE', *, *, #54297, .T. ) ;
#57387 = DIRECTION ( 'NONE',  ( 0.000000000000000000, 0.000000000000000000, -1.000000000000000000 ) ) ;
#57388 = CYLINDRICAL_SURFACE ( 'NONE', #1640, 1.929199999999998028 ) ;
#57389 = EDGE_CURVE ( 'NONE', #361, #42085, #24310, .T. ) ;
#57390 = AXIS2_PLACEMENT_3D ( 'NONE', #27360, #27009, #48579 ) ;
#57391 = LINE ( 'NONE', #29816, #10553 ) ;
#57392 = VERTEX_POINT ( 'NONE', #67089 ) ;
#57393 = ORIENTED_EDGE ( 'NONE', *, *, #33728, .T. ) ;
#57394 = ORIENTED_EDGE ( 'NONE', *, *, #39265, .T. ) ;
#57395 = CYLINDRICAL_SURFACE ( 'NONE', #62132, 0.1999999999999992339 ) ;
#57396 = VERTEX_POINT ( 'NONE', #45876 ) ;
#57397 = ORIENTED_EDGE ( 'NONE', *, *, #8631, .F. ) ;
#57398 = DIRECTION ( 'NONE',  ( -0.000000000000000000, 3.673940397442059868E-16, -1.000000000000000000 ) ) ;
#57399 = VERTEX_POINT ( 'NONE', #45517 ) ;
#57400 = ORIENTED_EDGE ( 'NONE', *, *, #4429, .T. ) ;
#57401 = DIRECTION ( 'NONE',  ( -1.000000000000000000, 0.000000000000000000, 0.000000000000000000 ) ) ;
#57402 = ADVANCED_FACE ( 'NONE', ( #19690 ), #67458, .F. ) ;
#57404 = VERTEX_POINT ( 'NONE', #29959 ) ;
#57403 = CARTESIAN_POINT ( 'NONE',  ( 30.00000000000000000, -11.85423089348099879, -9.852125413066602277 ) ) ;
#57405 = EDGE_LOOP ( 'NONE', ( #25181, #39714, #58431, #66899, #36446, #12558, #18729, #8177 ) ) ;
#57406 = CARTESIAN_POINT ( 'NONE',  ( 146.5599459900709860, 9.000000000000001776, 320.8239988703753056 ) ) ;
#57407 = CARTESIAN_POINT ( 'NONE',  ( 10.31452373788279964, 6.642976262117187503, 26.00000000000000711 ) ) ;
#57408 = DIRECTION ( 'NONE',  ( 0.000000000000000000, -1.000000000000000000, 0.000000000000000000 ) ) ;
#57409 = EDGE_CURVE ( 'NONE', #16440, #22852, #19007, .T. ) ;
#57411 = VERTEX_POINT ( 'NONE', #46222 ) ;
#57410 = DIRECTION ( 'NONE',  ( 0.000000000000000000, -1.000000000000000000, 0.000000000000000000 ) ) ;
#57412 = EDGE_CURVE ( 'NONE', #34054, #1375, #40915, .T. ) ;
#57413 = ORIENTED_EDGE ( 'NONE', *, *, #60056, .F. ) ;
#57414 = FACE_OUTER_BOUND ( 'NONE', #3154, .T. ) ;
#57415 = ADVANCED_FACE ( 'NONE', ( #8383 ), #40217, .T. ) ;
#57416 = DIRECTION ( 'NONE',  ( 1.000000000000000000, 0.000000000000000000, 0.000000000000000000 ) ) ;
#57417 = EDGE_CURVE ( 'NONE', #60243, #47516, #54472, .T. ) ;
#57418 = EDGE_CURVE ( 'NONE', #53050, #32475, #19350, .T. ) ;
#57419 = DIRECTION ( 'NONE',  ( 0.000000000000000000, -0.8206518066484758123, 0.5714285714283042772 ) ) ;
#57420 = CARTESIAN_POINT ( 'NONE',  ( 7.250000000000004441, 7.450000000000001954, -21.50000000000000000 ) ) ;
#57421 = VERTEX_POINT ( 'NONE', #57190 ) ;
#57422 = CARTESIAN_POINT ( 'NONE',  ( 7.250000000000005329, 7.250000000000000888, -25.00000000000000000 ) ) ;
#57423 = EDGE_CURVE ( 'NONE', #15308, #47849, #56723, .T. ) ;
#57424 = CARTESIAN_POINT ( 'NONE',  ( 6.500000000000002665, 6.500000000000000888, -1.000000000000000000 ) ) ;
#57425 = CYLINDRICAL_SURFACE ( 'NONE', #41357, 5.000000000000000000 ) ;
#57426 = EDGE_CURVE ( 'NONE', #46689, #36514, #19471, .T. ) ;
#57427 = ORIENTED_EDGE ( 'NONE', *, *, #57352, .T. ) ;
#57428 = CARTESIAN_POINT ( 'NONE',  ( 11.00000000000000000, -8.959999999999999076, -17.04524521594300523 ) ) ;
#57429 = EDGE_CURVE ( 'NONE', #2486, #32184, #30321, .T. ) ;
#57430 = CYLINDRICAL_SURFACE ( 'NONE', #62274, 2.000000000000000000 ) ;
#57431 = VECTOR ( 'NONE', #17492, 1000.000000000000000 ) ;
#57432 = DIRECTION ( 'NONE',  ( 0.000000000000000000, 0.000000000000000000, 1.000000000000000000 ) ) ;
#57433 = EDGE_LOOP ( 'NONE', ( #30541, #13549, #51343, #39532 ) ) ;
#57434 = CARTESIAN_POINT ( 'NONE',  ( 4.720772854004770203, 6.344366288193352688, 54.00000000000000711 ) ) ;
#57435 = EDGE_CURVE ( 'NONE', #53128, #64055, #3797, .T. ) ;
#57436 = DIRECTION ( 'NONE',  ( 0.000000000000000000, 1.000000000000000000, 0.000000000000000000 ) ) ;
#57437 = EDGE_CURVE ( 'NONE', #27985, #64753, #57806, .T. ) ;
#57438 = VECTOR ( 'NONE', #30127, 1000.000000000000000 ) ;
#57439 = FACE_OUTER_BOUND ( 'NONE', #68178, .T. ) ;
#57440 = EDGE_LOOP ( 'NONE', ( #19679, #64015, #54962, #6010 ) ) ;
#57441 = CARTESIAN_POINT ( 'NONE',  ( 30.00000000000000000, -10.85999999999999943, 9.000000000000001776 ) ) ;
#57442 = DIRECTION ( 'NONE',  ( 1.836970198721029934E-16, 1.836970198721010706E-16, -1.000000000000000000 ) ) ;
#57443 = FACE_OUTER_BOUND ( 'NONE', #38765, .T. ) ;
#57444 = DIRECTION ( 'NONE',  ( 0.000000000000000000, -0.000000000000000000, -1.000000000000000000 ) ) ;
#57445 = DIRECTION ( 'NONE',  ( -0.000000000000000000, 3.673940397442059868E-16, -1.000000000000000000 ) ) ;
#57446 = ORIENTED_EDGE ( 'NONE', *, *, #12642, .F. ) ;
#57447 = DIRECTION ( 'NONE',  ( 1.000000000000000000, -1.047444401652940007E-14, 1.836970198721010706E-16 ) ) ;
#57448 = LINE ( 'NONE', #56395, #22651 ) ;
#57449 = DIRECTION ( 'NONE',  ( 1.000000000000000000, -5.981805089575196197E-17, 0.000000000000000000 ) ) ;
#57450 = CYLINDRICAL_SURFACE ( 'NONE', #55414, 0.8100000000000017186 ) ;
#57451 = ORIENTED_EDGE ( 'NONE', *, *, #5068, .T. ) ;
#57453 = ORIENTED_EDGE ( 'NONE', *, *, #9025, .T. ) ;
#57452 = LINE ( 'NONE', #30587, #6845 ) ;
#57454 = CARTESIAN_POINT ( 'NONE',  ( 30.00000000000000000, -14.33999999999999986, -14.50000000000000000 ) ) ;
#57455 = CARTESIAN_POINT ( 'NONE',  ( 78.77321854994620765, 47.95351654967443977, 15.00000000000000000 ) ) ;
#57456 = DIRECTION ( 'NONE',  ( 1.836970198721029934E-16, 1.836970198721010706E-16, -1.000000000000000000 ) ) ;
#57457 = ORIENTED_EDGE ( 'NONE', *, *, #31398, .F. ) ;
#57458 = PLANE ( 'NONE',  #55562 ) ;
#57459 = EDGE_LOOP ( 'NONE', ( #28774, #47608, #17019, #40681 ) ) ;
#57460 = VERTEX_POINT ( 'NONE', #42242 ) ;
#57461 = AXIS2_PLACEMENT_3D ( 'NONE', #30260, #63836, #51822 ) ;
#57462 = EDGE_CURVE ( 'NONE', #41126, #36987, #52236, .T. ) ;
#57463 = EDGE_LOOP ( 'NONE', ( #21313, #50127, #5191, #53436, #3216, #16409, #18166, #57719 ) ) ;
#57464 = VERTEX_POINT ( 'NONE', #30945 ) ;
#57465 = CARTESIAN_POINT ( 'NONE',  ( 283.0000000000000568, -23.29603921945599865, -12.50000000000000000 ) ) ;
#57466 = CARTESIAN_POINT ( 'NONE',  ( -3.142976262117251451, 6.486996718459839606, 54.00000000000000711 ) ) ;
#57467 = EDGE_CURVE ( 'NONE', #36712, #829, #37567, .T. ) ;
#57468 = DIRECTION ( 'NONE',  ( 1.000000000000000000, 0.000000000000000000, 0.000000000000000000 ) ) ;
#57469 = CARTESIAN_POINT ( 'NONE',  ( 41.09999999999999432, -0.2000000000000000111, 0.000000000000000000 ) ) ;
#57470 = VERTEX_POINT ( 'NONE', #3370 ) ;
#57471 = ORIENTED_EDGE ( 'NONE', *, *, #30226, .F. ) ;
#57472 = EDGE_CURVE ( 'NONE', #16386, #17050, #46147, .T. ) ;
#57473 = CARTESIAN_POINT ( 'NONE',  ( -11.77351654964674310, -4.406483450353321452, 455.0000000000000568 ) ) ;
#57474 = VECTOR ( 'NONE', #29072, 1000.000000000000000 ) ;
#57475 = DIRECTION ( 'NONE',  ( -0.7071067811865472397, -0.5000000000000002220, -0.5000000000000002220 ) ) ;
#57476 = VERTEX_POINT ( 'NONE', #52515 ) ;
#57477 = EDGE_CURVE ( 'NONE', #43775, #24181, #30592, .T. ) ;
#57478 = ORIENTED_EDGE ( 'NONE', *, *, #6529, .F. ) ;
#57479 = ORIENTED_EDGE ( 'NONE', *, *, #24756, .F. ) ;
#57480 = VECTOR ( 'NONE', #40176, 1000.000000000000114 ) ;
#57481 = VERTEX_POINT ( 'NONE', #62400 ) ;
#57482 = CARTESIAN_POINT ( 'NONE',  ( -5.993516549646711766, 5.993516549646603409, 455.0000000000000568 ) ) ;
#57483 = EDGE_CURVE ( 'NONE', #3182, #52538, #9340, .T. ) ;
#57485 = ORIENTED_EDGE ( 'NONE', *, *, #16469, .F. ) ;
#57484 = CARTESIAN_POINT ( 'NONE',  ( 283.0000000000000568, -31.30000000000000071, 12.69999999999999929 ) ) ;
#57487 = AXIS2_PLACEMENT_3D ( 'NONE', #67751, #56788, #67417 ) ;
#57486 = CIRCLE ( 'NONE', #65377, 0.1749999999999980738 ) ;
#57488 = LINE ( 'NONE', #63146, #2924 ) ;
#57489 = DIRECTION ( 'NONE',  ( 0.000000000000000000, -0.000000000000000000, -1.000000000000000000 ) ) ;
#57490 = ORIENTED_EDGE ( 'NONE', *, *, #57311, .F. ) ;
#57491 = ORIENTED_EDGE ( 'NONE', *, *, #30593, .F. ) ;
#57492 = EDGE_CURVE ( 'NONE', #37690, #46086, #44294, .T. ) ;
#57493 = CIRCLE ( 'NONE', #41696, 0.2000000000000005107 ) ;
#57494 = EDGE_CURVE ( 'NONE', #29414, #22636, #13970, .T. ) ;
#57495 = DIRECTION ( 'NONE',  ( 0.000000000000000000, 0.000000000000000000, -1.000000000000000000 ) ) ;
#57496 = FACE_OUTER_BOUND ( 'NONE', #67622, .T. ) ;
#57497 = EDGE_LOOP ( 'NONE', ( #57208, #1089, #57645, #17190, #31856, #8983 ) ) ;
#57498 = DIRECTION ( 'NONE',  ( -1.000000000000000000, 0.000000000000000000, 0.000000000000000000 ) ) ;
#57499 = CYLINDRICAL_SURFACE ( 'NONE', #4247, 1.929199999999997139 ) ;
#57500 = VECTOR ( 'NONE', #41395, 1000.000000000000000 ) ;
#57501 = DIRECTION ( 'NONE',  ( -1.000000000000000000, 0.000000000000000000, 0.000000000000000000 ) ) ;
#57502 = EDGE_LOOP ( 'NONE', ( #42338, #24354, #68811, #41367 ) ) ;
#57503 = DIRECTION ( 'NONE',  ( 2.891205793294683355E-15, 1.000000000000000000, 0.000000000000000000 ) ) ;
#57504 = DIRECTION ( 'NONE',  ( -1.000000000000000000, 0.000000000000000000, 0.000000000000000000 ) ) ;
#57505 = DIRECTION ( 'NONE',  ( 0.000000000000000000, 0.000000000000000000, -1.000000000000000000 ) ) ;
#57506 = LINE ( 'NONE', #9075, #50524 ) ;
#57507 = CIRCLE ( 'NONE', #54157, 0.1749999999999998224 ) ;
#57508 = DIRECTION ( 'NONE',  ( -1.000000000000000000, 0.000000000000000000, 0.000000000000000000 ) ) ;
#57509 = ORIENTED_EDGE ( 'NONE', *, *, #44364, .T. ) ;
#57510 = CARTESIAN_POINT ( 'NONE',  ( 11.34648345035334671, 1.077516549646521327, 455.0000000000000568 ) ) ;
#57511 = LINE ( 'NONE', #52938, #53169 ) ;
#57512 = ADVANCED_FACE ( 'NONE', ( #35531 ), #3030, .F. ) ;
#57513 = VECTOR ( 'NONE', #32428, 1000.000000000000000 ) ;
#57514 = SURFACE_SIDE_STYLE ('',( #62822 ) ) ;
#57515 = AXIS2_PLACEMENT_3D ( 'NONE', #67479, #34919, #19368 ) ;
#57516 = PLANE ( 'NONE',  #14221 ) ;
#57517 = ADVANCED_FACE ( 'NONE', ( #20333 ), #25654, .T. ) ;
#57518 = DIRECTION ( 'NONE',  ( -1.000000000000000000, 0.000000000000000000, 0.000000000000000000 ) ) ;
#57519 = FACE_OUTER_BOUND ( 'NONE', #38111, .T. ) ;
#57520 = AXIS2_PLACEMENT_3D ( 'NONE', #60464, #12013, #33598 ) ;
#57521 = CARTESIAN_POINT ( 'NONE',  ( 7.450000000000004619, -1.336933437520057563E-15, -20.50000000000000000 ) ) ;
#57522 = DIRECTION ( 'NONE',  ( 1.836970198721029934E-16, -1.836970198721036344E-16, 1.000000000000000000 ) ) ;
#57523 = VERTEX_POINT ( 'NONE', #19986 ) ;
#57524 = FACE_OUTER_BOUND ( 'NONE', #40747, .T. ) ;
#57525 = CARTESIAN_POINT ( 'NONE',  ( 0.000000000000000000, -8.749999999999998224, -30.00000000000001066 ) ) ;
#57526 = ORIENTED_EDGE ( 'NONE', *, *, #27543, .F. ) ;
#57527 = DIRECTION ( 'NONE',  ( -1.920292680692490463E-14, -1.000000000000000000, -1.836970198721045958E-16 ) ) ;
#57528 = LINE ( 'NONE', #35597, #19814 ) ;
#57529 = AXIS2_PLACEMENT_3D ( 'NONE', #61383, #34519, #45838 ) ;
#57530 = DIRECTION ( 'NONE',  ( -0.000000000000000000, -0.000000000000000000, 1.000000000000000000 ) ) ;
#57531 = LINE ( 'NONE', #40566, #62417 ) ;
#57532 = DIRECTION ( 'NONE',  ( 0.000000000000000000, 1.000000000000000000, 0.000000000000000000 ) ) ;
#57533 = VERTEX_POINT ( 'NONE', #41190 ) ;
#57534 = VECTOR ( 'NONE', #63804, 1000.000000000000000 ) ;
#57535 = DIRECTION ( 'NONE',  ( -0.000000000000000000, 3.673940397442059868E-16, -1.000000000000000000 ) ) ;
#57536 = ORIENTED_EDGE ( 'NONE', *, *, #65325, .F. ) ;
#57537 = CARTESIAN_POINT ( 'NONE',  ( 6.619341603356837744, -7.265214908726241205, 455.0000000000000568 ) ) ;
#57538 = LINE ( 'NONE', #30674, #23233 ) ;
#57539 = ORIENTED_EDGE ( 'NONE', *, *, #7943, .T. ) ;
#57540 = DIRECTION ( 'NONE',  ( 0.000000000000000000, 0.000000000000000000, 1.000000000000000000 ) ) ;
#57541 = VECTOR ( 'NONE', #44351, 1000.000000000000000 ) ;
#57542 = DIRECTION ( 'NONE',  ( 0.000000000000000000, -1.000000000000000000, 0.000000000000000000 ) ) ;
#57543 = ORIENTED_EDGE ( 'NONE', *, *, #18125, .F. ) ;
#57544 = LINE ( 'NONE', #9825, #57077 ) ;
#57545 = ORIENTED_EDGE ( 'NONE', *, *, #49121, .F. ) ;
#57546 = VERTEX_POINT ( 'NONE', #62762 ) ;
#57547 = DIRECTION ( 'NONE',  ( 0.7671651518153044247, -0.6414496315691521344, 0.000000000000000000 ) ) ;
#57548 = ORIENTED_EDGE ( 'NONE', *, *, #61636, .T. ) ;
#57549 = EDGE_LOOP ( 'NONE', ( #20978, #54673, #40803, #37327 ) ) ;
#57550 = EDGE_CURVE ( 'NONE', #45925, #42134, #9015, .T. ) ;
#57551 = CARTESIAN_POINT ( 'NONE',  ( 9.900000000000000355, 0.000000000000000000, 2.154935995002245639E-16 ) ) ;
#57552 = DIRECTION ( 'NONE',  ( 0.000000000000000000, 0.000000000000000000, 1.000000000000000000 ) ) ;
#57553 = CARTESIAN_POINT ( 'NONE',  ( -2.530476262117327568, -9.737023737882829266, 54.00000000000000711 ) ) ;
#57554 = AXIS2_PLACEMENT_3D ( 'NONE', #24077, #13469, #51661 ) ;
#57555 = EDGE_LOOP ( 'NONE', ( #17290, #41089, #53887, #41803 ) ) ;
#57556 = EDGE_CURVE ( 'NONE', #58634, #59658, #35901, .T. ) ;
#57557 = DIRECTION ( 'NONE',  ( 1.000000000000000000, -0.000000000000000000, 0.000000000000000000 ) ) ;
#57559 = CARTESIAN_POINT ( 'NONE',  ( -7.450000000000001954, 7.250000000000000000, -18.00000000000000000 ) ) ;
#57558 = CARTESIAN_POINT ( 'NONE',  ( 289.9999999999998863, -41.99999999999992184, 26.49999999999997158 ) ) ;
#57560 = ORIENTED_EDGE ( 'NONE', *, *, #23491, .F. ) ;
#57562 = ORIENTED_EDGE ( 'NONE', *, *, #41454, .T. ) ;
#57561 = CARTESIAN_POINT ( 'NONE',  ( 7.606483450353380249, -11.78648345035339418, 195.0000000000000284 ) ) ;
#57563 = ADVANCED_FACE ( 'NONE', ( #58533, #26001 ), #69121, .T. ) ;
#57564 = EDGE_LOOP ( 'NONE', ( #3972, #39340, #27240, #59191, #57653, #34129, #25598, #49138 ) ) ;
#57565 = EDGE_CURVE ( 'NONE', #59900, #10965, #65811, .T. ) ;
#57566 = PRODUCT_CONTEXT ( 'NONE', #17819, 'mechanical' ) ;
#57567 = EDGE_CURVE ( 'NONE', #41995, #61368, #58166, .T. ) ;
#57568 = EDGE_CURVE ( 'NONE', #42522, #36943, #34141, .T. ) ;
#57569 = DIRECTION ( 'NONE',  ( 0.000000000000000000, 1.000000000000000000, 0.000000000000000000 ) ) ;
#57570 = VECTOR ( 'NONE', #61261, 1000.000000000000000 ) ;
#57571 = VECTOR ( 'NONE', #21131, 1000.000000000000000 ) ;
#57573 = ORIENTED_EDGE ( 'NONE', *, *, #8794, .T. ) ;
#57572 = LINE ( 'NONE', #58278, #9414 ) ;
#57574 = FACE_OUTER_BOUND ( 'NONE', #28608, .T. ) ;
#57575 = EDGE_CURVE ( 'NONE', #31525, #8587, #54611, .T. ) ;
#57576 = FACE_OUTER_BOUND ( 'NONE', #34905, .T. ) ;
#57577 = VERTEX_POINT ( 'NONE', #38682 ) ;
#57578 = EDGE_LOOP ( 'NONE', ( #20173, #39176, #56600, #69183, #38504, #39330, #10548, #6796 ) ) ;
#57579 = DIRECTION ( 'NONE',  ( 0.000000000000000000, 0.000000000000000000, -1.000000000000000000 ) ) ;
#57580 = ORIENTED_EDGE ( 'NONE', *, *, #62136, .T. ) ;
#57581 = AXIS2_PLACEMENT_3D ( 'NONE', #17344, #32927, #38919 ) ;
#57582 = FACE_OUTER_BOUND ( 'NONE', #59706, .T. ) ;
#57583 = PLANE ( 'NONE',  #29011 ) ;
#57584 = DIRECTION ( 'NONE',  ( -1.000000000000000000, 0.000000000000000000, 0.000000000000000000 ) ) ;
#57585 = VECTOR ( 'NONE', #30186, 1000.000000000000000 ) ;
#57586 = EDGE_LOOP ( 'NONE', ( #45093, #45395, #7481, #68608 ) ) ;
#57587 = AXIS2_PLACEMENT_3D ( 'NONE', #17785, #56657, #66568 ) ;
#57588 = LINE ( 'NONE', #25068, #48248 ) ;
#57589 = CARTESIAN_POINT ( 'NONE',  ( -3.650476262117221093, 10.49297626211717116, 26.00000000000000711 ) ) ;
#57591 = VERTEX_POINT ( 'NONE', #59564 ) ;
#57590 = CYLINDRICAL_SURFACE ( 'NONE', #28611, 3.500000000000003109 ) ;
#57593 = ORIENTED_EDGE ( 'NONE', *, *, #19268, .F. ) ;
#57592 = FACE_OUTER_BOUND ( 'NONE', #30415, .T. ) ;
#57594 = CARTESIAN_POINT ( 'NONE',  ( -7.250000000000001776, -7.249999999999998224, -23.00000000000000000 ) ) ;
#57595 = VECTOR ( 'NONE', #61220, 1000.000000000000000 ) ;
#57596 = CIRCLE ( 'NONE', #63257, 4.000000000000000000 ) ;
#57597 = CARTESIAN_POINT ( 'NONE',  ( 8.900000000000002132, -21.00000000000000000, -18.00000000000000355 ) ) ;
#57598 = CARTESIAN_POINT ( 'NONE',  ( -3.417780618358626565, 7.839518282750134404, 455.0000000000000568 ) ) ;
#57599 = DIRECTION ( 'NONE',  ( -1.000000000000000000, 0.000000000000000000, 0.000000000000000000 ) ) ;
#57600 = DIRECTION ( 'NONE',  ( 9.050731179009442381E-15, 1.000000000000000000, 3.673940397442060361E-16 ) ) ;
#57601 = ORIENTED_EDGE ( 'NONE', *, *, #52829, .T. ) ;
#57602 = CARTESIAN_POINT ( 'NONE',  ( 33.89999999999999858, -21.00000000000000000, 13.86939075806900057 ) ) ;
#57603 = FACE_OUTER_BOUND ( 'NONE', #9229, .T. ) ;
#57604 = DIRECTION ( 'NONE',  ( 1.836970198721029934E-16, 1.836970198721010706E-16, -1.000000000000000000 ) ) ;
#57606 = ORIENTED_EDGE ( 'NONE', *, *, #64540, .T. ) ;
#57605 = CARTESIAN_POINT ( 'NONE',  ( 30.00000000000000000, -17.50000000000000000, -15.70500000000000007 ) ) ;
#57607 = EDGE_CURVE ( 'NONE', #19822, #96, #35247, .T. ) ;
#57608 = DIRECTION ( 'NONE',  ( 0.000000000000000000, 0.000000000000000000, -1.000000000000000000 ) ) ;
#57609 = VECTOR ( 'NONE', #23556, 1000.000000000000000 ) ;
#57610 = EDGE_CURVE ( 'NONE', #60006, #26902, #37303, .T. ) ;
#57611 = CYLINDRICAL_SURFACE ( 'NONE', #9296, 25.39999999999999858 ) ;
#57612 = ADVANCED_FACE ( 'NONE', ( #38000 ), #60236, .F. ) ;
#57613 = DIRECTION ( 'NONE',  ( -7.808916176531286882E-15, -1.000000000000000000, -3.673940397442059868E-16 ) ) ;
#57614 = ORIENTED_EDGE ( 'NONE', *, *, #8605, .F. ) ;
#57615 = CARTESIAN_POINT ( 'NONE',  ( 47.00000000000000000, 0.7500000000000000000, 3.418698582794335028 ) ) ;
#57616 = DIRECTION ( 'NONE',  ( 1.000000000000000000, -5.981805089575194965E-17, 0.000000000000000000 ) ) ;
#57618 = VERTEX_POINT ( 'NONE', #53231 ) ;
#57617 = EDGE_CURVE ( 'NONE', #35171, #68411, #5482, .T. ) ;
#57619 = DIRECTION ( 'NONE',  ( 0.000000000000000000, -1.000000000000000000, 0.000000000000000000 ) ) ;
#57620 = CARTESIAN_POINT ( 'NONE',  ( 78.77321854994620765, 47.95351654967443977, 15.00000000000000000 ) ) ;
#57621 = CARTESIAN_POINT ( 'NONE',  ( 6.836383711243002814, 6.350872789121261519, 54.00000000000000711 ) ) ;
#57622 = VECTOR ( 'NONE', #19137, 1000.000000000000000 ) ;
#57623 = LINE ( 'NONE', #45968, #35356 ) ;
#57624 = VECTOR ( 'NONE', #60994, 1000.000000000000000 ) ;
#57625 = VERTEX_POINT ( 'NONE', #10763 ) ;
#57626 = DIRECTION ( 'NONE',  ( -1.000000000000000000, 0.000000000000000000, 0.000000000000000000 ) ) ;
#57627 = VERTEX_POINT ( 'NONE', #21026 ) ;
#57628 = ORIENTED_EDGE ( 'NONE', *, *, #47893, .T. ) ;
#57629 = VERTEX_POINT ( 'NONE', #69827 ) ;
#57630 = VECTOR ( 'NONE', #22487, 1000.000000000000000 ) ;
#57631 = CARTESIAN_POINT ( 'NONE',  ( 1.634292677759869639, 8.227189898828703107, 26.00000000000000711 ) ) ;
#57632 = DIRECTION ( 'NONE',  ( 1.000000000000000000, -1.047444401652940007E-14, 1.836970198721010706E-16 ) ) ;
#57633 = DIRECTION ( 'NONE',  ( 0.000000000000000000, 1.000000000000000000, 0.000000000000000000 ) ) ;
#57634 = ORIENTED_EDGE ( 'NONE', *, *, #67187, .F. ) ;
#57635 = ORIENTED_EDGE ( 'NONE', *, *, #67950, .F. ) ;
#57636 = VECTOR ( 'NONE', #53512, 1000.000000000000000 ) ;
#57637 = DIRECTION ( 'NONE',  ( 1.000000000000000000, 0.000000000000000000, 0.000000000000000000 ) ) ;
#57638 = EDGE_LOOP ( 'NONE', ( #11592, #61451, #10194, #42336 ) ) ;
#57639 = ORIENTED_EDGE ( 'NONE', *, *, #14774, .F. ) ;
#57640 = EDGE_CURVE ( 'NONE', #32481, #8571, #54263, .T. ) ;
#57641 = LINE ( 'NONE', #5318, #28145 ) ;
#57642 = CARTESIAN_POINT ( 'NONE',  ( 7.826483450353380000, -12.00648345035339659, 195.0000000000000284 ) ) ;
#57643 = CARTESIAN_POINT ( 'NONE',  ( 25.50000000000000355, -5.200000000000001066, -22.50000000000000000 ) ) ;
#57644 = DIRECTION ( 'NONE',  ( 0.000000000000000000, 0.000000000000000000, 1.000000000000000000 ) ) ;
#57645 = ORIENTED_EDGE ( 'NONE', *, *, #12294, .T. ) ;
#57646 = LINE ( 'NONE', #36076, #53771 ) ;
#57647 = AXIS2_PLACEMENT_3D ( 'NONE', #2797, #56887, #24376 ) ;
#57648 = VECTOR ( 'NONE', #7193, 1000.000000000000114 ) ;
#57650 = CARTESIAN_POINT ( 'NONE',  ( 0.000000000000000000, -8.249999999999998224, -10.50000000000000000 ) ) ;
#57649 = FACE_OUTER_BOUND ( 'NONE', #29680, .T. ) ;
#57651 = ORIENTED_EDGE ( 'NONE', *, *, #66083, .F. ) ;
#57653 = ORIENTED_EDGE ( 'NONE', *, *, #15144, .T. ) ;
#57652 = CARTESIAN_POINT ( 'NONE',  ( -7.250000000000000000, -7.449999999999998401, -11.00000000000000000 ) ) ;
#57654 = ORIENTED_EDGE ( 'NONE', *, *, #58593, .F. ) ;
#57655 = EDGE_CURVE ( 'NONE', #34366, #26875, #38708, .T. ) ;
#57656 = ADVANCED_FACE ( 'NONE', ( #885 ), #32684, .F. ) ;
#57657 = DIRECTION ( 'NONE',  ( -1.000000000000000000, 1.883404846338789915E-14, 0.000000000000000000 ) ) ;
#57658 = CARTESIAN_POINT ( 'NONE',  ( -8.697938382363135545, 2.406732575409538111, 54.00000000000000711 ) ) ;
#57659 = EDGE_CURVE ( 'NONE', #48724, #53008, #48602, .T. ) ;
#57660 = CIRCLE ( 'NONE', #27186, 0.5000000000001362244 ) ;
#57661 = VERTEX_POINT ( 'NONE', #5124 ) ;
#57662 = ORIENTED_EDGE ( 'NONE', *, *, #31953, .T. ) ;
#57663 = CARTESIAN_POINT ( 'NONE',  ( -8.393516549646712122, 7.603567055985436696, 195.0000000000000284 ) ) ;
#57664 = DIRECTION ( 'NONE',  ( 1.000000000000000000, -0.000000000000000000, 0.000000000000000000 ) ) ;
#57665 = ORIENTED_EDGE ( 'NONE', *, *, #26372, .T. ) ;
#57666 = EDGE_LOOP ( 'NONE', ( #40691, #1220, #64630, #29331, #58035, #40271, #9238, #49935 ) ) ;
#57667 = PLANE ( 'NONE',  #39810 ) ;
#57668 = VECTOR ( 'NONE', #54133, 1000.000000000000000 ) ;
#57669 = CARTESIAN_POINT ( 'NONE',  ( 9.737023737882806174, 7.955476262117184838, 54.00000000000000711 ) ) ;
#57670 = CIRCLE ( 'NONE', #14771, 0.5249999999999994671 ) ;
#57671 = ORIENTED_EDGE ( 'NONE', *, *, #17384, .T. ) ;
#57672 = VECTOR ( 'NONE', #52376, 1000.000000000000000 ) ;
#57673 = DIRECTION ( 'NONE',  ( -1.000000000000000000, 0.000000000000000000, 0.000000000000000000 ) ) ;
#57674 = CARTESIAN_POINT ( 'NONE',  ( 7.616533956692244089, 8.393516549646575342, 455.0000000000000568 ) ) ;
#57676 = ORIENTED_EDGE ( 'NONE', *, *, #1322, .F. ) ;
#57675 = DIRECTION ( 'NONE',  ( 0.000000000000000000, 0.000000000000000000, 1.000000000000000000 ) ) ;
#57677 = ORIENTED_EDGE ( 'NONE', *, *, #32474, .F. ) ;
#57678 = DIRECTION ( 'NONE',  ( 2.135044278125299371E-15, -1.000000000000000000, 0.000000000000000000 ) ) ;
#57679 = CARTESIAN_POINT ( 'NONE',  ( 9.562023737882812569, -8.144523737882813919, 26.00000000000000000 ) ) ;
#57680 = DIRECTION ( 'NONE',  ( -1.836970198721029934E-16, 1.836970198721036590E-16, -1.000000000000000000 ) ) ;
#57681 = DIRECTION ( 'NONE',  ( -1.000000000000000000, 0.000000000000000000, 0.000000000000000000 ) ) ;
#57682 = AXIS2_PLACEMENT_3D ( 'NONE', #68852, #32067, #20404 ) ;
#57683 = CIRCLE ( 'NONE', #48656, 0.5000000000001386669 ) ;
#57684 = LINE ( 'NONE', #47083, #42959 ) ;
#57685 = DIRECTION ( 'NONE',  ( 0.000000000000000000, 0.7057491738665943037, -0.7084617869628675457 ) ) ;
#57686 = VERTEX_POINT ( 'NONE', #42600 ) ;
#57687 = CARTESIAN_POINT ( 'NONE',  ( 7.000000000000000000, -40.30000000000000426, 8.900000000000000355 ) ) ;
#57688 = VECTOR ( 'NONE', #1202, 1000.000000000000000 ) ;
#57690 = ORIENTED_EDGE ( 'NONE', *, *, #65651, .T. ) ;
#57689 = DIRECTION ( 'NONE',  ( -1.000000000000000000, 1.794541526872559352E-16, 0.000000000000000000 ) ) ;
#57691 = CARTESIAN_POINT ( 'NONE',  ( -7.250000000000000888, 8.250000000000001776, -17.50000000000000000 ) ) ;
#57692 = EDGE_CURVE ( 'NONE', #66827, #69141, #16429, .T. ) ;
#57693 = LINE ( 'NONE', #9264, #26209 ) ;
#57694 = ADVANCED_FACE ( 'NONE', ( #64186 ), #43291, .F. ) ;
#57695 = ADVANCED_FACE ( 'NONE', ( #16776 ), #49949, .F. ) ;
#57696 = AXIS2_PLACEMENT_3D ( 'NONE', #26834, #14821, #37782 ) ;
#57697 = EDGE_LOOP ( 'NONE', ( #17627, #27822, #28330, #62798 ) ) ;
#57698 = DIRECTION ( 'NONE',  ( -0.7671651518153028704, -0.6414496315691537998, -2.587583378555113506E-16 ) ) ;
#57699 = CARTESIAN_POINT ( 'NONE',  ( 29.89999999999999858, -0.2000000000089119934, 8.909539772616881237E-12 ) ) ;
#57701 = ORIENTED_EDGE ( 'NONE', *, *, #57429, .F. ) ;
#57700 = EDGE_CURVE ( 'NONE', #42130, #69664, #174, .T. ) ;
#57702 = LINE ( 'NONE', #7593, #21046 ) ;
#57703 = CARTESIAN_POINT ( 'NONE',  ( 7.250000000000005329, 7.250000000000000888, -26.00000000000001066 ) ) ;
#57704 = DIRECTION ( 'NONE',  ( -5.981805089575196197E-17, -1.000000000000000000, 0.000000000000000000 ) ) ;
#57705 = ORIENTED_EDGE ( 'NONE', *, *, #33031, .F. ) ;
#57706 = AXIS2_PLACEMENT_3D ( 'NONE', #49748, #982, #7291 ) ;
#57707 = DIRECTION ( 'NONE',  ( -1.000000000000000000, 7.304098846218132892E-15, 0.000000000000000000 ) ) ;
#57708 = ORIENTED_EDGE ( 'NONE', *, *, #36107, .T. ) ;
#57709 = ORIENTED_EDGE ( 'NONE', *, *, #60518, .F. ) ;
#57710 = DIRECTION ( 'NONE',  ( -0.7671651518152985405, 0.6414496315691592399, 2.587583378555132735E-16 ) ) ;
#57711 = DIRECTION ( 'NONE',  ( 0.000000000000000000, 0.000000000000000000, -1.000000000000000000 ) ) ;
#57712 = DIRECTION ( 'NONE',  ( 1.000000000000000000, 0.000000000000000000, 0.000000000000000000 ) ) ;
#57713 = CARTESIAN_POINT ( 'NONE',  ( -30.00000000000000000, -5.599999999999999645, -9.400000000000000355 ) ) ;
#57714 = CARTESIAN_POINT ( 'NONE',  ( 5.793274621760841292, 6.344366288193348247, 54.00000000000000711 ) ) ;
#57715 = ORIENTED_EDGE ( 'NONE', *, *, #43503, .T. ) ;
#57716 = ORIENTED_EDGE ( 'NONE', *, *, #3423, .F. ) ;
#57717 = CIRCLE ( 'NONE', #9170, 4.000000000000000888 ) ;
#57719 = ORIENTED_EDGE ( 'NONE', *, *, #45588, .T. ) ;
#57718 = DIRECTION ( 'NONE',  ( 1.000000000000000000, 0.000000000000000000, 0.000000000000000000 ) ) ;
#57720 = ORIENTED_EDGE ( 'NONE', *, *, #22371, .F. ) ;
#57721 = CARTESIAN_POINT ( 'NONE',  ( 69.92576880110416937, 0.000000000000000000, 335.4830310981152479 ) ) ;
#57722 = DIRECTION ( 'NONE',  ( -1.836970198721029934E-16, 1.836970198721036344E-16, -1.000000000000000000 ) ) ;
#57723 = DIRECTION ( 'NONE',  ( -1.000000000000000000, 0.000000000000000000, 0.000000000000000000 ) ) ;
#57724 = DIRECTION ( 'NONE',  ( -0.000000000000000000, 0.000000000000000000, -1.000000000000000000 ) ) ;
#57725 = VECTOR ( 'NONE', #3785, 1000.000000000000000 ) ;
#57726 = CARTESIAN_POINT ( 'NONE',  ( 17.89999999999999858, -21.00000000000000000, 13.86939075806900057 ) ) ;
#57728 = CARTESIAN_POINT ( 'NONE',  ( 8.580623737882818958, -9.703773737882825046, 54.00000000000000711 ) ) ;
#57727 = FACE_OUTER_BOUND ( 'NONE', #20705, .T. ) ;
#57729 = ORIENTED_EDGE ( 'NONE', *, *, #13965, .F. ) ;
#57730 = ORIENTED_EDGE ( 'NONE', *, *, #29573, .F. ) ;
#57731 = ORIENTED_EDGE ( 'NONE', *, *, #10270, .F. ) ;
#57732 = AXIS2_PLACEMENT_3D ( 'NONE', #58070, #31221, #25557 ) ;
#57733 = VECTOR ( 'NONE', #39790, 1000.000000000000000 ) ;
#57734 = ORIENTED_EDGE ( 'NONE', *, *, #48405, .T. ) ;
#57735 = FACE_OUTER_BOUND ( 'NONE', #67738, .T. ) ;
#57736 = DIRECTION ( 'NONE',  ( 0.000000000000000000, 1.000000000000000000, 3.673940397442059868E-16 ) ) ;
#57737 = VECTOR ( 'NONE', #16333, 1000.000000000000000 ) ;
#57738 = EDGE_CURVE ( 'NONE', #33741, #25825, #45453, .T. ) ;
#57739 = DIRECTION ( 'NONE',  ( -1.000000000000000000, 0.000000000000000000, 0.000000000000000000 ) ) ;
#57740 = ADVANCED_FACE ( 'NONE', ( #27728 ), #43978, .F. ) ;
#57741 = ORIENTED_EDGE ( 'NONE', *, *, #52669, .T. ) ;
#57742 = ORIENTED_EDGE ( 'NONE', *, *, #60020, .T. ) ;
#57743 = EDGE_CURVE ( 'NONE', #27522, #51726, #59214, .T. ) ;
#57744 = EDGE_LOOP ( 'NONE', ( #51664, #57017, #26150, #41530 ) ) ;
#57746 = LINE ( 'NONE', #68722, #45167 ) ;
#57745 = AXIS2_PLACEMENT_3D ( 'NONE', #50642, #55262, #55605 ) ;
#57747 = ORIENTED_EDGE ( 'NONE', *, *, #41564, .F. ) ;
#57748 = ADVANCED_FACE ( 'NONE', ( #7535 ), #6833, .F. ) ;
#57749 = ORIENTED_EDGE ( 'NONE', *, *, #12782, .F. ) ;
#57750 = CARTESIAN_POINT ( 'NONE',  ( -10.08346604330787777, 9.093516549646603053, 455.0000000000000568 ) ) ;
#57751 = EDGE_LOOP ( 'NONE', ( #56626, #34761, #54199, #1909, #14055, #34459, #33045, #5989 ) ) ;
#57752 = ORIENTED_EDGE ( 'NONE', *, *, #40773, .T. ) ;
#57754 = ADVANCED_FACE ( 'NONE', ( #11792 ), #50671, .F. ) ;
#57753 = DIRECTION ( 'NONE',  ( -1.836970198721029934E-16, 1.836970198721036344E-16, -1.000000000000000000 ) ) ;
#57755 = EDGE_CURVE ( 'NONE', #62211, #54853, #55298, .T. ) ;
#57757 = ORIENTED_EDGE ( 'NONE', *, *, #15449, .F. ) ;
#57756 = CARTESIAN_POINT ( 'NONE',  ( 7.969523737882813208, 8.821682069070710952, 54.00000000000000711 ) ) ;
#57759 = ORIENTED_EDGE ( 'NONE', *, *, #6936, .F. ) ;
#57758 = ADVANCED_FACE ( 'NONE', ( #34753, #29451 ), #12824, .F. ) ;
#57760 = FACE_OUTER_BOUND ( 'NONE', #46555, .T. ) ;
#57761 = AXIS2_PLACEMENT_3D ( 'NONE', #42973, #10794, #9406 ) ;
#57762 = CARTESIAN_POINT ( 'NONE',  ( -7.250000000000000888, 7.250000000000001776, -20.00000000000000000 ) ) ;
#57764 = ORIENTED_EDGE ( 'NONE', *, *, #2853, .F. ) ;
#57763 = FACE_OUTER_BOUND ( 'NONE', #18807, .T. ) ;
#57765 = ORIENTED_EDGE ( 'NONE', *, *, #30751, .T. ) ;
#57766 = DIRECTION ( 'NONE',  ( -1.000000000000000000, 0.000000000000000000, 0.000000000000000000 ) ) ;
#57767 = LINE ( 'NONE', #42202, #18181 ) ;
#57768 = DIRECTION ( 'NONE',  ( 0.000000000000000000, 3.673940397442059868E-16, -1.000000000000000000 ) ) ;
#57769 = DIRECTION ( 'NONE',  ( 1.836970198721029934E-16, 1.836970198721010706E-16, -1.000000000000000000 ) ) ;
#57770 = AXIS2_PLACEMENT_3D ( 'NONE', #12006, #22974, #27944 ) ;
#57771 = VERTEX_POINT ( 'NONE', #23804 ) ;
#57772 = CARTESIAN_POINT ( 'NONE',  ( -7.250000000000000888, 7.250000000000001776, -7.500000000000000000 ) ) ;
#57773 = DIRECTION ( 'NONE',  ( 0.000000000000000000, 0.000000000000000000, -1.000000000000000000 ) ) ;
#57774 = VECTOR ( 'NONE', #34615, 1000.000000000000000 ) ;
#57775 = CARTESIAN_POINT ( 'NONE',  ( 0.000000000000000000, -7.449999999999998401, -23.50000000000000000 ) ) ;
#57776 = VERTEX_POINT ( 'NONE', #29109 ) ;
#57777 = LINE ( 'NONE', #15000, #50567 ) ;
#57778 = DIRECTION ( 'NONE',  ( 8.728482790395504563E-15, 1.000000000000000000, 3.673940397442059868E-16 ) ) ;
#57779 = DIRECTION ( 'NONE',  ( 0.000000000000000000, -0.6787500000000000755, -0.7343694148723788340 ) ) ;
#57780 = VECTOR ( 'NONE', #27984, 1000.000000000000000 ) ;
#57781 = CLOSED_SHELL ( 'NONE', ( #68355, #58351, #47119, #6792, #4688, #55198, #1367, #34065, #50388, #41870 ) ) ;
#57782 = EDGE_LOOP ( 'NONE', ( #52424, #3561, #63816, #16723 ) ) ;
#57783 = CARTESIAN_POINT ( 'NONE',  ( 275.0000000000000000, -32.44999999999905071, -13.20000000000091944 ) ) ;
#57784 = DIRECTION ( 'NONE',  ( 0.000000000000000000, 1.000000000000000000, 0.000000000000000000 ) ) ;
#57785 = DIRECTION ( 'NONE',  ( 0.000000000000000000, 0.000000000000000000, 1.000000000000000000 ) ) ;
#57786 = ORIENTED_EDGE ( 'NONE', *, *, #50287, .F. ) ;
#57787 = PLANE ( 'NONE',  #20293 ) ;
#57788 = DIRECTION ( 'NONE',  ( -4.336808689942025625E-15, -1.000000000000000000, 0.000000000000000000 ) ) ;
#57789 = FACE_OUTER_BOUND ( 'NONE', #39780, .T. ) ;
#57790 = VECTOR ( 'NONE', #43172, 1000.000000000000000 ) ;
#57791 = DIRECTION ( 'NONE',  ( 1.836970198721029934E-16, 1.836970198721010706E-16, -1.000000000000000000 ) ) ;
#57792 = CARTESIAN_POINT ( 'NONE',  ( 3.003254798005744242, -6.872275254348413576, 54.00000000000000711 ) ) ;
#57794 = VERTEX_POINT ( 'NONE', #17450 ) ;
#57793 = EDGE_CURVE ( 'NONE', #31832, #13993, #44315, .T. ) ;
#57795 = DIRECTION ( 'NONE',  ( -1.000000000000000000, 0.000000000000000000, 0.000000000000000000 ) ) ;
#57796 = CARTESIAN_POINT ( 'NONE',  ( -6.467976262117279163, -5.257023737882803083, 54.00000000000000711 ) ) ;
#57797 = DIRECTION ( 'NONE',  ( 0.000000000000000000, -2.854859206170826497E-12, -1.000000000000000000 ) ) ;
#57798 =( LENGTH_UNIT ( ) NAMED_UNIT ( * ) SI_UNIT ( .MILLI., .METRE. ) );
#57799 = EDGE_CURVE ( 'NONE', #50438, #46957, #44657, .T. ) ;
#57800 = DIRECTION ( 'NONE',  ( 0.000000000000000000, 0.000000000000000000, 1.000000000000000000 ) ) ;
#57801 = VERTEX_POINT ( 'NONE', #1207 ) ;
#57803 = ORIENTED_EDGE ( 'NONE', *, *, #3536, .T. ) ;
#57802 = FACE_OUTER_BOUND ( 'NONE', #35618, .T. ) ;
#57804 = LINE ( 'NONE', #4776, #51923 ) ;
#57805 = CARTESIAN_POINT ( 'NONE',  ( -7.250000000000000888, -8.249999999999998224, -22.00000000000000000 ) ) ;
#57806 = LINE ( 'NONE', #4082, #36439 ) ;
#57808 = VERTEX_POINT ( 'NONE', #54961 ) ;
#57807 = EDGE_CURVE ( 'NONE', #17836, #26867, #45359, .T. ) ;
#57809 = CARTESIAN_POINT ( 'NONE',  ( -10.03972626211731978, -8.930623737882752877, 54.00000000000000711 ) ) ;
#57810 = CARTESIAN_POINT ( 'NONE',  ( 9.900000000000000355, 18.00000000000000355, 21.00000000000000000 ) ) ;
#57811 = VERTEX_POINT ( 'NONE', #49634 ) ;
#57812 = ORIENTED_EDGE ( 'NONE', *, *, #7717, .F. ) ;
#57813 = ADVANCED_FACE ( 'NONE', ( #65889 ), #12485, .F. ) ;
#57814 = ORIENTED_EDGE ( 'NONE', *, *, #55708, .T. ) ;
#57815 = DIRECTION ( 'NONE',  ( -1.000000000000000000, 0.000000000000000000, 0.000000000000000000 ) ) ;
#57816 = AXIS2_PLACEMENT_3D ( 'NONE', #35667, #9163, #41328 ) ;
#57817 = CARTESIAN_POINT ( 'NONE',  ( 24.00000000000000000, -16.64230188589300141, 14.64519951917099583 ) ) ;
#57818 = PLANE ( 'NONE',  #8906 ) ;
#57819 = LINE ( 'NONE', #69134, #928 ) ;
#57820 = EDGE_CURVE ( 'NONE', #64281, #1632, #2556, .T. ) ;
#57821 = VERTEX_POINT ( 'NONE', #67294 ) ;
#57822 = VERTEX_POINT ( 'NONE', #45012 ) ;
#57823 = VECTOR ( 'NONE', #65819, 1000.000000000000000 ) ;
#57824 = CARTESIAN_POINT ( 'NONE',  ( -11.18071654964677997, -12.00648345035332554, 195.0000000000000284 ) ) ;
#57825 = PLANE ( 'NONE',  #38425 ) ;
#57826 = ORIENTED_EDGE ( 'NONE', *, *, #32986, .T. ) ;
#57827 = ORIENTED_EDGE ( 'NONE', *, *, #26258, .F. ) ;
#57828 = VECTOR ( 'NONE', #15737, 1000.000000000000000 ) ;
#57829 = ORIENTED_EDGE ( 'NONE', *, *, #991, .T. ) ;
#57830 = ORIENTED_EDGE ( 'NONE', *, *, #985, .T. ) ;
#57831 = LINE ( 'NONE', #57136, #49682 ) ;
#57832 = UNCERTAINTY_MEASURE_WITH_UNIT (LENGTH_MEASURE( 1.000000000000000082E-05 ), #8524, 'distance_accuracy_value', 'NONE');
#57833 = ADVANCED_FACE ( 'NONE', ( #22763 ), #61264, .F. ) ;
#57835 = VERTEX_POINT ( 'NONE', #66588 ) ;
#57834 = LINE ( 'NONE', #63504, #22055 ) ;
#57836 = AXIS2_PLACEMENT_3D ( 'NONE', #56496, #51192, #57201 ) ;
#57837 = EDGE_CURVE ( 'NONE', #16097, #36514, #34389, .T. ) ;
#57838 = CARTESIAN_POINT ( 'NONE',  ( 2.369523737882793135, -8.835729544836311788, 26.00000000000000000 ) ) ;
#57840 = PLANE ( 'NONE',  #38538 ) ;
#57839 = AXIS2_PLACEMENT_3D ( 'NONE', #42411, #9903, #31473 ) ;
#57841 = ORIENTED_EDGE ( 'NONE', *, *, #42294, .F. ) ;
#57842 = ORIENTED_EDGE ( 'NONE', *, *, #67633, .F. ) ;
#57843 = CIRCLE ( 'NONE', #40922, 24.99999999998784972 ) ;
#57844 = EDGE_CURVE ( 'NONE', #26597, #587, #22902, .T. ) ;
#57845 = DIRECTION ( 'NONE',  ( 0.000000000000000000, 0.000000000000000000, -1.000000000000000000 ) ) ;
#57846 = LINE ( 'NONE', #41939, #34896 ) ;
#57847 = EDGE_LOOP ( 'NONE', ( #37382, #23495, #59648, #49086 ) ) ;
#57848 =( NAMED_UNIT ( * ) SI_UNIT ( $, .STERADIAN. ) SOLID_ANGLE_UNIT ( ) );
#57849 = PLANE ( 'NONE',  #20024 ) ;
#57850 = CARTESIAN_POINT ( 'NONE',  ( 15.89999999999999680, -0.2000000000089119934, 8.909539772616881237E-12 ) ) ;
#57851 = EDGE_LOOP ( 'NONE', ( #25096, #13724, #59429, #44996 ) ) ;
#57852 = DIRECTION ( 'NONE',  ( 0.000000000000000000, 1.000000000000000000, 0.000000000000000000 ) ) ;
#57853 = CARTESIAN_POINT ( 'NONE',  ( -7.250000000000001776, -7.249999999999998224, -10.50000000000000000 ) ) ;
#57854 = CARTESIAN_POINT ( 'NONE',  ( -9.690000000000001279, 8.750000000000000000, -5.000000000000000000 ) ) ;
#57855 = LINE ( 'NONE', #41241, #11020 ) ;
#57856 = CIRCLE ( 'NONE', #34120, 0.5000000000009372503 ) ;
#57857 = EDGE_CURVE ( 'NONE', #69389, #31564, #61291, .T. ) ;
#57858 = CARTESIAN_POINT ( 'NONE',  ( 39.00000000000000000, -21.00000000000000000, 16.96999999999999886 ) ) ;
#57859 = ORIENTED_EDGE ( 'NONE', *, *, #19385, .F. ) ;
#57860 = CARTESIAN_POINT ( 'NONE',  ( 8.093267424590464998, -8.711985858128699078, 54.00000000000000711 ) ) ;
#57861 = CARTESIAN_POINT ( 'NONE',  ( -9.722976262117249746, -3.682023737882726522, 54.00000000000000711 ) ) ;
#57862 = AXIS2_PLACEMENT_3D ( 'NONE', #24287, #4133, #67065 ) ;
#57863 = CARTESIAN_POINT ( 'NONE',  ( 7.826483450353374671, 11.99351654964662295, 195.0000000000000284 ) ) ;
#57864 = EDGE_CURVE ( 'NONE', #42030, #62306, #37619, .T. ) ;
#57865 = DIRECTION ( 'NONE',  ( 0.000000000000000000, -0.000000000000000000, 1.000000000000000000 ) ) ;
#57866 = DIRECTION ( 'NONE',  ( -0.000000000000000000, -0.000000000000000000, -1.000000000000000000 ) ) ;
#57867 = DIRECTION ( 'NONE',  ( 1.000000000000000000, 0.000000000000000000, 0.000000000000000000 ) ) ;
#57868 = EDGE_CURVE ( 'NONE', #45355, #22560, #46069, .T. ) ;
#57869 = AXIS2_PLACEMENT_3D ( 'NONE', #49562, #27312, #16005 ) ;
#57870 = CYLINDRICAL_SURFACE ( 'NONE', #27804, 0.3499999999999996447 ) ;
#57871 = CYLINDRICAL_SURFACE ( 'NONE', #19494, 0.1750000000000002387 ) ;
#57872 = EDGE_LOOP ( 'NONE', ( #27574, #50644, #12705, #7114 ) ) ;
#57873 = CARTESIAN_POINT ( 'NONE',  ( 15.50000000000000000, -0.2038245569916604938, 23.94337567297399971 ) ) ;
#57874 = EDGE_CURVE ( 'NONE', #69312, #20150, #19197, .T. ) ;
#57875 = CARTESIAN_POINT ( 'NONE',  ( 2.290483450353415495, 9.828310488885934504, 455.0000000000000568 ) ) ;
#57876 = DIRECTION ( 'NONE',  ( 0.000000000000000000, 0.000000000000000000, -1.000000000000000000 ) ) ;
#57877 = LINE ( 'NONE', #40210, #33496 ) ;
#57878 = LINE ( 'NONE', #25012, #7281 ) ;
#57879 = PLANE ( 'NONE',  #15052 ) ;
#57880 = ADVANCED_FACE ( 'NONE', ( #8583, #41469 ), #56677, .F. ) ;
#57881 = DIRECTION ( 'NONE',  ( 0.000000000000000000, -1.000000000000000000, 0.000000000000000000 ) ) ;
#57882 = VERTEX_POINT ( 'NONE', #46760 ) ;
#57883 = AXIS2_PLACEMENT_3D ( 'NONE', #35603, #8749, #30670 ) ;
#57884 = ORIENTED_EDGE ( 'NONE', *, *, #44076, .T. ) ;
#57885 = DIRECTION ( 'NONE',  ( 1.000000000000000000, -0.000000000000000000, -0.000000000000000000 ) ) ;
#57886 = DIRECTION ( 'NONE',  ( -1.836970198721029934E-16, 1.836970198721036590E-16, -1.000000000000000000 ) ) ;
#57888 = VERTEX_POINT ( 'NONE', #3994 ) ;
#57887 = EDGE_CURVE ( 'NONE', #62304, #35449, #13890, .T. ) ;
#57889 = CARTESIAN_POINT ( 'NONE',  ( 13.90000000000000213, 13.66939075806899240, -20.79999999999999361 ) ) ;
#57890 = EDGE_CURVE ( 'NONE', #29633, #21334, #29801, .T. ) ;
#57891 = AXIS2_PLACEMENT_3D ( 'NONE', #27440, #12204, #572 ) ;
#57892 = CARTESIAN_POINT ( 'NONE',  ( 3.664523737882820598, 10.49297626211720491, 54.00000000000000711 ) ) ;
#57893 = VERTEX_POINT ( 'NONE', #30506 ) ;
#57894 = EDGE_CURVE ( 'NONE', #42070, #64467, #40765, .T. ) ;
#57895 = EDGE_CURVE ( 'NONE', #3872, #5817, #52078, .T. ) ;
#57896 = LINE ( 'NONE', #26425, #50312 ) ;
#57897 = VERTEX_POINT ( 'NONE', #57377 ) ;
#57898 = CIRCLE ( 'NONE', #1464, 0.7499999999999997780 ) ;
#57899 = VERTEX_POINT ( 'NONE', #25921 ) ;
#57900 = LINE ( 'NONE', #41279, #36230 ) ;
#57901 = VERTEX_POINT ( 'NONE', #25568 ) ;
#57902 = EDGE_LOOP ( 'NONE', ( #61627, #21744, #48069, #54104 ) ) ;
#57903 = ADVANCED_FACE ( 'NONE', ( #2935 ), #30158, .F. ) ;
#57904 = FACE_OUTER_BOUND ( 'NONE', #38985, .T. ) ;
#57905 = CARTESIAN_POINT ( 'NONE',  ( 146.5599459900709860, 5.000000000000000000, 284.4801873289890182 ) ) ;
#57906 = CARTESIAN_POINT ( 'NONE',  ( 15.00000000000000000, -25.93000000000544958, -9.412893218815410634 ) ) ;
#57907 = AXIS2_PLACEMENT_3D ( 'NONE', #23742, #30451, #36094 ) ;
#57908 = ORIENTED_EDGE ( 'NONE', *, *, #5494, .T. ) ;
#57909 = DIRECTION ( 'NONE',  ( 1.836970198721029934E-16, 1.836970198721010706E-16, -1.000000000000000000 ) ) ;
#57911 = LINE ( 'NONE', #63579, #9652 ) ;
#57910 = CARTESIAN_POINT ( 'NONE',  ( 275.0000000000000000, -25.00000000000000000, 17.50000000000000000 ) ) ;
#57912 = EDGE_LOOP ( 'NONE', ( #19641, #46006, #36457, #3200 ) ) ;
#57913 = ORIENTED_EDGE ( 'NONE', *, *, #17971, .F. ) ;
#57914 = VECTOR ( 'NONE', #49622, 1000.000000000000000 ) ;
#57915 = VERTEX_POINT ( 'NONE', #41105 ) ;
#57916 = PRODUCT_CONTEXT ( 'NONE', #10589, 'mechanical' ) ;
#57917 = DIRECTION ( 'NONE',  ( -1.000000000000000000, 0.000000000000000000, 0.000000000000000000 ) ) ;
#57918 = VECTOR ( 'NONE', #65331, 1000.000000000000000 ) ;
#57919 = EDGE_CURVE ( 'NONE', #28197, #44220, #31962, .T. ) ;
#57921 = ORIENTED_EDGE ( 'NONE', *, *, #35295, .F. ) ;
#57920 = CARTESIAN_POINT ( 'NONE',  ( -7.250000000000000888, -8.249999999999998224, -23.50000000000000000 ) ) ;
#57922 = ADVANCED_FACE ( 'NONE', ( #24856, #46414, #9295, #30860, #19541, #58078, #67991, #14253, #35806, #3642 ), #25207, .T. ) ;
#57923 = DIRECTION ( 'NONE',  ( -1.000000000000000000, 0.000000000000000000, 0.000000000000000000 ) ) ;
#57924 = CARTESIAN_POINT ( 'NONE',  ( -14.25000000000000000, -2.500000000000000000, 21.77831216351300014 ) ) ;
#57925 = ORIENTED_EDGE ( 'NONE', *, *, #12459, .F. ) ;
#57926 = ORIENTED_EDGE ( 'NONE', *, *, #24990, .T. ) ;
#57927 = CARTESIAN_POINT ( 'NONE',  ( -1.466476262117236029, 8.598420958951576765, 54.00000000000000711 ) ) ;
#57928 = VERTEX_POINT ( 'NONE', #52433 ) ;
#57929 = CARTESIAN_POINT ( 'NONE',  ( 18.85410196625000268, -15.50000000000000000, 21.50000000000000000 ) ) ;
#57930 = DIRECTION ( 'NONE',  ( 0.000000000000000000, -3.673940397442059868E-16, 1.000000000000000000 ) ) ;
#57931 = CARTESIAN_POINT ( 'NONE',  ( -11.00000000000000000, -14.33999999999999986, -14.50000000000000000 ) ) ;
#57932 = ORIENTED_EDGE ( 'NONE', *, *, #35332, .F. ) ;
#57933 = EDGE_CURVE ( 'NONE', #13530, #20828, #1451, .T. ) ;
#57934 = AXIS2_PLACEMENT_3D ( 'NONE', #68340, #57724, #31230 ) ;
#57935 = DIRECTION ( 'NONE',  ( 0.000000000000000000, 0.7071067811865475727, 0.7071067811865475727 ) ) ;
#57936 = CARTESIAN_POINT ( 'NONE',  ( 30.00000000000000000, -5.200000000000001066, -26.25000000000000000 ) ) ;
#57937 = VERTEX_POINT ( 'NONE', #41812 ) ;
#57939 = ORIENTED_EDGE ( 'NONE', *, *, #45179, .T. ) ;
#57938 = LINE ( 'NONE', #9507, #2707 ) ;
#57941 = DIRECTION ( 'NONE',  ( 1.836970198721029934E-16, -1.836970198721036344E-16, 1.000000000000000000 ) ) ;
#57940 = AXIS2_PLACEMENT_3D ( 'NONE', #45424, #50390, #45075 ) ;
#57942 =( GEOMETRIC_REPRESENTATION_CONTEXT ( 3 ) GLOBAL_UNCERTAINTY_ASSIGNED_CONTEXT ( ( #5504 ) ) GLOBAL_UNIT_ASSIGNED_CONTEXT ( ( #41262, #14756, #67086 ) ) REPRESENTATION_CONTEXT ( 'NONE', 'WORKASPACE' ) );
#57943 = CARTESIAN_POINT ( 'NONE',  ( 283.0000000000000568, -21.00000000000000000, 12.50000000000000000 ) ) ;
#57944 = LINE ( 'NONE', #20813, #12111 ) ;
#57945 = CARTESIAN_POINT ( 'NONE',  ( 8.250000000000005329, -7.249999999999998224, -18.00000000000000000 ) ) ;
#57946 = PRESENTATION_LAYER_ASSIGNMENT (  '', '', ( #7153 ) ) ;
#57947 = AXIS2_PLACEMENT_3D ( 'NONE', #68482, #15084, #41601 ) ;
#57948 = DIRECTION ( 'NONE',  ( 0.7071067811865401342, -0.7071067811865550112, -1.367410260514937456E-30 ) ) ;
#57949 = ORIENTED_EDGE ( 'NONE', *, *, #66656, .F. ) ;
#57950 = LINE ( 'NONE', #42039, #23401 ) ;
#57951 = DIRECTION ( 'NONE',  ( -0.6414496315691521344, -0.7671651518153043137, -2.309356642088964526E-17 ) ) ;
#57952 = SURFACE_STYLE_FILL_AREA ( #63265 ) ;
#57953 = ADVANCED_FACE ( 'NONE', ( #63389 ), #14951, .F. ) ;
#57955 = ORIENTED_EDGE ( 'NONE', *, *, #37497, .F. ) ;
#57954 = LINE ( 'NONE', #42740, #19818 ) ;
#57956 = CARTESIAN_POINT ( 'NONE',  ( -9.828310488886049967, -2.290483450353357320, 455.0000000000000568 ) ) ;
#57957 = DIRECTION ( 'NONE',  ( 0.000000000000000000, -1.000000000000000000, 0.000000000000000000 ) ) ;
#57958 = EDGE_CURVE ( 'NONE', #57686, #14101, #20593, .T. ) ;
#57959 = CARTESIAN_POINT ( 'NONE',  ( 0.000000000000000000, 8.250000000000001776, -23.50000000000000000 ) ) ;
#57960 = ORIENTED_EDGE ( 'NONE', *, *, #5087, .F. ) ;
#57961 = FACE_OUTER_BOUND ( 'NONE', #44216, .T. ) ;
#57962 = EDGE_CURVE ( 'NONE', #45972, #3676, #48179, .T. ) ;
#57963 = DIRECTION ( 'NONE',  ( -1.000000000000000000, 0.000000000000000000, 0.000000000000000000 ) ) ;
#57964 = VECTOR ( 'NONE', #14937, 1000.000000000000000 ) ;
#57965 = VERTEX_POINT ( 'NONE', #10002 ) ;
#57966 = CARTESIAN_POINT ( 'NONE',  ( 2.369523737882786918, -9.562023737882798358, 54.00000000000000711 ) ) ;
#57967 = DIRECTION ( 'NONE',  ( -1.000000000000000000, 0.000000000000000000, 0.000000000000000000 ) ) ;
#57968 = FACE_OUTER_BOUND ( 'NONE', #50827, .T. ) ;
#57969 = EDGE_CURVE ( 'NONE', #57893, #16799, #59823, .T. ) ;
#57970 = EDGE_CURVE ( 'NONE', #26906, #40491, #69247, .T. ) ;
#57971 = AXIS2_PLACEMENT_3D ( 'NONE', #48015, #36351, #26110 ) ;
#57972 = DIRECTION ( 'NONE',  ( 0.000000000000000000, 0.000000000000000000, 1.000000000000000000 ) ) ;
#57973 = FACE_OUTER_BOUND ( 'NONE', #13456, .T. ) ;
#57974 = ORIENTED_EDGE ( 'NONE', *, *, #47494, .T. ) ;
#57975 = DIRECTION ( 'NONE',  ( 0.000000000000000000, 0.000000000000000000, 1.000000000000000000 ) ) ;
#57976 = ORIENTED_EDGE ( 'NONE', *, *, #36756, .T. ) ;
#57977 = ORIENTED_EDGE ( 'NONE', *, *, #29679, .T. ) ;
#57978 = ORIENTED_EDGE ( 'NONE', *, *, #15845, .T. ) ;
#57979 = EDGE_LOOP ( 'NONE', ( #42509, #1228, #8610, #8912 ) ) ;
#57980 = AXIS2_PLACEMENT_3D ( 'NONE', #62157, #25393, #9130 ) ;
#57981 = DIRECTION ( 'NONE',  ( 1.000000000000000000, -3.491481338843133355E-15, -1.836970198721036344E-16 ) ) ;
#57982 = DIRECTION ( 'NONE',  ( -5.981805089575196197E-17, -1.000000000000000000, 0.000000000000000000 ) ) ;
#57983 = DIRECTION ( 'NONE',  ( 1.000000000000000000, 0.000000000000000000, 0.000000000000000000 ) ) ;
#57984 = EDGE_LOOP ( 'NONE', ( #4091, #52839, #65123, #20165 ) ) ;
#57985 = ORIENTED_EDGE ( 'NONE', *, *, #40574, .F. ) ;
#57986 = DIRECTION ( 'NONE',  ( -0.000000000000000000, -0.000000000000000000, -1.000000000000000000 ) ) ;
#57987 = EDGE_LOOP ( 'NONE', ( #13719, #14456, #66529, #38788 ) ) ;
#57988 = ORIENTED_EDGE ( 'NONE', *, *, #54669, .T. ) ;
#57989 = DIRECTION ( 'NONE',  ( -1.794541526872559352E-16, -1.000000000000000000, 0.000000000000000000 ) ) ;
#57990 = CARTESIAN_POINT ( 'NONE',  ( 15.50000000000000000, -2.500000000000000000, -21.05662432702600029 ) ) ;
#57991 = AXIS2_PLACEMENT_3D ( 'NONE', #16675, #66127, #12359 ) ;
#57992 = CIRCLE ( 'NONE', #27503, 0.4000000000000010214 ) ;
#57993 = FACE_OUTER_BOUND ( 'NONE', #50692, .T. ) ;
#57994 = ORIENTED_EDGE ( 'NONE', *, *, #19011, .F. ) ;
#57995 = VECTOR ( 'NONE', #55112, 1000.000000000000000 ) ;
#57996 = FACE_OUTER_BOUND ( 'NONE', #52444, .T. ) ;
#57998 = LINE ( 'NONE', #53066, #36640 ) ;
#57997 = CARTESIAN_POINT ( 'NONE',  ( 5.552858015815571591, 7.342976262117199227, 54.00000000000000711 ) ) ;
#57999 = COLOUR_RGB ( '', 0.31764706, 0.68627451, 0.89019608) ;
#58001 = VERTEX_POINT ( 'NONE', #32949 ) ;
#58000 = VECTOR ( 'NONE', #56882, 1000.000000000000000 ) ;
#58003 = VERTEX_POINT ( 'NONE', #54527 ) ;
#58002 = FACE_OUTER_BOUND ( 'NONE', #32566, .T. ) ;
#58004 = ORIENTED_EDGE ( 'NONE', *, *, #2056, .T. ) ;
#58005 = AXIS2_PLACEMENT_3D ( 'NONE', #6082, #27640, #794 ) ;
#58006 = AXIS2_PLACEMENT_3D ( 'NONE', #23510, #12880, #45068 ) ;
#58007 = CARTESIAN_POINT ( 'NONE',  ( -4.727349090213559535, -7.811466277050794993, 455.0000000000000568 ) ) ;
#58008 = EDGE_CURVE ( 'NONE', #66944, #3209, #44343, .T. ) ;
#58009 = EDGE_CURVE ( 'NONE', #48363, #35816, #9390, .T. ) ;
#58010 = DIRECTION ( 'NONE',  ( 1.000000000000000000, 0.000000000000000000, 0.000000000000000000 ) ) ;
#58011 = ORIENTED_EDGE ( 'NONE', *, *, #59378, .F. ) ;
#58012 = VERTEX_POINT ( 'NONE', #4693 ) ;
#58013 = EDGE_CURVE ( 'NONE', #18037, #45394, #6083, .T. ) ;
#58014 = CARTESIAN_POINT ( 'NONE',  ( -9.689999999999999503, -10.50000000000000178, -5.000000000000000000 ) ) ;
#58015 = CARTESIAN_POINT ( 'NONE',  ( -29.50000000000000355, -15.46862696659690073, -14.50000000000000000 ) ) ;
#58016 = ORIENTED_EDGE ( 'NONE', *, *, #16855, .F. ) ;
#58017 = ORIENTED_EDGE ( 'NONE', *, *, #20279, .F. ) ;
#58018 = CARTESIAN_POINT ( 'NONE',  ( 146.5599459900709860, 5.000000000000000000, 316.5239988703752942 ) ) ;
#58019 = CARTESIAN_POINT ( 'NONE',  ( -15.50000000000000000, -1.037157890325000054, -19.00000000000000000 ) ) ;
#58020 = ORIENTED_EDGE ( 'NONE', *, *, #52563, .T. ) ;
#58021 = CARTESIAN_POINT ( 'NONE',  ( 49.00000000000000000, -0.1999999999911430404, -8.864436962241481021E-12 ) ) ;
#58022 = LINE ( 'NONE', #20542, #57672 ) ;
#58023 = EDGE_CURVE ( 'NONE', #30559, #35173, #5405, .T. ) ;
#58024 = AXIS2_PLACEMENT_3D ( 'NONE', #61331, #46130, #56389 ) ;
#58026 = ORIENTED_EDGE ( 'NONE', *, *, #62526, .T. ) ;
#58025 = PLANE ( 'NONE',  #55454 ) ;
#58028 = ORIENTED_EDGE ( 'NONE', *, *, #7024, .T. ) ;
#58027 = CARTESIAN_POINT ( 'NONE',  ( -7.250000000000000888, -8.249999999999998224, -8.500000000000000000 ) ) ;
#58029 = FACE_OUTER_BOUND ( 'NONE', #58348, .T. ) ;
#58030 = LINE ( 'NONE', #51690, #61176 ) ;
#58031 = DIRECTION ( 'NONE',  ( 0.000000000000000000, 0.000000000000000000, 1.000000000000000000 ) ) ;
#58032 = CARTESIAN_POINT ( 'NONE',  ( 6.364920264886885448, -3.677663764522618450, 26.00000000000000711 ) ) ;
#58033 = DIRECTION ( 'NONE',  ( -1.570596175624152290E-15, 1.000000000000000000, 3.673940397442059868E-16 ) ) ;
#58034 = FACE_OUTER_BOUND ( 'NONE', #36687, .T. ) ;
#58035 = ORIENTED_EDGE ( 'NONE', *, *, #68978, .T. ) ;
#58036 = LINE ( 'NONE', #14911, #12326 ) ;
#58038 = VERTEX_POINT ( 'NONE', #37570 ) ;
#58037 = CARTESIAN_POINT ( 'NONE',  ( 30.00000000000000000, -15.46862696659690073, 14.50000000000000000 ) ) ;
#58039 = ADVANCED_FACE ( 'NONE', ( #53151 ), #35350, .F. ) ;
#58040 = CYLINDRICAL_SURFACE ( 'NONE', #37857, 1.224999999999997868 ) ;
#58041 = VECTOR ( 'NONE', #10229, 1000.000000000000000 ) ;
#58042 = CIRCLE ( 'NONE', #465, 0.8099999999999999423 ) ;
#58043 = DIRECTION ( 'NONE',  ( -0.000000000000000000, -0.000000000000000000, -1.000000000000000000 ) ) ;
#58044 = DIRECTION ( 'NONE',  ( -1.000000000000000000, 0.000000000000000000, 0.000000000000000000 ) ) ;
#58045 = CARTESIAN_POINT ( 'NONE',  ( -7.793516549646712477, 11.31351654964660014, 455.0000000000000568 ) ) ;
#58046 = AXIS2_PLACEMENT_3D ( 'NONE', #60229, #49961, #55623 ) ;
#58047 = CIRCLE ( 'NONE', #51270, 1.000000000000000000 ) ;
#58048 = ORIENTED_EDGE ( 'NONE', *, *, #3134, .F. ) ;
#58049 = LINE ( 'NONE', #31196, #43302 ) ;
#58050 = EDGE_CURVE ( 'NONE', #61156, #46508, #42517, .T. ) ;
#58051 = DIRECTION ( 'NONE',  ( 0.000000000000000000, -3.673940397442059868E-16, 1.000000000000000000 ) ) ;
#58052 = EDGE_CURVE ( 'NONE', #66887, #67098, #68082, .T. ) ;
#58053 = ORIENTED_EDGE ( 'NONE', *, *, #58480, .F. ) ;
#58054 = LINE ( 'NONE', #46735, #50411 ) ;
#58055 = AXIS2_PLACEMENT_3D ( 'NONE', #46678, #4272, #4617 ) ;
#58056 = PRESENTATION_STYLE_ASSIGNMENT (( #64086 ) ) ;
#58057 = EDGE_CURVE ( 'NONE', #27455, #48929, #40964, .T. ) ;
#58058 = EDGE_CURVE ( 'NONE', #48724, #14752, #58447, .T. ) ;
#58059 = DIRECTION ( 'NONE',  ( -1.000000000000000000, 0.000000000000000000, 0.000000000000000000 ) ) ;
#58060 = EDGE_CURVE ( 'NONE', #8950, #30328, #25184, .T. ) ;
#58061 = ORIENTED_EDGE ( 'NONE', *, *, #45749, .F. ) ;
#58062 = DIRECTION ( 'NONE',  ( 1.000000000000000000, 0.000000000000000000, 0.000000000000000000 ) ) ;
#58063 = ORIENTED_EDGE ( 'NONE', *, *, #60908, .F. ) ;
#58064 = ORIENTED_EDGE ( 'NONE', *, *, #6841, .F. ) ;
#58065 = AXIS2_PLACEMENT_3D ( 'NONE', #61979, #56681, #8231 ) ;
#58066 = CARTESIAN_POINT ( 'NONE',  ( 41.09999999999999432, 13.66939075806899950, -20.80000000000000426 ) ) ;
#58067 = DIRECTION ( 'NONE',  ( 0.000000000000000000, 0.000000000000000000, -1.000000000000000000 ) ) ;
#58068 = CARTESIAN_POINT ( 'NONE',  ( 7.250000000000005329, 8.250000000000001776, -26.00000000000001066 ) ) ;
#58069 = DIRECTION ( 'NONE',  ( -0.000000000000000000, -0.000000000000000000, 1.000000000000000000 ) ) ;
#58070 = CARTESIAN_POINT ( 'NONE',  ( -24.00000000000000000, -15.50000000000000000, -19.33772233983200195 ) ) ;
#58071 = ORIENTED_EDGE ( 'NONE', *, *, #51776, .F. ) ;
#58072 = ORIENTED_EDGE ( 'NONE', *, *, #12557, .F. ) ;
#58074 = ORIENTED_EDGE ( 'NONE', *, *, #444, .F. ) ;
#58073 = LINE ( 'NONE', #19533, #46425 ) ;
#58075 = ORIENTED_EDGE ( 'NONE', *, *, #65055, .T. ) ;
#58076 = CARTESIAN_POINT ( 'NONE',  ( 275.0000000000000000, -21.00000000000000000, -17.50000000000000000 ) ) ;
#58077 = CARTESIAN_POINT ( 'NONE',  ( -10.08346604330797547, -9.306483450353381315, 455.0000000000000568 ) ) ;
#58078 = FACE_BOUND ( 'NONE', #40690, .T. ) ;
#58079 = AXIS2_PLACEMENT_3D ( 'NONE', #152, #38327, #54592 ) ;
#58080 = DIRECTION ( 'NONE',  ( 1.836970198721029934E-16, 1.836970198721010706E-16, -1.000000000000000000 ) ) ;
#58082 = DIRECTION ( 'NONE',  ( -1.836970198721029934E-16, 1.836970198721036590E-16, -1.000000000000000000 ) ) ;
#58081 = FACE_OUTER_BOUND ( 'NONE', #10573, .T. ) ;
#58083 = ORIENTED_EDGE ( 'NONE', *, *, #23528, .T. ) ;
#58084 = CIRCLE ( 'NONE', #27595, 0.1749999999999989342 ) ;
#58085 = ORIENTED_EDGE ( 'NONE', *, *, #48965, .T. ) ;
#58086 = ORIENTED_EDGE ( 'NONE', *, *, #11581, .T. ) ;
#58087 = ORIENTED_EDGE ( 'NONE', *, *, #18112, .T. ) ;
#58088 = CARTESIAN_POINT ( 'NONE',  ( 12.00648345035338238, 4.173516549646515195, 455.0000000000000568 ) ) ;
#58089 = DIRECTION ( 'NONE',  ( 0.000000000000000000, 1.000000000000000000, 0.000000000000000000 ) ) ;
#58090 = CARTESIAN_POINT ( 'NONE',  ( 85.07737089618306925, 47.45351654964651544, 253.7837994620735742 ) ) ;
#58091 = AXIS2_PLACEMENT_3D ( 'NONE', #24923, #3708, #46483 ) ;
#58093 = DIRECTION ( 'NONE',  ( 1.000000000000000000, 0.000000000000000000, 0.000000000000000000 ) ) ;
#58092 = AXIS2_PLACEMENT_3D ( 'NONE', #43222, #38618, #21666 ) ;
#58094 = ORIENTED_EDGE ( 'NONE', *, *, #4549, .T. ) ;
#58095 = ORIENTED_EDGE ( 'NONE', *, *, #32099, .F. ) ;
#58096 = EDGE_LOOP ( 'NONE', ( #49233, #22667, #950, #63760 ) ) ;
#58097 = EDGE_CURVE ( 'NONE', #25429, #34832, #43205, .T. ) ;
#58098 = EDGE_CURVE ( 'NONE', #8587, #3391, #46617, .T. ) ;
#58099 = FACE_OUTER_BOUND ( 'NONE', #8596, .T. ) ;
#58100 = VERTEX_POINT ( 'NONE', #5035 ) ;
#58101 = CIRCLE ( 'NONE', #28707, 0.9999999999999991118 ) ;
#58102 = VECTOR ( 'NONE', #31621, 1000.000000000000000 ) ;
#58103 = ORIENTED_EDGE ( 'NONE', *, *, #32950, .T. ) ;
#58104 = CARTESIAN_POINT ( 'NONE',  ( 105.8309041053263257, 63.65740854044500452, 2.000000000000000000 ) ) ;
#58105 = ADVANCED_FACE ( 'NONE', ( #11036 ), #32613, .T. ) ;
#58106 = EDGE_LOOP ( 'NONE', ( #62031, #27934, #30176, #19629 ) ) ;
#58107 = VERTEX_POINT ( 'NONE', #27307 ) ;
#58108 = LINE ( 'NONE', #59151, #27158 ) ;
#58109 = AXIS2_PLACEMENT_3D ( 'NONE', #56168, #7708, #29267 ) ;
#58111 = ORIENTED_EDGE ( 'NONE', *, *, #69100, .F. ) ;
#58110 = PLANE ( 'NONE',  #61590 ) ;
#58112 = VERTEX_POINT ( 'NONE', #48872 ) ;
#58113 = DIRECTION ( 'NONE',  ( -0.000000000000000000, -0.000000000000000000, -1.000000000000000000 ) ) ;
#58114 = DIRECTION ( 'NONE',  ( 0.000000000000000000, 0.000000000000000000, -1.000000000000000000 ) ) ;
#58115 = CIRCLE ( 'NONE', #36654, 2.204799999999997429 ) ;
#58117 = ORIENTED_EDGE ( 'NONE', *, *, #1372, .F. ) ;
#58116 = CARTESIAN_POINT ( 'NONE',  ( 9.306483450353379538, -10.09643294401456259, 195.0000000000000284 ) ) ;
#58118 = VECTOR ( 'NONE', #9927, 1000.000000000000114 ) ;
#58119 = ORIENTED_EDGE ( 'NONE', *, *, #68476, .T. ) ;
#58120 = CARTESIAN_POINT ( 'NONE',  ( 30.00000000000000000, -16.28999999999710369, -15.00000000000794920 ) ) ;
#58121 = DIRECTION ( 'NONE',  ( -1.000000000000000000, 0.000000000000000000, 0.000000000000000000 ) ) ;
#58122 = FACE_OUTER_BOUND ( 'NONE', #69972, .T. ) ;
#58123 = LINE ( 'NONE', #62364, #64374 ) ;
#58124 = VERTEX_POINT ( 'NONE', #21993 ) ;
#58125 = DIRECTION ( 'NONE',  ( -1.836970198721029934E-16, 1.836970198721036344E-16, -1.000000000000000000 ) ) ;
#58126 = CARTESIAN_POINT ( 'NONE',  ( 4.747751991980663000, 5.380658396643107189, 455.0000000000000568 ) ) ;
#58127 = CARTESIAN_POINT ( 'NONE',  ( 8.250000000000005329, 7.250000000000000888, -26.00000000000001066 ) ) ;
#58128 = AXIS2_PLACEMENT_3D ( 'NONE', #24411, #67190, #62230 ) ;
#58129 = FACE_OUTER_BOUND ( 'NONE', #37039, .T. ) ;
#58130 = CARTESIAN_POINT ( 'NONE',  ( 277.0217896459287203, -25.18021646000300606, 17.31978353999699749 ) ) ;
#58131 = CARTESIAN_POINT ( 'NONE',  ( -30.00000000000000000, -5.200000000000001066, 26.59999999999999787 ) ) ;
#58132 = AXIS2_PLACEMENT_3D ( 'NONE', #32421, #53989, #5542 ) ;
#58133 = ORIENTED_EDGE ( 'NONE', *, *, #65490, .T. ) ;
#58134 = SURFACE_STYLE_USAGE ( .BOTH. , #47530 ) ;
#58135 = ADVANCED_FACE ( 'NONE', ( #43554 ), #38266, .F. ) ;
#58136 = DIRECTION ( 'NONE',  ( 0.000000000000000000, -1.000000000000000000, 0.000000000000000000 ) ) ;
#58137 = ADVANCED_FACE ( 'NONE', ( #56247 ), #23377, .F. ) ;
#58138 = VECTOR ( 'NONE', #13059, 1000.000000000000000 ) ;
#58139 = AXIS2_PLACEMENT_3D ( 'NONE', #49829, #22949, #27922 ) ;
#58140 = EDGE_CURVE ( 'NONE', #3647, #2847, #44575, .T. ) ;
#58141 = DIRECTION ( 'NONE',  ( 0.000000000000000000, -3.673940397442059868E-16, 1.000000000000000000 ) ) ;
#58142 = EDGE_LOOP ( 'NONE', ( #23784, #63911, #10122, #57164 ) ) ;
#58143 = DIRECTION ( 'NONE',  ( 0.000000000000000000, 1.000000000000000000, 0.000000000000000000 ) ) ;
#58144 = CARTESIAN_POINT ( 'NONE',  ( -3.667976262117328190, -9.737023737882820384, 54.00000000000000711 ) ) ;
#58145 = EDGE_CURVE ( 'NONE', #48513, #2608, #44238, .T. ) ;
#58146 = LINE ( 'NONE', #36221, #33106 ) ;
#58147 = CARTESIAN_POINT ( 'NONE',  ( 40.90000000000000568, -16.96999999999999886, -21.00000000000000000 ) ) ;
#58148 = LINE ( 'NONE', #30575, #9363 ) ;
#58149 = AXIS2_PLACEMENT_3D ( 'NONE', #66069, #61105, #7363 ) ;
#58150 = VERTEX_POINT ( 'NONE', #12395 ) ;
#58151 = DIRECTION ( 'NONE',  ( -0.000000000000000000, -0.000000000000000000, 1.000000000000000000 ) ) ;
#58152 = CARTESIAN_POINT ( 'NONE',  ( 0.000000000000000000, 0.000000000000000000, -21.50000000000000000 ) ) ;
#58153 = DIRECTION ( 'NONE',  ( 1.000000000000000000, -0.000000000000000000, 0.000000000000000000 ) ) ;
#58154 = VECTOR ( 'NONE', #8771, 1000.000000000000000 ) ;
#58155 = LINE ( 'NONE', #58525, #2662 ) ;
#58156 = EDGE_CURVE ( 'NONE', #42522, #29082, #29360, .T. ) ;
#58157 = CARTESIAN_POINT ( 'NONE',  ( -8.697938382363135545, 2.406732575409538111, 54.00000000000000711 ) ) ;
#58158 = VERTEX_POINT ( 'NONE', #50241 ) ;
#58160 = VERTEX_POINT ( 'NONE', #17369 ) ;
#58159 = CARTESIAN_POINT ( 'NONE',  ( 39.90000000000000568, 21.00000000000000000, -16.96999999999999886 ) ) ;
#58161 = EDGE_CURVE ( 'NONE', #17846, #11392, #66844, .T. ) ;
#58162 = CIRCLE ( 'NONE', #22026, 0.1999999999999987899 ) ;
#58163 = DIRECTION ( 'NONE',  ( 1.836970198721029934E-16, 1.836970198721010706E-16, -1.000000000000000000 ) ) ;
#58164 = DIRECTION ( 'NONE',  ( -1.000000000000000000, 0.000000000000000000, 0.000000000000000000 ) ) ;
#58165 = CIRCLE ( 'NONE', #33329, 4.000000000000000888 ) ;
#58166 = LINE ( 'NONE', #31318, #64654 ) ;
#58167 = ORIENTED_EDGE ( 'NONE', *, *, #51999, .F. ) ;
#58168 = AXIS2_PLACEMENT_3D ( 'NONE', #15773, #17415, #6125 ) ;
#58169 = CYLINDRICAL_SURFACE ( 'NONE', #49168, 0.3999999999993835154 ) ;
#58170 = CARTESIAN_POINT ( 'NONE',  ( 9.247904806590725002, 9.942044687070426434, 455.0000000000000568 ) ) ;
#58171 = ORIENTED_EDGE ( 'NONE', *, *, #5743, .F. ) ;
#58172 = VERTEX_POINT ( 'NONE', #66158 ) ;
#58173 = ORIENTED_EDGE ( 'NONE', *, *, #28837, .T. ) ;
#58174 = CARTESIAN_POINT ( 'NONE',  ( 11.00000000000000000, -13.54524521594299991, -17.53999999999999915 ) ) ;
#58175 = FACE_OUTER_BOUND ( 'NONE', #57912, .T. ) ;
#58176 = LINE ( 'NONE', #37320, #8824 ) ;
#58177 = VERTEX_POINT ( 'NONE', #49556 ) ;
#58178 = ORIENTED_EDGE ( 'NONE', *, *, #26718, .T. ) ;
#58179 = CARTESIAN_POINT ( 'NONE',  ( 30.00000000000000000, -17.35230188589299871, 15.35019951917099945 ) ) ;
#58180 = DIRECTION ( 'NONE',  ( 0.4999999999989410693, 0.000000000000000000, 0.8660254037850499964 ) ) ;
#58181 = ORIENTED_EDGE ( 'NONE', *, *, #65783, .F. ) ;
#58182 = VECTOR ( 'NONE', #14938, 1000.000000000000000 ) ;
#58183 = ORIENTED_EDGE ( 'NONE', *, *, #27808, .F. ) ;
#58184 = ADVANCED_FACE ( 'NONE', ( #54872, #22353 ), #7449, .F. ) ;
#58185 = ORIENTED_EDGE ( 'NONE', *, *, #31491, .F. ) ;
#58186 = ORIENTED_EDGE ( 'NONE', *, *, #38243, .T. ) ;
#58187 = CIRCLE ( 'NONE', #49154, 24.99999999998784972 ) ;
#58188 = DIRECTION ( 'NONE',  ( 1.221996412923863792E-14, 1.000000000000000000, 1.836970198721013910E-16 ) ) ;
#58190 = VERTEX_POINT ( 'NONE', #33639 ) ;
#58189 = LINE ( 'NONE', #46520, #66093 ) ;
#58191 = PLANE ( 'NONE',  #32319 ) ;
#58192 = AXIS2_PLACEMENT_3D ( 'NONE', #55098, #54744, #6298 ) ;
#58193 = VECTOR ( 'NONE', #15831, 1000.000000000000000 ) ;
#58194 = CARTESIAN_POINT ( 'NONE',  ( -7.450000000000001954, 0.000000000000000000, -22.50000000000000000 ) ) ;
#58195 = CIRCLE ( 'NONE', #66046, 0.3999999999999993006 ) ;
#58196 = DIRECTION ( 'NONE',  ( -1.000000000000000000, 0.000000000000000000, 0.000000000000000000 ) ) ;
#58197 = ORIENTED_EDGE ( 'NONE', *, *, #39388, .T. ) ;
#58198 = VERTEX_POINT ( 'NONE', #1454 ) ;
#58199 = VECTOR ( 'NONE', #59308, 1000.000000000000000 ) ;
#58200 = EDGE_CURVE ( 'NONE', #48227, #60663, #7095, .T. ) ;
#58201 = PLANE ( 'NONE',  #44693 ) ;
#58202 = VECTOR ( 'NONE', #28005, 1000.000000000000000 ) ;
#58203 = ADVANCED_FACE ( 'NONE', ( #6432, #43898 ), #33296, .T. ) ;
#58204 = CARTESIAN_POINT ( 'NONE',  ( -4.393516549646667713, 11.77351654964658856, 455.0000000000000568 ) ) ;
#58205 = ORIENTED_EDGE ( 'NONE', *, *, #33509, .T. ) ;
#58206 = AXIS2_PLACEMENT_3D ( 'NONE', #5461, #58136, #42573 ) ;
#58207 = CARTESIAN_POINT ( 'NONE',  ( 7.250000000000005329, -7.249999999999998224, -10.50000000000000000 ) ) ;
#58208 = FACE_OUTER_BOUND ( 'NONE', #15753, .T. ) ;
#58209 = DIRECTION ( 'NONE',  ( 1.047444401652940007E-14, 1.000000000000000000, 1.836970198721029934E-16 ) ) ;
#58210 = VERTEX_POINT ( 'NONE', #33969 ) ;
#58211 = DIRECTION ( 'NONE',  ( 0.000000000000000000, 1.000000000000000000, -0.000000000000000000 ) ) ;
#58212 = DIRECTION ( 'NONE',  ( 0.6414496315691537998, -0.7671651518153029814, -2.309356642088714309E-17 ) ) ;
#58213 = CARTESIAN_POINT ( 'NONE',  ( 41.09999999999999432, 13.66939075806899950, 20.80000000000000426 ) ) ;
#58214 = LINE ( 'NONE', #41951, #43770 ) ;
#58215 = EDGE_CURVE ( 'NONE', #9315, #35140, #61181, .T. ) ;
#58216 = CARTESIAN_POINT ( 'NONE',  ( -1.466476262117236029, 8.598420958951576765, 54.00000000000000711 ) ) ;
#58217 = VERTEX_POINT ( 'NONE', #60504 ) ;
#58218 = DIRECTION ( 'NONE',  ( 0.7071067811865401342, -0.7071067811865549002, 0.000000000000000000 ) ) ;
#58219 = FACE_OUTER_BOUND ( 'NONE', #27021, .T. ) ;
#58220 = CARTESIAN_POINT ( 'NONE',  ( 75.42576880091937142, 0.000000000000000000, 282.4830310981789125 ) ) ;
#58221 = FACE_OUTER_BOUND ( 'NONE', #63735, .T. ) ;
#58222 = EDGE_CURVE ( 'NONE', #42575, #37879, #55211, .T. ) ;
#58223 = ORIENTED_EDGE ( 'NONE', *, *, #22219, .F. ) ;
#58224 = CARTESIAN_POINT ( 'NONE',  ( 15.00000000000000000, -0.5000000000000000000, 26.50000000000000000 ) ) ;
#58225 = ADVANCED_FACE ( 'NONE', ( #18395 ), #38606, .F. ) ;
#58226 = AXIS2_PLACEMENT_3D ( 'NONE', #50098, #38469, #54729 ) ;
#58227 = DIRECTION ( 'NONE',  ( 0.000000000000000000, 0.000000000000000000, 1.000000000000000000 ) ) ;
#58228 = DIRECTION ( 'NONE',  ( 0.000000000000000000, 0.000000000000000000, 1.000000000000000000 ) ) ;
#58229 = CARTESIAN_POINT ( 'NONE',  ( 7.450000000000006395, 7.250000000000000888, -23.00000000000000000 ) ) ;
#58230 = ORIENTED_EDGE ( 'NONE', *, *, #43607, .F. ) ;
#58231 = FACE_OUTER_BOUND ( 'NONE', #6829, .T. ) ;
#58232 = DIRECTION ( 'NONE',  ( 0.000000000000000000, 1.000000000000000000, 0.000000000000000000 ) ) ;
#58233 = EDGE_CURVE ( 'NONE', #18504, #47849, #28673, .T. ) ;
#58234 = CIRCLE ( 'NONE', #67261, 0.1749999999999989342 ) ;
#58235 = DIRECTION ( 'NONE',  ( 0.000000000000000000, 1.000000000000000000, 0.000000000000000000 ) ) ;
#58236 = DIRECTION ( 'NONE',  ( 0.000000000000000000, -1.000000000000000000, -6.036837696397607468E-13 ) ) ;
#58237 = AXIS2_PLACEMENT_3D ( 'NONE', #51093, #30580, #46834 ) ;
#58238 = EDGE_CURVE ( 'NONE', #127, #34015, #45272, .T. ) ;
#58239 = DIRECTION ( 'NONE',  ( -1.000000000000000000, 0.000000000000000000, 0.000000000000000000 ) ) ;
#58240 = EDGE_LOOP ( 'NONE', ( #13146, #44437, #24870, #45626 ) ) ;
#58241 = EDGE_CURVE ( 'NONE', #64033, #37901, #61528, .T. ) ;
#58242 = VECTOR ( 'NONE', #39389, 1000.000000000000000 ) ;
#58243 = AXIS2_PLACEMENT_3D ( 'NONE', #33438, #17864, #59955 ) ;
#58244 = VECTOR ( 'NONE', #43232, 1000.000000000000000 ) ;
#58245 = EDGE_LOOP ( 'NONE', ( #57562, #44646, #55160, #67834 ) ) ;
#58246 = FACE_OUTER_BOUND ( 'NONE', #69735, .T. ) ;
#58247 = FACE_OUTER_BOUND ( 'NONE', #55807, .T. ) ;
#58248 = ORIENTED_EDGE ( 'NONE', *, *, #28447, .T. ) ;
#58249 = CARTESIAN_POINT ( 'NONE',  ( 11.00000000000000000, -14.03999999999999915, 14.79999999999999893 ) ) ;
#58250 = AXIS2_PLACEMENT_3D ( 'NONE', #66969, #18530, #57419 ) ;
#58251 = AXIS2_PLACEMENT_3D ( 'NONE', #67809, #51550, #30329 ) ;
#58252 = AXIS2_PLACEMENT_3D ( 'NONE', #58791, #69038, #20595 ) ;
#58253 = CARTESIAN_POINT ( 'NONE',  ( 41.09999999999999432, 21.00000000000000000, 13.98999642601811999 ) ) ;
#58254 = EDGE_LOOP ( 'NONE', ( #66741, #48793, #17480, #7956 ) ) ;
#58255 = AXIS2_PLACEMENT_3D ( 'NONE', #64980, #61030, #43394 ) ;
#58256 = DIRECTION ( 'NONE',  ( 0.000000000000000000, -0.7057491738665938596, 0.7084617869628679898 ) ) ;
#58257 = ORIENTED_EDGE ( 'NONE', *, *, #27975, .T. ) ;
#58258 = ORIENTED_EDGE ( 'NONE', *, *, #59905, .F. ) ;
#58259 = CARTESIAN_POINT ( 'NONE',  ( -3.842976262117327124, -10.31452373788281207, 26.00000000000000000 ) ) ;
#58260 = ORIENTED_EDGE ( 'NONE', *, *, #12303, .T. ) ;
#58261 = CYLINDRICAL_SURFACE ( 'NONE', #41769, 4.500000000000189182 ) ;
#58262 = DIRECTION ( 'NONE',  ( 0.000000000000000000, 0.000000000000000000, 1.000000000000000000 ) ) ;
#58263 = MECHANICAL_DESIGN_GEOMETRIC_PRESENTATION_REPRESENTATION (  '', ( #10809 ), #57141 ) ;
#58264 = LINE ( 'NONE', #45893, #20852 ) ;
#58265 = EDGE_CURVE ( 'NONE', #11613, #44153, #64268, .T. ) ;
#58266 = ORIENTED_EDGE ( 'NONE', *, *, #48405, .F. ) ;
#58267 = CIRCLE ( 'NONE', #47964, 24.99999999998784972 ) ;
#58268 = LINE ( 'NONE', #48004, #65074 ) ;
#58270 = DIRECTION ( 'NONE',  ( 0.000000000000000000, 0.000000000000000000, -1.000000000000000000 ) ) ;
#58269 = DIRECTION ( 'NONE',  ( 1.836970198721029934E-16, 1.836970198721010706E-16, -1.000000000000000000 ) ) ;
#58271 = EDGE_LOOP ( 'NONE', ( #37247, #9459, #63372, #60066 ) ) ;
#58272 = VERTEX_POINT ( 'NONE', #51287 ) ;
#58273 = ORIENTED_EDGE ( 'NONE', *, *, #786, .F. ) ;
#58274 = ADVANCED_FACE ( 'NONE', ( #30778 ), #41020, .F. ) ;
#58276 = ORIENTED_EDGE ( 'NONE', *, *, #49673, .F. ) ;
#58275 = PRODUCT_CONTEXT ( 'NONE', #66133, 'mechanical' ) ;
#58277 = CARTESIAN_POINT ( 'NONE',  ( 30.00000000000000000, -5.200000000000001066, -26.59999999999999787 ) ) ;
#58279 = ORIENTED_EDGE ( 'NONE', *, *, #4726, .T. ) ;
#58278 = CARTESIAN_POINT ( 'NONE',  ( 10.50702373788281996, -6.849523737882823760, 54.00000000000000711 ) ) ;
#58280 = ADVANCED_FACE ( 'NONE', ( #2495 ), #2657, .T. ) ;
#58281 = DIRECTION ( 'NONE',  ( -0.000000000000000000, -0.000000000000000000, -1.000000000000000000 ) ) ;
#58282 = DIRECTION ( 'NONE',  ( 0.000000000000000000, 0.000000000000000000, -1.000000000000000000 ) ) ;
#58283 = ORIENTED_EDGE ( 'NONE', *, *, #20637, .T. ) ;
#58284 = VECTOR ( 'NONE', #15074, 1000.000000000000000 ) ;
#58285 = ORIENTED_EDGE ( 'NONE', *, *, #44320, .T. ) ;
#58286 = EDGE_CURVE ( 'NONE', #16314, #20965, #32084, .T. ) ;
#58287 = LINE ( 'NONE', #47668, #47091 ) ;
#58288 = AXIS2_PLACEMENT_3D ( 'NONE', #21805, #58944, #44056 ) ;
#58289 = ORIENTED_EDGE ( 'NONE', *, *, #42180, .F. ) ;
#58290 = DIRECTION ( 'NONE',  ( 0.000000000000000000, 1.000000000000000000, 0.000000000000000000 ) ) ;
#58291 = CARTESIAN_POINT ( 'NONE',  ( -11.00000000000000000, -13.54524521594299991, -17.53999999999999915 ) ) ;
#58292 = AXIS2_PLACEMENT_3D ( 'NONE', #17438, #1197, #54600 ) ;
#58293 = ADVANCED_FACE ( 'NONE', ( #62240 ), #40680, .T. ) ;
#58294 = DIRECTION ( 'NONE',  ( -1.000000000000000000, 0.000000000000000000, -0.000000000000000000 ) ) ;
#58295 = ORIENTED_EDGE ( 'NONE', *, *, #53160, .T. ) ;
#58296 = AXIS2_PLACEMENT_3D ( 'NONE', #61214, #12775, #7131 ) ;
#58297 = AXIS2_PLACEMENT_3D ( 'NONE', #36129, #20571, #42135 ) ;
#58298 = CIRCLE ( 'NONE', #69608, 1.000000000000000000 ) ;
#58299 = DIRECTION ( 'NONE',  ( -1.000000000000000000, 0.000000000000000000, 0.000000000000000000 ) ) ;
#58300 = DIRECTION ( 'NONE',  ( 1.000000000000000000, -0.000000000000000000, -0.000000000000000000 ) ) ;
#58301 = EDGE_CURVE ( 'NONE', #16822, #43665, #52349, .T. ) ;
#58303 = ORIENTED_EDGE ( 'NONE', *, *, #50949, .T. ) ;
#58302 = FILL_AREA_STYLE_COLOUR ( '', #18407 ) ;
#58305 = EDGE_LOOP ( 'NONE', ( #48689, #23444, #27741, #55031 ) ) ;
#58304 = FACE_OUTER_BOUND ( 'NONE', #42320, .T. ) ;
#58306 = ADVANCED_FACE ( 'NONE', ( #30070 ), #18762, .T. ) ;
#58307 = LINE ( 'NONE', #9511, #21623 ) ;
#58308 = CIRCLE ( 'NONE', #66216, 24.99999999998789946 ) ;
#58309 = AXIS2_PLACEMENT_3D ( 'NONE', #58451, #15658, #59132 ) ;
#58310 = AXIS2_PLACEMENT_3D ( 'NONE', #15585, #68257, #58707 ) ;
#58311 = CARTESIAN_POINT ( 'NONE',  ( -5.242976262117280406, -5.257023737882805747, 54.00000000000000711 ) ) ;
#58312 = ADVANCED_FACE ( 'NONE', ( #19799 ), #41378, .F. ) ;
#58313 = LINE ( 'NONE', #52299, #38085 ) ;
#58314 = EDGE_CURVE ( 'NONE', #15685, #13374, #15819, .T. ) ;
#58315 = EDGE_CURVE ( 'NONE', #59376, #23171, #52000, .T. ) ;
#58316 = DIRECTION ( 'NONE',  ( -0.000000000000000000, 0.000000000000000000, 1.000000000000000000 ) ) ;
#58317 = VECTOR ( 'NONE', #11822, 1000.000000000000114 ) ;
#58318 = CARTESIAN_POINT ( 'NONE',  ( 8.580623737882818958, -9.703773737882814387, 26.00000000000000000 ) ) ;
#58319 = VERTEX_POINT ( 'NONE', #8138 ) ;
#58320 = CARTESIAN_POINT ( 'NONE',  ( 14.50000000000000000, 1.110223024625156540E-16, -26.50000000000000000 ) ) ;
#58321 = LINE ( 'NONE', #5274, #20335 ) ;
#58322 = EDGE_CURVE ( 'NONE', #63857, #61547, #34239, .T. ) ;
#58324 = ORIENTED_EDGE ( 'NONE', *, *, #22793, .T. ) ;
#58323 = CARTESIAN_POINT ( 'NONE',  ( -2.993516549646701108, 7.415254214038204061, 455.0000000000000568 ) ) ;
#58325 = CIRCLE ( 'NONE', #34561, 2.204799999999999205 ) ;
#58326 = LINE ( 'NONE', #62208, #51612 ) ;
#58327 = EDGE_CURVE ( 'NONE', #32793, #16596, #62453, .T. ) ;
#58328 = DIRECTION ( 'NONE',  ( -1.000000000000000000, 0.000000000000000000, 0.000000000000000000 ) ) ;
#58329 = PLANE ( 'NONE',  #6999 ) ;
#58330 = EDGE_CURVE ( 'NONE', #17298, #67142, #67908, .T. ) ;
#58331 = DIRECTION ( 'NONE',  ( 1.000000000000000000, -0.000000000000000000, -0.000000000000000000 ) ) ;
#58332 = ORIENTED_EDGE ( 'NONE', *, *, #66840, .T. ) ;
#58333 = DIRECTION ( 'NONE',  ( 0.000000000000000000, 0.000000000000000000, 1.000000000000000000 ) ) ;
#58334 = CARTESIAN_POINT ( 'NONE',  ( 0.2500000000000000000, -42.25000000000000000, -26.75000000000000000 ) ) ;
#58335 = ORIENTED_EDGE ( 'NONE', *, *, #14141, .T. ) ;
#58336 =( NAMED_UNIT ( * ) SI_UNIT ( $, .STERADIAN. ) SOLID_ANGLE_UNIT ( ) );
#58337 = FACE_OUTER_BOUND ( 'NONE', #58987, .T. ) ;
#58338 = LINE ( 'NONE', #69281, #8342 ) ;
#58339 = EDGE_CURVE ( 'NONE', #40605, #62248, #42192, .T. ) ;
#58340 = CARTESIAN_POINT ( 'NONE',  ( -30.00000000000000000, -5.000000000000000000, -27.00000000000000000 ) ) ;
#58341 = EDGE_CURVE ( 'NONE', #8948, #15366, #36073, .T. ) ;
#58342 = DIRECTION ( 'NONE',  ( 0.000000000000000000, 0.000000000000000000, -1.000000000000000000 ) ) ;
#58343 = VERTEX_POINT ( 'NONE', #9215 ) ;
#58344 = ORIENTED_EDGE ( 'NONE', *, *, #6355, .F. ) ;
#58345 = DIRECTION ( 'NONE',  ( 1.000000000000000000, 0.000000000000000000, 0.000000000000000000 ) ) ;
#58346 = VERTEX_POINT ( 'NONE', #4867 ) ;
#58347 = AXIS2_PLACEMENT_3D ( 'NONE', #10049, #53536, #5090 ) ;
#58348 = EDGE_LOOP ( 'NONE', ( #45834, #47500, #20101, #32594 ) ) ;
#58349 = FACE_OUTER_BOUND ( 'NONE', #11630, .T. ) ;
#58350 = AXIS2_PLACEMENT_3D ( 'NONE', #18142, #29450, #24153 ) ;
#58351 = ADVANCED_FACE ( 'NONE', ( #26430 ), #47997, .T. ) ;
#58352 = CARTESIAN_POINT ( 'NONE',  ( 7.500000000000000000, -25.50000000000000355, -20.00000000000000000 ) ) ;
#58353 = VECTOR ( 'NONE', #49508, 1000.000000000000000 ) ;
#58354 = CARTESIAN_POINT ( 'NONE',  ( 39.00000000000000000, 21.00000000000000000, -16.96999999999999886 ) ) ;
#58355 = ORIENTED_EDGE ( 'NONE', *, *, #9189, .F. ) ;
#58356 = ORIENTED_EDGE ( 'NONE', *, *, #27174, .T. ) ;
#58357 = CYLINDRICAL_SURFACE ( 'NONE', #31864, 4.000000000000000000 ) ;
#58358 = ORIENTED_EDGE ( 'NONE', *, *, #32749, .F. ) ;
#58359 = ORIENTED_EDGE ( 'NONE', *, *, #13200, .T. ) ;
#58360 = VECTOR ( 'NONE', #49376, 1000.000000000000000 ) ;
#58361 = AXIS2_PLACEMENT_3D ( 'NONE', #62465, #50817, #2387 ) ;
#58362 = VECTOR ( 'NONE', #53772, 1000.000000000000000 ) ;
#58363 = CARTESIAN_POINT ( 'NONE',  ( -4.383466043307968185, -8.406483450353443132, 455.0000000000000568 ) ) ;
#58364 = DIRECTION ( 'NONE',  ( 0.5000000000000019984, 0.8660254037844375974, 3.181725716174716554E-16 ) ) ;
#58365 = CYLINDRICAL_SURFACE ( 'NONE', #2711, 3.999999999999993339 ) ;
#58366 = ORIENTED_EDGE ( 'NONE', *, *, #24130, .T. ) ;
#58367 = CARTESIAN_POINT ( 'NONE',  ( 7.250000000000005329, -7.249999999999998224, -16.00000000000000000 ) ) ;
#58368 = AXIS2_PLACEMENT_3D ( 'NONE', #24100, #45662, #8531 ) ;
#58369 = VECTOR ( 'NONE', #263, 1000.000000000000000 ) ;
#58371 = CARTESIAN_POINT ( 'NONE',  ( 7.000000000000000000, -25.50000000000000355, -14.74860679774999994 ) ) ;
#58370 = LINE ( 'NONE', #41025, #8425 ) ;
#58372 = EDGE_LOOP ( 'NONE', ( #6984, #36499, #58940, #2076, #59638, #1383, #29669, #6261, #27259 ) ) ;
#58374 = VERTEX_POINT ( 'NONE', #48348 ) ;
#58373 = DIRECTION ( 'NONE',  ( -1.000000000000000000, 0.000000000000000000, 0.000000000000000000 ) ) ;
#58375 = ORIENTED_EDGE ( 'NONE', *, *, #32837, .F. ) ;
#58376 = DIRECTION ( 'NONE',  ( 1.000000000000000000, -0.000000000000000000, 0.000000000000000000 ) ) ;
#58377 = ADVANCED_FACE ( 'NONE', ( #603 ), #48693, .T. ) ;
#58378 = VECTOR ( 'NONE', #35051, 1000.000000000000000 ) ;
#58379 = CYLINDRICAL_SURFACE ( 'NONE', #8993, 0.7499999999999997780 ) ;
#58380 = VERTEX_POINT ( 'NONE', #26788 ) ;
#58381 = ADVANCED_FACE ( 'NONE', ( #22174 ), #65313, .T. ) ;
#58382 = PLANE ( 'NONE',  #65915 ) ;
#58383 = EDGE_CURVE ( 'NONE', #30690, #35743, #53657, .T. ) ;
#58384 = CARTESIAN_POINT ( 'NONE',  ( 30.00000000000000000, -9.199999999999999289, -12.69999999999986073 ) ) ;
#58385 = ORIENTED_EDGE ( 'NONE', *, *, #54240, .T. ) ;
#58386 = ORIENTED_EDGE ( 'NONE', *, *, #20539, .F. ) ;
#58387 = CARTESIAN_POINT ( 'NONE',  ( -22.14589803375000088, -15.50000000000000000, 21.50000000000000000 ) ) ;
#58388 = EDGE_CURVE ( 'NONE', #51018, #22980, #16864, .T. ) ;
#58389 = LINE ( 'NONE', #729, #11332 ) ;
#58390 = ORIENTED_EDGE ( 'NONE', *, *, #20613, .F. ) ;
#58391 = CARTESIAN_POINT ( 'NONE',  ( 7.250000000000005329, -8.249999999999998224, -26.00000000000001066 ) ) ;
#58392 = CARTESIAN_POINT ( 'NONE',  ( -9.722976262117258628, 6.817976262117182884, 54.00000000000000711 ) ) ;
#58393 = VECTOR ( 'NONE', #28986, 1000.000000000000000 ) ;
#58395 = EDGE_LOOP ( 'NONE', ( #43312, #30150, #9758, #718, #29758, #508, #11024, #68365 ) ) ;
#58394 = DIRECTION ( 'NONE',  ( -1.000000000000000000, 0.000000000000000000, 0.000000000000000000 ) ) ;
#58397 = ORIENTED_EDGE ( 'NONE', *, *, #36727, .F. ) ;
#58396 = DIRECTION ( 'NONE',  ( 1.836970198721029934E-16, 1.836970198721010706E-16, -1.000000000000000000 ) ) ;
#58398 = CARTESIAN_POINT ( 'NONE',  ( 11.32648345035337734, -7.806483450353490561, 455.0000000000000568 ) ) ;
#58399 = AXIS2_PLACEMENT_3D ( 'NONE', #6958, #17225, #22885 ) ;
#58400 = CARTESIAN_POINT ( 'NONE',  ( 11.48848345035334617, -11.08848345035349148, 455.0000000000000568 ) ) ;
#58401 = DIRECTION ( 'NONE',  ( -0.6414496315691619044, -0.7671651518152962090, 0.000000000000000000 ) ) ;
#58402 = LINE ( 'NONE', #31531, #43709 ) ;
#58403 = EDGE_CURVE ( 'NONE', #2479, #30178, #22854, .T. ) ;
#58404 = LINE ( 'NONE', #4318, #45208 ) ;
#58405 = VECTOR ( 'NONE', #32489, 1000.000000000000000 ) ;
#58406 = VECTOR ( 'NONE', #18002, 1000.000000000000000 ) ;
#58407 = CARTESIAN_POINT ( 'NONE',  ( -7.250000000000000888, 7.450000000000003730, -13.50000000000000178 ) ) ;
#58408 = EDGE_LOOP ( 'NONE', ( #30333, #41522, #9147, #39784 ) ) ;
#58409 = FACE_OUTER_BOUND ( 'NONE', #12607, .T. ) ;
#58411 = VERTEX_POINT ( 'NONE', #59298 ) ;
#58410 = CARTESIAN_POINT ( 'NONE',  ( 23.50000000000000000, -5.200000000000001066, -22.50000000000000000 ) ) ;
#58412 = CIRCLE ( 'NONE', #1951, 0.3999999999993835154 ) ;
#58414 = CARTESIAN_POINT ( 'NONE',  ( 14.50000000000000000, -42.50000000000000000, -26.50000000000000000 ) ) ;
#58413 = VECTOR ( 'NONE', #25687, 1000.000000000000000 ) ;
#58415 = FACE_OUTER_BOUND ( 'NONE', #24169, .T. ) ;
#58416 = AXIS2_PLACEMENT_3D ( 'NONE', #20957, #64119, #42171 ) ;
#58417 = DIRECTION ( 'NONE',  ( 0.000000000000000000, 0.000000000000000000, 1.000000000000000000 ) ) ;
#58418 = CARTESIAN_POINT ( 'NONE',  ( -6.822336235477446387, 4.135079735113102117, 26.00000000000000711 ) ) ;
#58419 = AXIS2_PLACEMENT_3D ( 'NONE', #14306, #13942, #50718 ) ;
#58420 = VECTOR ( 'NONE', #52258, 1000.000000000000000 ) ;
#58421 = EDGE_LOOP ( 'NONE', ( #12849, #56698, #63898, #66664 ) ) ;
#58422 = DIRECTION ( 'NONE',  ( 1.000000000000000000, -8.612436249475772606E-15, -1.836970198721045711E-16 ) ) ;
#58423 = LINE ( 'NONE', #37539, #12487 ) ;
#58424 = ORIENTED_EDGE ( 'NONE', *, *, #47027, .F. ) ;
#58425 = FACE_OUTER_BOUND ( 'NONE', #18508, .T. ) ;
#58426 = CARTESIAN_POINT ( 'NONE',  ( -9.547976262117304103, -8.144523737882758851, 54.00000000000000711 ) ) ;
#58427 = EDGE_CURVE ( 'NONE', #26334, #65847, #64957, .T. ) ;
#58428 = ADVANCED_FACE ( 'NONE', ( #5225 ), #11536, .F. ) ;
#58429 = VECTOR ( 'NONE', #14820, 1000.000000000000000 ) ;
#58430 = FACE_OUTER_BOUND ( 'NONE', #60835, .T. ) ;
#58431 = ORIENTED_EDGE ( 'NONE', *, *, #6491, .T. ) ;
#58432 = CARTESIAN_POINT ( 'NONE',  ( -11.31351654964674402, -4.406483450353330333, 455.0000000000000568 ) ) ;
#58433 = ORIENTED_EDGE ( 'NONE', *, *, #27442, .F. ) ;
#58434 = ORIENTED_EDGE ( 'NONE', *, *, #19731, .T. ) ;
#58435 = LINE ( 'NONE', #58066, #38164 ) ;
#58436 = CARTESIAN_POINT ( 'NONE',  ( 7.500000000000000000, -25.60000000000000142, 20.00000000000000000 ) ) ;
#58437 = DIRECTION ( 'NONE',  ( -0.6414496315691565753, -0.7671651518153006499, 0.000000000000000000 ) ) ;
#58438 = LINE ( 'NONE', #42149, #29869 ) ;
#58439 = LINE ( 'NONE', #31563, #44192 ) ;
#58440 = ORIENTED_EDGE ( 'NONE', *, *, #13410, .T. ) ;
#58441 = ORIENTED_EDGE ( 'NONE', *, *, #56565, .T. ) ;
#58443 = ORIENTED_EDGE ( 'NONE', *, *, #1534, .F. ) ;
#58442 = DIRECTION ( 'NONE',  ( 1.000000000000000000, 0.000000000000000000, 0.000000000000000000 ) ) ;
#58444 = ORIENTED_EDGE ( 'NONE', *, *, #48773, .F. ) ;
#58445 = CYLINDRICAL_SURFACE ( 'NONE', #8908, 24.99999999998789946 ) ;
#58446 = CARTESIAN_POINT ( 'NONE',  ( 3.664523737882781518, -10.31452373788281029, 54.00000000000000711 ) ) ;
#58447 = LINE ( 'NONE', #47813, #66958 ) ;
#58448 = VECTOR ( 'NONE', #51787, 1000.000000000000000 ) ;
#58449 = PLANE ( 'NONE',  #58252 ) ;
#58451 = CARTESIAN_POINT ( 'NONE',  ( -7.603567055985634759, -8.406483450353409381, 455.0000000000000568 ) ) ;
#58450 = FACE_OUTER_BOUND ( 'NONE', #21295, .T. ) ;
#58452 = VERTEX_POINT ( 'NONE', #16168 ) ;
#58453 = ORIENTED_EDGE ( 'NONE', *, *, #51832, .T. ) ;
#58454 = ORIENTED_EDGE ( 'NONE', *, *, #40940, .F. ) ;
#58455 = AXIS2_PLACEMENT_3D ( 'NONE', #5250, #53688, #42368 ) ;
#58456 = AXIS2_PLACEMENT_3D ( 'NONE', #64574, #43701, #11500 ) ;
#58457 = AXIS2_PLACEMENT_3D ( 'NONE', #7657, #40179, #2360 ) ;
#58458 = DIRECTION ( 'NONE',  ( -0.000000000000000000, 1.000000000000000000, -0.000000000000000000 ) ) ;
#58459 = FACE_OUTER_BOUND ( 'NONE', #57984, .T. ) ;
#58460 = VECTOR ( 'NONE', #22671, 1000.000000000000000 ) ;
#58461 = ADVANCED_FACE ( 'NONE', ( #54012 ), #44402, .F. ) ;
#58462 = VECTOR ( 'NONE', #37255, 1000.000000000000000 ) ;
#58463 = LINE ( 'NONE', #103, #51167 ) ;
#58464 = ORIENTED_EDGE ( 'NONE', *, *, #50523, .T. ) ;
#58465 = ORIENTED_EDGE ( 'NONE', *, *, #36602, .F. ) ;
#58466 = VERTEX_POINT ( 'NONE', #32773 ) ;
#58467 = ORIENTED_EDGE ( 'NONE', *, *, #9736, .F. ) ;
#58468 = EDGE_CURVE ( 'NONE', #53491, #40746, #26399, .T. ) ;
#58469 = CARTESIAN_POINT ( 'NONE',  ( -5.242976262117259978, 5.242976262117182706, 54.00000000000000711 ) ) ;
#58470 = AXIS2_PLACEMENT_3D ( 'NONE', #54929, #6483, #28043 ) ;
#58471 = AXIS2_PLACEMENT_3D ( 'NONE', #17201, #33119, #55056 ) ;
#58472 = ORIENTED_EDGE ( 'NONE', *, *, #21580, .F. ) ;
#58473 = EDGE_CURVE ( 'NONE', #54695, #21488, #17540, .T. ) ;
#58474 = CARTESIAN_POINT ( 'NONE',  ( 6.849523737882818430, 10.49297626211719603, 54.00000000000000711 ) ) ;
#58475 = ADVANCED_FACE ( 'NONE', ( #55054 ), #38097, .T. ) ;
#58476 = ORIENTED_EDGE ( 'NONE', *, *, #11433, .T. ) ;
#58477 = ORIENTED_EDGE ( 'NONE', *, *, #7984, .T. ) ;
#58478 = DIRECTION ( 'NONE',  ( 0.000000000000000000, 0.000000000000000000, 1.000000000000000000 ) ) ;
#58479 = ADVANCED_FACE ( 'NONE', ( #64608 ), #11201, .F. ) ;
#58480 = EDGE_CURVE ( 'NONE', #9620, #25742, #43737, .T. ) ;
#58482 = ORIENTED_EDGE ( 'NONE', *, *, #34729, .F. ) ;
#58481 = CARTESIAN_POINT ( 'NONE',  ( 9.912023737882801555, 6.642976262117184838, 54.00000000000000711 ) ) ;
#58483 = ORIENTED_EDGE ( 'NONE', *, *, #65638, .T. ) ;
#58484 = VECTOR ( 'NONE', #20036, 1000.000000000000000 ) ;
#58485 = DIRECTION ( 'NONE',  ( 1.000000000000000000, 0.000000000000000000, 0.000000000000000000 ) ) ;
#58486 = EDGE_CURVE ( 'NONE', #37433, #27463, #49725, .T. ) ;
#58487 = LINE ( 'NONE', #10032, #48301 ) ;
#58489 = VERTEX_POINT ( 'NONE', #65646 ) ;
#58488 = DIRECTION ( 'NONE',  ( -0.6414496315691565753, -0.7671651518153006499, 0.000000000000000000 ) ) ;
#58490 = ORIENTED_EDGE ( 'NONE', *, *, #66662, .F. ) ;
#58491 = CARTESIAN_POINT ( 'NONE',  ( 17.00000000000000000, -16.28999999999999915, 14.50000000000000000 ) ) ;
#58492 = FACE_OUTER_BOUND ( 'NONE', #39968, .T. ) ;
#58493 = DIRECTION ( 'NONE',  ( 0.000000000000000000, -0.000000000000000000, 1.000000000000000000 ) ) ;
#58494 = DIRECTION ( 'NONE',  ( -1.000000000000000000, 0.000000000000000000, 0.000000000000000000 ) ) ;
#58495 = DIRECTION ( 'NONE',  ( 0.000000000000000000, 0.000000000000000000, -1.000000000000000000 ) ) ;
#58496 = ORIENTED_EDGE ( 'NONE', *, *, #32201, .T. ) ;
#58497 = DIRECTION ( 'NONE',  ( 1.000000000000000000, -1.088659024508174415E-14, 1.836970198721009966E-16 ) ) ;
#58498 = ORIENTED_EDGE ( 'NONE', *, *, #17927, .T. ) ;
#58499 = DIRECTION ( 'NONE',  ( 0.000000000000000000, 1.000000000000000000, 0.000000000000000000 ) ) ;
#58500 = CARTESIAN_POINT ( 'NONE',  ( 290.0000000000000000, -21.00000000000000000, 0.000000000000000000 ) ) ;
#58501 = AXIS2_PLACEMENT_3D ( 'NONE', #24488, #40391, #39681 ) ;
#58502 = DIRECTION ( 'NONE',  ( 0.000000000000000000, -0.7071067811865474617, -0.7071067811865474617 ) ) ;
#58503 = DIRECTION ( 'NONE',  ( 0.000000000000000000, 1.000000000000000000, 0.000000000000000000 ) ) ;
#58504 = DIRECTION ( 'NONE',  ( 0.000000000000000000, 1.000000000000000000, 0.000000000000000000 ) ) ;
#58505 = ORIENTED_EDGE ( 'NONE', *, *, #48970, .T. ) ;
#58506 = CARTESIAN_POINT ( 'NONE',  ( -9.942044687070568543, 2.752095193409294982, 195.0000000000000284 ) ) ;
#58507 = CARTESIAN_POINT ( 'NONE',  ( -7.250000000000000888, 7.250000000000001776, -13.50000000000000178 ) ) ;
#58508 = CIRCLE ( 'NONE', #42688, 0.5000000000009320322 ) ;
#58509 = EDGE_CURVE ( 'NONE', #9679, #22670, #55710, .T. ) ;
#58510 = CARTESIAN_POINT ( 'NONE',  ( 13.00000000000000178, -16.28999999999999915, 14.50000000000000000 ) ) ;
#58511 = VERTEX_POINT ( 'NONE', #60324 ) ;
#58512 = CARTESIAN_POINT ( 'NONE',  ( 2.632023737882806191, 6.486996718459881350, 54.00000000000000711 ) ) ;
#58513 = DIRECTION ( 'NONE',  ( -1.836970198721029934E-16, 1.836970198721036590E-16, -1.000000000000000000 ) ) ;
#58514 = CARTESIAN_POINT ( 'NONE',  ( 9.912023737882778462, 3.842976262117153485, 26.00000000000000711 ) ) ;
#58515 = EDGE_CURVE ( 'NONE', #28003, #14054, #28836, .T. ) ;
#58516 = EDGE_CURVE ( 'NONE', #61299, #55382, #53467, .T. ) ;
#58517 = VECTOR ( 'NONE', #45219, 1000.000000000000000 ) ;
#58518 = DIRECTION ( 'NONE',  ( -4.121462285523434951E-16, -1.000000000000000000, -0.000000000000000000 ) ) ;
#58519 = CARTESIAN_POINT ( 'NONE',  ( 9.106483450353380249, -10.09643294401465852, 455.0000000000000568 ) ) ;
#58520 = ORIENTED_EDGE ( 'NONE', *, *, #16331, .F. ) ;
#58521 = DIRECTION ( 'NONE',  ( 0.000000000000000000, -0.000000000000000000, -1.000000000000000000 ) ) ;
#58522 = PLANE ( 'NONE',  #21540 ) ;
#58523 = CARTESIAN_POINT ( 'NONE',  ( 0.000000000000000000, 0.7500000000000000000, 0.000000000000000000 ) ) ;
#58524 = EDGE_CURVE ( 'NONE', #11076, #59106, #7270, .T. ) ;
#58525 = CARTESIAN_POINT ( 'NONE',  ( 8.406483450353379183, -7.616533956692325802, 455.0000000000000568 ) ) ;
#58526 =( REPRESENTATION_RELATIONSHIP ('NONE','NONE', #4299, #25847 ) REPRESENTATION_RELATIONSHIP_WITH_TRANSFORMATION ( #6940 )SHAPE_REPRESENTATION_RELATIONSHIP( ) );
#58527 = DIRECTION ( 'NONE',  ( -1.000000000000000000, 0.000000000000000000, 0.000000000000000000 ) ) ;
#58528 = ORIENTED_EDGE ( 'NONE', *, *, #30838, .F. ) ;
#58530 = VERTEX_POINT ( 'NONE', #39454 ) ;
#58529 = DIRECTION ( 'NONE',  ( -1.000000000000000000, 0.000000000000000000, 0.000000000000000000 ) ) ;
#58531 = DIRECTION ( 'NONE',  ( 0.000000000000000000, -1.000000000000000000, 0.000000000000000000 ) ) ;
#58532 = DIRECTION ( 'NONE',  ( 0.000000000000000000, 1.000000000000000000, 1.922073611378672844E-12 ) ) ;
#58533 = FACE_BOUND ( 'NONE', #59975, .T. ) ;
#58534 = ORIENTED_EDGE ( 'NONE', *, *, #61148, .F. ) ;
#58535 = CARTESIAN_POINT ( 'NONE',  ( -9.234937905884020637, 9.942044687070460185, 455.0000000000000568 ) ) ;
#58536 = CARTESIAN_POINT ( 'NONE',  ( 40.90000000000000568, -0.2000000000000000111, 0.000000000000000000 ) ) ;
#58537 = ORIENTED_EDGE ( 'NONE', *, *, #37142, .F. ) ;
#58538 = EDGE_LOOP ( 'NONE', ( #51960, #53116, #33035, #27903, #69836, #58083, #69874 ) ) ;
#58539 = ORIENTED_EDGE ( 'NONE', *, *, #59813, .F. ) ;
#58540 = LINE ( 'NONE', #42609, #60251 ) ;
#58541 = DIRECTION ( 'NONE',  ( 0.000000000000000000, 0.000000000000000000, 1.000000000000000000 ) ) ;
#58542 = CYLINDRICAL_SURFACE ( 'NONE', #52868, 9.300000000000002487 ) ;
#58543 = EDGE_CURVE ( 'NONE', #65577, #48640, #24605, .T. ) ;
#58544 = AXIS2_PLACEMENT_3D ( 'NONE', #55531, #12716, #8465 ) ;
#58545 = ORIENTED_EDGE ( 'NONE', *, *, #63654, .T. ) ;
#58546 = ORIENTED_EDGE ( 'NONE', *, *, #69730, .T. ) ;
#58547 = DIRECTION ( 'NONE',  ( -1.000000000000000000, 0.000000000000000000, 0.000000000000000000 ) ) ;
#58548 = ORIENTED_EDGE ( 'NONE', *, *, #46632, .F. ) ;
#58549 = VERTEX_POINT ( 'NONE', #18581 ) ;
#58550 = ORIENTED_EDGE ( 'NONE', *, *, #1740, .F. ) ;
#58551 = ORIENTED_EDGE ( 'NONE', *, *, #27751, .T. ) ;
#58552 = DIRECTION ( 'NONE',  ( 0.000000000000000000, 0.000000000000000000, -1.000000000000000000 ) ) ;
#58553 = UNCERTAINTY_MEASURE_WITH_UNIT (LENGTH_MEASURE( 1.000000000000000082E-05 ), #39233, 'distance_accuracy_value', 'NONE');
#58554 = EDGE_CURVE ( 'NONE', #67915, #17187, #29544, .T. ) ;
#58556 = ORIENTED_EDGE ( 'NONE', *, *, #33728, .F. ) ;
#58555 = DIRECTION ( 'NONE',  ( 1.000000000000000000, 0.000000000000000000, 0.000000000000000000 ) ) ;
#58557 = CIRCLE ( 'NONE', #19006, 0.8100000000000017186 ) ;
#58558 = DIRECTION ( 'NONE',  ( 1.000000000000000000, 0.000000000000000000, 0.000000000000000000 ) ) ;
#58559 = DIRECTION ( 'NONE',  ( -1.000000000000000000, 0.000000000000000000, 0.000000000000000000 ) ) ;
#58560 = ADVANCED_FACE ( 'NONE', ( #50758 ), #17892, .F. ) ;
#58561 = DIRECTION ( 'NONE',  ( -0.000000000000000000, -0.000000000000000000, 1.000000000000000000 ) ) ;
#58562 = VERTEX_POINT ( 'NONE', #50425 ) ;
#58563 = ORIENTED_EDGE ( 'NONE', *, *, #7658, .F. ) ;
#58564 = AXIS2_PLACEMENT_3D ( 'NONE', #29147, #2281, #66975 ) ;
#58565 = CARTESIAN_POINT ( 'NONE',  ( 8.750000000000003553, 7.750000000000000000, -5.000000000000000000 ) ) ;
#58566 = CARTESIAN_POINT ( 'NONE',  ( 1.634292677759859869, -8.241237374594282628, 54.00000000000000711 ) ) ;
#58567 = EDGE_LOOP ( 'NONE', ( #15427, #7541, #58677, #56163 ) ) ;
#58568 = AXIS2_PLACEMENT_3D ( 'NONE', #50990, #45325, #66894 ) ;
#58569 = EDGE_CURVE ( 'NONE', #17943, #69312, #51113, .T. ) ;
#58570 = CARTESIAN_POINT ( 'NONE',  ( 23.90000000000000213, -0.1999999999911795112, 8.826273045769999343E-12 ) ) ;
#58571 = DIRECTION ( 'NONE',  ( 1.000000000000000000, -0.000000000000000000, 0.000000000000000000 ) ) ;
#58572 = CARTESIAN_POINT ( 'NONE',  ( 49.00000000000000000, -0.1999999999911430404, -8.864436962241481021E-12 ) ) ;
#58573 = ORIENTED_EDGE ( 'NONE', *, *, #68480, .T. ) ;
#58574 = DIRECTION ( 'NONE',  ( 0.000000000000000000, 0.000000000000000000, -1.000000000000000000 ) ) ;
#58575 = DIRECTION ( 'NONE',  ( 0.000000000000000000, 0.000000000000000000, 1.000000000000000000 ) ) ;
#58576 = PLANE ( 'NONE',  #21785 ) ;
#58577 = CARTESIAN_POINT ( 'NONE',  ( 105.8309041053263257, 3.657408540445008960, 2.000000000000000000 ) ) ;
#58578 = DIRECTION ( 'NONE',  ( 0.000000000000000000, 0.000000000000000000, 1.000000000000000000 ) ) ;
#58579 = VERTEX_POINT ( 'NONE', #61722 ) ;
#58580 = DIRECTION ( 'NONE',  ( -3.491481338843133355E-15, -1.000000000000000000, -1.836970198721029934E-16 ) ) ;
#58581 = DIRECTION ( 'NONE',  ( -0.000000000000000000, 1.000000000000000000, -0.000000000000000000 ) ) ;
#58582 = DIRECTION ( 'NONE',  ( 0.7071067811865436870, -0.7071067811865514585, -2.597868168706495388E-16 ) ) ;
#58583 = VERTEX_POINT ( 'NONE', #55728 ) ;
#58584 = DIRECTION ( 'NONE',  ( 9.912705577010336396E-15, 1.000000000000000000, 0.000000000000000000 ) ) ;
#58585 = DIRECTION ( 'NONE',  ( 1.819560449471430698E-15, 1.000000000000000000, 1.836970198721032892E-16 ) ) ;
#58586 = EDGE_CURVE ( 'NONE', #37838, #27624, #2330, .T. ) ;
#58587 = LINE ( 'NONE', #10140, #33495 ) ;
#58588 = DIRECTION ( 'NONE',  ( 0.000000000000000000, 0.7096009616570518874, 0.7046037717862339012 ) ) ;
#58589 = ORIENTED_EDGE ( 'NONE', *, *, #35862, .T. ) ;
#58590 = LINE ( 'NONE', #15459, #50203 ) ;
#58591 = CARTESIAN_POINT ( 'NONE',  ( -11.00000000000000000, -14.33999999999999986, -14.50000000000000000 ) ) ;
#58592 = CYLINDRICAL_SURFACE ( 'NONE', #8552, 0.5999999999999989786 ) ;
#58593 = EDGE_CURVE ( 'NONE', #57888, #68679, #23895, .T. ) ;
#58594 = AXIS2_PLACEMENT_3D ( 'NONE', #43300, #64882, #21043 ) ;
#58595 = CARTESIAN_POINT ( 'NONE',  ( -1.077516549646832189, -11.34648345035347994, 455.0000000000000568 ) ) ;
#58596 = DIRECTION ( 'NONE',  ( 1.000000000000000000, -0.000000000000000000, -0.000000000000000000 ) ) ;
#58597 = CARTESIAN_POINT ( 'NONE',  ( 25.50000000000000355, -15.50000000000000000, -25.99999999999985434 ) ) ;
#58598 = ORIENTED_EDGE ( 'NONE', *, *, #8572, .T. ) ;
#58599 = VECTOR ( 'NONE', #41808, 1000.000000000000000 ) ;
#58600 = ORIENTED_EDGE ( 'NONE', *, *, #4113, .T. ) ;
#58601 = CARTESIAN_POINT ( 'NONE',  ( 17.00000000000000000, -17.35230188589299871, -15.35019951917099945 ) ) ;
#58602 = DIRECTION ( 'NONE',  ( 1.000000000000000000, 6.938893903907222067E-15, 0.000000000000000000 ) ) ;
#58603 = EDGE_LOOP ( 'NONE', ( #39220, #13704, #29199, #31139, #39194, #47716, #69690, #47061, #14424, #58285, #17687, #6913, #60931, #1794, #18389, #34982 ) ) ;
#58604 = DIRECTION ( 'NONE',  ( 1.836970198721029934E-16, 1.836970198721010706E-16, -1.000000000000000000 ) ) ;
#58605 = VECTOR ( 'NONE', #35856, 1000.000000000000000 ) ;
#58606 = FACE_OUTER_BOUND ( 'NONE', #29191, .T. ) ;
#58607 = ORIENTED_EDGE ( 'NONE', *, *, #22420, .F. ) ;
#58608 = AXIS2_PLACEMENT_3D ( 'NONE', #30761, #41001, #24751 ) ;
#58609 = EDGE_CURVE ( 'NONE', #13118, #22414, #64758, .T. ) ;
#58610 = DIRECTION ( 'NONE',  ( -1.836970198721029934E-16, 1.836970198721036344E-16, -1.000000000000000000 ) ) ;
#58611 = ORIENTED_EDGE ( 'NONE', *, *, #59248, .T. ) ;
#58612 = EDGE_LOOP ( 'NONE', ( #43671, #50991, #51122, #17002 ) ) ;
#58613 = CARTESIAN_POINT ( 'NONE',  ( 283.0000000000000568, -37.14999999999894698, 8.200000000002349410 ) ) ;
#58614 = VERTEX_POINT ( 'NONE', #2673 ) ;
#58615 = DIRECTION ( 'NONE',  ( 0.000000000000000000, 0.000000000000000000, -1.000000000000000000 ) ) ;
#58616 = CARTESIAN_POINT ( 'NONE',  ( 7.250000000000005329, -7.249999999999998224, -11.50000000000000000 ) ) ;
#58617 = DIRECTION ( 'NONE',  ( 0.000000000000000000, 0.000000000000000000, 1.000000000000000000 ) ) ;
#58618 = ORIENTED_EDGE ( 'NONE', *, *, #8142, .F. ) ;
#58619 = ORIENTED_EDGE ( 'NONE', *, *, #47887, .T. ) ;
#58620 = DIRECTION ( 'NONE',  ( 0.000000000000000000, -1.887379141859195671E-12, 1.000000000000000000 ) ) ;
#58622 = CARTESIAN_POINT ( 'NONE',  ( 7.250000000000005329, -8.249999999999998224, -7.500000000000000000 ) ) ;
#58621 = LINE ( 'NONE', #59662, #54186 ) ;
#58623 = ORIENTED_EDGE ( 'NONE', *, *, #51431, .F. ) ;
#58624 = ORIENTED_EDGE ( 'NONE', *, *, #37493, .T. ) ;
#58626 = ORIENTED_EDGE ( 'NONE', *, *, #68428, .F. ) ;
#58625 = ITEM_DEFINED_TRANSFORMATION ( 'NONE', 'NONE', #25652,  #45918 ) ;
#58627 = DIRECTION ( 'NONE',  ( 0.000000000000000000, 0.000000000000000000, -1.000000000000000000 ) ) ;
#58629 = ORIENTED_EDGE ( 'NONE', *, *, #36199, .F. ) ;
#58628 = CARTESIAN_POINT ( 'NONE',  ( 283.0000000000000568, -32.95000000000000284, -13.19999999999999929 ) ) ;
#58630 = EDGE_CURVE ( 'NONE', #10620, #42134, #43303, .T. ) ;
#58631 = DIRECTION ( 'NONE',  ( -0.000000000000000000, 3.673940397442059868E-16, -1.000000000000000000 ) ) ;
#58632 = CARTESIAN_POINT ( 'NONE',  ( 41.09999999999999432, 20.60000000000000142, 13.86939075806900057 ) ) ;
#58633 = ADVANCED_FACE ( 'NONE', ( #66339 ), #61013, .F. ) ;
#58634 = VERTEX_POINT ( 'NONE', #61359 ) ;
#58635 = EDGE_CURVE ( 'NONE', #68965, #37762, #57992, .T. ) ;
#58636 = VERTEX_POINT ( 'NONE', #34486 ) ;
#58637 = CARTESIAN_POINT ( 'NONE',  ( 9.562023737882814345, -2.544523737882816050, 26.00000000000000711 ) ) ;
#58638 = EDGE_CURVE ( 'NONE', #22897, #54988, #67392, .T. ) ;
#58639 = ORIENTED_EDGE ( 'NONE', *, *, #2509, .F. ) ;
#58640 = CIRCLE ( 'NONE', #69933, 1.500000000000850875 ) ;
#58641 = CARTESIAN_POINT ( 'NONE',  ( -14.25000000000000000, -0.2038245569916330158, -23.22168783648699986 ) ) ;
#58642 = CARTESIAN_POINT ( 'NONE',  ( -11.00000000000000000, -11.50000000000000000, 15.00000000000000000 ) ) ;
#58643 = ADVANCED_FACE ( 'NONE', ( #18946 ), #40502, .T. ) ;
#58644 = DIRECTION ( 'NONE',  ( -0.4999999999989410693, 0.000000000000000000, -0.8660254037850499964 ) ) ;
#58645 = VERTEX_POINT ( 'NONE', #51467 ) ;
#58646 = EDGE_CURVE ( 'NONE', #49618, #57533, #3040, .T. ) ;
#58647 = VECTOR ( 'NONE', #19109, 1000.000000000000114 ) ;
#58648 = FACE_OUTER_BOUND ( 'NONE', #65400, .T. ) ;
#58649 = LINE ( 'NONE', #4903, #49361 ) ;
#58651 = ORIENTED_EDGE ( 'NONE', *, *, #48308, .F. ) ;
#58650 = CARTESIAN_POINT ( 'NONE',  ( 4.206483450353421638, 11.11351654964658486, 455.0000000000000568 ) ) ;
#58653 = ORIENTED_EDGE ( 'NONE', *, *, #26728, .T. ) ;
#58652 = LINE ( 'NONE', #22122, #54674 ) ;
#58654 = CARTESIAN_POINT ( 'NONE',  ( 4.622483450353380263, -3.606483450353491271, 455.0000000000000568 ) ) ;
#58655 = AXIS2_PLACEMENT_3D ( 'NONE', #56976, #24105, #8536 ) ;
#58656 = DIRECTION ( 'NONE',  ( 0.000000000000000000, 0.000000000000000000, 1.000000000000000000 ) ) ;
#58657 = DIRECTION ( 'NONE',  ( -1.000000000000000000, 0.000000000000000000, 0.000000000000000000 ) ) ;
#58658 = B_SPLINE_CURVE_WITH_KNOTS ( 'NONE', 3,
 ( #54149, #6053, #65105, #5712, #54498, #47435 ),
 .UNSPECIFIED., .F., .F.,
 ( 4, 2, 4 ),
 ( 1.820537833122031657, 2.555393473688635897, 3.290249114255240137 ),
 .UNSPECIFIED. ) ;
#58659 = VECTOR ( 'NONE', #43326, 1000.000000000000000 ) ;
#58660 = CARTESIAN_POINT ( 'NONE',  ( -13.00000000000000178, -15.50000000000000000, -14.50000000000000000 ) ) ;
#58661 = VERTEX_POINT ( 'NONE', #67728 ) ;
#58662 = DIRECTION ( 'NONE',  ( -1.000000000000000000, 0.000000000000000000, 0.000000000000000000 ) ) ;
#58663 = PLANE ( 'NONE',  #26003 ) ;
#58664 = DIRECTION ( 'NONE',  ( -5.981805089575196197E-17, -1.000000000000000000, 0.000000000000000000 ) ) ;
#58665 = AXIS2_PLACEMENT_3D ( 'NONE', #54591, #59193, #37984 ) ;
#58667 = ORIENTED_EDGE ( 'NONE', *, *, #60765, .F. ) ;
#58666 = DIRECTION ( 'NONE',  ( -0.7071067811865361374, 0.7071067811865588970, 2.810316974849854557E-30 ) ) ;
#58668 = CARTESIAN_POINT ( 'NONE',  ( 6.006483450353379716, -6.006483450353490738, 455.0000000000000568 ) ) ;
#58669 = EDGE_CURVE ( 'NONE', #36712, #21488, #58540, .T. ) ;
#58670 = CARTESIAN_POINT ( 'NONE',  ( 11.08848345035341687, 10.19191654964656379, 455.0000000000000568 ) ) ;
#58671 = LINE ( 'NONE', #26845, #37572 ) ;
#58672 = AXIS2_PLACEMENT_3D ( 'NONE', #18531, #40085, #61668 ) ;
#58673 = DIRECTION ( 'NONE',  ( -1.000000000000000000, 0.000000000000000000, 0.000000000000000000 ) ) ;
#58674 = VERTEX_POINT ( 'NONE', #52527 ) ;
#58675 = CARTESIAN_POINT ( 'NONE',  ( 7.450000000000006395, 7.250000000000000888, -18.00000000000000000 ) ) ;
#58676 = DIRECTION ( 'NONE',  ( 0.000000000000000000, 1.000000000000000000, 0.000000000000000000 ) ) ;
#58677 = ORIENTED_EDGE ( 'NONE', *, *, #41463, .F. ) ;
#58678 = CARTESIAN_POINT ( 'NONE',  ( 29.25000000000000000, -5.000000000000000000, -11.75000000000000000 ) ) ;
#58679 = DIRECTION ( 'NONE',  ( 1.000000000000000000, -6.308085367188447236E-15, -2.317552966102676720E-30 ) ) ;
#58680 = PLANE ( 'NONE',  #38837 ) ;
#58681 = LINE ( 'NONE', #10237, #67767 ) ;
#58682 = CARTESIAN_POINT ( 'NONE',  ( -7.250000000000000888, -8.249999999999998224, -21.50000000000000000 ) ) ;
#58683 = ORIENTED_EDGE ( 'NONE', *, *, #40878, .T. ) ;
#58684 = ORIENTED_EDGE ( 'NONE', *, *, #47980, .T. ) ;
#58685 = CARTESIAN_POINT ( 'NONE',  ( 50.83090410532631864, 3.657408540445007628, 10.00000000000000000 ) ) ;
#58686 = CIRCLE ( 'NONE', #13482, 2.458500000000000796 ) ;
#58687 = VERTEX_POINT ( 'NONE', #41201 ) ;
#58688 = ORIENTED_EDGE ( 'NONE', *, *, #47210, .T. ) ;
#58689 = DIRECTION ( 'NONE',  ( -1.000000000000000000, 3.491481338843133355E-15, 1.836970198721036590E-16 ) ) ;
#58690 = EDGE_CURVE ( 'NONE', #1782, #40074, #52171, .T. ) ;
#58691 = LINE ( 'NONE', #20157, #62569 ) ;
#58692 = EDGE_CURVE ( 'NONE', #44397, #17399, #15396, .T. ) ;
#58693 = DIRECTION ( 'NONE',  ( -1.000000000000000000, 3.903627567395476653E-15, 1.836970198721037083E-16 ) ) ;
#58694 = ORIENTED_EDGE ( 'NONE', *, *, #62348, .T. ) ;
#58695 = VERTEX_POINT ( 'NONE', #30258 ) ;
#58696 = FACE_OUTER_BOUND ( 'NONE', #49735, .T. ) ;
#58697 = CIRCLE ( 'NONE', #1149, 0.5000000000001357803 ) ;
#58698 = ORIENTED_EDGE ( 'NONE', *, *, #47215, .F. ) ;
#58699 = AXIS2_PLACEMENT_3D ( 'NONE', #38846, #32865, #49122 ) ;
#58700 = ORIENTED_EDGE ( 'NONE', *, *, #47372, .F. ) ;
#58701 = DIRECTION ( 'NONE',  ( 8.673617379884051249E-15, 1.000000000000000000, 0.000000000000000000 ) ) ;
#58702 = CARTESIAN_POINT ( 'NONE',  ( 8.250000000000005329, 0.000000000000000000, -11.00000000000000000 ) ) ;
#58703 = CARTESIAN_POINT ( 'NONE',  ( 7.408280051175162306, 6.775514141871318508, 54.00000000000000711 ) ) ;
#58704 = ADVANCED_FACE ( 'NONE', ( #4447 ), #41561, .F. ) ;
#58705 = ORIENTED_EDGE ( 'NONE', *, *, #36187, .T. ) ;
#58706 = AXIS2_PLACEMENT_3D ( 'NONE', #19758, #52306, #41336 ) ;
#58707 = DIRECTION ( 'NONE',  ( 0.000000000000000000, 0.000000000000000000, 1.000000000000000000 ) ) ;
#58709 = CYLINDRICAL_SURFACE ( 'NONE', #60300, 1.000000000000000000 ) ;
#58708 = CARTESIAN_POINT ( 'NONE',  ( 7.250000000000004441, 7.450000000000001954, -11.50000000000000000 ) ) ;
#58710 = ORIENTED_EDGE ( 'NONE', *, *, #12007, .T. ) ;
#58713 = EDGE_CURVE ( 'NONE', #31923, #46792, #47226, .T. ) ;
#58712 = ORIENTED_EDGE ( 'NONE', *, *, #52802, .F. ) ;
#58711 = LINE ( 'NONE', #16963, #47736 ) ;
#58714 = EDGE_LOOP ( 'NONE', ( #18669, #64687, #57635, #26848 ) ) ;
#58715 = EDGE_CURVE ( 'NONE', #3267, #67437, #9488, .T. ) ;
#58716 = VECTOR ( 'NONE', #51970, 1000.000000000000000 ) ;
#58717 = CARTESIAN_POINT ( 'NONE',  ( -9.722976262117256852, 2.530476262117183683, 54.00000000000000711 ) ) ;
#58718 = CIRCLE ( 'NONE', #49663, 0.5000000000023507862 ) ;
#58719 = LINE ( 'NONE', #36438, #59789 ) ;
#58720 = ADVANCED_FACE ( 'NONE', ( #41906 ), #15041, .F. ) ;
#58721 = ORIENTED_EDGE ( 'NONE', *, *, #64658, .T. ) ;
#58722 = VECTOR ( 'NONE', #59169, 999.9999999999998863 ) ;
#58723 = CARTESIAN_POINT ( 'NONE',  ( 15.50000000000000000, -5.000000000000000000, -22.50000000000000000 ) ) ;
#58724 = CARTESIAN_POINT ( 'NONE',  ( 10.31452373788280141, 6.835476262117187396, 26.00000000000000711 ) ) ;
#58725 = ORIENTED_EDGE ( 'NONE', *, *, #52928, .T. ) ;
#58726 = ORIENTED_EDGE ( 'NONE', *, *, #42186, .F. ) ;
#58727 = CARTESIAN_POINT ( 'NONE',  ( 29.50000000000000355, -11.50000000000100009, 19.50000000000103739 ) ) ;
#58728 = LINE ( 'NONE', #25236, #26715 ) ;
#58729 = EDGE_CURVE ( 'NONE', #66591, #11358, #8685, .T. ) ;
#58730 = CYLINDRICAL_SURFACE ( 'NONE', #54256, 0.3999999999999993006 ) ;
#58731 = ORIENTED_EDGE ( 'NONE', *, *, #34088, .F. ) ;
#58732 = ADVANCED_FACE ( 'NONE', ( #20683 ), #36251, .F. ) ;
#58733 = CARTESIAN_POINT ( 'NONE',  ( -9.781776262117313436, -9.795823737882745519, 54.00000000000000711 ) ) ;
#58734 = AXIS2_PLACEMENT_3D ( 'NONE', #39127, #23210, #34853 ) ;
#58735 = CARTESIAN_POINT ( 'NONE',  ( 10.62249899919920004, -53.81370849898476649, 17.50000000000000000 ) ) ;
#58737 = ORIENTED_EDGE ( 'NONE', *, *, #6487, .F. ) ;
#58736 = CYLINDRICAL_SURFACE ( 'NONE', #46461, 3.500000000000000000 ) ;
#58739 = ORIENTED_EDGE ( 'NONE', *, *, #990, .F. ) ;
#58738 = DIRECTION ( 'NONE',  ( 0.000000000000000000, 1.000000000000000000, 0.000000000000000000 ) ) ;
#58740 = DIRECTION ( 'NONE',  ( 1.000000000000000000, 0.000000000000000000, 0.000000000000000000 ) ) ;
#58741 = DIRECTION ( 'NONE',  ( 0.000000000000000000, 0.000000000000000000, 1.000000000000000000 ) ) ;
#58742 = EDGE_CURVE ( 'NONE', #59802, #35090, #53240, .T. ) ;
#58743 = DIRECTION ( 'NONE',  ( 0.000000000000000000, -3.673940397442059868E-16, 1.000000000000000000 ) ) ;
#58744 = DIRECTION ( 'NONE',  ( -0.7671651518153006499, -0.6414496315691565753, -2.356647714346250026E-16 ) ) ;
#58745 = CARTESIAN_POINT ( 'NONE',  ( -15.50000000000000000, -2.500000000000000000, 21.05662432702600029 ) ) ;
#58746 = CARTESIAN_POINT ( 'NONE',  ( -7.793516549646712477, 11.11351654964660085, 455.0000000000000568 ) ) ;
#58747 = EDGE_LOOP ( 'NONE', ( #1809, #7588, #63314, #25949 ) ) ;
#58748 = PLANE ( 'NONE',  #53063 ) ;
#58749 = CIRCLE ( 'NONE', #36116, 1.399999999999999245 ) ;
#58751 = ORIENTED_EDGE ( 'NONE', *, *, #2942, .T. ) ;
#58750 = FACE_OUTER_BOUND ( 'NONE', #32928, .T. ) ;
#58752 = FACE_OUTER_BOUND ( 'NONE', #50360, .T. ) ;
#58753 = DIRECTION ( 'NONE',  ( 4.121462285523434951E-16, 1.000000000000000000, 3.673940397442059868E-16 ) ) ;
#58754 = FACE_OUTER_BOUND ( 'NONE', #6559, .T. ) ;
#58755 = VECTOR ( 'NONE', #62821, 1000.000000000000000 ) ;
#58756 = ORIENTED_EDGE ( 'NONE', *, *, #4592, .F. ) ;
#58757 = DIRECTION ( 'NONE',  ( 0.000000000000000000, 0.000000000000000000, -1.000000000000000000 ) ) ;
#58758 = DIRECTION ( 'NONE',  ( 0.000000000000000000, 0.000000000000000000, -1.000000000000000000 ) ) ;
#58759 = VERTEX_POINT ( 'NONE', #47909 ) ;
#58760 = CIRCLE ( 'NONE', #22613, 25.39999999999999858 ) ;
#58761 = EDGE_CURVE ( 'NONE', #25574, #65042, #1548, .T. ) ;
#58762 = CARTESIAN_POINT ( 'NONE',  ( -29.50000000000000355, -11.50000000000100009, -15.00000000000084910 ) ) ;
#58763 = LINE ( 'NONE', #10319, #20116 ) ;
#58764 = AXIS2_PLACEMENT_3D ( 'NONE', #1920, #23484, #61286 ) ;
#58765 = AXIS2_PLACEMENT_3D ( 'NONE', #64423, #26241, #31899 ) ;
#58766 = EDGE_CURVE ( 'NONE', #51393, #50235, #52896, .T. ) ;
#58767 = CARTESIAN_POINT ( 'NONE',  ( -8.227189898828745740, 1.620245201994245043, 26.00000000000000711 ) ) ;
#58768 = ORIENTED_EDGE ( 'NONE', *, *, #8300, .F. ) ;
#58769 = CYLINDRICAL_SURFACE ( 'NONE', #58765, 4.000000000000000000 ) ;
#58770 = VERTEX_POINT ( 'NONE', #58174 ) ;
#58771 = EDGE_CURVE ( 'NONE', #55046, #57189, #4093, .T. ) ;
#58772 = ORIENTED_EDGE ( 'NONE', *, *, #59770, .T. ) ;
#58773 = DIRECTION ( 'NONE',  ( 0.000000000000000000, 0.7096009616570518874, -0.7046037717862339012 ) ) ;
#58774 = VECTOR ( 'NONE', #4995, 1000.000000000000000 ) ;
#58775 = CARTESIAN_POINT ( 'NONE',  ( 30.00000000000000000, -17.14999999999999858, -27.00000000000000000 ) ) ;
#58776 = EDGE_CURVE ( 'NONE', #24121, #37027, #31328, .T. ) ;
#58777 = DIRECTION ( 'NONE',  ( 1.000000000000000000, 0.000000000000000000, 0.000000000000000000 ) ) ;
#58778 = EDGE_CURVE ( 'NONE', #69932, #65808, #26346, .T. ) ;
#58779 = DIRECTION ( 'NONE',  ( -0.8660254037844482555, 0.000000000000000000, 0.4999999999999831801 ) ) ;
#58780 = ORIENTED_EDGE ( 'NONE', *, *, #8424, .T. ) ;
#58781 = ORIENTED_EDGE ( 'NONE', *, *, #29796, .F. ) ;
#58783 = ORIENTED_EDGE ( 'NONE', *, *, #4368, .F. ) ;
#58782 = FACE_OUTER_BOUND ( 'NONE', #68376, .T. ) ;
#58784 = ORIENTED_EDGE ( 'NONE', *, *, #65406, .F. ) ;
#58785 = FACE_OUTER_BOUND ( 'NONE', #29719, .T. ) ;
#58786 = DIRECTION ( 'NONE',  ( -4.121462285523434951E-16, -1.000000000000000000, -0.000000000000000000 ) ) ;
#58787 = VECTOR ( 'NONE', #53859, 1000.000000000000000 ) ;
#58788 = CARTESIAN_POINT ( 'NONE',  ( 2.544523737882792069, -8.835729544836324223, 54.00000000000000711 ) ) ;
#58789 = ADVANCED_FACE ( 'NONE', ( #69480 ), #21041, .F. ) ;
#58790 = ADVANCED_FACE ( 'NONE', ( #62772 ), #9028, .T. ) ;
#58791 = CARTESIAN_POINT ( 'NONE',  ( 8.250000000000005329, 8.250000000000001776, -26.00000000000001066 ) ) ;
#58793 = DIRECTION ( 'NONE',  ( 0.000000000000000000, -3.673940397442059868E-16, 1.000000000000000000 ) ) ;
#58792 = DIRECTION ( 'NONE',  ( 0.000000000000000000, -0.1249999999999996531, -0.9921567416492215186 ) ) ;
#58794 = ORIENTED_EDGE ( 'NONE', *, *, #25663, .F. ) ;
#58795 = VERTEX_POINT ( 'NONE', #22439 ) ;
#58796 = ORIENTED_EDGE ( 'NONE', *, *, #6716, .T. ) ;
#58797 = VERTEX_POINT ( 'NONE', #32353 ) ;
#58798 = ADVANCED_FACE ( 'NONE', ( #896 ), #37317, .T. ) ;
#58799 = ADVANCED_FACE ( 'NONE', ( #43987 ), #38353, .T. ) ;
#58800 = DIRECTION ( 'NONE',  ( 1.000000000000000000, 0.000000000000000000, 0.000000000000000000 ) ) ;
#58801 = DIRECTION ( 'NONE',  ( -1.678252938371784572E-14, -1.000000000000000000, -1.836970198721041520E-16 ) ) ;
#58802 = EDGE_CURVE ( 'NONE', #5450, #63858, #58042, .T. ) ;
#58803 = CARTESIAN_POINT ( 'NONE',  ( 41.09999999999999432, -21.00000000000000000, -13.86939075806900057 ) ) ;
#58804 = VECTOR ( 'NONE', #15944, 1000.000000000000000 ) ;
#58805 = ORIENTED_EDGE ( 'NONE', *, *, #53279, .T. ) ;
#58806 = ORIENTED_EDGE ( 'NONE', *, *, #56117, .F. ) ;
#58807 = ORIENTED_EDGE ( 'NONE', *, *, #38805, .F. ) ;
#58808 = AXIS2_PLACEMENT_3D ( 'NONE', #47787, #20568, #27284 ) ;
#58809 = DIRECTION ( 'NONE',  ( -0.000000000000000000, -0.000000000000000000, -1.000000000000000000 ) ) ;
#58810 = ORIENTED_EDGE ( 'NONE', *, *, #34332, .T. ) ;
#58811 = DIRECTION ( 'NONE',  ( -1.836970198721029934E-16, 1.836970198721036590E-16, -1.000000000000000000 ) ) ;
#58812 = CARTESIAN_POINT ( 'NONE',  ( -7.250000000000001776, -7.249999999999998224, -21.00000000000000000 ) ) ;
#58813 = ORIENTED_EDGE ( 'NONE', *, *, #9158, .T. ) ;
#58814 = AXIS2_PLACEMENT_3D ( 'NONE', #6231, #12215, #23180 ) ;
#58815 = ORIENTED_EDGE ( 'NONE', *, *, #64535, .F. ) ;
#58816 = DIRECTION ( 'NONE',  ( -1.836970198721029934E-16, 1.836970198721036344E-16, -1.000000000000000000 ) ) ;
#58817 = EDGE_CURVE ( 'NONE', #37901, #11813, #16089, .T. ) ;
#58819 = VERTEX_POINT ( 'NONE', #43299 ) ;
#58818 = CARTESIAN_POINT ( 'NONE',  ( -11.31351654964671027, 4.393516549646604652, 455.0000000000000568 ) ) ;
#58820 = ORIENTED_EDGE ( 'NONE', *, *, #51501, .T. ) ;
#58821 = AXIS2_PLACEMENT_3D ( 'NONE', #68066, #62757, #15381 ) ;
#58822 = ADVANCED_FACE ( 'NONE', ( #37660 ), #59224, .F. ) ;
#58823 = CARTESIAN_POINT ( 'NONE',  ( 7.000000000000000000, -42.50000000000000000, -15.10000000000000142 ) ) ;
#58825 = ORIENTED_EDGE ( 'NONE', *, *, #51342, .F. ) ;
#58824 = PLANE ( 'NONE',  #30622 ) ;
#58826 = VERTEX_POINT ( 'NONE', #11463 ) ;
#58828 = CARTESIAN_POINT ( 'NONE',  ( 283.0000000000000568, -25.50000000000000355, -17.00000000000000000 ) ) ;
#58827 = AXIS2_PLACEMENT_3D ( 'NONE', #59343, #53013, #43078 ) ;
#58829 = DIRECTION ( 'NONE',  ( 0.000000000000000000, 0.7071067811865475727, 0.7071067811865475727 ) ) ;
#58830 = CARTESIAN_POINT ( 'NONE',  ( 7.000000000000000000, -26.28355339059299922, 9.766446609406699508 ) ) ;
#58831 = DIRECTION ( 'NONE',  ( -1.794541526872559352E-16, -1.000000000000000000, 0.000000000000000000 ) ) ;
#58832 = CARTESIAN_POINT ( 'NONE',  ( 15.89999999999999680, 20.60000000000000142, 13.86939075806899702 ) ) ;
#58833 = EDGE_LOOP ( 'NONE', ( #52870, #50572, #58589, #36069 ) ) ;
#58834 = DIRECTION ( 'NONE',  ( -8.802523127157697409E-15, -1.000000000000000000, -1.836970198721026976E-16 ) ) ;
#58835 = EDGE_LOOP ( 'NONE', ( #7508, #23642, #54911, #30098, #52254 ) ) ;
#58836 = CARTESIAN_POINT ( 'NONE',  ( -30.00000000000000000, -9.200000000000120082, -17.30000000000000071 ) ) ;
#58837 =( NAMED_UNIT ( * ) PLANE_ANGLE_UNIT ( ) SI_UNIT ( $, .RADIAN. ) );
#58838 = VECTOR ( 'NONE', #5583, 1000.000000000000000 ) ;
#58839 = DIRECTION ( 'NONE',  ( 0.000000000000000000, 0.000000000000000000, 1.000000000000000000 ) ) ;
#58840 = LINE ( 'NONE', #10735, #11456 ) ;
#58841 = CARTESIAN_POINT ( 'NONE',  ( 17.00000000000000000, -16.64230188589299786, 14.64519951917100116 ) ) ;
#58842 = ORIENTED_EDGE ( 'NONE', *, *, #62478, .F. ) ;
#58843 = CARTESIAN_POINT ( 'NONE',  ( -6.661338147750939243E-15, -17.79289321881346808, -20.50000000000000000 ) ) ;
#58844 = AXIS2_PLACEMENT_3D ( 'NONE', #28110, #42370, #39062 ) ;
#58845 = FILL_AREA_STYLE_COLOUR ( '', #10760 ) ;
#58846 = ADVANCED_FACE ( 'NONE', ( #11803 ), #5132, .F. ) ;
#58847 = AXIS2_PLACEMENT_3D ( 'NONE', #65511, #10718, #16035 ) ;
#58848 = EDGE_LOOP ( 'NONE', ( #17965, #1985, #36334, #29207 ) ) ;
#58849 = PLANE ( 'NONE',  #58665 ) ;
#58850 = CARTESIAN_POINT ( 'NONE',  ( 25.50000000000000355, -15.50000000000000000, 20.49999999999999645 ) ) ;
#58851 = CARTESIAN_POINT ( 'NONE',  ( 6.657023737882821202, 10.30047626211719347, 54.00000000000000711 ) ) ;
#58852 = EDGE_CURVE ( 'NONE', #27400, #8148, #65942, .T. ) ;
#58853 = ORIENTED_EDGE ( 'NONE', *, *, #38773, .T. ) ;
#58854 = CARTESIAN_POINT ( 'NONE',  ( -11.18999999999999950, 11.25000000000000178, -4.250000000000000000 ) ) ;
#58855 = DIRECTION ( 'NONE',  ( -1.000000000000000000, 0.000000000000000000, 0.000000000000000000 ) ) ;
#58856 = ORIENTED_EDGE ( 'NONE', *, *, #10801, .T. ) ;
#58857 = CARTESIAN_POINT ( 'NONE',  ( -16.75000000000000000, -2.500000000000000000, 23.22168783648699986 ) ) ;
#58858 = CARTESIAN_POINT ( 'NONE',  ( 11.00000000000000000, -16.28999999999710369, -14.50000000000000000 ) ) ;
#58859 = EDGE_CURVE ( 'NONE', #34373, #43142, #5493, .T. ) ;
#58860 = EDGE_CURVE ( 'NONE', #12243, #31223, #11124, .T. ) ;
#58861 = DIRECTION ( 'NONE',  ( 0.000000000000000000, -0.7071067811865474617, 0.7071067811865474617 ) ) ;
#58862 = VECTOR ( 'NONE', #36232, 1000.000000000000000 ) ;
#58863 = AXIS2_PLACEMENT_3D ( 'NONE', #37736, #9828, #10857 ) ;
#58864 = FILL_AREA_STYLE ('',( #15377 ) ) ;
#58865 = EDGE_CURVE ( 'NONE', #25048, #11040, #17124, .T. ) ;
#58866 = CARTESIAN_POINT ( 'NONE',  ( 8.406483450353379183, -6.344579767990935260, 455.0000000000000568 ) ) ;
#58867 = ADVANCED_FACE ( 'NONE', ( #21741 ), #22772, .F. ) ;
#58868 = ORIENTED_EDGE ( 'NONE', *, *, #7106, .T. ) ;
#58870 = ORIENTED_EDGE ( 'NONE', *, *, #59511, .F. ) ;
#58869 = LINE ( 'NONE', #31651, #21557 ) ;
#58871 = CIRCLE ( 'NONE', #8048, 1.000000000000000000 ) ;
#58872 = AXIS2_PLACEMENT_3D ( 'NONE', #56542, #34619, #62905 ) ;
#58873 = DIRECTION ( 'NONE',  ( 0.000000000000000000, 0.000000000000000000, -1.000000000000000000 ) ) ;
#58874 = DIRECTION ( 'NONE',  ( -1.794541526872559352E-16, -1.000000000000000000, 0.000000000000000000 ) ) ;
#58875 = DIRECTION ( 'NONE',  ( 1.000000000000000000, -3.491481338843132961E-15, 0.000000000000000000 ) ) ;
#58876 = VERTEX_POINT ( 'NONE', #21391 ) ;
#58877 = VECTOR ( 'NONE', #68749, 1000.000000000000000 ) ;
#58878 = FACE_OUTER_BOUND ( 'NONE', #26345, .T. ) ;
#58879 = CARTESIAN_POINT ( 'NONE',  ( 3.848229544836322180, -7.532023737882802550, 26.00000000000000000 ) ) ;
#58880 = ORIENTED_EDGE ( 'NONE', *, *, #54380, .T. ) ;
#58881 = EDGE_LOOP ( 'NONE', ( #53757, #17040 ) ) ;
#58882 = VERTEX_POINT ( 'NONE', #10434 ) ;
#58883 = DIRECTION ( 'NONE',  ( -1.000000000000000000, 0.000000000000000000, 0.000000000000000000 ) ) ;
#58884 = CARTESIAN_POINT ( 'NONE',  ( 283.0000000000000568, -42.50000000000000000, 15.10000000000000142 ) ) ;
#58885 = CARTESIAN_POINT ( 'NONE',  ( 25.57999999999999829, 0.000000000000000000, 0.000000000000000000 ) ) ;
#58886 = CIRCLE ( 'NONE', #45321, 24.99999999998784972 ) ;
#58887 = VERTEX_POINT ( 'NONE', #26699 ) ;
#58888 = ORIENTED_EDGE ( 'NONE', *, *, #36016, .T. ) ;
#58889 = DIRECTION ( 'NONE',  ( 0.5773502691896285066, -0.5773502691896285066, -0.5773502691896201799 ) ) ;
#58890 = ORIENTED_EDGE ( 'NONE', *, *, #12557, .T. ) ;
#58891 = ORIENTED_EDGE ( 'NONE', *, *, #13432, .T. ) ;
#58892 = EDGE_LOOP ( 'NONE', ( #44853, #50034 ) ) ;
#58893 = ORIENTED_EDGE ( 'NONE', *, *, #4342, .F. ) ;
#58894 = LINE ( 'NONE', #31341, #5638 ) ;
#58895 = CIRCLE ( 'NONE', #10338, 0.5000000000000000000 ) ;
#58897 = ORIENTED_EDGE ( 'NONE', *, *, #11995, .F. ) ;
#58896 = DIRECTION ( 'NONE',  ( -0.7071067811865490160, 0.7071067811865461294, 0.000000000000000000 ) ) ;
#58898 = CARTESIAN_POINT ( 'NONE',  ( 26.90000000000000213, -0.1999999999911795112, 8.826273045769999343E-12 ) ) ;
#58899 = ADVANCED_FACE ( 'NONE', ( #64196 ), #27738, .F. ) ;
#58900 = VECTOR ( 'NONE', #378, 1000.000000000000000 ) ;
#58901 = LINE ( 'NONE', #21409, #24997 ) ;
#58902 = CARTESIAN_POINT ( 'NONE',  ( -9.722976262117288826, -6.832023737882753522, 26.00000000000000000 ) ) ;
#58903 = EDGE_CURVE ( 'NONE', #17826, #22769, #12837, .T. ) ;
#58904 = VERTEX_POINT ( 'NONE', #1218 ) ;
#58905 = VECTOR ( 'NONE', #19888, 1000.000000000000000 ) ;
#58906 = CIRCLE ( 'NONE', #9234, 0.2000000000000005107 ) ;
#58907 = DIRECTION ( 'NONE',  ( 1.836970198721029934E-16, 1.836970198721010706E-16, -1.000000000000000000 ) ) ;
#58908 = DIRECTION ( 'NONE',  ( 0.000000000000000000, 0.000000000000000000, 1.000000000000000000 ) ) ;
#58909 = ORIENTED_EDGE ( 'NONE', *, *, #9736, .T. ) ;
#58910 = CIRCLE ( 'NONE', #65666, 3.500000000000114131 ) ;
#58911 = PLANE ( 'NONE',  #18743 ) ;
#58912 = DIRECTION ( 'NONE',  ( -1.836970198721029934E-16, 1.836970198721036344E-16, -1.000000000000000000 ) ) ;
#58913 = EDGE_LOOP ( 'NONE', ( #64254, #50902, #32622, #7824, #48385, #24052, #52828, #36612 ) ) ;
#58914 = LINE ( 'NONE', #42290, #30180 ) ;
#58915 = CIRCLE ( 'NONE', #1365, 0.5999999999999989786 ) ;
#58916 = CARTESIAN_POINT ( 'NONE',  ( 10.70000000000000107, -25.60000000000000142, -17.60000000000000142 ) ) ;
#58917 = CYLINDRICAL_SURFACE ( 'NONE', #18973, 0.5250000000000001332 ) ;
#58918 = CARTESIAN_POINT ( 'NONE',  ( -9.689726262117330791, -10.05377373788272699, 54.00000000000000711 ) ) ;
#58919 = VERTEX_POINT ( 'NONE', #524 ) ;
#58920 = CARTESIAN_POINT ( 'NONE',  ( -4.727349090213552429, -4.201500623656063915, 455.0000000000000568 ) ) ;
#58921 = CARTESIAN_POINT ( 'NONE',  ( -7.259684009080030975, -7.811466277050769236, 455.0000000000000568 ) ) ;
#58922 = LINE ( 'NONE', #27436, #19727 ) ;
#58923 = DIRECTION ( 'NONE',  ( -1.000000000000000000, 0.000000000000000000, 0.000000000000000000 ) ) ;
#58924 = EDGE_CURVE ( 'NONE', #53142, #40323, #33392, .T. ) ;
#58925 = ORIENTED_EDGE ( 'NONE', *, *, #19924, .F. ) ;
#58926 = DIRECTION ( 'NONE',  ( 0.000000000000000000, 0.000000000000000000, -1.000000000000000000 ) ) ;
#58927 = LINE ( 'NONE', #10827, #7048 ) ;
#58928 = CARTESIAN_POINT ( 'NONE',  ( -9.722976262117258628, 6.817976262117182884, 54.00000000000000711 ) ) ;
#58929 = DIRECTION ( 'NONE',  ( 1.000000000000000000, -0.000000000000000000, -0.000000000000000000 ) ) ;
#58930 = ORIENTED_EDGE ( 'NONE', *, *, #15672, .T. ) ;
#58931 = LINE ( 'NONE', #64936, #23096 ) ;
#58932 = CARTESIAN_POINT ( 'NONE',  ( 46.39999999999999858, 21.00000000000000000, -2.250000000000000444 ) ) ;
#58933 = EDGE_CURVE ( 'NONE', #55576, #51933, #37706, .T. ) ;
#58934 = FACE_OUTER_BOUND ( 'NONE', #63675, .T. ) ;
#58935 = CARTESIAN_POINT ( 'NONE',  ( 30.00000000000000000, -5.000000000000000000, 27.00000000000000000 ) ) ;
#58936 = EDGE_CURVE ( 'NONE', #17426, #28515, #7546, .T. ) ;
#58937 = FACE_OUTER_BOUND ( 'NONE', #52167, .T. ) ;
#58938 = EDGE_CURVE ( 'NONE', #28168, #51859, #17464, .T. ) ;
#58939 = VECTOR ( 'NONE', #10992, 1000.000000000000000 ) ;
#58940 = ORIENTED_EDGE ( 'NONE', *, *, #3455, .T. ) ;
#58941 = ORIENTED_EDGE ( 'NONE', *, *, #43588, .T. ) ;
#58942 = ADVANCED_FACE ( 'NONE', ( #61629 ), #23111, .T. ) ;
#58943 = DIRECTION ( 'NONE',  ( 0.000000000000000000, 1.000000000000000000, 0.000000000000000000 ) ) ;
#58944 = DIRECTION ( 'NONE',  ( -0.000000000000000000, -0.000000000000000000, -1.000000000000000000 ) ) ;
#58945 = ORIENTED_EDGE ( 'NONE', *, *, #54508, .T. ) ;
#58946 = CARTESIAN_POINT ( 'NONE',  ( -9.942044687070620057, -9.247904806590648619, 195.0000000000000284 ) ) ;
#58947 = CARTESIAN_POINT ( 'NONE',  ( 7.000000000000000000, -21.00000000000000000, 0.000000000000000000 ) ) ;
#58948 = ORIENTED_EDGE ( 'NONE', *, *, #47876, .T. ) ;
#58949 = VECTOR ( 'NONE', #25735, 1000.000000000000000 ) ;
#58950 = CIRCLE ( 'NONE', #55563, 0.2000000000000005107 ) ;
#58951 = CARTESIAN_POINT ( 'NONE',  ( 9.737023737882800845, 7.955476262117190167, 26.00000000000000711 ) ) ;
#58952 = ORIENTED_EDGE ( 'NONE', *, *, #64066, .F. ) ;
#58953 = ORIENTED_EDGE ( 'NONE', *, *, #43677, .F. ) ;
#58954 = LINE ( 'NONE', #52965, #41937 ) ;
#58955 = VERTEX_POINT ( 'NONE', #12496 ) ;
#58956 = VECTOR ( 'NONE', #3553, 1000.000000000000000 ) ;
#58957 = CARTESIAN_POINT ( 'NONE',  ( -4.727349090213560423, -7.811466277050794993, 455.0000000000000568 ) ) ;
#58958 = LINE ( 'NONE', #5226, #11282 ) ;
#58959 = DIRECTION ( 'NONE',  ( 0.000000000000000000, 0.000000000000000000, 1.000000000000000000 ) ) ;
#58960 = VERTEX_POINT ( 'NONE', #55645 ) ;
#58961 = ORIENTED_EDGE ( 'NONE', *, *, #21479, .F. ) ;
#58962 = DIRECTION ( 'NONE',  ( 0.000000000000000000, 0.000000000000000000, 1.000000000000000000 ) ) ;
#58963 = VECTOR ( 'NONE', #45953, 1000.000000000000000 ) ;
#58965 = LINE ( 'NONE', #20088, #42397 ) ;
#58964 = LINE ( 'NONE', #66289, #57541 ) ;
#58966 = EDGE_LOOP ( 'NONE', ( #8171, #19841, #56841, #55900 ) ) ;
#58967 = EDGE_LOOP ( 'NONE', ( #25674, #41032, #26119, #54347 ) ) ;
#58968 = ORIENTED_EDGE ( 'NONE', *, *, #16689, .T. ) ;
#58969 = DIRECTION ( 'NONE',  ( 8.673617379884051249E-15, 1.000000000000000000, 0.000000000000000000 ) ) ;
#58971 = VERTEX_POINT ( 'NONE', #2946 ) ;
#58970 = CARTESIAN_POINT ( 'NONE',  ( -5.655420232009359616, -8.406483450353428921, 455.0000000000000568 ) ) ;
#58972 = DIRECTION ( 'NONE',  ( -0.000000000000000000, -0.000000000000000000, 1.000000000000000000 ) ) ;
#58973 = LINE ( 'NONE', #31058, #48680 ) ;
#58974 = ORIENTED_EDGE ( 'NONE', *, *, #26288, .F. ) ;
#58975 = ORIENTED_EDGE ( 'NONE', *, *, #41917, .T. ) ;
#58976 = EDGE_CURVE ( 'NONE', #68520, #54250, #25283, .T. ) ;
#58977 = EDGE_CURVE ( 'NONE', #23736, #42184, #29121, .T. ) ;
#58978 = EDGE_CURVE ( 'NONE', #24086, #29722, #18497, .T. ) ;
#58979 = DIRECTION ( 'NONE',  ( 1.000000000000000000, -0.000000000000000000, -0.000000000000000000 ) ) ;
#58980 = AXIS2_PLACEMENT_3D ( 'NONE', #38454, #5580, #39129 ) ;
#58981 = VERTEX_POINT ( 'NONE', #28413 ) ;
#58982 = EDGE_CURVE ( 'NONE', #69650, #6870, #39032, .T. ) ;
#58983 = CYLINDRICAL_SURFACE ( 'NONE', #58455, 4.000000000000000000 ) ;
#58984 = LINE ( 'NONE', #11908, #44797 ) ;
#58985 = PLANE ( 'NONE',  #40755 ) ;
#58986 = AXIS2_PLACEMENT_3D ( 'NONE', #60719, #17233, #45140 ) ;
#58987 = EDGE_LOOP ( 'NONE', ( #50236, #7531, #49978, #49807 ) ) ;
#58988 = DIRECTION ( 'NONE',  ( 0.000000000000000000, 0.7071067811865474617, -0.7071067811865474617 ) ) ;
#58989 = LINE ( 'NONE', #49431, #28998 ) ;
#58991 = EDGE_LOOP ( 'NONE', ( #2888, #35811, #40659, #52007, #43386, #53590, #61389, #55444, #12689, #9728, #64865, #31818, #67787, #43861, #53846, #379, #40280 ) ) ;
#58990 = PLANE ( 'NONE',  #25251 ) ;
#58992 = VERTEX_POINT ( 'NONE', #6844 ) ;
#58993 = AXIS2_PLACEMENT_3D ( 'NONE', #67204, #14159, #19807 ) ;
#58994 = CYLINDRICAL_SURFACE ( 'NONE', #25140, 0.2000000000000005107 ) ;
#58995 = DIRECTION ( 'NONE',  ( 0.000000000000000000, 1.000000000000000000, 0.000000000000000000 ) ) ;
#58996 = DIRECTION ( 'NONE',  ( -1.000000000000000000, 0.000000000000000000, 0.000000000000000000 ) ) ;
#58997 = VECTOR ( 'NONE', #60930, 1000.000000000000000 ) ;
#58998 = CARTESIAN_POINT ( 'NONE',  ( 1.480523737882794233, -8.612468434717207799, 26.00000000000000000 ) ) ;
#58999 = DIRECTION ( 'NONE',  ( 0.000000000000000000, -3.673940397442059868E-16, 1.000000000000000000 ) ) ;
#59000 = ORIENTED_EDGE ( 'NONE', *, *, #33247, .F. ) ;
#59001 = CARTESIAN_POINT ( 'NONE',  ( 7.250000000000004441, 7.450000000000001954, -22.50000000000000000 ) ) ;
#59002 = DIRECTION ( 'NONE',  ( -0.000000000000000000, -0.000000000000000000, -1.000000000000000000 ) ) ;
#59003 = DIRECTION ( 'NONE',  ( 1.000000000000000000, -0.000000000000000000, -0.000000000000000000 ) ) ;
#59005 = ORIENTED_EDGE ( 'NONE', *, *, #34807, .T. ) ;
#59004 = CARTESIAN_POINT ( 'NONE',  ( -30.00000000000000000, -15.97213595500069871, -14.50000000000000000 ) ) ;
#59006 = FILL_AREA_STYLE_COLOUR ( '', #35807 ) ;
#59007 = AXIS2_PLACEMENT_3D ( 'NONE', #63824, #15386, #51809 ) ;
#59008 = DIRECTION ( 'NONE',  ( 0.000000000000000000, 0.000000000000000000, -1.000000000000000000 ) ) ;
#59009 = DIRECTION ( 'NONE',  ( -1.836970198721029934E-16, -1.836970198721010706E-16, 1.000000000000000000 ) ) ;
#59010 = LINE ( 'NONE', #10569, #52609 ) ;
#59011 = VECTOR ( 'NONE', #69016, 1000.000000000000000 ) ;
#59012 = ORIENTED_EDGE ( 'NONE', *, *, #45184, .T. ) ;
#59013 = CARTESIAN_POINT ( 'NONE',  ( 283.0000000000000568, -29.94999999999999929, 14.50000000000000000 ) ) ;
#59014 = LINE ( 'NONE', #10572, #54358 ) ;
#59015 = EDGE_LOOP ( 'NONE', ( #8315, #38042, #10864, #33194 ) ) ;
#59016 = DIRECTION ( 'NONE',  ( -0.000000000000000000, -0.000000000000000000, -1.000000000000000000 ) ) ;
#59017 = LINE ( 'NONE', #11261, #36910 ) ;
#59018 = DIRECTION ( 'NONE',  ( -0.7071067811865588970, -0.7071067811865361374, -2.597868168706466299E-16 ) ) ;
#59019 = VECTOR ( 'NONE', #56546, 1000.000000000000114 ) ;
#59020 = DIRECTION ( 'NONE',  ( -1.000000000000000000, 0.000000000000000000, 0.000000000000000000 ) ) ;
#59021 = EDGE_CURVE ( 'NONE', #66347, #48590, #14006, .T. ) ;
#59022 = LINE ( 'NONE', #31817, #27365 ) ;
#59023 = B_SPLINE_CURVE_WITH_KNOTS ( 'NONE', 3,
 ( #16990, #33251, #16292, #54824, #32573, #6382 ),
 .UNSPECIFIED., .F., .F.,
 ( 4, 2, 4 ),
 ( 1.820537833122031213, 2.555393473688635453, 3.290249114255239693 ),
 .UNSPECIFIED. ) ;
#59024 = EDGE_LOOP ( 'NONE', ( #56174, #25279, #48730, #26467 ) ) ;
#59025 = EDGE_CURVE ( 'NONE', #6582, #63655, #34290, .T. ) ;
#59026 = VERTEX_POINT ( 'NONE', #49982 ) ;
#59027 = LINE ( 'NONE', #27207, #31858 ) ;
#59028 = ORIENTED_EDGE ( 'NONE', *, *, #2090, .F. ) ;
#59029 = EDGE_CURVE ( 'NONE', #44582, #8558, #35106, .T. ) ;
#59030 = ORIENTED_EDGE ( 'NONE', *, *, #54718, .F. ) ;
#59031 = CARTESIAN_POINT ( 'NONE',  ( -15.50000000000000000, -15.50000000000000000, -25.99999999999985079 ) ) ;
#59032 = EDGE_CURVE ( 'NONE', #68712, #32441, #28763, .T. ) ;
#59033 = FACE_OUTER_BOUND ( 'NONE', #59885, .T. ) ;
#59034 = CARTESIAN_POINT ( 'NONE',  ( 7.000000000000000000, -20.40000000000000213, -12.40000000000000213 ) ) ;
#59035 = ORIENTED_EDGE ( 'NONE', *, *, #48658, .F. ) ;
#59036 = ADVANCED_FACE ( 'NONE', ( #1904 ), #51034, .F. ) ;
#59037 = EDGE_LOOP ( 'NONE', ( #69840, #18952, #1922, #4848, #32789, #63728 ) ) ;
#59038 = AXIS2_PLACEMENT_3D ( 'NONE', #52203, #24644, #51511 ) ;
#59039 = DIRECTION ( 'NONE',  ( 1.000000000000000000, -0.000000000000000000, -0.000000000000000000 ) ) ;
#59041 = ORIENTED_EDGE ( 'NONE', *, *, #28749, .F. ) ;
#59040 = EDGE_CURVE ( 'NONE', #25574, #57533, #23815, .T. ) ;
#59042 = EDGE_LOOP ( 'NONE', ( #25780, #10960, #47662, #26291, #40117, #35334, #68897, #62505, #791, #45652 ) ) ;
#59043 = DIRECTION ( 'NONE',  ( -1.000000000000000000, 1.047444401652939849E-14, 0.000000000000000000 ) ) ;
#59044 = CARTESIAN_POINT ( 'NONE',  ( -11.50000000000000000, -11.50000000000100009, -15.00000000000084910 ) ) ;
#59045 = DIRECTION ( 'NONE',  ( 0.7071067811865451302, -0.7071067811865500152, -2.597868168706484048E-16 ) ) ;
#59046 = ORIENTED_EDGE ( 'NONE', *, *, #42927, .F. ) ;
#59047 = FACE_OUTER_BOUND ( 'NONE', #57029, .T. ) ;
#59049 = DIRECTION ( 'NONE',  ( 1.000000000000000000, -0.000000000000000000, 0.000000000000000000 ) ) ;
#59048 = FACE_OUTER_BOUND ( 'NONE', #57586, .T. ) ;
#59050 = ORIENTED_EDGE ( 'NONE', *, *, #23572, .T. ) ;
#59052 = ORIENTED_EDGE ( 'NONE', *, *, #35787, .T. ) ;
#59051 = DIRECTION ( 'NONE',  ( 0.000000000000000000, 0.000000000000000000, 1.000000000000000000 ) ) ;
#59053 = VERTEX_POINT ( 'NONE', #44328 ) ;
#59054 = DIRECTION ( 'NONE',  ( 0.000000000000000000, 0.000000000000000000, 1.000000000000000000 ) ) ;
#59055 = DIRECTION ( 'NONE',  ( -1.000000000000000000, 0.000000000000000000, 0.000000000000000000 ) ) ;
#59056 = AXIS2_PLACEMENT_3D ( 'NONE', #54184, #26604, #5742 ) ;
#59057 = ORIENTED_EDGE ( 'NONE', *, *, #40326, .F. ) ;
#59058 = VECTOR ( 'NONE', #4837, 1000.000000000000000 ) ;
#59060 = DIRECTION ( 'NONE',  ( 0.7071067811865451302, -0.7071067811865500152, 0.000000000000000000 ) ) ;
#59059 = VECTOR ( 'NONE', #43357, 1000.000000000000000 ) ;
#59061 = DIRECTION ( 'NONE',  ( 3.540573132209561620E-15, 1.000000000000000000, 0.000000000000000000 ) ) ;
#59062 = EDGE_LOOP ( 'NONE', ( #7857, #46407, #17611, #2790 ) ) ;
#59063 = ORIENTED_EDGE ( 'NONE', *, *, #34568, .T. ) ;
#59064 = ADVANCED_FACE ( 'NONE', ( #66940 ), #61985, .F. ) ;
#59065 = CARTESIAN_POINT ( 'NONE',  ( -4.173516549646839380, -12.00648345035344811, 455.0000000000000568 ) ) ;
#59066 = LINE ( 'NONE', #10622, #66222 ) ;
#59067 = VECTOR ( 'NONE', #9791, 1000.000000000000000 ) ;
#59068 = CARTESIAN_POINT ( 'NONE',  ( -30.00000000000000000, -5.000000000000000000, -27.00000000000000000 ) ) ;
#59069 = VERTEX_POINT ( 'NONE', #29467 ) ;
#59070 = VECTOR ( 'NONE', #50869, 1000.000000000000000 ) ;
#59071 = DIRECTION ( 'NONE',  ( -1.000000000000000000, 0.000000000000000000, 0.000000000000000000 ) ) ;
#59072 = DIRECTION ( 'NONE',  ( -1.000000000000000000, 2.135044278125299371E-15, 0.000000000000000000 ) ) ;
#59074 = VERTEX_POINT ( 'NONE', #18858 ) ;
#59073 = CARTESIAN_POINT ( 'NONE',  ( 10.92648345035337520, -9.106483450353398013, 195.0000000000000284 ) ) ;
#59076 = VERTEX_POINT ( 'NONE', #40430 ) ;
#59075 = CARTESIAN_POINT ( 'NONE',  ( -17.24945551514599984, -17.50000000000000000, -25.53140320652400064 ) ) ;
#59077 = CARTESIAN_POINT ( 'NONE',  ( 7.450000000000006395, 7.250000000000000888, -9.500000000000001776 ) ) ;
#59078 = ADVANCED_FACE ( 'NONE', ( #56691 ), #29812, .F. ) ;
#59079 = CARTESIAN_POINT ( 'NONE',  ( -11.00000000000000000, -13.79999999999979998, -17.30000000000000071 ) ) ;
#59080 = AXIS2_PLACEMENT_3D ( 'NONE', #9359, #53216, #37288 ) ;
#59081 = CARTESIAN_POINT ( 'NONE',  ( 11.78648345035337819, -4.406483450353394282, 195.0000000000000284 ) ) ;
#59082 = LINE ( 'NONE', #6383, #26755 ) ;
#59083 = CARTESIAN_POINT ( 'NONE',  ( 289.5000000000000000, -42.00000000000000000, -27.00000000000000000 ) ) ;
#59084 = EDGE_CURVE ( 'NONE', #55561, #63676, #69350, .T. ) ;
#59085 = CARTESIAN_POINT ( 'NONE',  ( 283.0000000000000568, -21.00000000000000000, -12.50000000000000000 ) ) ;
#59086 = VECTOR ( 'NONE', #30355, 1000.000000000000000 ) ;
#59087 = EDGE_LOOP ( 'NONE', ( #54082, #9865, #30207, #42038 ) ) ;
#59088 = LINE ( 'NONE', #21615, #14631 ) ;
#59090 = EDGE_LOOP ( 'NONE', ( #54067, #31319, #12749, #67301 ) ) ;
#59089 = FACE_OUTER_BOUND ( 'NONE', #9369, .T. ) ;
#59092 = ORIENTED_EDGE ( 'NONE', *, *, #36009, .F. ) ;
#59091 = LINE ( 'NONE', #48488, #3938 ) ;
#59093 = SURFACE_STYLE_FILL_AREA ( #38907 ) ;
#59094 = AXIS2_PLACEMENT_3D ( 'NONE', #55820, #50517, #66767 ) ;
#59095 = CARTESIAN_POINT ( 'NONE',  ( 275.0000000000000000, -32.00000000000000000, -8.400000000000000355 ) ) ;
#59096 = EDGE_LOOP ( 'NONE', ( #67839, #3761, #24024, #26220 ) ) ;
#59097 = DIRECTION ( 'NONE',  ( -1.000000000000000000, 0.000000000000000000, 0.000000000000000000 ) ) ;
#59098 = CARTESIAN_POINT ( 'NONE',  ( -6.606374702650164465, -4.747751991980617703, 195.0000000000000284 ) ) ;
#59099 = EDGE_CURVE ( 'NONE', #63655, #56223, #24864, .T. ) ;
#59100 = ORIENTED_EDGE ( 'NONE', *, *, #3222, .F. ) ;
#59101 = DIRECTION ( 'NONE',  ( 0.000000000000000000, -1.000000000000000000, 0.000000000000000000 ) ) ;
#59102 = LINE ( 'NONE', #33614, #46193 ) ;
#59103 = LINE ( 'NONE', #15974, #7673 ) ;
#59104 = AXIS2_PLACEMENT_3D ( 'NONE', #15630, #69010, #58757 ) ;
#59105 = VECTOR ( 'NONE', #5908, 1000.000000000000114 ) ;
#59106 = VERTEX_POINT ( 'NONE', #47142 ) ;
#59107 = EDGE_CURVE ( 'NONE', #45635, #43736, #42169, .T. ) ;
#59108 = DIRECTION ( 'NONE',  ( -1.000000000000000000, 0.000000000000000000, 0.000000000000000000 ) ) ;
#59109 = ORIENTED_EDGE ( 'NONE', *, *, #16892, .F. ) ;
#59110 = ORIENTED_EDGE ( 'NONE', *, *, #34535, .T. ) ;
#59111 = AXIS2_PLACEMENT_3D ( 'NONE', #13436, #8468, #19094 ) ;
#59112 = DIRECTION ( 'NONE',  ( 0.000000000000000000, -1.000000000000000000, -6.036837696397607468E-13 ) ) ;
#59113 = DIRECTION ( 'NONE',  ( -1.000000000000000000, 0.000000000000000000, 0.000000000000000000 ) ) ;
#59114 = PRESENTATION_LAYER_ASSIGNMENT (  '', '', ( #18450 ) ) ;
#59115 = VECTOR ( 'NONE', #4009, 1000.000000000000000 ) ;
#59116 = DIRECTION ( 'NONE',  ( 0.000000000000000000, 0.000000000000000000, 1.000000000000000000 ) ) ;
#59117 = VECTOR ( 'NONE', #2018, 1000.000000000000000 ) ;
#59118 = VECTOR ( 'NONE', #28015, 1000.000000000000000 ) ;
#59119 = LINE ( 'NONE', #43889, #37459 ) ;
#59120 = ORIENTED_EDGE ( 'NONE', *, *, #15469, .T. ) ;
#59121 = EDGE_CURVE ( 'NONE', #21614, #44081, #30171, .T. ) ;
#59122 = EDGE_LOOP ( 'NONE', ( #30747, #68599, #66363, #33178 ) ) ;
#59124 = ORIENTED_EDGE ( 'NONE', *, *, #32476, .F. ) ;
#59123 = DIRECTION ( 'NONE',  ( 0.6414496315691539108, -0.7671651518153028704, -2.587583378555131256E-16 ) ) ;
#59126 = ORIENTED_EDGE ( 'NONE', *, *, #32449, .F. ) ;
#59125 = EDGE_CURVE ( 'NONE', #6262, #21629, #63754, .T. ) ;
#59127 = DIRECTION ( 'NONE',  ( 0.000000000000000000, 1.000000000000000000, 0.000000000000000000 ) ) ;
#59128 = CARTESIAN_POINT ( 'NONE',  ( 4.396432944014576627, 8.393516549646587777, 455.0000000000000568 ) ) ;
#59129 = DIRECTION ( 'NONE',  ( 0.000000000000000000, 0.000000000000000000, 1.000000000000000000 ) ) ;
#59130 = CARTESIAN_POINT ( 'NONE',  ( 7.450000000000003730, -7.249999999999997335, -11.50000000000000000 ) ) ;
#59132 = DIRECTION ( 'NONE',  ( -1.000000000000000000, 1.047444401652939849E-14, 0.000000000000000000 ) ) ;
#59131 = DIRECTION ( 'NONE',  ( 0.000000000000000000, -0.000000000000000000, -1.000000000000000000 ) ) ;
#59133 = ORIENTED_EDGE ( 'NONE', *, *, #32966, .T. ) ;
#59135 = ORIENTED_EDGE ( 'NONE', *, *, #29936, .T. ) ;
#59134 = DIRECTION ( 'NONE',  ( 0.000000000000000000, 3.673940397442059868E-16, -1.000000000000000000 ) ) ;
#59136 = EDGE_CURVE ( 'NONE', #14058, #13109, #41120, .T. ) ;
#59137 = ORIENTED_EDGE ( 'NONE', *, *, #14717, .F. ) ;
#59138 = ORIENTED_EDGE ( 'NONE', *, *, #65300, .T. ) ;
#59139 = DIRECTION ( 'NONE',  ( 1.000000000000000000, 0.000000000000000000, 0.000000000000000000 ) ) ;
#59140 = CARTESIAN_POINT ( 'NONE',  ( -18.85410196625000268, -15.50000000000000000, 21.50000000000000000 ) ) ;
#59141 = DIRECTION ( 'NONE',  ( 1.000000000000000000, -0.000000000000000000, 0.000000000000000000 ) ) ;
#59142 = ORIENTED_EDGE ( 'NONE', *, *, #38437, .T. ) ;
#59143 = VERTEX_POINT ( 'NONE', #36165 ) ;
#59144 = ORIENTED_EDGE ( 'NONE', *, *, #46784, .T. ) ;
#59145 = CARTESIAN_POINT ( 'NONE',  ( -2.355476262117325525, -9.562023737882830332, 54.00000000000000711 ) ) ;
#59146 = DIRECTION ( 'NONE',  ( 0.000000000000000000, 1.000000000000000000, 0.000000000000000000 ) ) ;
#59147 = CARTESIAN_POINT ( 'NONE',  ( 4.406483450353335662, -11.78648345035347766, 455.0000000000000568 ) ) ;
#59148 = ORIENTED_EDGE ( 'NONE', *, *, #275, .F. ) ;
#59149 = EDGE_CURVE ( 'NONE', #22769, #38702, #20258, .T. ) ;
#59150 = VERTEX_POINT ( 'NONE', #30515 ) ;
#59151 = CARTESIAN_POINT ( 'NONE',  ( -11.31351654964678843, -7.606483450353371367, 455.0000000000000568 ) ) ;
#59152 = CARTESIAN_POINT ( 'NONE',  ( 0.000000000000000000, -7.449999999999998401, -23.50000000000000000 ) ) ;
#59153 = ORIENTED_EDGE ( 'NONE', *, *, #13703, .F. ) ;
#59154 = EDGE_CURVE ( 'NONE', #14428, #28990, #46424, .T. ) ;
#59155 = AXIS2_PLACEMENT_3D ( 'NONE', #59792, #11344, #43174 ) ;
#59156 = AXIS2_PLACEMENT_3D ( 'NONE', #38691, #28086, #54273 ) ;
#59157 = CARTESIAN_POINT ( 'NONE',  ( -11.75000000000000000, -5.200000000000001066, 11.75000000000000000 ) ) ;
#59158 = EDGE_CURVE ( 'NONE', #27929, #1782, #14604, .T. ) ;
#59160 = ORIENTED_EDGE ( 'NONE', *, *, #68682, .T. ) ;
#59159 = DIRECTION ( 'NONE',  ( 0.000000000000000000, 0.000000000000000000, 1.000000000000000000 ) ) ;
#59161 = ORIENTED_EDGE ( 'NONE', *, *, #12131, .F. ) ;
#59162 = DIRECTION ( 'NONE',  ( 1.000000000000000000, 0.000000000000000000, 0.000000000000000000 ) ) ;
#59163 = CARTESIAN_POINT ( 'NONE',  ( 39.00000000000000000, 21.00000000000000000, 13.98999642601811999 ) ) ;
#59164 = VECTOR ( 'NONE', #45696, 1000.000000000000000 ) ;
#59165 = AXIS2_PLACEMENT_3D ( 'NONE', #23660, #8088, #18706 ) ;
#59166 = ADVANCED_FACE ( 'NONE', ( #58459 ), #57388, .F. ) ;
#59167 = LINE ( 'NONE', #53883, #59983 ) ;
#59168 = LINE ( 'NONE', #54569, #41381 ) ;
#59169 = DIRECTION ( 'NONE',  ( -0.7071067811865391350, 0.7071067811865560104, 1.750285133459120294E-30 ) ) ;
#59170 = VECTOR ( 'NONE', #48035, 1000.000000000000000 ) ;
#59171 = VECTOR ( 'NONE', #51286, 1000.000000000000000 ) ;
#59172 = AXIS2_PLACEMENT_3D ( 'NONE', #10368, #32279, #21674 ) ;
#59173 = EDGE_CURVE ( 'NONE', #6619, #57899, #52089, .T. ) ;
#59174 = EDGE_LOOP ( 'NONE', ( #13184, #25956, #59221, #67061, #1865 ) ) ;
#59175 = CYLINDRICAL_SURFACE ( 'NONE', #39399, 2.250000000000001776 ) ;
#59176 = ORIENTED_EDGE ( 'NONE', *, *, #14967, .F. ) ;
#59177 = DIRECTION ( 'NONE',  ( -1.000000000000000000, 0.000000000000000000, 0.000000000000000000 ) ) ;
#59178 = LINE ( 'NONE', #16388, #32345 ) ;
#59179 = EDGE_CURVE ( 'NONE', #11814, #41587, #19658, .T. ) ;
#59180 = CARTESIAN_POINT ( 'NONE',  ( -7.603567055985545942, 8.593516549646603053, 195.0000000000000284 ) ) ;
#59182 = EDGE_CURVE ( 'NONE', #26651, #15828, #57034, .T. ) ;
#59181 = AXIS2_PLACEMENT_3D ( 'NONE', #43558, #54530, #11378 ) ;
#59183 = CARTESIAN_POINT ( 'NONE',  ( -8.821682069070824639, -7.969523737882762582, 26.00000000000000000 ) ) ;
#59184 = CYLINDRICAL_SURFACE ( 'NONE', #30289, 0.5000000000079367624 ) ;
#59185 = EDGE_CURVE ( 'NONE', #22480, #63319, #19909, .T. ) ;
#59186 = EDGE_CURVE ( 'NONE', #18830, #36149, #51313, .T. ) ;
#59187 = EDGE_CURVE ( 'NONE', #60907, #43920, #4005, .T. ) ;
#59188 = VERTEX_POINT ( 'NONE', #25932 ) ;
#59189 = SURFACE_STYLE_FILL_AREA ( #4412 ) ;
#59190 = EDGE_CURVE ( 'NONE', #62916, #65806, #9664, .T. ) ;
#59191 = ORIENTED_EDGE ( 'NONE', *, *, #46218, .F. ) ;
#59192 = EDGE_CURVE ( 'NONE', #61399, #5119, #4371, .T. ) ;
#59193 = DIRECTION ( 'NONE',  ( -0.7071067811865552333, -0.7071067811865398012, 2.368893831596300099E-30 ) ) ;
#59194 = DIRECTION ( 'NONE',  ( -1.000000000000000000, 0.000000000000000000, 0.000000000000000000 ) ) ;
#59195 = ORIENTED_EDGE ( 'NONE', *, *, #2545, .F. ) ;
#59196 = ADVANCED_FACE ( 'NONE', ( #31584 ), #5418, .F. ) ;
#59197 = DIRECTION ( 'NONE',  ( 1.000000000000000000, 0.000000000000000000, 0.000000000000000000 ) ) ;
#59198 = FACE_OUTER_BOUND ( 'NONE', #4000, .T. ) ;
#59199 = ORIENTED_EDGE ( 'NONE', *, *, #24056, .F. ) ;
#59200 = CARTESIAN_POINT ( 'NONE',  ( 7.000000000000000000, -42.50000000000000000, 7.500000000000000000 ) ) ;
#59201 = VECTOR ( 'NONE', #69643, 1000.000000000000000 ) ;
#59202 = CARTESIAN_POINT ( 'NONE',  ( 283.0000000000000568, -38.10000000000000142, 8.400000000000000355 ) ) ;
#59203 = CARTESIAN_POINT ( 'NONE',  ( 39.00000000000000000, -16.96999999999999886, -21.00000000000000000 ) ) ;
#59204 = CARTESIAN_POINT ( 'NONE',  ( -11.50000000000000000, -11.50000000000100009, 15.00000000000084910 ) ) ;
#59205 = ADVANCED_FACE ( 'NONE', ( #4705 ), #26269, .T. ) ;
#59206 = ORIENTED_EDGE ( 'NONE', *, *, #5254, .F. ) ;
#59208 = ORIENTED_EDGE ( 'NONE', *, *, #52227, .F. ) ;
#59207 = LINE ( 'NONE', #64864, #46374 ) ;
#59209 = EDGE_CURVE ( 'NONE', #4613, #69832, #27319, .T. ) ;
#59210 = AXIS2_PLACEMENT_3D ( 'NONE', #55780, #60733, #50477 ) ;
#59211 = VECTOR ( 'NONE', #58089, 1000.000000000000000 ) ;
#59212 = LINE ( 'NONE', #33027, #42889 ) ;
#59213 = CARTESIAN_POINT ( 'NONE',  ( -30.00000000000000000, -11.50000000000100009, 10.50000000000065903 ) ) ;
#59214 = LINE ( 'NONE', #34049, #308 ) ;
#59215 = ORIENTED_EDGE ( 'NONE', *, *, #31239, .T. ) ;
#59216 = LINE ( 'NONE', #10766, #48055 ) ;
#59217 = VECTOR ( 'NONE', #43539, 1000.000000000000000 ) ;
#59218 = DIRECTION ( 'NONE',  ( 1.000000000000000000, -1.610765207321970913E-14, 0.000000000000000000 ) ) ;
#59219 = AXIS2_PLACEMENT_3D ( 'NONE', #68305, #19160, #9261 ) ;
#59220 = ORIENTED_EDGE ( 'NONE', *, *, #102, .T. ) ;
#59221 = ORIENTED_EDGE ( 'NONE', *, *, #27103, .T. ) ;
#59223 = VERTEX_POINT ( 'NONE', #53498 ) ;
#59222 = CIRCLE ( 'NONE', #60307, 0.1749999999999998224 ) ;
#59224 = PLANE ( 'NONE',  #62562 ) ;
#59225 = DIRECTION ( 'NONE',  ( -1.000000000000000000, -1.570596175624152093E-15, 0.000000000000000000 ) ) ;
#59226 = ORIENTED_EDGE ( 'NONE', *, *, #66621, .T. ) ;
#59227 = EDGE_LOOP ( 'NONE', ( #8758, #25214, #19379, #51232 ) ) ;
#59228 = AXIS2_PLACEMENT_3D ( 'NONE', #8857, #25478, #46335 ) ;
#59229 = DIRECTION ( 'NONE',  ( -1.000000000000000000, 0.000000000000000000, 0.000000000000000000 ) ) ;
#59230 = EDGE_LOOP ( 'NONE', ( #67932, #15979, #59890, #4715 ) ) ;
#59231 = VERTEX_POINT ( 'NONE', #65489 ) ;
#59232 = ORIENTED_EDGE ( 'NONE', *, *, #35517, .T. ) ;
#59233 = VERTEX_POINT ( 'NONE', #59140 ) ;
#59234 = DIRECTION ( 'NONE',  ( 1.000000000000000000, 0.000000000000000000, 0.000000000000000000 ) ) ;
#59235 = UNCERTAINTY_MEASURE_WITH_UNIT (LENGTH_MEASURE( 1.000000000000000082E-05 ), #1868, 'distance_accuracy_value', 'NONE');
#59237 = VERTEX_POINT ( 'NONE', #47825 ) ;
#59236 = PLANE ( 'NONE',  #69499 ) ;
#59238 = ADVANCED_FACE ( 'NONE', ( #48188 ), #69395, .F. ) ;
#59239 = CARTESIAN_POINT ( 'NONE',  ( -28.00000000000000000, -17.35230188589299871, 15.35019951917099945 ) ) ;
#59240 = DIRECTION ( 'NONE',  ( -0.7071067811865475727, -0.7071067811865475727, -2.597868168706480597E-16 ) ) ;
#59241 = FACE_OUTER_BOUND ( 'NONE', #69591, .T. ) ;
#59242 = AXIS2_PLACEMENT_3D ( 'NONE', #37474, #57633, #20505 ) ;
#59243 = EDGE_CURVE ( 'NONE', #40746, #56650, #37932, .T. ) ;
#59244 = ORIENTED_EDGE ( 'NONE', *, *, #17816, .T. ) ;
#59245 = EDGE_CURVE ( 'NONE', #10498, #34600, #20956, .T. ) ;
#59246 = VECTOR ( 'NONE', #69544, 1000.000000000000000 ) ;
#59247 = DIRECTION ( 'NONE',  ( -1.000000000000000000, 0.000000000000000000, 0.000000000000000000 ) ) ;
#59248 = EDGE_CURVE ( 'NONE', #32586, #12501, #26501, .T. ) ;
#59249 = LINE ( 'NONE', #34008, #40564 ) ;
#59250 = ORIENTED_EDGE ( 'NONE', *, *, #9838, .F. ) ;
#59251 = DIRECTION ( 'NONE',  ( 0.6785983445458472207, -0.6785983445458458885, -0.2810846377148227826 ) ) ;
#59252 = VECTOR ( 'NONE', #49380, 1000.000000000000000 ) ;
#59253 = VECTOR ( 'NONE', #1725, 1000.000000000000000 ) ;
#59254 = DIRECTION ( 'NONE',  ( 0.000000000000000000, 0.6857142857146703019, -0.7278708115914659382 ) ) ;
#59255 = CARTESIAN_POINT ( 'NONE',  ( 8.144523737882810366, 9.547976262117190416, 26.00000000000000711 ) ) ;
#59256 = ORIENTED_EDGE ( 'NONE', *, *, #30919, .F. ) ;
#59257 = CARTESIAN_POINT ( 'NONE',  ( -9.722976262117256852, 2.530476262117183683, 26.00000000000000711 ) ) ;
#59258 = CYLINDRICAL_SURFACE ( 'NONE', #31941, 0.8100000000000017186 ) ;
#59259 = DIRECTION ( 'NONE',  ( -1.836970198721029934E-16, 1.836970198721036344E-16, -1.000000000000000000 ) ) ;
#59260 = ADVANCED_FACE ( 'NONE', ( #32270 ), #53849, .F. ) ;
#59261 = AXIS2_PLACEMENT_3D ( 'NONE', #34397, #18857, #55992 ) ;
#59262 = CARTESIAN_POINT ( 'NONE',  ( 6.750000000000000000, 7.750000000000000000, 5.000000000000000000 ) ) ;
#59263 = DIRECTION ( 'NONE',  ( 0.000000000000000000, -1.000000000000000000, 0.000000000000000000 ) ) ;
#59264 = DIRECTION ( 'NONE',  ( 1.000000000000000000, 0.000000000000000000, 0.000000000000000000 ) ) ;
#59265 = CARTESIAN_POINT ( 'NONE',  ( -8.250000000000001776, -7.249999999999998224, -26.00000000000001066 ) ) ;
#59266 = CARTESIAN_POINT ( 'NONE',  ( 9.247904806590689475, -9.955011587777253368, 195.0000000000000284 ) ) ;
#59267 = VECTOR ( 'NONE', #22137, 1000.000000000000000 ) ;
#59268 = EDGE_LOOP ( 'NONE', ( #25738, #25879, #619, #60212 ) ) ;
#59269 = DIRECTION ( 'NONE',  ( 0.000000000000000000, 0.000000000000000000, -1.000000000000000000 ) ) ;
#59270 = LINE ( 'NONE', #32054, #34146 ) ;
#59271 = STYLED_ITEM ( 'NONE', ( #69167 ), #43380 ) ;
#59272 = CARTESIAN_POINT ( 'NONE',  ( 8.250000000000005329, 8.250000000000001776, -26.00000000000001066 ) ) ;
#59273 = CARTESIAN_POINT ( 'NONE',  ( 25.50000000000000355, -5.578999999999999737, -22.50000000000000000 ) ) ;
#59274 = EDGE_LOOP ( 'NONE', ( #24695, #56889, #19523, #5041 ) ) ;
#59275 = CARTESIAN_POINT ( 'NONE',  ( 7.250000000000005329, -7.449999999999998401, -14.50000000000000000 ) ) ;
#59276 = CARTESIAN_POINT ( 'NONE',  ( 10.70000000000000107, -20.40000000000000213, 17.60000000000000142 ) ) ;
#59277 = LINE ( 'NONE', #9811, #14217 ) ;
#59278 = CARTESIAN_POINT ( 'NONE',  ( 3.664523737882819709, 10.30047626211720413, 54.00000000000000711 ) ) ;
#59279 = DIRECTION ( 'NONE',  ( 0.000000000000000000, 0.000000000000000000, -1.000000000000000000 ) ) ;
#59280 = DIRECTION ( 'NONE',  ( -1.000000000000000000, 0.000000000000000000, 0.000000000000000000 ) ) ;
#59281 = ADVANCED_FACE ( 'NONE', ( #26616 ), #15664, .T. ) ;
#59282 = ORIENTED_EDGE ( 'NONE', *, *, #40561, .F. ) ;
#59283 = EDGE_CURVE ( 'NONE', #7725, #45178, #43396, .T. ) ;
#59284 = ORIENTED_EDGE ( 'NONE', *, *, #22656, .F. ) ;
#59285 = DIRECTION ( 'NONE',  ( 0.000000000000000000, 1.000000000000000000, 0.000000000000000000 ) ) ;
#59286 = DIRECTION ( 'NONE',  ( 0.000000000000000000, -1.000000000000000000, 0.000000000000000000 ) ) ;
#59287 = ORIENTED_EDGE ( 'NONE', *, *, #60547, .T. ) ;
#59288 = EDGE_CURVE ( 'NONE', #12989, #11613, #99, .T. ) ;
#59289 = LINE ( 'NONE', #33713, #64210 ) ;
#59290 = PLANE ( 'NONE',  #3581 ) ;
#59291 = AXIS2_PLACEMENT_3D ( 'NONE', #6503, #17791, #17436 ) ;
#59292 = VERTEX_POINT ( 'NONE', #11047 ) ;
#59293 = CARTESIAN_POINT ( 'NONE',  ( -14.25000000000000000, -2.500000000000000000, -21.77831216351300014 ) ) ;
#59294 = ORIENTED_EDGE ( 'NONE', *, *, #26445, .T. ) ;
#59295 = ORIENTED_EDGE ( 'NONE', *, *, #21141, .F. ) ;
#59296 = CARTESIAN_POINT ( 'NONE',  ( 7.250000000000005329, -7.249999999999998224, -10.50000000000000000 ) ) ;
#59297 = ORIENTED_EDGE ( 'NONE', *, *, #31727, .F. ) ;
#59298 = CARTESIAN_POINT ( 'NONE',  ( 31.89999999999999858, -21.00000000000001421, -13.86939075806900945 ) ) ;
#59299 = PLANE ( 'NONE',  #23689 ) ;
#59300 = LINE ( 'NONE', #4869, #38127 ) ;
#59301 = VECTOR ( 'NONE', #8191, 1000.000000000000000 ) ;
#59302 = AXIS2_PLACEMENT_3D ( 'NONE', #2957, #51392, #40790 ) ;
#59303 = AXIS2_PLACEMENT_3D ( 'NONE', #35728, #36078, #30077 ) ;
#59304 = ORIENTED_EDGE ( 'NONE', *, *, #42882, .T. ) ;
#59305 = ORIENTED_EDGE ( 'NONE', *, *, #61539, .T. ) ;
#59306 = DIRECTION ( 'NONE',  ( 1.000000000000000000, -0.000000000000000000, 0.000000000000000000 ) ) ;
#59308 = DIRECTION ( 'NONE',  ( -1.000000000000000000, 0.000000000000000000, 0.000000000000000000 ) ) ;
#59307 = CARTESIAN_POINT ( 'NONE',  ( -3.842976262117329345, -9.912023737882817542, 54.00000000000000711 ) ) ;
#59309 = VECTOR ( 'NONE', #16529, 1000.000000000000000 ) ;
#59310 = VECTOR ( 'NONE', #38684, 1000.000000000000000 ) ;
#59311 = ORIENTED_EDGE ( 'NONE', *, *, #1405, .T. ) ;
#59312 = ORIENTED_EDGE ( 'NONE', *, *, #15677, .F. ) ;
#59313 = ORIENTED_EDGE ( 'NONE', *, *, #17123, .T. ) ;
#59314 = CARTESIAN_POINT ( 'NONE',  ( 24.90000000000000213, 13.66939075806899240, 20.79999999999999361 ) ) ;
#59316 = ORIENTED_EDGE ( 'NONE', *, *, #9285, .F. ) ;
#59315 = CYLINDRICAL_SURFACE ( 'NONE', #23933, 2.458500000000000796 ) ;
#59317 = ADVANCED_FACE ( 'NONE', ( #32624 ), #54195, .T. ) ;
#59318 = PLANE ( 'NONE',  #28853 ) ;
#59319 = AXIS2_PLACEMENT_3D ( 'NONE', #43264, #47532, #63800 ) ;
#59320 = CARTESIAN_POINT ( 'NONE',  ( 8.250000000000005329, -7.249999999999998224, -8.500000000000000000 ) ) ;
#59321 = ORIENTED_EDGE ( 'NONE', *, *, #15144, .F. ) ;
#59322 = VERTEX_POINT ( 'NONE', #447 ) ;
#59323 = VECTOR ( 'NONE', #12109, 1000.000000000000000 ) ;
#59324 = EDGE_CURVE ( 'NONE', #44995, #24136, #60170, .T. ) ;
#59325 = CARTESIAN_POINT ( 'NONE',  ( -3.834182069070823040, -7.357023737882818715, 54.00000000000000711 ) ) ;
#59326 = EDGE_CURVE ( 'NONE', #6900, #50683, #43568, .T. ) ;
#59327 = EDGE_CURVE ( 'NONE', #61785, #11023, #11386, .T. ) ;
#59328 = ORIENTED_EDGE ( 'NONE', *, *, #14227, .F. ) ;
#59329 = DIRECTION ( 'NONE',  ( 0.000000000000000000, -3.673940397442059868E-16, 1.000000000000000000 ) ) ;
#59330 = DIRECTION ( 'NONE',  ( 0.000000000000000000, 0.000000000000000000, -1.000000000000000000 ) ) ;
#59331 = ADVANCED_FACE ( 'NONE', ( #6095 ), #805, .F. ) ;
#59332 = EDGE_CURVE ( 'NONE', #2177, #64205, #23031, .T. ) ;
#59333 = VERTEX_POINT ( 'NONE', #12074 ) ;
#59334 = EDGE_CURVE ( 'NONE', #64531, #30734, #29035, .T. ) ;
#59335 = SURFACE_STYLE_FILL_AREA ( #67943 ) ;
#59336 = DIRECTION ( 'NONE',  ( -1.000000000000000000, 0.000000000000000000, 0.000000000000000000 ) ) ;
#59338 = ORIENTED_EDGE ( 'NONE', *, *, #42359, .F. ) ;
#59337 = DIRECTION ( 'NONE',  ( 0.000000000000000000, 0.000000000000000000, -1.000000000000000000 ) ) ;
#59339 = VERTEX_POINT ( 'NONE', #18776 ) ;
#59340 = CARTESIAN_POINT ( 'NONE',  ( -8.393516549646712122, 4.383466043307770121, 195.0000000000000284 ) ) ;
#59341 = DIRECTION ( 'NONE',  ( 0.000000000000000000, 1.000000000000000000, 0.000000000000000000 ) ) ;
#59342 = DIRECTION ( 'NONE',  ( 1.000000000000000000, -0.000000000000000000, -0.000000000000000000 ) ) ;
#59343 = CARTESIAN_POINT ( 'NONE',  ( -10.19191654964685689, -10.20488345035338362, 455.0000000000000568 ) ) ;
#59344 = CIRCLE ( 'NONE', #69545, 0.1749999999999998224 ) ;
#59345 = DIRECTION ( 'NONE',  ( -1.000000000000000000, 0.000000000000000000, 0.000000000000000000 ) ) ;
#59346 = EDGE_LOOP ( 'NONE', ( #13449, #41355, #68091, #12914 ) ) ;
#59347 = DIRECTION ( 'NONE',  ( -1.000000000000000000, 0.000000000000000000, 0.000000000000000000 ) ) ;
#59348 = DIRECTION ( 'NONE',  ( 0.7071067811865446862, -0.7071067811865503483, 0.000000000000000000 ) ) ;
#59349 = DIRECTION ( 'NONE',  ( -0.6414496315691617934, 0.7671651518152962090, 0.000000000000000000 ) ) ;
#59351 = ORIENTED_EDGE ( 'NONE', *, *, #43762, .T. ) ;
#59350 = DIRECTION ( 'NONE',  ( -0.000000000000000000, 3.673940397442059868E-16, -1.000000000000000000 ) ) ;
#59352 = VECTOR ( 'NONE', #41215, 1000.000000000000000 ) ;
#59353 = VECTOR ( 'NONE', #31457, 1000.000000000000000 ) ;
#59354 = CIRCLE ( 'NONE', #29962, 0.5000000000009302559 ) ;
#59355 = DIRECTION ( 'NONE',  ( 0.000000000000000000, 0.7071067811865470176, -0.7071067811865480168 ) ) ;
#59356 = CARTESIAN_POINT ( 'NONE',  ( -7.342976262117259623, 6.651770455163663165, 54.00000000000000711 ) ) ;
#59357 = CARTESIAN_POINT ( 'NONE',  ( -11.07551654964667520, 11.47551654964660450, 455.0000000000000568 ) ) ;
#59358 = AXIS2_PLACEMENT_3D ( 'NONE', #6329, #49469, #6664 ) ;
#59359 = CIRCLE ( 'NONE', #68397, 24.99999999998784972 ) ;
#59360 = DIRECTION ( 'NONE',  ( -1.000000000000000000, 0.000000000000000000, 0.000000000000000000 ) ) ;
#59361 = ORIENTED_EDGE ( 'NONE', *, *, #24613, .T. ) ;
#59362 = CARTESIAN_POINT ( 'NONE',  ( 11.50000000000000000, -11.50000000000000000, -11.00000000000000000 ) ) ;
#59363 = CARTESIAN_POINT ( 'NONE',  ( 41.09999999999999432, -21.00000000000000000, -14.57806571531351914 ) ) ;
#59364 = ORIENTED_EDGE ( 'NONE', *, *, #5072, .T. ) ;
#59365 = DIRECTION ( 'NONE',  ( 0.000000000000000000, 0.000000000000000000, 1.000000000000000000 ) ) ;
#59366 = CARTESIAN_POINT ( 'NONE',  ( 11.75000000000000000, -5.000000000000000000, 26.25000000000000000 ) ) ;
#59367 = VECTOR ( 'NONE', #7644, 1000.000000000000000 ) ;
#59368 = LINE ( 'NONE', #38162, #502 ) ;
#59369 = LINE ( 'NONE', #10930, #38411 ) ;
#59370 = FACE_OUTER_BOUND ( 'NONE', #59174, .T. ) ;
#59371 = EDGE_CURVE ( 'NONE', #69428, #56924, #49907, .T. ) ;
#59372 = VECTOR ( 'NONE', #47009, 1000.000000000000000 ) ;
#59373 = VERTEX_POINT ( 'NONE', #7107 ) ;
#59374 = EDGE_LOOP ( 'NONE', ( #12239, #19718, #65809, #60756 ) ) ;
#59375 = CARTESIAN_POINT ( 'NONE',  ( -7.250000000000000888, 7.450000000000003730, -8.500000000000000000 ) ) ;
#59376 = VERTEX_POINT ( 'NONE', #23386 ) ;
#59377 = ORIENTED_EDGE ( 'NONE', *, *, #57700, .T. ) ;
#59378 = EDGE_CURVE ( 'NONE', #47169, #35057, #9543, .T. ) ;
#59379 = DIRECTION ( 'NONE',  ( 0.000000000000000000, 1.000000000000000000, 0.000000000000000000 ) ) ;
#59380 = EDGE_CURVE ( 'NONE', #30577, #35602, #2508, .T. ) ;
#59381 = EDGE_CURVE ( 'NONE', #7253, #49868, #55906, .T. ) ;
#59382 = DIRECTION ( 'NONE',  ( -0.000000000000000000, 3.673940397442059868E-16, -1.000000000000000000 ) ) ;
#59383 = DIRECTION ( 'NONE',  ( 0.000000000000000000, -0.7071067811865475727, -0.7071067811865475727 ) ) ;
#59384 = VERTEX_POINT ( 'NONE', #24076 ) ;
#59385 = ORIENTED_EDGE ( 'NONE', *, *, #48744, .T. ) ;
#59386 = CARTESIAN_POINT ( 'NONE',  ( -10.91351654964670814, 9.093516549646603053, 455.0000000000000568 ) ) ;
#59387 = ORIENTED_EDGE ( 'NONE', *, *, #59986, .F. ) ;
#59388 = ORIENTED_EDGE ( 'NONE', *, *, #18664, .F. ) ;
#59389 = LINE ( 'NONE', #10952, #38355 ) ;
#59390 = DIRECTION ( 'NONE',  ( -0.000000000000000000, 0.000000000000000000, 1.000000000000000000 ) ) ;
#59391 = PLANE ( 'NONE',  #522 ) ;
#59392 = AXIS2_PLACEMENT_3D ( 'NONE', #26383, #26733, #52924 ) ;
#59393 = ORIENTED_EDGE ( 'NONE', *, *, #5654, .T. ) ;
#59394 = DIRECTION ( 'NONE',  ( 0.000000000000000000, 1.000000000000000000, 0.000000000000000000 ) ) ;
#59396 = FACE_OUTER_BOUND ( 'NONE', #37078, .T. ) ;
#59395 = CARTESIAN_POINT ( 'NONE',  ( 176.4833316329832940, -10.00000000000000178, 280.6301873289890523 ) ) ;
#59397 = ORIENTED_EDGE ( 'NONE', *, *, #57409, .T. ) ;
#59398 = VERTEX_POINT ( 'NONE', #60855 ) ;
#59400 = EDGE_LOOP ( 'NONE', ( #57543, #3687, #36423, #35549 ) ) ;
#59399 = DIRECTION ( 'NONE',  ( 0.000000000000000000, -3.673940397442059868E-16, 1.000000000000000000 ) ) ;
#59401 = VECTOR ( 'NONE', #34831, 1000.000000000000114 ) ;
#59402 = ORIENTED_EDGE ( 'NONE', *, *, #1372, .T. ) ;
#59403 = CIRCLE ( 'NONE', #4090, 24.99999999998784972 ) ;
#59404 = DIRECTION ( 'NONE',  ( 0.000000000000000000, 1.000000000000000000, 0.000000000000000000 ) ) ;
#59405 = CIRCLE ( 'NONE', #49215, 0.5999999999999989786 ) ;
#59406 = VECTOR ( 'NONE', #18628, 1000.000000000000000 ) ;
#59408 = FACE_OUTER_BOUND ( 'NONE', #10409, .T. ) ;
#59407 = VECTOR ( 'NONE', #56951, 1000.000000000000000 ) ;
#59409 = EDGE_LOOP ( 'NONE', ( #12329, #34915, #10923, #16970 ) ) ;
#59410 = VERTEX_POINT ( 'NONE', #66855 ) ;
#59411 = CIRCLE ( 'NONE', #26661, 0.2000000000000005107 ) ;
#59412 = VECTOR ( 'NONE', #34133, 1000.000000000000000 ) ;
#59413 = AXIS2_PLACEMENT_3D ( 'NONE', #40240, #45897, #45538 ) ;
#59414 = DIRECTION ( 'NONE',  ( 0.000000000000000000, 0.000000000000000000, -1.000000000000000000 ) ) ;
#59415 = DIRECTION ( 'NONE',  ( 1.000000000000000000, 0.000000000000000000, 0.000000000000000000 ) ) ;
#59416 = VERTEX_POINT ( 'NONE', #55222 ) ;
#59417 = EDGE_LOOP ( 'NONE', ( #58103, #46119, #26342, #20495 ) ) ;
#59418 = CARTESIAN_POINT ( 'NONE',  ( -11.00000000000000000, -14.04000000000000092, -14.80000000000000071 ) ) ;
#59420 = VECTOR ( 'NONE', #10109, 1000.000000000000000 ) ;
#59419 = DIRECTION ( 'NONE',  ( 1.000000000000000000, -5.120954910632640039E-15, 0.000000000000000000 ) ) ;
#59421 = DIRECTION ( 'NONE',  ( 0.000000000000000000, 0.000000000000000000, -1.000000000000000000 ) ) ;
#59422 = EDGE_CURVE ( 'NONE', #6870, #61285, #45632, .T. ) ;
#59423 = ORIENTED_EDGE ( 'NONE', *, *, #3047, .T. ) ;
#59424 = VECTOR ( 'NONE', #46107, 1000.000000000000000 ) ;
#59425 = EDGE_CURVE ( 'NONE', #63788, #48129, #6443, .T. ) ;
#59426 = DIRECTION ( 'NONE',  ( 0.000000000000000000, 0.000000000000000000, 1.000000000000000000 ) ) ;
#59427 = CYLINDRICAL_SURFACE ( 'NONE', #24913, 0.1999999999999996503 ) ;
#59429 = ORIENTED_EDGE ( 'NONE', *, *, #42795, .F. ) ;
#59428 = CARTESIAN_POINT ( 'NONE',  ( 10.14575131106465378, -20.50000000000000000, 17.00000000000000000 ) ) ;
#59431 = EDGE_LOOP ( 'NONE', ( #55793, #6635, #13423, #975, #5217, #13179, #19559, #36513, #24875, #35113, #17389, #23036, #4601, #10221, #43136, #36787, #10824 ) ) ;
#59430 = DIRECTION ( 'NONE',  ( -0.000000000000000000, -1.000000000000000000, 0.000000000000000000 ) ) ;
#59432 = CYLINDRICAL_SURFACE ( 'NONE', #38172, 3.500000000000114131 ) ;
#59433 = CARTESIAN_POINT ( 'NONE',  ( 8.250000000000005329, -7.249999999999998224, -18.50000000000000000 ) ) ;
#59434 = CARTESIAN_POINT ( 'NONE',  ( -15.50000000000000000, -2.500000000000000000, 23.94337567297399971 ) ) ;
#59435 = DIRECTION ( 'NONE',  ( -1.000000000000000000, 0.000000000000000000, 0.000000000000000000 ) ) ;
#59436 = LINE ( 'NONE', #42819, #2320 ) ;
#59437 = DIRECTION ( 'NONE',  ( 0.7671651518152939886, -0.6414496315691644579, -2.587583378555133721E-16 ) ) ;
#59438 = VERTEX_POINT ( 'NONE', #50251 ) ;
#59439 = DIRECTION ( 'NONE',  ( -0.000000000000000000, -1.000000000000000000, -0.000000000000000000 ) ) ;
#59440 = EDGE_CURVE ( 'NONE', #59443, #8072, #512, .T. ) ;
#59441 = VERTEX_POINT ( 'NONE', #1465 ) ;
#59443 = VERTEX_POINT ( 'NONE', #40344 ) ;
#59442 = DIRECTION ( 'NONE',  ( -1.000000000000000000, 0.000000000000000000, 0.000000000000000000 ) ) ;
#59444 = LINE ( 'NONE', #37535, #48194 ) ;
#59445 = AXIS2_PLACEMENT_3D ( 'NONE', #55258, #6802, #28375 ) ;
#59446 = DIRECTION ( 'NONE',  ( 8.480870326997715333E-15, -0.000000000000000000, -1.000000000000000000 ) ) ;
#59447 = CIRCLE ( 'NONE', #38005, 0.9999999999999991118 ) ;
#59448 = ORIENTED_EDGE ( 'NONE', *, *, #10705, .T. ) ;
#59449 = CARTESIAN_POINT ( 'NONE',  ( 7.250000000000005329, -8.249999999999998224, -25.50000000000000355 ) ) ;
#59450 = CARTESIAN_POINT ( 'NONE',  ( -30.00000000000000000, -13.79999999999979998, -17.30000000000000071 ) ) ;
#59451 = ORIENTED_EDGE ( 'NONE', *, *, #38865, .F. ) ;
#59452 = LINE ( 'NONE', #64419, #4097 ) ;
#59453 = FACE_OUTER_BOUND ( 'NONE', #59488, .T. ) ;
#59454 = VECTOR ( 'NONE', #58396, 1000.000000000000000 ) ;
#59455 = SURFACE_STYLE_USAGE ( .BOTH. , #32233 ) ;
#59456 = VECTOR ( 'NONE', #63178, 1000.000000000000000 ) ;
#59457 = AXIS2_PLACEMENT_3D ( 'NONE', #42834, #65112, #31547 ) ;
#59458 = AXIS2_PLACEMENT_3D ( 'NONE', #44172, #61841, #60785 ) ;
#59459 = ORIENTED_EDGE ( 'NONE', *, *, #23715, .T. ) ;
#59460 = CARTESIAN_POINT ( 'NONE',  ( 10.05377373788281581, 8.916576262117182239, 54.00000000000000711 ) ) ;
#59461 = ORIENTED_EDGE ( 'NONE', *, *, #58638, .T. ) ;
#59462 = ORIENTED_EDGE ( 'NONE', *, *, #30838, .T. ) ;
#59463 = CARTESIAN_POINT ( 'NONE',  ( 283.0000000000000568, -20.40000000000000213, 12.40000000000000213 ) ) ;
#59465 = DIRECTION ( 'NONE',  ( 0.000000000000000000, 0.000000000000000000, -1.000000000000000000 ) ) ;
#59464 = VECTOR ( 'NONE', #62279, 1000.000000000000000 ) ;
#59466 = VECTOR ( 'NONE', #58962, 1000.000000000000000 ) ;
#59467 = EDGE_CURVE ( 'NONE', #40165, #38683, #67111, .T. ) ;
#59468 = VECTOR ( 'NONE', #46269, 1000.000000000000000 ) ;
#59469 = PLANE ( 'NONE',  #45657 ) ;
#59470 = DIRECTION ( 'NONE',  ( -1.000000000000000000, 0.000000000000000000, 0.000000000000000000 ) ) ;
#59471 = EDGE_LOOP ( 'NONE', ( #30488, #12266, #38418, #51507 ) ) ;
#59472 = ORIENTED_EDGE ( 'NONE', *, *, #30524, .T. ) ;
#59474 = ORIENTED_EDGE ( 'NONE', *, *, #10236, .F. ) ;
#59473 = CARTESIAN_POINT ( 'NONE',  ( 13.00000000000000178, -17.35230188589299871, 15.35019951917099945 ) ) ;
#59475 = VERTEX_POINT ( 'NONE', #12406 ) ;
#59476 = CIRCLE ( 'NONE', #49340, 0.1749999999999998224 ) ;
#59477 = CARTESIAN_POINT ( 'NONE',  ( -6.350872789121377870, -6.836383711242978833, 54.00000000000000711 ) ) ;
#59478 = LINE ( 'NONE', #64784, #53531 ) ;
#59479 = DIRECTION ( 'NONE',  ( -1.000000000000000000, 0.000000000000000000, 0.000000000000000000 ) ) ;
#59480 = CARTESIAN_POINT ( 'NONE',  ( -9.791916549646867196, -11.08848345035335115, 455.0000000000000568 ) ) ;
#59481 = ADVANCED_FACE ( 'NONE', ( #61540 ), #49568, .F. ) ;
#59483 = CARTESIAN_POINT ( 'NONE',  ( 10.20488345035338185, -9.804883450353528929, 455.0000000000000568 ) ) ;
#59482 = CYLINDRICAL_SURFACE ( 'NONE', #45622, 0.1749999999999989342 ) ;
#59484 = EDGE_LOOP ( 'NONE', ( #6751, #56781, #4967, #47392 ) ) ;
#59486 = EDGE_LOOP ( 'NONE', ( #46660, #43751, #1747, #44499 ) ) ;
#59485 = CARTESIAN_POINT ( 'NONE',  ( -4.135079735113166954, 3.663616288757006512, 54.00000000000000711 ) ) ;
#59487 = ORIENTED_EDGE ( 'NONE', *, *, #13100, .T. ) ;
#59488 = EDGE_LOOP ( 'NONE', ( #3468, #31715, #17459, #55868 ) ) ;
#59489 = ADVANCED_FACE ( 'NONE', ( #18409 ), #56258, .F. ) ;
#59490 = CARTESIAN_POINT ( 'NONE',  ( 283.0000000000000568, -40.30000000000000426, 12.20000000000000107 ) ) ;
#59491 = DIRECTION ( 'NONE',  ( 0.000000000000000000, 1.000000000000000000, 0.000000000000000000 ) ) ;
#59492 = FACE_OUTER_BOUND ( 'NONE', #25688, .T. ) ;
#59493 = ORIENTED_EDGE ( 'NONE', *, *, #16075, .T. ) ;
#59494 = ORIENTED_EDGE ( 'NONE', *, *, #60505, .F. ) ;
#59495 = VECTOR ( 'NONE', #61147, 1000.000000000000000 ) ;
#59496 = ORIENTED_EDGE ( 'NONE', *, *, #60423, .F. ) ;
#59497 = DIRECTION ( 'NONE',  ( 0.000000000000000000, 3.673940397442059868E-16, -1.000000000000000000 ) ) ;
#59498 = CARTESIAN_POINT ( 'NONE',  ( -11.00000000000000000, -15.46862696659690073, -14.50000000000000000 ) ) ;
#59499 = VECTOR ( 'NONE', #67058, 1000.000000000000000 ) ;
#59500 = DIRECTION ( 'NONE',  ( -0.000000000000000000, 3.673940397442059868E-16, -1.000000000000000000 ) ) ;
#59501 = VERTEX_POINT ( 'NONE', #39631 ) ;
#59502 = ORIENTED_EDGE ( 'NONE', *, *, #14618, .F. ) ;
#59503 = AXIS2_PLACEMENT_3D ( 'NONE', #28884, #6970, #62105 ) ;
#59505 = CARTESIAN_POINT ( 'NONE',  ( 7.000000000000000000, -21.00000000000000000, 7.799999999999999822 ) ) ;
#59504 = AXIS2_PLACEMENT_3D ( 'NONE', #33913, #2786, #55157 ) ;
#59506 = CARTESIAN_POINT ( 'NONE',  ( 26.90000000000000213, -14.06939075806902117, -20.80000000000000426 ) ) ;
#59507 = ORIENTED_EDGE ( 'NONE', *, *, #69589, .T. ) ;
#59508 = EDGE_CURVE ( 'NONE', #27839, #52379, #22695, .T. ) ;
#59509 = CIRCLE ( 'NONE', #18808, 1.000000000000000000 ) ;
#59510 = AXIS2_PLACEMENT_3D ( 'NONE', #63943, #64629, #16192 ) ;
#59511 = EDGE_CURVE ( 'NONE', #32653, #29119, #50947, .T. ) ;
#59512 = LINE ( 'NONE', #11073, #68642 ) ;
#59513 = EDGE_CURVE ( 'NONE', #58466, #39629, #44250, .T. ) ;
#59515 = ORIENTED_EDGE ( 'NONE', *, *, #67959, .F. ) ;
#59514 = DIRECTION ( 'NONE',  ( -1.000000000000000000, 0.000000000000000000, 0.000000000000000000 ) ) ;
#59516 = ORIENTED_EDGE ( 'NONE', *, *, #2571, .T. ) ;
#59517 = DIRECTION ( 'NONE',  ( 1.000000000000000000, -3.491481338843133355E-15, -1.836970198721036590E-16 ) ) ;
#59518 = AXIS2_PLACEMENT_3D ( 'NONE', #62098, #1413, #8005 ) ;
#59519 = DIRECTION ( 'NONE',  ( -0.000000000000000000, -1.000000000000000000, -0.000000000000000000 ) ) ;
#59520 = VECTOR ( 'NONE', #66422, 1000.000000000000114 ) ;
#59521 = ADVANCED_FACE ( 'NONE', ( #41038 ), #56945, .F. ) ;
#59522 = CARTESIAN_POINT ( 'NONE',  ( 30.00000000000000000, -15.97213595500069871, -14.50000000000000000 ) ) ;
#59523 = DIRECTION ( 'NONE',  ( 0.000000000000000000, -1.000000000000000000, 0.000000000000000000 ) ) ;
#59524 = EDGE_CURVE ( 'NONE', #38554, #34859, #57306, .T. ) ;
#59525 = DIRECTION ( 'NONE',  ( 1.000000000000000000, -0.000000000000000000, -0.000000000000000000 ) ) ;
#59526 = VECTOR ( 'NONE', #38466, 1000.000000000000000 ) ;
#59527 = EDGE_CURVE ( 'NONE', #44836, #44460, #65994, .T. ) ;
#59528 = VERTEX_POINT ( 'NONE', #14166 ) ;
#59529 = CARTESIAN_POINT ( 'NONE',  ( 7.000000000000000000, -23.50007830495750127, 12.58007262201399890 ) ) ;
#59530 = ADVANCED_FACE ( 'NONE', ( #4286 ), #35735, .F. ) ;
#59531 = ORIENTED_EDGE ( 'NONE', *, *, #64048, .F. ) ;
#59532 = AXIS2_PLACEMENT_3D ( 'NONE', #59691, #27173, #32814 ) ;
#59533 = CARTESIAN_POINT ( 'NONE',  ( 30.00000000000000000, -17.35230188589299871, 15.35019951917099945 ) ) ;
#59534 = CARTESIAN_POINT ( 'NONE',  ( 49.00000000000000000, -21.00000000000000000, 13.86939075806900057 ) ) ;
#59535 = DIRECTION ( 'NONE',  ( -1.836970198721029934E-16, -1.836970198721010706E-16, 1.000000000000000000 ) ) ;
#59536 = CARTESIAN_POINT ( 'NONE',  ( 283.0000000000000568, -28.95000000000155183, 14.49999999999845990 ) ) ;
#59537 = CARTESIAN_POINT ( 'NONE',  ( -2.530476262117228092, 9.722976262117159152, 26.00000000000000711 ) ) ;
#59538 = ORIENTED_EDGE ( 'NONE', *, *, #11965, .F. ) ;
#59539 = DIRECTION ( 'NONE',  ( -1.000000000000000000, 0.000000000000000000, 0.000000000000000000 ) ) ;
#59540 = DIRECTION ( 'NONE',  ( -0.000000000000000000, -0.000000000000000000, 1.000000000000000000 ) ) ;
#59541 = ORIENTED_EDGE ( 'NONE', *, *, #12091, .F. ) ;
#59542 = DIRECTION ( 'NONE',  ( -1.000000000000000000, 0.000000000000000000, 0.000000000000000000 ) ) ;
#59543 = EDGE_CURVE ( 'NONE', #57065, #18717, #30788, .T. ) ;
#59544 = DIRECTION ( 'NONE',  ( -0.000000000000000000, -0.000000000000000000, -1.000000000000000000 ) ) ;
#59545 = AXIS2_PLACEMENT_3D ( 'NONE', #57956, #35317, #3175 ) ;
#59546 = ORIENTED_EDGE ( 'NONE', *, *, #26705, .F. ) ;
#59547 = DIRECTION ( 'NONE',  ( -0.000000000000000000, -0.000000000000000000, 1.000000000000000000 ) ) ;
#59548 = DIRECTION ( 'NONE',  ( -0.000000000000000000, -0.000000000000000000, -1.000000000000000000 ) ) ;
#59549 = ORIENTED_EDGE ( 'NONE', *, *, #1282, .T. ) ;
#59550 = DIRECTION ( 'NONE',  ( 1.000000000000000000, 0.000000000000000000, 0.000000000000000000 ) ) ;
#59551 = FACE_OUTER_BOUND ( 'NONE', #52819, .T. ) ;
#59552 = ADVANCED_FACE ( 'NONE', ( #46342 ), #36084, .T. ) ;
#59553 = VECTOR ( 'NONE', #21088, 1000.000000000000000 ) ;
#59554 = VECTOR ( 'NONE', #15428, 1000.000000000000000 ) ;
#59555 = CARTESIAN_POINT ( 'NONE',  ( 30.00000000000000000, -8.959999999999999076, 12.95475478405700009 ) ) ;
#59556 = DIRECTION ( 'NONE',  ( -0.000000000000000000, -0.000000000000000000, 1.000000000000000000 ) ) ;
#59557 = VERTEX_POINT ( 'NONE', #30440 ) ;
#59559 = ORIENTED_EDGE ( 'NONE', *, *, #42359, .T. ) ;
#59558 = PLANE ( 'NONE',  #13661 ) ;
#59560 = VECTOR ( 'NONE', #61961, 1000.000000000000000 ) ;
#59561 = AXIS2_PLACEMENT_3D ( 'NONE', #19232, #13225, #34422 ) ;
#59562 = CARTESIAN_POINT ( 'NONE',  ( -30.00000000000000000, -17.35230188589299871, 15.35019951917099945 ) ) ;
#59563 = CARTESIAN_POINT ( 'NONE',  ( 7.000000000000000000, -21.00000000000000000, 0.000000000000000000 ) ) ;
#59564 = CARTESIAN_POINT ( 'NONE',  ( -11.99351654964674729, -7.826483450353316051, 195.0000000000000284 ) ) ;
#59565 = EDGE_LOOP ( 'NONE', ( #12376, #15988, #36120, #38208 ) ) ;
#59566 = AXIS2_PLACEMENT_3D ( 'NONE', #55682, #39752, #16823 ) ;
#59567 = VECTOR ( 'NONE', #58364, 999.9999999999998863 ) ;
#59568 = DIRECTION ( 'NONE',  ( -1.610765207321970913E-14, -1.000000000000000000, -1.836970198721006761E-16 ) ) ;
#59569 = ORIENTED_EDGE ( 'NONE', *, *, #48646, .T. ) ;
#59570 = ORIENTED_EDGE ( 'NONE', *, *, #35073, .F. ) ;
#59571 = ORIENTED_EDGE ( 'NONE', *, *, #26051, .F. ) ;
#59572 = EDGE_CURVE ( 'NONE', #65336, #54250, #10698, .T. ) ;
#59573 = DIRECTION ( 'NONE',  ( 0.000000000000000000, 0.000000000000000000, -1.000000000000000000 ) ) ;
#59574 = DIRECTION ( 'NONE',  ( -1.570596175624152093E-15, 1.000000000000000000, 3.673940397442060361E-16 ) ) ;
#59575 = AXIS2_PLACEMENT_3D ( 'NONE', #20727, #52933, #62446 ) ;
#59576 = ORIENTED_EDGE ( 'NONE', *, *, #60777, .F. ) ;
#59578 = ADVANCED_FACE ( 'NONE', ( #19468 ), #24437, .F. ) ;
#59577 = ORIENTED_EDGE ( 'NONE', *, *, #62045, .F. ) ;
#59579 = ORIENTED_EDGE ( 'NONE', *, *, #46648, .F. ) ;
#59580 = EDGE_CURVE ( 'NONE', #26524, #33050, #24786, .T. ) ;
#59581 = CARTESIAN_POINT ( 'NONE',  ( 10.92648345035340895, 9.293516549646565039, 455.0000000000000568 ) ) ;
#59582 = VERTEX_POINT ( 'NONE', #62250 ) ;
#59583 = EDGE_CURVE ( 'NONE', #69650, #20506, #9224, .T. ) ;
#59584 = ORIENTED_EDGE ( 'NONE', *, *, #68525, .T. ) ;
#59585 = ADVANCED_FACE ( 'NONE', ( #68627 ), #19124, .F. ) ;
#59586 = EDGE_CURVE ( 'NONE', #69253, #53260, #52363, .T. ) ;
#59587 = VERTEX_POINT ( 'NONE', #52012 ) ;
#59588 = ORIENTED_EDGE ( 'NONE', *, *, #24599, .T. ) ;
#59589 = CARTESIAN_POINT ( 'NONE',  ( -7.250000000000000888, 7.450000000000003730, -16.50000000000000000 ) ) ;
#59591 = VERTEX_POINT ( 'NONE', #68266 ) ;
#59590 = DIRECTION ( 'NONE',  ( -0.7071067811865460184, -0.7071067811865489050, 0.000000000000000000 ) ) ;
#59592 = EDGE_CURVE ( 'NONE', #26669, #63858, #19815, .T. ) ;
#59593 = FACE_OUTER_BOUND ( 'NONE', #21603, .T. ) ;
#59594 = LINE ( 'NONE', #11144, #56589 ) ;
#59595 = ADVANCED_FACE ( 'NONE', ( #41738 ), #63316, .F. ) ;
#59596 = LINE ( 'NONE', #22798, #47146 ) ;
#59597 = VERTEX_POINT ( 'NONE', #58007 ) ;
#59598 = EDGE_CURVE ( 'NONE', #52379, #20859, #9575, .T. ) ;
#59599 = CARTESIAN_POINT ( 'NONE',  ( -29.50000000000000355, -15.97213595500069871, 14.50000000000000000 ) ) ;
#59600 = AXIS2_PLACEMENT_3D ( 'NONE', #60708, #12252, #54378 ) ;
#59601 = ADVANCED_FACE ( 'NONE', ( #37498 ), #15231, .F. ) ;
#59602 = ORIENTED_EDGE ( 'NONE', *, *, #4592, .T. ) ;
#59603 = FACE_BOUND ( 'NONE', #5776, .T. ) ;
#59604 = EDGE_CURVE ( 'NONE', #67686, #25494, #32185, .T. ) ;
#59605 = AXIS2_PLACEMENT_3D ( 'NONE', #24046, #61517, #39945 ) ;
#59606 = AXIS2_PLACEMENT_3D ( 'NONE', #12095, #37948, #826 ) ;
#59607 = DIRECTION ( 'NONE',  ( 0.000000000000000000, 0.000000000000000000, 1.000000000000000000 ) ) ;
#59608 = DIRECTION ( 'NONE',  ( 0.000000000000000000, -1.000000000000000000, 0.000000000000000000 ) ) ;
#59609 = VECTOR ( 'NONE', #27592, 1000.000000000000000 ) ;
#59610 = ORIENTED_EDGE ( 'NONE', *, *, #29542, .F. ) ;
#59611 = CARTESIAN_POINT ( 'NONE',  ( -8.130476262117319664, -9.562023737882764607, 26.00000000000000000 ) ) ;
#59612 = VECTOR ( 'NONE', #59870, 1000.000000000000000 ) ;
#59613 = CIRCLE ( 'NONE', #41537, 1.000000000000000000 ) ;
#59614 = DIRECTION ( 'NONE',  ( -0.000000000000000000, -0.000000000000000000, -1.000000000000000000 ) ) ;
#59615 = CARTESIAN_POINT ( 'NONE',  ( 8.241237374594303944, -1.634292677759887846, 54.00000000000000711 ) ) ;
#59616 = EDGE_CURVE ( 'NONE', #12839, #39380, #69318, .T. ) ;
#59617 = DIRECTION ( 'NONE',  ( 1.000000000000000000, -0.000000000000000000, 0.000000000000000000 ) ) ;
#59618 = DIRECTION ( 'NONE',  ( -0.000000000000000000, -0.000000000000000000, -1.000000000000000000 ) ) ;
#59619 = DIRECTION ( 'NONE',  ( 0.000000000000000000, 0.7096009616570518874, 0.7046037717862339012 ) ) ;
#59620 = PLANE ( 'NONE',  #27675 ) ;
#59621 = PLANE ( 'NONE',  #17594 ) ;
#59622 = VECTOR ( 'NONE', #53619, 1000.000000000000000 ) ;
#59623 = ORIENTED_EDGE ( 'NONE', *, *, #12990, .T. ) ;
#59624 = DIRECTION ( 'NONE',  ( 0.000000000000000000, 0.000000000000000000, -1.000000000000000000 ) ) ;
#59625 = DIRECTION ( 'NONE',  ( 1.000000000000000000, 0.000000000000000000, 0.000000000000000000 ) ) ;
#59626 = PLANE ( 'NONE',  #42547 ) ;
#59627 = DIRECTION ( 'NONE',  ( 0.000000000000000000, 0.000000000000000000, 1.000000000000000000 ) ) ;
#59628 = VERTEX_POINT ( 'NONE', #10613 ) ;
#59629 = FACE_OUTER_BOUND ( 'NONE', #66194, .T. ) ;
#59630 = CARTESIAN_POINT ( 'NONE',  ( 26.90000000000000213, 20.60000000000000142, -13.86939075806900057 ) ) ;
#59631 = CARTESIAN_POINT ( 'NONE',  ( 10.74648345035335240, 1.677516549646529409, 455.0000000000000568 ) ) ;
#59632 = ADVANCED_FACE ( 'NONE', ( #21240 ), #5335, .T. ) ;
#59633 = CARTESIAN_POINT ( 'NONE',  ( 7.000000000000000000, -26.50000000000000000, -5.809475019311129529 ) ) ;
#59634 = CARTESIAN_POINT ( 'NONE',  ( 7.250000000000005329, -7.449999999999998401, -19.50000000000000000 ) ) ;
#59635 = PLANE ( 'NONE',  #50853 ) ;
#59636 = VERTEX_POINT ( 'NONE', #58717 ) ;
#59637 = EDGE_CURVE ( 'NONE', #52963, #58636, #37843, .T. ) ;
#59638 = ORIENTED_EDGE ( 'NONE', *, *, #21431, .F. ) ;
#59639 = CARTESIAN_POINT ( 'NONE',  ( 1.634292677759859869, -8.241237374594282628, 54.00000000000000711 ) ) ;
#59640 = CARTESIAN_POINT ( 'NONE',  ( 32.89999999999999858, 0.000000000000000000, 2.458500000000000796 ) ) ;
#59641 = PRESENTATION_LAYER_ASSIGNMENT (  '', '', ( #65304 ) ) ;
#59642 = ORIENTED_EDGE ( 'NONE', *, *, #47846, .T. ) ;
#59643 = ADVANCED_FACE ( 'NONE', ( #53414 ), #6007, .F. ) ;
#59644 = CARTESIAN_POINT ( 'NONE',  ( 0.000000000000000000, 0.000000000000000000, -9.000000000000001776 ) ) ;
#59645 = EDGE_CURVE ( 'NONE', #36435, #32668, #69681, .T. ) ;
#59646 = EDGE_LOOP ( 'NONE', ( #67106, #44346, #62411, #10342 ) ) ;
#59647 = CARTESIAN_POINT ( 'NONE',  ( 6.501044194225490180, -3.157023737882814540, 26.00000000000000711 ) ) ;
#59648 = ORIENTED_EDGE ( 'NONE', *, *, #26527, .T. ) ;
#59649 = ADVANCED_FACE ( 'NONE', ( #16 ), #31502, .T. ) ;
#59650 = ORIENTED_EDGE ( 'NONE', *, *, #13033, .F. ) ;
#59651 = DIRECTION ( 'NONE',  ( -1.000000000000000000, 0.000000000000000000, 0.000000000000000000 ) ) ;
#59652 = ORIENTED_EDGE ( 'NONE', *, *, #69179, .F. ) ;
#59653 = CARTESIAN_POINT ( 'NONE',  ( 283.0000000000000568, -26.42999999999999972, -9.412893218813501051 ) ) ;
#59654 = VECTOR ( 'NONE', #24673, 1000.000000000000000 ) ;
#59655 = CYLINDRICAL_SURFACE ( 'NONE', #36118, 0.7500000000000006661 ) ;
#59656 = LINE ( 'NONE', #12573, #25705 ) ;
#59657 = ORIENTED_EDGE ( 'NONE', *, *, #21079, .T. ) ;
#59658 = VERTEX_POINT ( 'NONE', #31849 ) ;
#59659 = CARTESIAN_POINT ( 'NONE',  ( 35.89999999999999858, 13.66939075806899240, 20.79999999999999361 ) ) ;
#59660 = EDGE_CURVE ( 'NONE', #25985, #65968, #11835, .T. ) ;
#59661 = AXIS2_PLACEMENT_3D ( 'NONE', #18685, #8419, #29998 ) ;
#59663 = CARTESIAN_POINT ( 'NONE',  ( -11.50000000000000000, -11.70000000000000284, -11.00000000000000000 ) ) ;
#59662 = CARTESIAN_POINT ( 'NONE',  ( 9.703773737882785966, -8.580623737882856261, 54.00000000000000711 ) ) ;
#59664 = VERTEX_POINT ( 'NONE', #42788 ) ;
#59665 = ORIENTED_EDGE ( 'NONE', *, *, #17982, .T. ) ;
#59666 = EDGE_CURVE ( 'NONE', #21706, #22191, #712, .T. ) ;
#59667 = EDGE_CURVE ( 'NONE', #34851, #64638, #46820, .T. ) ;
#59668 = ORIENTED_EDGE ( 'NONE', *, *, #32909, .T. ) ;
#59669 = DIRECTION ( 'NONE',  ( -1.000000000000000000, 0.000000000000000000, 0.000000000000000000 ) ) ;
#59671 = VERTEX_POINT ( 'NONE', #47744 ) ;
#59670 = DIRECTION ( 'NONE',  ( 1.000000000000000000, -0.000000000000000000, 0.000000000000000000 ) ) ;
#59672 = EDGE_CURVE ( 'NONE', #14096, #65971, #32547, .T. ) ;
#59673 = DIRECTION ( 'NONE',  ( 0.000000000000000000, 3.673940397442059868E-16, -1.000000000000000000 ) ) ;
#59674 = CARTESIAN_POINT ( 'NONE',  ( 9.703773737882785966, -9.703773737882823269, 54.00000000000000711 ) ) ;
#59675 = ORIENTED_EDGE ( 'NONE', *, *, #49354, .F. ) ;
#59676 = ORIENTED_EDGE ( 'NONE', *, *, #2989, .T. ) ;
#59677 = FACE_OUTER_BOUND ( 'NONE', #17976, .T. ) ;
#59678 = VERTEX_POINT ( 'NONE', #48800 ) ;
#59679 = CYLINDRICAL_SURFACE ( 'NONE', #35868, 3.499999999999999556 ) ;
#59680 = CYLINDRICAL_SURFACE ( 'NONE', #40320, 0.5000000000009320322 ) ;
#59681 = ADVANCED_FACE ( 'NONE', ( #22282, #43832 ), #357, .F. ) ;
#59682 = ORIENTED_EDGE ( 'NONE', *, *, #64688, .T. ) ;
#59683 = EDGE_CURVE ( 'NONE', #3920, #50336, #15593, .T. ) ;
#59684 = CARTESIAN_POINT ( 'NONE',  ( 0.000000000000000000, 5.000000000000000000, 0.000000000000000000 ) ) ;
#59685 = CARTESIAN_POINT ( 'NONE',  ( -2.693516549646827851, -10.92648345035345692, 455.0000000000000568 ) ) ;
#59687 = ORIENTED_EDGE ( 'NONE', *, *, #24037, .T. ) ;
#59686 = FACE_OUTER_BOUND ( 'NONE', #44507, .T. ) ;
#59688 = VERTEX_POINT ( 'NONE', #59750 ) ;
#59689 = LINE ( 'NONE', #55426, #62206 ) ;
#59690 = CARTESIAN_POINT ( 'NONE',  ( -9.828310488886039309, -1.690483450353358119, 455.0000000000000568 ) ) ;
#59691 = CARTESIAN_POINT ( 'NONE',  ( -15.50000000000000000, -5.000000000000000000, -22.50000000000000000 ) ) ;
#59692 = LINE ( 'NONE', #32815, #54324 ) ;
#59693 = AXIS2_PLACEMENT_3D ( 'NONE', #53317, #15484, #4868 ) ;
#59694 = FACE_OUTER_BOUND ( 'NONE', #61981, .T. ) ;
#59695 = ORIENTED_EDGE ( 'NONE', *, *, #9495, .F. ) ;
#59696 = DIRECTION ( 'NONE',  ( 1.000000000000000000, 0.000000000000000000, -0.000000000000000000 ) ) ;
#59697 = DIRECTION ( 'NONE',  ( 0.000000000000000000, 3.673940397442059868E-16, -1.000000000000000000 ) ) ;
#59698 = AXIS2_PLACEMENT_3D ( 'NONE', #54000, #32076, #48339 ) ;
#59700 = ORIENTED_EDGE ( 'NONE', *, *, #38049, .T. ) ;
#59699 = DIRECTION ( 'NONE',  ( -8.612436249475772606E-15, -1.000000000000000000, -1.836970198721020566E-16 ) ) ;
#59701 =( NAMED_UNIT ( * ) PLANE_ANGLE_UNIT ( ) SI_UNIT ( $, .RADIAN. ) );
#59702 = CARTESIAN_POINT ( 'NONE',  ( 1.634292677759859869, -8.241237374594271969, 26.00000000000000000 ) ) ;
#59703 = LINE ( 'NONE', #23249, #42048 ) ;
#59704 = AXIS2_PLACEMENT_3D ( 'NONE', #57772, #52847, #8273 ) ;
#59705 = CARTESIAN_POINT ( 'NONE',  ( 12.00648345035338060, -7.826483450353395988, 195.0000000000000284 ) ) ;
#59706 = EDGE_LOOP ( 'NONE', ( #39042, #45850, #56540, #37011 ) ) ;
#59707 = CARTESIAN_POINT ( 'NONE',  ( -11.11351654964671631, -2.906483450353335218, 455.0000000000000568 ) ) ;
#59708 = CARTESIAN_POINT ( 'NONE',  ( 8.250000000000005329, 7.250000000000000888, -24.50000000000000000 ) ) ;
#59709 = ORIENTED_EDGE ( 'NONE', *, *, #20057, .F. ) ;
#59710 = CARTESIAN_POINT ( 'NONE',  ( -2.752095193409374030, 9.942044687070435316, 455.0000000000000568 ) ) ;
#59711 = DIRECTION ( 'NONE',  ( 1.836970198721029934E-16, -1.836970198721036344E-16, 1.000000000000000000 ) ) ;
#59712 = CARTESIAN_POINT ( 'NONE',  ( 46.39999999999999858, 33.00000000000000000, 2.250000000000000444 ) ) ;
#59713 = FACE_OUTER_BOUND ( 'NONE', #31414, .T. ) ;
#59714 = VECTOR ( 'NONE', #29421, 1000.000000000000000 ) ;
#59715 = EDGE_CURVE ( 'NONE', #68411, #61023, #32200, .T. ) ;
#59716 = LINE ( 'NONE', #5973, #61349 ) ;
#59717 = EDGE_LOOP ( 'NONE', ( #11886, #4264, #5995, #59448 ) ) ;
#59718 = ORIENTED_EDGE ( 'NONE', *, *, #34956, .T. ) ;
#59719 = CARTESIAN_POINT ( 'NONE',  ( -7.250000000000000888, 7.250000000000001776, -18.50000000000000000 ) ) ;
#59720 = ORIENTED_EDGE ( 'NONE', *, *, #55745, .T. ) ;
#59721 = CARTESIAN_POINT ( 'NONE',  ( 2.369523737882793135, -8.835729544836320670, 54.00000000000000711 ) ) ;
#59722 = ORIENTED_EDGE ( 'NONE', *, *, #53456, .T. ) ;
#59723 = EDGE_CURVE ( 'NONE', #57577, #4484, #3939, .T. ) ;
#59724 = CARTESIAN_POINT ( 'NONE',  ( 37.90000000000000568, -14.06939075806900874, 20.80000000000001137 ) ) ;
#59725 = ADVANCED_FACE ( 'NONE', ( #17644 ), #11978, .F. ) ;
#59726 = EDGE_CURVE ( 'NONE', #49724, #3924, #23987, .T. ) ;
#59727 = DIRECTION ( 'NONE',  ( -1.000000000000000000, 0.000000000000000000, 0.000000000000000000 ) ) ;
#59728 = CARTESIAN_POINT ( 'NONE',  ( 48.50000000000000000, 0.000000000000000000, 0.000000000000000000 ) ) ;
#59729 = ORIENTED_EDGE ( 'NONE', *, *, #66103, .T. ) ;
#59730 = ADVANCED_FACE ( 'NONE', ( #7719 ), #12319, .F. ) ;
#59731 = VERTEX_POINT ( 'NONE', #7369 ) ;
#59732 = EDGE_CURVE ( 'NONE', #8035, #63019, #39547, .T. ) ;
#59733 = FACE_OUTER_BOUND ( 'NONE', #51975, .T. ) ;
#59734 = ORIENTED_EDGE ( 'NONE', *, *, #12454, .F. ) ;
#59735 = ORIENTED_EDGE ( 'NONE', *, *, #4505, .F. ) ;
#59736 = CARTESIAN_POINT ( 'NONE',  ( 0.000000000000000000, 0.000000000000000000, -5.000000000000000000 ) ) ;
#59737 = DIRECTION ( 'NONE',  ( -0.000000000000000000, -0.000000000000000000, -1.000000000000000000 ) ) ;
#59738 = DIRECTION ( 'NONE',  ( 9.912705577010336396E-15, 1.000000000000000000, 0.000000000000000000 ) ) ;
#59739 = ADVANCED_FACE ( 'NONE', ( #60424 ), #1388, .T. ) ;
#59740 = ORIENTED_EDGE ( 'NONE', *, *, #55289, .T. ) ;
#59741 = DIRECTION ( 'NONE',  ( -1.000000000000000000, 0.000000000000000000, 0.000000000000000000 ) ) ;
#59743 = CARTESIAN_POINT ( 'NONE',  ( -11.00000000000000000, -5.599999999999379696, -27.00000000000000000 ) ) ;
#59742 = CARTESIAN_POINT ( 'NONE',  ( -8.250000000000001776, 0.000000000000000000, -9.500000000000001776 ) ) ;
#59744 = EDGE_LOOP ( 'NONE', ( #3290, #25443, #35091, #15708 ) ) ;
#59745 = VERTEX_POINT ( 'NONE', #38534 ) ;
#59747 = ORIENTED_EDGE ( 'NONE', *, *, #57874, .T. ) ;
#59746 = DIRECTION ( 'NONE',  ( 0.000000000000000000, 3.989863994748342081E-13, 1.000000000000000000 ) ) ;
#59748 = EDGE_LOOP ( 'NONE', ( #39602, #41015, #64979, #47149, #64084, #14057, #3442, #26610 ) ) ;
#59749 = VECTOR ( 'NONE', #54621, 1000.000000000000000 ) ;
#59750 = CARTESIAN_POINT ( 'NONE',  ( 0.4999999999999940603, -0.5000000000000000000, 27.00000000000000000 ) ) ;
#59751 = CIRCLE ( 'NONE', #14570, 1.929199999999997139 ) ;
#59752 = CARTESIAN_POINT ( 'NONE',  ( 25.50000000000000355, 0.000000000000000000, 20.24999999999999645 ) ) ;
#59753 = VERTEX_POINT ( 'NONE', #33221 ) ;
#59754 = ORIENTED_EDGE ( 'NONE', *, *, #24209, .F. ) ;
#59755 = VECTOR ( 'NONE', #67605, 1000.000000000000000 ) ;
#59756 = FACE_OUTER_BOUND ( 'NONE', #69828, .T. ) ;
#59757 = CARTESIAN_POINT ( 'NONE',  ( -23.48000000000000043, -17.50000000000000000, -26.00000000000000355 ) ) ;
#59758 = ORIENTED_EDGE ( 'NONE', *, *, #8083, .F. ) ;
#59759 = AXIS2_PLACEMENT_3D ( 'NONE', #10805, #4815, #21767 ) ;
#59760 = CARTESIAN_POINT ( 'NONE',  ( 8.250000000000005329, 7.250000000000000888, -26.00000000000001066 ) ) ;
#59761 = CARTESIAN_POINT ( 'NONE',  ( -10.91351654964675610, -9.106483450353326958, 195.0000000000000284 ) ) ;
#59762 = DIRECTION ( 'NONE',  ( -1.000000000000000000, 0.000000000000000000, -0.000000000000000000 ) ) ;
#59763 = VERTEX_POINT ( 'NONE', #55143 ) ;
#59765 = VECTOR ( 'NONE', #63782, 1000.000000000000000 ) ;
#59764 = VECTOR ( 'NONE', #66389, 1000.000000000000000 ) ;
#59766 = EDGE_CURVE ( 'NONE', #55314, #69042, #61494, .T. ) ;
#59767 = CARTESIAN_POINT ( 'NONE',  ( 17.24945551514599984, -15.50000000000000000, 25.53140320652400064 ) ) ;
#59768 = CARTESIAN_POINT ( 'NONE',  ( -11.47551654964667733, 11.07551654964660237, 455.0000000000000568 ) ) ;
#59771 = VERTEX_POINT ( 'NONE', #65410 ) ;
#59770 = EDGE_CURVE ( 'NONE', #22560, #16097, #28595, .T. ) ;
#59769 = LINE ( 'NONE', #27256, #58900 ) ;
#59773 = EDGE_LOOP ( 'NONE', ( #39537, #47222, #58248, #68156, #14089, #23531, #19452, #66185, #12733, #68164, #67298, #22453, #1524, #30409, #7005, #63226, #38358 ) ) ;
#59772 = CARTESIAN_POINT ( 'NONE',  ( -11.07551654964667520, 9.791916549646639822, 455.0000000000000568 ) ) ;
#59774 = DIRECTION ( 'NONE',  ( -1.000000000000000000, 0.000000000000000000, 0.000000000000000000 ) ) ;
#59775 = AXIS2_PLACEMENT_3D ( 'NONE', #49174, #1415, #54828 ) ;
#59776 = CARTESIAN_POINT ( 'NONE',  ( 7.450000000000003730, -7.249999999999997335, -21.50000000000000000 ) ) ;
#59777 = CARTESIAN_POINT ( 'NONE',  ( -30.00000000000000000, -11.50000000000100009, -15.00000000000084910 ) ) ;
#59778 = DIRECTION ( 'NONE',  ( -1.000000000000000000, 0.000000000000000000, 0.000000000000000000 ) ) ;
#59779 = EDGE_CURVE ( 'NONE', #11292, #18694, #54794, .T. ) ;
#59780 = EDGE_CURVE ( 'NONE', #24071, #34366, #16352, .T. ) ;
#59781 = DIRECTION ( 'NONE',  ( 1.000000000000000000, -1.334402673828313093E-16, 0.000000000000000000 ) ) ;
#59782 = FACE_OUTER_BOUND ( 'NONE', #13208, .T. ) ;
#59783 = ORIENTED_EDGE ( 'NONE', *, *, #24177, .F. ) ;
#59784 = LINE ( 'NONE', #44537, #15749 ) ;
#59786 = ORIENTED_EDGE ( 'NONE', *, *, #67006, .T. ) ;
#59785 = CARTESIAN_POINT ( 'NONE',  ( 8.406483450353379183, -6.344579767990839336, 195.0000000000000284 ) ) ;
#59788 = ORIENTED_EDGE ( 'NONE', *, *, #64757, .T. ) ;
#59787 = LINE ( 'NONE', #31884, #29911 ) ;
#59789 = VECTOR ( 'NONE', #53415, 1000.000000000000000 ) ;
#59790 = DIRECTION ( 'NONE',  ( 0.000000000000000000, 0.000000000000000000, -1.000000000000000000 ) ) ;
#59791 = ORIENTED_EDGE ( 'NONE', *, *, #44184, .F. ) ;
#59792 = CARTESIAN_POINT ( 'NONE',  ( 87.07321854994620480, 47.95351654967443977, 40.00000000000000000 ) ) ;
#59793 = CARTESIAN_POINT ( 'NONE',  ( 34.89999999999999858, 0.000000000000000000, 0.000000000000000000 ) ) ;
#59794 = EDGE_LOOP ( 'NONE', ( #20120, #14475, #23122, #2362, #38649, #44685, #45387, #56942, #53643, #45578, #36673, #14945, #37672, #39005, #1986, #21644, #65885, #6294, #31124, #6851 ) ) ;
#59795 = PLANE ( 'NONE',  #714 ) ;
#59796 = PLANE ( 'NONE',  #30412 ) ;
#59797 = CARTESIAN_POINT ( 'NONE',  ( -9.781776262117249487, 10.49297626211718359, 54.00000000000000711 ) ) ;
#59798 = DIRECTION ( 'NONE',  ( 0.000000000000000000, -0.9938079899998859545, 0.1111111111112941946 ) ) ;
#59799 = VECTOR ( 'NONE', #45794, 1000.000000000000000 ) ;
#59800 = AXIS2_PLACEMENT_3D ( 'NONE', #58363, #37481, #59043 ) ;
#59801 = EDGE_CURVE ( 'NONE', #35057, #20416, #11633, .T. ) ;
#59802 = VERTEX_POINT ( 'NONE', #55485 ) ;
#59803 = DIRECTION ( 'NONE',  ( 1.000000000000000000, 0.000000000000000000, 0.000000000000000000 ) ) ;
#59804 = ORIENTED_EDGE ( 'NONE', *, *, #63654, .F. ) ;
#59805 = ORIENTED_EDGE ( 'NONE', *, *, #35478, .T. ) ;
#59806 = AXIS2_PLACEMENT_3D ( 'NONE', #8449, #50890, #8100 ) ;
#59807 = LINE ( 'NONE', #1111, #68641 ) ;
#59808 = CARTESIAN_POINT ( 'NONE',  ( 0.000000000000000000, 8.250000000000001776, -17.00000000000000000 ) ) ;
#59809 = AXIS2_PLACEMENT_3D ( 'NONE', #64333, #54076, #21206 ) ;
#59810 = DIRECTION ( 'NONE',  ( 0.000000000000000000, 1.000000000000000000, 0.000000000000000000 ) ) ;
#59811 = CARTESIAN_POINT ( 'NONE',  ( -8.250000000000001776, 0.000000000000000000, -21.00000000000000000 ) ) ;
#59812 = ORIENTED_EDGE ( 'NONE', *, *, #32391, .T. ) ;
#59813 = EDGE_CURVE ( 'NONE', #48587, #13221, #7026, .T. ) ;
#59814 = ORIENTED_EDGE ( 'NONE', *, *, #33339, .F. ) ;
#59815 = ADVANCED_FACE ( 'NONE', ( #23296 ), #44857, .T. ) ;
#59817 = ORIENTED_EDGE ( 'NONE', *, *, #17034, .F. ) ;
#59816 = LINE ( 'NONE', #59473, #64519 ) ;
#59818 = EDGE_LOOP ( 'NONE', ( #11726, #56152, #14052, #7350 ) ) ;
#59819 = CIRCLE ( 'NONE', #63191, 24.99999999998784972 ) ;
#59820 = PLANE ( 'NONE',  #38310 ) ;
#59821 = DIRECTION ( 'NONE',  ( 0.000000000000000000, 0.000000000000000000, 1.000000000000000000 ) ) ;
#59822 = ADVANCED_FACE ( 'NONE', ( #49491 ), #12665, .T. ) ;
#59823 = LINE ( 'NONE', #11376, #29708 ) ;
#59824 = PRESENTATION_STYLE_ASSIGNMENT (( #11712 ) ) ;
#59825 = VECTOR ( 'NONE', #23115, 1000.000000000000000 ) ;
#59827 = FACE_OUTER_BOUND ( 'NONE', #45988, .T. ) ;
#59826 = CARTESIAN_POINT ( 'NONE',  ( 9.804883450353456098, 11.07551654964653132, 455.0000000000000568 ) ) ;
#59828 = VERTEX_POINT ( 'NONE', #2079 ) ;
#59830 = VERTEX_POINT ( 'NONE', #23635 ) ;
#59829 = DIRECTION ( 'NONE',  ( -0.000000000000000000, -0.000000000000000000, -1.000000000000000000 ) ) ;
#59831 = ORIENTED_EDGE ( 'NONE', *, *, #11252, .F. ) ;
#59832 = ORIENTED_EDGE ( 'NONE', *, *, #5901, .T. ) ;
#59833 = DIRECTION ( 'NONE',  ( 0.000000000000000000, 0.000000000000000000, 1.000000000000000000 ) ) ;
#59834 = CARTESIAN_POINT ( 'NONE',  ( -6.350872789121327244, 3.663616288756986084, 26.00000000000000711 ) ) ;
#59835 = DIRECTION ( 'NONE',  ( -3.016910393003147986E-15, 1.000000000000000000, 3.673940397442060361E-16 ) ) ;
#59836 = VECTOR ( 'NONE', #29557, 1000.000000000000000 ) ;
#59837 = ORIENTED_EDGE ( 'NONE', *, *, #64493, .T. ) ;
#59838 = EDGE_LOOP ( 'NONE', ( #38028, #62480, #13476, #36876 ) ) ;
#59839 = CARTESIAN_POINT ( 'NONE',  ( -29.50000000000000355, -11.50000000000100009, 15.00000000000084910 ) ) ;
#59840 = CARTESIAN_POINT ( 'NONE',  ( 283.0000000000000568, -42.50000000000000000, 14.50000000000000000 ) ) ;
#59841 = LINE ( 'NONE', #11398, #23246 ) ;
#59842 = ORIENTED_EDGE ( 'NONE', *, *, #4902, .F. ) ;
#59843 = ORIENTED_EDGE ( 'NONE', *, *, #16546, .T. ) ;
#59844 = DIRECTION ( 'NONE',  ( 1.000000000000000000, -0.000000000000000000, -0.000000000000000000 ) ) ;
#59845 =( REPRESENTATION_RELATIONSHIP ('NONE','NONE', #33057, #35 ) REPRESENTATION_RELATIONSHIP_WITH_TRANSFORMATION ( #38110 )SHAPE_REPRESENTATION_RELATIONSHIP( ) );
#59846 = CARTESIAN_POINT ( 'NONE',  ( 11.00000000000000000, -17.50000000000000000, 60.00000000000000000 ) ) ;
#59847 = EDGE_LOOP ( 'NONE', ( #53978, #35990, #53468, #33292 ) ) ;
#59848 = AXIS2_PLACEMENT_3D ( 'NONE', #34194, #66729, #49454 ) ;
#59849 = LINE ( 'NONE', #64819, #21209 ) ;
#59852 = VERTEX_POINT ( 'NONE', #46600 ) ;
#59851 = ADVANCED_FACE ( 'NONE', ( #45200 ), #66770, .T. ) ;
#59850 = DIRECTION ( 'NONE',  ( -1.000000000000000000, 0.000000000000000000, 0.000000000000000000 ) ) ;
#59853 = ORIENTED_EDGE ( 'NONE', *, *, #24610, .T. ) ;
#59854 = AXIS2_PLACEMENT_3D ( 'NONE', #17241, #38813, #60369 ) ;
#59855 = EDGE_CURVE ( 'NONE', #23669, #33316, #3826, .T. ) ;
#59856 = EDGE_CURVE ( 'NONE', #32498, #52692, #18601, .T. ) ;
#59857 = DIRECTION ( 'NONE',  ( -1.000000000000000000, 0.000000000000000000, 0.000000000000000000 ) ) ;
#59858 = CARTESIAN_POINT ( 'NONE',  ( -4.947141984184539432, -7.357023737882807168, 54.00000000000000711 ) ) ;
#59859 = DIRECTION ( 'NONE',  ( -0.7071067811865530128, -0.7071067811865421326, 0.000000000000000000 ) ) ;
#59860 = CARTESIAN_POINT ( 'NONE',  ( 8.250000000000005329, 8.250000000000001776, -26.00000000000001066 ) ) ;
#59861 = ADVANCED_FACE ( 'NONE', ( #40602 ), #3485, .F. ) ;
#59862 = VECTOR ( 'NONE', #65029, 1000.000000000000000 ) ;
#59863 = PLANE ( 'NONE',  #19182 ) ;
#59864 = ORIENTED_EDGE ( 'NONE', *, *, #28069, .T. ) ;
#59865 = FACE_OUTER_BOUND ( 'NONE', #20001, .T. ) ;
#59867 = ORIENTED_EDGE ( 'NONE', *, *, #16980, .T. ) ;
#59866 = DIRECTION ( 'NONE',  ( 0.000000000000000000, 0.000000000000000000, 1.000000000000000000 ) ) ;
#59868 = LINE ( 'NONE', #10392, #25339 ) ;
#59869 = PLANE ( 'NONE',  #43647 ) ;
#59870 = DIRECTION ( 'NONE',  ( 0.000000000000000000, -1.000000000000000000, 0.000000000000000000 ) ) ;
#59871 = DIRECTION ( 'NONE',  ( -0.000000000000000000, -0.000000000000000000, -1.000000000000000000 ) ) ;
#59872 = CIRCLE ( 'NONE', #40630, 24.99999999998784972 ) ;
#59873 = VECTOR ( 'NONE', #53247, 1000.000000000000000 ) ;
#59874 = DIRECTION ( 'NONE',  ( 0.7071067811865514585, 0.7071067811865435759, -0.000000000000000000 ) ) ;
#59875 = ORIENTED_EDGE ( 'NONE', *, *, #34474, .T. ) ;
#59876 = LINE ( 'NONE', #28381, #65259 ) ;
#59877 = LINE ( 'NONE', #49613, #5228 ) ;
#59878 = ORIENTED_EDGE ( 'NONE', *, *, #49141, .F. ) ;
#59879 = VECTOR ( 'NONE', #63410, 1000.000000000000000 ) ;
#59880 = CARTESIAN_POINT ( 'NONE',  ( -11.00000000000000000, -12.00000000000000000, -10.52786404500095863 ) ) ;
#59881 = CARTESIAN_POINT ( 'NONE',  ( -7.250000000000000000, -7.449999999999998401, -15.50000000000000000 ) ) ;
#59882 = ORIENTED_EDGE ( 'NONE', *, *, #42323, .F. ) ;
#59883 = LINE ( 'NONE', #11438, #61753 ) ;
#59884 = DIRECTION ( 'NONE',  ( -1.836970198721029934E-16, 1.836970198721036344E-16, -1.000000000000000000 ) ) ;
#59885 = EDGE_LOOP ( 'NONE', ( #54009, #8657, #6907, #53878 ) ) ;
#59886 = DIRECTION ( 'NONE',  ( 0.000000000000000000, 1.000000000000000000, 0.000000000000000000 ) ) ;
#59887 = DIRECTION ( 'NONE',  ( -1.000000000000000000, 0.000000000000000000, 0.000000000000000000 ) ) ;
#59888 = CARTESIAN_POINT ( 'NONE',  ( 0.000000000000000000, -8.249999999999998224, -23.50000000000000000 ) ) ;
#59889 = CARTESIAN_POINT ( 'NONE',  ( 7.000000000000000000, -42.50000000000000000, -7.500000000000000000 ) ) ;
#59890 = ORIENTED_EDGE ( 'NONE', *, *, #50607, .F. ) ;
#59891 = AXIS2_PLACEMENT_3D ( 'NONE', #34331, #63326, #67586 ) ;
#59893 = ORIENTED_EDGE ( 'NONE', *, *, #34576, .T. ) ;
#59892 = CARTESIAN_POINT ( 'NONE',  ( 7.900000000000000355, -14.48845687959340012, -21.00000000000000000 ) ) ;
#59894 = EDGE_CURVE ( 'NONE', #15758, #14752, #25384, .T. ) ;
#59895 = AXIS2_PLACEMENT_3D ( 'NONE', #66655, #35515, #23526 ) ;
#59896 = CARTESIAN_POINT ( 'NONE',  ( -13.00000000000000178, -17.50000000000000000, 15.70499999999969809 ) ) ;
#59897 = ADVANCED_FACE ( 'NONE', ( #9483 ), #56516, .F. ) ;
#59898 = PLANE ( 'NONE',  #23291 ) ;
#59899 = DIRECTION ( 'NONE',  ( 0.000000000000000000, -1.000000000000000000, 0.000000000000000000 ) ) ;
#59900 = VERTEX_POINT ( 'NONE', #67126 ) ;
#59901 = EDGE_CURVE ( 'NONE', #22220, #66935, #29639, .T. ) ;
#59902 = AXIS2_PLACEMENT_3D ( 'NONE', #46733, #60980, #24828 ) ;
#59903 = LINE ( 'NONE', #32687, #16414 ) ;
#59904 = CARTESIAN_POINT ( 'NONE',  ( 0.000000000000000000, 8.250000000000001776, -22.50000000000000000 ) ) ;
#59905 = EDGE_CURVE ( 'NONE', #35824, #64638, #24698, .T. ) ;
#59906 = VERTEX_POINT ( 'NONE', #24344 ) ;
#59907 = ORIENTED_EDGE ( 'NONE', *, *, #35254, .T. ) ;
#59908 = VECTOR ( 'NONE', #65962, 1000.000000000000000 ) ;
#59909 = EDGE_LOOP ( 'NONE', ( #50500, #23304 ) ) ;
#59910 = CARTESIAN_POINT ( 'NONE',  ( 7.357023737882817827, -4.961189459950063885, 54.00000000000000711 ) ) ;
#59911 = ADVANCED_FACE ( 'NONE', ( #20095 ), #68541, .T. ) ;
#59912 = AXIS2_PLACEMENT_3D ( 'NONE', #10372, #32634, #20270 ) ;
#59913 = DIRECTION ( 'NONE',  ( 1.000000000000000000, 0.000000000000000000, 0.000000000000000000 ) ) ;
#59914 = EDGE_CURVE ( 'NONE', #47230, #53423, #36350, .T. ) ;
#59915 = CARTESIAN_POINT ( 'NONE',  ( -7.250000000000000888, -8.249999999999998224, -16.00000000000000000 ) ) ;
#59916 = ORIENTED_EDGE ( 'NONE', *, *, #47757, .T. ) ;
#59917 = ORIENTED_EDGE ( 'NONE', *, *, #46306, .T. ) ;
#59918 = ORIENTED_EDGE ( 'NONE', *, *, #41295, .F. ) ;
#59920 = LINE ( 'NONE', #44334, #7916 ) ;
#59919 = VECTOR ( 'NONE', #46284, 1000.000000000000000 ) ;
#59921 = VECTOR ( 'NONE', #64544, 1000.000000000000000 ) ;
#59922 = EDGE_LOOP ( 'NONE', ( #175, #36424, #29977, #66602 ) ) ;
#59923 = ORIENTED_EDGE ( 'NONE', *, *, #57494, .T. ) ;
#59924 = EDGE_LOOP ( 'NONE', ( #42500, #1902, #46611, #2640 ) ) ;
#59925 = ORIENTED_EDGE ( 'NONE', *, *, #61708, .T. ) ;
#59926 = LINE ( 'NONE', #33739, #38415 ) ;
#59927 = UNCERTAINTY_MEASURE_WITH_UNIT (LENGTH_MEASURE( 1.000000000000000082E-05 ), #45026, 'distance_accuracy_value', 'NONE');
#59929 = ORIENTED_EDGE ( 'NONE', *, *, #2676, .F. ) ;
#59928 = CARTESIAN_POINT ( 'NONE',  ( -7.250000000000000888, 7.250000000000001776, -26.00000000000001066 ) ) ;
#59930 = DIRECTION ( 'NONE',  ( -0.000000000000000000, -0.000000000000000000, 1.000000000000000000 ) ) ;
#59931 = CARTESIAN_POINT ( 'NONE',  ( 6.836383711242970840, 4.135079735113107446, 26.00000000000000711 ) ) ;
#59932 = DIRECTION ( 'NONE',  ( 1.000000000000000000, 0.000000000000000000, 0.000000000000000000 ) ) ;
#59933 = VERTEX_POINT ( 'NONE', #25398 ) ;
#59934 = PLANE ( 'NONE',  #28894 ) ;
#59935 = CIRCLE ( 'NONE', #24961, 1.000000000000000000 ) ;
#59936 = VERTEX_POINT ( 'NONE', #62876 ) ;
#59937 = PLANE ( 'NONE',  #51783 ) ;
#59938 = DIRECTION ( 'NONE',  ( -1.000000000000000000, 0.000000000000000000, 0.000000000000000000 ) ) ;
#59939 = AXIS2_PLACEMENT_3D ( 'NONE', #59768, #49161, #54128 ) ;
#59940 = LINE ( 'NONE', #55343, #22142 ) ;
#59941 = FACE_OUTER_BOUND ( 'NONE', #39931, .T. ) ;
#59942 = ORIENTED_EDGE ( 'NONE', *, *, #3174, .T. ) ;
#59943 = DIRECTION ( 'NONE',  ( 0.000000000000000000, 0.000000000000000000, 1.000000000000000000 ) ) ;
#59944 = EDGE_CURVE ( 'NONE', #68361, #55748, #59354, .T. ) ;
#59945 = CARTESIAN_POINT ( 'NONE',  ( -15.50000000000000000, 0.000000000000000000, 26.50000000000000000 ) ) ;
#59946 = CARTESIAN_POINT ( 'NONE',  ( 55.00000000000000000, -21.00000000000000000, -16.96999999999999886 ) ) ;
#59947 = VECTOR ( 'NONE', #36579, 1000.000000000000114 ) ;
#59948 = CIRCLE ( 'NONE', #63506, 3.499999999999850342 ) ;
#59949 = ADVANCED_FACE ( 'NONE', ( #61831 ), #3140, .T. ) ;
#59950 = DIRECTION ( 'NONE',  ( -1.000000000000000000, 0.000000000000000000, 0.000000000000000000 ) ) ;
#59951 = CARTESIAN_POINT ( 'NONE',  ( 33.89999999999999858, -0.1999999999911430404, -8.864436962241481021E-12 ) ) ;
#59952 = DIRECTION ( 'NONE',  ( 0.000000000000000000, 0.7046037717862339012, -0.7096009616570518874 ) ) ;
#59953 = CARTESIAN_POINT ( 'NONE',  ( -4.727349090213463612, 7.798499376343949407, 195.0000000000000284 ) ) ;
#59954 = AXIS2_PLACEMENT_3D ( 'NONE', #42938, #6512, #10758 ) ;
#59955 = DIRECTION ( 'NONE',  ( 0.000000000000000000, 0.7096009616570518874, 0.7046037717862339012 ) ) ;
#59956 = ORIENTED_EDGE ( 'NONE', *, *, #61270, .F. ) ;
#59957 = FACE_OUTER_BOUND ( 'NONE', #4701, .T. ) ;
#59958 = ADVANCED_FACE ( 'NONE', ( #67495 ), #9137, .F. ) ;
#59959 = CARTESIAN_POINT ( 'NONE',  ( 8.250000000000005329, 0.000000000000000000, -11.50000000000000000 ) ) ;
#59960 = VECTOR ( 'NONE', #5946, 1000.000000000000000 ) ;
#59961 = DIRECTION ( 'NONE',  ( 0.000000000000000000, 0.000000000000000000, -1.000000000000000000 ) ) ;
#59962 = CARTESIAN_POINT ( 'NONE',  ( -16.75000000000000000, -2.500000000000000000, -23.22168783648699986 ) ) ;
#59963 = VERTEX_POINT ( 'NONE', #19382 ) ;
#59964 = DIRECTION ( 'NONE',  ( -0.000000000000000000, -0.000000000000000000, -1.000000000000000000 ) ) ;
#59965 = CARTESIAN_POINT ( 'NONE',  ( -7.250000000000000888, 7.450000000000003730, -19.50000000000000000 ) ) ;
#59966 = EDGE_CURVE ( 'NONE', #8573, #51508, #52270, .T. ) ;
#59967 = CARTESIAN_POINT ( 'NONE',  ( -7.250000000000001776, -7.249999999999998224, -30.00000000000001066 ) ) ;
#59968 = LINE ( 'NONE', #65624, #30900 ) ;
#59969 = FACE_OUTER_BOUND ( 'NONE', #51751, .T. ) ;
#59970 = ORIENTED_EDGE ( 'NONE', *, *, #43807, .F. ) ;
#59971 = ORIENTED_EDGE ( 'NONE', *, *, #48565, .T. ) ;
#59972 = FACE_OUTER_BOUND ( 'NONE', #44493, .T. ) ;
#59973 = EDGE_CURVE ( 'NONE', #12301, #47019, #37858, .T. ) ;
#59974 = CARTESIAN_POINT ( 'NONE',  ( 0.000000000000000000, 0.000000000000000000, -21.00000000000000000 ) ) ;
#59975 = EDGE_LOOP ( 'NONE', ( #21273, #43906, #59546, #50378, #54046, #66045, #13558, #39973 ) ) ;
#59976 = PLANE ( 'NONE',  #25079 ) ;
#59977 = ORIENTED_EDGE ( 'NONE', *, *, #30136, .T. ) ;
#59978 = CARTESIAN_POINT ( 'NONE',  ( 7.250000000000005329, -7.249999999999998224, -11.00000000000000000 ) ) ;
#59979 = ORIENTED_EDGE ( 'NONE', *, *, #36682, .F. ) ;
#59980 = VERTEX_POINT ( 'NONE', #40948 ) ;
#59982 = EDGE_CURVE ( 'NONE', #24664, #36931, #46254, .T. ) ;
#59981 = LINE ( 'NONE', #33115, #18197 ) ;
#59983 = VECTOR ( 'NONE', #5446, 1000.000000000000000 ) ;
#59984 = ORIENTED_EDGE ( 'NONE', *, *, #66924, .T. ) ;
#59985 = DIRECTION ( 'NONE',  ( 0.000000000000000000, -1.000000000000000000, 0.000000000000000000 ) ) ;
#59986 = EDGE_CURVE ( 'NONE', #68597, #29795, #35637, .T. ) ;
#59987 = FACE_OUTER_BOUND ( 'NONE', #55128, .T. ) ;
#59988 = DIRECTION ( 'NONE',  ( -1.000000000000000000, 0.000000000000000000, 0.000000000000000000 ) ) ;
#59989 = ORIENTED_EDGE ( 'NONE', *, *, #10874, .T. ) ;
#59990 = ORIENTED_EDGE ( 'NONE', *, *, #54678, .F. ) ;
#59991 = CYLINDRICAL_SURFACE ( 'NONE', #64027, 2.204799999999997429 ) ;
#59992 = CARTESIAN_POINT ( 'NONE',  ( 30.00000000000000000, -13.79999999999979998, 17.64999999999988844 ) ) ;
#59993 = ORIENTED_EDGE ( 'NONE', *, *, #2871, .T. ) ;
#59994 = ADVANCED_FACE ( 'NONE', ( #4881 ), #32786, .F. ) ;
#59995 = ORIENTED_EDGE ( 'NONE', *, *, #34576, .F. ) ;
#59996 = CIRCLE ( 'NONE', #16009, 24.99999999998789946 ) ;
#59997 = AXIS2_PLACEMENT_3D ( 'NONE', #58613, #5560, #27469 ) ;
#59999 = ORIENTED_EDGE ( 'NONE', *, *, #20241, .F. ) ;
#59998 = ITEM_DEFINED_TRANSFORMATION ( 'NONE', 'NONE', #18863,  #45918 ) ;
#60000 = CARTESIAN_POINT ( 'NONE',  ( -15.50000000000000000, -5.000000000000000000, 18.50000000000000000 ) ) ;
#60002 = EDGE_LOOP ( 'NONE', ( #69017, #64876, #51767, #35259 ) ) ;
#60001 = DIRECTION ( 'NONE',  ( -1.000000000000000000, 0.000000000000000000, 0.000000000000000000 ) ) ;
#60003 = CARTESIAN_POINT ( 'NONE',  ( 17.89999999999999858, 20.60000000000000142, -13.86939075806900057 ) ) ;
#60004 = CARTESIAN_POINT ( 'NONE',  ( 15.00000000000000000, -42.00000000000000000, 26.50000000000000000 ) ) ;
#60005 = ORIENTED_EDGE ( 'NONE', *, *, #40574, .T. ) ;
#60006 = VERTEX_POINT ( 'NONE', #26805 ) ;
#60007 = VECTOR ( 'NONE', #40734, 1000.000000000000000 ) ;
#60008 = VERTEX_POINT ( 'NONE', #48014 ) ;
#60009 = EDGE_CURVE ( 'NONE', #50215, #64072, #54029, .T. ) ;
#60010 = LINE ( 'NONE', #283, #7639 ) ;
#60011 = FACE_OUTER_BOUND ( 'NONE', #46095, .T. ) ;
#60012 = ORIENTED_EDGE ( 'NONE', *, *, #69892, .T. ) ;
#60013 = EDGE_CURVE ( 'NONE', #56701, #67879, #3990, .T. ) ;
#60014 = FACE_OUTER_BOUND ( 'NONE', #14147, .T. ) ;
#60015 = FACE_OUTER_BOUND ( 'NONE', #59818, .T. ) ;
#60016 = AXIS2_PLACEMENT_3D ( 'NONE', #26286, #20973, #42549 ) ;
#60018 = ORIENTED_EDGE ( 'NONE', *, *, #38413, .F. ) ;
#60017 = DIRECTION ( 'NONE',  ( -0.7671651518152939886, 0.6414496315691644579, 0.000000000000000000 ) ) ;
#60019 = ORIENTED_EDGE ( 'NONE', *, *, #37886, .F. ) ;
#60020 = EDGE_CURVE ( 'NONE', #60253, #10983, #16181, .T. ) ;
#60021 = DIRECTION ( 'NONE',  ( -0.7071067811865500152, -0.7071067811865451302, 4.683861624749757595E-31 ) ) ;
#60022 = DIRECTION ( 'NONE',  ( -0.7071067811865527908, -0.7071067811865422437, 0.000000000000000000 ) ) ;
#60023 = EDGE_CURVE ( 'NONE', #22866, #20587, #69501, .T. ) ;
#60024 = DIRECTION ( 'NONE',  ( 0.000000000000000000, 0.000000000000000000, -1.000000000000000000 ) ) ;
#60025 = DIRECTION ( 'NONE',  ( -0.000000000000000000, -0.000000000000000000, -1.000000000000000000 ) ) ;
#60026 = EDGE_CURVE ( 'NONE', #16692, #26902, #10182, .T. ) ;
#60027 = CYLINDRICAL_SURFACE ( 'NONE', #37583, 24.99999999998784972 ) ;
#60028 = ORIENTED_EDGE ( 'NONE', *, *, #55889, .F. ) ;
#60029 = CARTESIAN_POINT ( 'NONE',  ( 7.969523737882816761, 9.547976262117186863, 54.00000000000000711 ) ) ;
#60030 = CARTESIAN_POINT ( 'NONE',  ( -10.91351654964671525, -2.906483450353338771, 455.0000000000000568 ) ) ;
#60031 = VECTOR ( 'NONE', #26916, 1000.000000000000000 ) ;
#60032 = LINE ( 'NONE', #304, #25516 ) ;
#60033 = DIRECTION ( 'NONE',  ( 9.912705577010386883E-15, 1.000000000000000000, 0.000000000000000000 ) ) ;
#60034 = PRODUCT_DEFINITION_SHAPE ( 'NONE', 'NONE',  #69985 ) ;
#60035 = CIRCLE ( 'NONE', #19351, 2.458500000000000796 ) ;
#60036 = CARTESIAN_POINT ( 'NONE',  ( 8.250000000000005329, 0.000000000000000000, -15.50000000000000000 ) ) ;
#60037 = CARTESIAN_POINT ( 'NONE',  ( -5.993516549646776603, -6.006483450353426790, 455.0000000000000568 ) ) ;
#60038 = EDGE_CURVE ( 'NONE', #54703, #38450, #52987, .T. ) ;
#60039 = DIRECTION ( 'NONE',  ( -0.000000000000000000, 3.673940397442059868E-16, -1.000000000000000000 ) ) ;
#60040 = ADVANCED_FACE ( 'NONE', ( #63935 ), #25766, .F. ) ;
#60041 = CARTESIAN_POINT ( 'NONE',  ( 49.00000000000000000, -0.1999999999911430404, -8.864436962241481021E-12 ) ) ;
#60042 = ORIENTED_EDGE ( 'NONE', *, *, #32438, .T. ) ;
#60043 = DIRECTION ( 'NONE',  ( -0.000000000000000000, 0.000000000000000000, -1.000000000000000000 ) ) ;
#60044 = DIRECTION ( 'NONE',  ( 0.000000000000000000, 0.000000000000000000, -1.000000000000000000 ) ) ;
#60045 = EDGE_CURVE ( 'NONE', #30328, #44316, #5579, .T. ) ;
#60046 = EDGE_LOOP ( 'NONE', ( #36087, #60200, #26921, #9223 ) ) ;
#60047 = LINE ( 'NONE', #59710, #5170 ) ;
#60049 = EDGE_CURVE ( 'NONE', #27219, #9490, #47312, .T. ) ;
#60048 = CIRCLE ( 'NONE', #69093, 4.000000000000000888 ) ;
#60050 = EDGE_CURVE ( 'NONE', #39788, #58819, #63587, .T. ) ;
#60051 = CLOSED_SHELL ( 'NONE', ( #29780, #31332, #29021, #9702, #32197, #31505, #7415, #68303, #46439, #45056, #4803, #49291, #19876, #5084, #56726, #50963, #45762, #68277, #65329, #29726, #67234, #50867, #13247, #54602, #537, #40062, #50620, #808, #7511, #33321, #35508, #31018, #53895, #57748, #54388, #28516, #52697, #59317, #66411, #17209, #58137, #15110, #25433, #58790, #54667, #37230, #41022, #44763, #60354, #33433, #63212, #4722, #45906, #38744, #60671, #25906, #15409, #24762, #31086, #48271, #27364, #62029, #57880, #10087, #6212, #37883, #53975, #47908, #8619, #13823, #58720, #67813, #57563, #13334, #58867, #48805, #66800, #53060, #24714, #66449, #4336, #24511, #37398, #5102, #39610, #228, #57035, #63244, #48213, #9879, #51899, #34689, #65492, #54259, #8484, #47663, #9134, #41525, #14722, #15317, #61240, #19576, #58312, #34188, #44062, #15, #19557, #65212, #26397, #16295, #49537, #52215, #37266, #63092, #7750, #62753, #57517, #38277, #31460, #2291, #54452, #17113, #36249, #21176, #51991, #65446, #23124, #27369, #66516, #36348, #56797, #67778, #66794, #13309, #61294, #43530, #23343, #5696, #60916, #26437, #66973, #26926, #60199, #65955, #14229, #19567, #13601, #23219, #10916, #31550, #6084, #34507, #26091, #7295, #2367, #69885, #35204, #46472, #60318, #1216, #44439, #2091, #7288, #14079, #37556, #63835, #25006, #37187, #61876, #42818, #19515, #42886, #49741, #21353, #18529, #52340, #18881, #46658, #68689, #69872, #29922, #64974, #36014, #1273, #62885, #28181, #23309, #17966, #31162, #65260, #42618, #45023, #3829, #55862, #39857, #45292, #15847, #40068, #61373, #56528, #46473, #66829, #45952, #19436, #1358, #39606, #16383, #41053, #11659, #51984, #58633, #27892, #59595, #46478, #19725, #22840, #38500, #53363, #36604, #50450, #33342, #1168, #47208, #18757, #32032, #25160, #36117, #54991, #28272, #8162, #14691, #31481, #68690, #68716, #61303, #33000, #21585, #14390, #63983, #6339, #25462, #30789, #1306, #36656, #28443, #29231, #52845, #19017, #59730, #71, #57833, #61103, #53370, #50346, #4421, #16701, #38198, #26161, #28270, #18537, #30683, #31732, #47010, #48769, #55843, #4999, #10712, #10417, #27671, #35473, #4945, #63952, #22774, #63289, #53555, #21106, #12380, #49575, #69140, #27569, #57903, #44837, #22697, #64067, #435, #7429, #68816, #1684, #28023, #36002, #18993, #57173, #51259, #39530, #9349, #48566, #63521, #50404, #9869, #9240, #36834, #69979, #15599, #61143, #51920, #41854, #18446, #30400, #67718, #62529, #22834, #40955, #51455, #2027, #45346, #45599, #44570, #48413, #10753, #66018, #67750, #403, #63647, #20602, #65450, #55293, #57612, #17659, #1453, #49585, #57159, #69969, #29078, #65647, #27242, #12069, #56898, #1886, #66892, #45090, #67329, #59681, #3577, #49674, #11068, #69420, #33073, #2239, #54546, #58798, #54557, #42133, #22859, #12786, #43572, #52814, #5772, #47556, #43265, #61863, #2908, #58225, #17411, #38063, #272, #1774, #31342, #48652, #10650, #25975, #52206, #32692, #40127, #21516, #65632, #22567, #2292, #58184, #56330, #63968, #24213, #22994, #65202, #68072, #25877, #41361, #7897, #68270, #25840, #43056, #13937, #23042, #1754, #21345, #63985, #556, #10787, #42756, #27625 ) ) ;
#60052 = CARTESIAN_POINT ( 'NONE',  ( 7.450000000000004619, -1.336933437520057563E-15, -15.50000000000000000 ) ) ;
#60053 = DIRECTION ( 'NONE',  ( -1.000000000000000000, 0.000000000000000000, 0.000000000000000000 ) ) ;
#60054 = CARTESIAN_POINT ( 'NONE',  ( 10.00000000000000000, -18.00000000000000355, -21.00000000000000000 ) ) ;
#60055 = DIRECTION ( 'NONE',  ( 8.802523127157697409E-15, 1.000000000000000000, 0.000000000000000000 ) ) ;
#60056 = EDGE_CURVE ( 'NONE', #26381, #55064, #269, .T. ) ;
#60057 = CARTESIAN_POINT ( 'NONE',  ( 25.50000000000000355, -5.200000000000001066, 20.24999999999999645 ) ) ;
#60058 = ORIENTED_EDGE ( 'NONE', *, *, #37787, .T. ) ;
#60059 = DIRECTION ( 'NONE',  ( -1.000000000000000000, 0.000000000000000000, 0.000000000000000000 ) ) ;
#60060 = DIRECTION ( 'NONE',  ( 0.000000000000000000, -1.000000000000000000, 0.000000000000000000 ) ) ;
#60061 = ORIENTED_EDGE ( 'NONE', *, *, #29292, .T. ) ;
#60062 = DIRECTION ( 'NONE',  ( 0.000000000000000000, 0.000000000000000000, 1.000000000000000000 ) ) ;
#60063 = CIRCLE ( 'NONE', #38626, 1.224999999999999423 ) ;
#60064 = DIRECTION ( 'NONE',  ( -0.000000000000000000, 3.673940397442059868E-16, -1.000000000000000000 ) ) ;
#60065 = CARTESIAN_POINT ( 'NONE',  ( 10.09643294401454661, -9.306483450353491449, 455.0000000000000568 ) ) ;
#60066 = ORIENTED_EDGE ( 'NONE', *, *, #39139, .T. ) ;
#60067 = ORIENTED_EDGE ( 'NONE', *, *, #568, .F. ) ;
#60069 = ADVANCED_FACE ( 'NONE', ( #53334, #36710 ), #26450, .F. ) ;
#60068 = DIRECTION ( 'NONE',  ( -1.000000000000000000, 0.000000000000000000, 0.000000000000000000 ) ) ;
#60070 = ORIENTED_EDGE ( 'NONE', *, *, #25026, .T. ) ;
#60071 = VERTEX_POINT ( 'NONE', #43391 ) ;
#60072 = EDGE_CURVE ( 'NONE', #65035, #55322, #69232, .T. ) ;
#60073 = DIRECTION ( 'NONE',  ( -1.000000000000000000, 1.047444401652940007E-14, -1.836970198721010952E-16 ) ) ;
#60074 = DIRECTION ( 'NONE',  ( -1.836970198721029934E-16, 1.836970198721036344E-16, -1.000000000000000000 ) ) ;
#60075 = FACE_OUTER_BOUND ( 'NONE', #61116, .T. ) ;
#60076 = ORIENTED_EDGE ( 'NONE', *, *, #52253, .F. ) ;
#60077 = CARTESIAN_POINT ( 'NONE',  ( -1.466476262117236029, 8.598420958951576765, 26.00000000000000711 ) ) ;
#60079 = CARTESIAN_POINT ( 'NONE',  ( 11.19000000000000128, -11.25000000000000178, -5.000000000000000000 ) ) ;
#60078 = DIRECTION ( 'NONE',  ( -1.836970198721029934E-16, 1.836970198721036344E-16, -1.000000000000000000 ) ) ;
#60080 = VERTEX_POINT ( 'NONE', #42704 ) ;
#60081 = ORIENTED_EDGE ( 'NONE', *, *, #55599, .T. ) ;
#60083 = ORIENTED_EDGE ( 'NONE', *, *, #40615, .F. ) ;
#60082 = DIRECTION ( 'NONE',  ( 0.000000000000000000, 0.000000000000000000, 1.000000000000000000 ) ) ;
#60084 = AXIS2_PLACEMENT_3D ( 'NONE', #33132, #33483, #22536 ) ;
#60085 = VERTEX_POINT ( 'NONE', #59314 ) ;
#60086 = DIRECTION ( 'NONE',  ( -1.000000000000000000, 0.000000000000000000, 0.000000000000000000 ) ) ;
#60087 = VECTOR ( 'NONE', #11237, 1000.000000000000000 ) ;
#60088 = DIRECTION ( 'NONE',  ( 0.000000000000000000, -5.800915303574361727E-12, 1.000000000000000000 ) ) ;
#60089 = EDGE_CURVE ( 'NONE', #23316, #24412, #64284, .T. ) ;
#60090 = ORIENTED_EDGE ( 'NONE', *, *, #501, .F. ) ;
#60091 = ORIENTED_EDGE ( 'NONE', *, *, #30358, .T. ) ;
#60092 = AXIS2_PLACEMENT_3D ( 'NONE', #24432, #66507, #13812 ) ;
#60093 = CYLINDRICAL_SURFACE ( 'NONE', #44780, 2.000000000000001776 ) ;
#60094 = DIRECTION ( 'NONE',  ( 0.000000000000000000, -1.000000000000000000, 0.000000000000000000 ) ) ;
#60095 = VECTOR ( 'NONE', #13544, 1000.000000000000000 ) ;
#60096 = ORIENTED_EDGE ( 'NONE', *, *, #53349, .T. ) ;
#60097 = DIRECTION ( 'NONE',  ( 0.4998444328988824181, 0.000000000000000000, -0.8661152018640445593 ) ) ;
#60098 = LINE ( 'NONE', #44175, #41390 ) ;
#60099 = DIRECTION ( 'NONE',  ( -1.000000000000000000, 0.000000000000000000, 0.000000000000000000 ) ) ;
#60100 = VERTEX_POINT ( 'NONE', #38117 ) ;
#60101 = EDGE_CURVE ( 'NONE', #40247, #42678, #64621, .T. ) ;
#60102 = CARTESIAN_POINT ( 'NONE',  ( -15.50000000000000000, -15.50000000000000000, 22.50000000000000000 ) ) ;
#60103 = CARTESIAN_POINT ( 'NONE',  ( 283.0000000000000568, -42.50000000000000000, 10.20000000000000107 ) ) ;
#60105 = EDGE_LOOP ( 'NONE', ( #44231, #18872, #2373, #48619 ) ) ;
#60104 = LINE ( 'NONE', #61849, #15995 ) ;
#60107 = VERTEX_POINT ( 'NONE', #21831 ) ;
#60106 = DIRECTION ( 'NONE',  ( 1.836970198721029934E-16, 1.836970198721010706E-16, -1.000000000000000000 ) ) ;
#60108 = EDGE_CURVE ( 'NONE', #11005, #69324, #11217, .T. ) ;
#60110 = LINE ( 'NONE', #33920, #14435 ) ;
#60109 = VECTOR ( 'NONE', #43790, 1000.000000000000000 ) ;
#60111 = FACE_OUTER_BOUND ( 'NONE', #41086, .T. ) ;
#60112 = ADVANCED_FACE ( 'NONE', ( #60337 ), #27834, .F. ) ;
#60113 = DIRECTION ( 'NONE',  ( 0.000000000000000000, 3.673940397442059868E-16, -1.000000000000000000 ) ) ;
#60114 = DIRECTION ( 'NONE',  ( 0.000000000000000000, -1.000000000000000000, 0.000000000000000000 ) ) ;
#60115 = LINE ( 'NONE', #33923, #15864 ) ;
#60116 = ADVANCED_FACE ( 'NONE', ( #24175 ), #65330, .F. ) ;
#60117 = CARTESIAN_POINT ( 'NONE',  ( 24.00000000000000000, -17.35230188589299871, 15.35019951917099945 ) ) ;
#60118 = EDGE_LOOP ( 'NONE', ( #64653, #6275, #64603, #59676 ) ) ;
#60119 = DIRECTION ( 'NONE',  ( 0.000000000000000000, 0.000000000000000000, 1.000000000000000000 ) ) ;
#60121 = ORIENTED_EDGE ( 'NONE', *, *, #60590, .T. ) ;
#60120 = FACE_OUTER_BOUND ( 'NONE', #25066, .T. ) ;
#60123 = VERTEX_POINT ( 'NONE', #65662 ) ;
#60122 = LINE ( 'NONE', #34629, #6200 ) ;
#60124 = CARTESIAN_POINT ( 'NONE',  ( -7.250000000000000888, -8.249999999999998224, -25.00000000000000000 ) ) ;
#60125 = DIRECTION ( 'NONE',  ( 0.000000000000000000, 0.000000000000000000, 1.000000000000000000 ) ) ;
#60126 = ORIENTED_EDGE ( 'NONE', *, *, #39815, .T. ) ;
#60127 = CARTESIAN_POINT ( 'NONE',  ( 0.000000000000000000, 8.750000000000001776, -30.00000000000001066 ) ) ;
#60128 = CYLINDRICAL_SURFACE ( 'NONE', #11394, 2.204799999999997873 ) ;
#60129 = AXIS2_PLACEMENT_3D ( 'NONE', #9807, #58929, #32056 ) ;
#60130 = ORIENTED_EDGE ( 'NONE', *, *, #26537, .F. ) ;
#60131 = ADVANCED_FACE ( 'NONE', ( #13913 ), #44086, .F. ) ;
#60132 = CARTESIAN_POINT ( 'NONE',  ( 7.265214908726123078, -6.619341603356961201, 455.0000000000000568 ) ) ;
#60133 = CARTESIAN_POINT ( 'NONE',  ( 3.682023737882814451, 9.897976262117207824, 26.00000000000000711 ) ) ;
#60134 = DIRECTION ( 'NONE',  ( -1.000000000000000000, 0.000000000000000000, 0.000000000000000000 ) ) ;
#60135 = AXIS2_PLACEMENT_3D ( 'NONE', #39413, #33077, #55347 ) ;
#60136 = CARTESIAN_POINT ( 'NONE',  ( 158.8349105750994568, -35.83962462487175316, 0.000000000000000000 ) ) ;
#60137 = CYLINDRICAL_SURFACE ( 'NONE', #26354, 0.5000000000079367624 ) ;
#60138 = EDGE_LOOP ( 'NONE', ( #62763, #35582, #66776, #50021 ) ) ;
#60139 = LINE ( 'NONE', #38250, #29355 ) ;
#60140 = ORIENTED_EDGE ( 'NONE', *, *, #59186, .T. ) ;
#60141 = VERTEX_POINT ( 'NONE', #55067 ) ;
#60142 = CARTESIAN_POINT ( 'NONE',  ( -11.50000000000000000, -11.50000000000000000, -15.00000000000000000 ) ) ;
#60143 = DIRECTION ( 'NONE',  ( 1.836970198721029934E-16, 1.836970198721010706E-16, -1.000000000000000000 ) ) ;
#60144 = LINE ( 'NONE', #49206, #59217 ) ;
#60145 = CARTESIAN_POINT ( 'NONE',  ( -25.50000000000000355, -15.50000000000000000, -22.50000000000000000 ) ) ;
#60146 = ORIENTED_EDGE ( 'NONE', *, *, #28258, .F. ) ;
#60147 = ORIENTED_EDGE ( 'NONE', *, *, #38773, .F. ) ;
#60150 = VERTEX_POINT ( 'NONE', #38782 ) ;
#60149 = ADVANCED_FACE ( 'NONE', ( #17212 ), #39128, .F. ) ;
#60148 = LINE ( 'NONE', #21643, #19366 ) ;
#60151 = VERTEX_POINT ( 'NONE', #621 ) ;
#60152 = EDGE_CURVE ( 'NONE', #27398, #10620, #49055, .T. ) ;
#60153 = CYLINDRICAL_SURFACE ( 'NONE', #55208, 1.399999999999998579 ) ;
#60154 = VECTOR ( 'NONE', #55983, 1000.000000000000000 ) ;
#60155 = CARTESIAN_POINT ( 'NONE',  ( -8.250000000000001776, -8.249999999999998224, -26.00000000000001066 ) ) ;
#60156 = CARTESIAN_POINT ( 'NONE',  ( 7.616533956692244978, 8.593516549646574632, 455.0000000000000568 ) ) ;
#60157 = EDGE_CURVE ( 'NONE', #67890, #30509, #33482, .T. ) ;
#60158 = VECTOR ( 'NONE', #62036, 1000.000000000000000 ) ;
#60159 = FACE_OUTER_BOUND ( 'NONE', #65590, .T. ) ;
#60161 = CARTESIAN_POINT ( 'NONE',  ( 7.261609891743268541, -8.000000000000000000, 0.000000000000000000 ) ) ;
#60160 = PLANE ( 'NONE',  #16271 ) ;
#60162 = CIRCLE ( 'NONE', #52245, 1.000000000000000000 ) ;
#60163 = VERTEX_POINT ( 'NONE', #22870 ) ;
#60165 = ORIENTED_EDGE ( 'NONE', *, *, #58766, .F. ) ;
#60164 = LINE ( 'NONE', #17041, #40902 ) ;
#60166 = EDGE_LOOP ( 'NONE', ( #52113, #22444, #12107, #13919, #21467, #61113, #5201, #15329 ) ) ;
#60167 = ORIENTED_EDGE ( 'NONE', *, *, #21973, .F. ) ;
#60168 = DIRECTION ( 'NONE',  ( 1.000000000000000000, -0.000000000000000000, -0.000000000000000000 ) ) ;
#60169 = CIRCLE ( 'NONE', #55624, 0.1999999999999987899 ) ;
#60170 = LINE ( 'NONE', #38278, #68231 ) ;
#60171 = DIRECTION ( 'NONE',  ( 0.000000000000000000, -1.000000000000000000, 0.000000000000000000 ) ) ;
#60172 = AXIS2_PLACEMENT_3D ( 'NONE', #48459, #64719, #43143 ) ;
#60173 = DIRECTION ( 'NONE',  ( 0.000000000000000000, 1.000000000000000000, 0.000000000000000000 ) ) ;
#60174 = VERTEX_POINT ( 'NONE', #44416 ) ;
#60175 = ORIENTED_EDGE ( 'NONE', *, *, #32950, .F. ) ;
#60176 = CARTESIAN_POINT ( 'NONE',  ( -8.598420958951683346, 1.466476262117183182, 26.00000000000000711 ) ) ;
#60177 = DIRECTION ( 'NONE',  ( 0.000000000000000000, 0.000000000000000000, 1.000000000000000000 ) ) ;
#60178 = VECTOR ( 'NONE', #64173, 1000.000000000000000 ) ;
#60179 = ORIENTED_EDGE ( 'NONE', *, *, #62946, .F. ) ;
#60180 = ORIENTED_EDGE ( 'NONE', *, *, #20456, .T. ) ;
#60181 = DIRECTION ( 'NONE',  ( -0.5000000000000068834, -0.8660254037844345998, 0.000000000000000000 ) ) ;
#60182 = AXIS2_PLACEMENT_3D ( 'NONE', #39634, #60173, #49910 ) ;
#60183 = CARTESIAN_POINT ( 'NONE',  ( -15.50000000000000000, -0.2038245569916614930, -23.94337567297399971 ) ) ;
#60184 = ORIENTED_EDGE ( 'NONE', *, *, #3710, .F. ) ;
#60185 = EDGE_CURVE ( 'NONE', #64953, #17826, #65990, .T. ) ;
#60186 = CARTESIAN_POINT ( 'NONE',  ( 0.000000000000000000, 8.250000000000001776, -12.50000000000000000 ) ) ;
#60187 = AXIS2_PLACEMENT_3D ( 'NONE', #19717, #18207, #66996 ) ;
#60189 = ORIENTED_EDGE ( 'NONE', *, *, #31507, .T. ) ;
#60188 = DIRECTION ( 'NONE',  ( 0.000000000000000000, 0.000000000000000000, -1.000000000000000000 ) ) ;
#60190 = ORIENTED_EDGE ( 'NONE', *, *, #51675, .T. ) ;
#60191 = DIRECTION ( 'NONE',  ( 0.000000000000000000, 0.000000000000000000, -1.000000000000000000 ) ) ;
#60192 = CYLINDRICAL_SURFACE ( 'NONE', #28949, 0.1999999999999987899 ) ;
#60193 = PLANE ( 'NONE',  #52120 ) ;
#60194 = EDGE_CURVE ( 'NONE', #52241, #68881, #61996, .T. ) ;
#60195 = EDGE_CURVE ( 'NONE', #24795, #55692, #56699, .T. ) ;
#60196 = CARTESIAN_POINT ( 'NONE',  ( 16.33565937784172917, -0.3156604612126656106, 23.46090750622625976 ) ) ;
#60197 = DIRECTION ( 'NONE',  ( 0.000000000000000000, 0.000000000000000000, -1.000000000000000000 ) ) ;
#60198 = EDGE_CURVE ( 'NONE', #13897, #57808, #62342, .T. ) ;
#60199 = ADVANCED_FACE ( 'NONE', ( #16880 ), #27482, .F. ) ;
#60200 = ORIENTED_EDGE ( 'NONE', *, *, #58058, .T. ) ;
#60201 = ORIENTED_EDGE ( 'NONE', *, *, #11451, .T. ) ;
#60202 = PLANE ( 'NONE',  #26460 ) ;
#60203 = AXIS2_PLACEMENT_3D ( 'NONE', #52801, #4358, #69037 ) ;
#60204 = CARTESIAN_POINT ( 'NONE',  ( -1.077516549646784449, -11.34648345035343198, 195.0000000000000284 ) ) ;
#60205 = EDGE_CURVE ( 'NONE', #29890, #53596, #13564, .T. ) ;
#60206 = DIRECTION ( 'NONE',  ( -8.903847840905249551E-15, -1.000000000000000000, -1.836970198721027222E-16 ) ) ;
#60208 = DIRECTION ( 'NONE',  ( -1.836970198721029934E-16, 1.836970198721036344E-16, -1.000000000000000000 ) ) ;
#60207 = CIRCLE ( 'NONE', #16204, 4.500000000000191847 ) ;
#60209 = CIRCLE ( 'NONE', #29717, 0.1999999999999996503 ) ;
#60210 = DIRECTION ( 'NONE',  ( 1.836970198721029934E-16, 1.836970198721010706E-16, -1.000000000000000000 ) ) ;
#60211 = AXIS2_PLACEMENT_3D ( 'NONE', #25582, #47147, #10017 ) ;
#60212 = ORIENTED_EDGE ( 'NONE', *, *, #50214, .F. ) ;
#60213 = ORIENTED_EDGE ( 'NONE', *, *, #9797, .T. ) ;
#60214 = CIRCLE ( 'NONE', #1510, 2.000000000000001776 ) ;
#60215 = LINE ( 'NONE', #11768, #34736 ) ;
#60216 = VECTOR ( 'NONE', #10817, 1000.000000000000000 ) ;
#60217 = PLANE ( 'NONE',  #25511 ) ;
#60218 = ORIENTED_EDGE ( 'NONE', *, *, #23652, .F. ) ;
#60219 = DIRECTION ( 'NONE',  ( 1.000000000000000000, -0.000000000000000000, -0.000000000000000000 ) ) ;
#60220 = DIRECTION ( 'NONE',  ( 0.000000000000000000, 0.000000000000000000, -1.000000000000000000 ) ) ;
#60221 = VERTEX_POINT ( 'NONE', #60000 ) ;
#60222 = DIRECTION ( 'NONE',  ( 0.000000000000000000, 0.000000000000000000, -1.000000000000000000 ) ) ;
#60223 = CARTESIAN_POINT ( 'NONE',  ( 39.90000000000000568, 16.96999999999999886, 21.00000000000000000 ) ) ;
#60224 = VERTEX_POINT ( 'NONE', #45730 ) ;
#60225 = LINE ( 'NONE', #49624, #1681 ) ;
#60226 = VECTOR ( 'NONE', #43191, 1000.000000000000000 ) ;
#60227 = LINE ( 'NONE', #43635, #62816 ) ;
#60229 = CARTESIAN_POINT ( 'NONE',  ( -4.193516549646673752, 11.31351654964658771, 455.0000000000000568 ) ) ;
#60228 = SHAPE_REPRESENTATION ( 'END CAP_6266N13', ( #45918 ), #25755 ) ;
#60230 = DIRECTION ( 'NONE',  ( -1.836970198721029934E-16, 1.836970198721036344E-16, -1.000000000000000000 ) ) ;
#60231 = ORIENTED_EDGE ( 'NONE', *, *, #39904, .F. ) ;
#60233 = ORIENTED_EDGE ( 'NONE', *, *, #33851, .T. ) ;
#60232 = CARTESIAN_POINT ( 'NONE',  ( -9.880476262117236175, 7.447976262117216528, 25.99999580000000421 ) ) ;
#60234 = LINE ( 'NONE', #33376, #45127 ) ;
#60235 = DIRECTION ( 'NONE',  ( 0.000000000000000000, 0.000000000000000000, 1.000000000000000000 ) ) ;
#60236 = PLANE ( 'NONE',  #4805 ) ;
#60237 = ORIENTED_EDGE ( 'NONE', *, *, #17891, .T. ) ;
#60238 = AXIS2_PLACEMENT_3D ( 'NONE', #2301, #12203, #33776 ) ;
#60239 = ADVANCED_FACE ( 'NONE', ( #67315 ), #8248, .F. ) ;
#60240 = EDGE_CURVE ( 'NONE', #42765, #40726, #46093, .T. ) ;
#60241 = LINE ( 'NONE', #33382, #23151 ) ;
#60242 = LINE ( 'NONE', #28407, #43193 ) ;
#60243 = VERTEX_POINT ( 'NONE', #25229 ) ;
#60244 = ORIENTED_EDGE ( 'NONE', *, *, #50170, .T. ) ;
#60245 = EDGE_CURVE ( 'NONE', #56934, #44584, #24876, .T. ) ;
#60246 = EDGE_LOOP ( 'NONE', ( #13774, #61011, #14956, #52967 ) ) ;
#60247 = CARTESIAN_POINT ( 'NONE',  ( -7.250000000000000888, 7.250000000000001776, -16.00000000000000000 ) ) ;
#60248 = DIRECTION ( 'NONE',  ( 0.000000000000000000, -1.000000000000000000, 0.000000000000000000 ) ) ;
#60249 = DIRECTION ( 'NONE',  ( 1.000000000000000000, 0.000000000000000000, 0.000000000000000000 ) ) ;
#60250 = VECTOR ( 'NONE', #24391, 1000.000000000000000 ) ;
#60251 = VECTOR ( 'NONE', #19631, 1000.000000000000000 ) ;
#60252 = VERTEX_POINT ( 'NONE', #14973 ) ;
#60253 = VERTEX_POINT ( 'NONE', #8952 ) ;
#60254 = ORIENTED_EDGE ( 'NONE', *, *, #54430, .T. ) ;
#60255 = CARTESIAN_POINT ( 'NONE',  ( 6.849523737882817542, -10.31452373788281207, 26.00000000000000000 ) ) ;
#60256 = ORIENTED_EDGE ( 'NONE', *, *, #30709, .F. ) ;
#60257 = MECHANICAL_DESIGN_GEOMETRIC_PRESENTATION_REPRESENTATION (  '', ( #18450 ), #27510 ) ;
#60258 = CIRCLE ( 'NONE', #59165, 4.000000000000000000 ) ;
#60259 = ORIENTED_EDGE ( 'NONE', *, *, #19215, .F. ) ;
#60260 = VERTEX_POINT ( 'NONE', #41495 ) ;
#60261 = EDGE_LOOP ( 'NONE', ( #59853, #24849, #47905, #69652 ) ) ;
#60262 = LINE ( 'NONE', #6186, #51937 ) ;
#60263 = VECTOR ( 'NONE', #10001, 1000.000000000000000 ) ;
#60264 = VECTOR ( 'NONE', #29158, 1000.000000000000000 ) ;
#60266 = VERTEX_POINT ( 'NONE', #30183 ) ;
#60265 = DIRECTION ( 'NONE',  ( 0.000000000000000000, -3.673940397442059868E-16, 1.000000000000000000 ) ) ;
#60267 = PLANE ( 'NONE',  #62788 ) ;
#60268 = FACE_OUTER_BOUND ( 'NONE', #20871, .T. ) ;
#60269 = LINE ( 'NONE', #53951, #9850 ) ;
#60270 = ORIENTED_EDGE ( 'NONE', *, *, #23829, .T. ) ;
#60271 = LINE ( 'NONE', #49672, #54298 ) ;
#60272 = DIRECTION ( 'NONE',  ( -1.836970198721029934E-16, 1.836970198721036590E-16, -1.000000000000000000 ) ) ;
#60273 = LINE ( 'NONE', #18180, #40579 ) ;
#60274 = EDGE_CURVE ( 'NONE', #19320, #62370, #15676, .T. ) ;
#60275 = ORIENTED_EDGE ( 'NONE', *, *, #55035, .F. ) ;
#60276 = FACE_BOUND ( 'NONE', #21257, .T. ) ;
#60277 = EDGE_CURVE ( 'NONE', #58530, #1475, #26276, .T. ) ;
#60278 = FACE_OUTER_BOUND ( 'NONE', #60732, .T. ) ;
#60279 = LINE ( 'NONE', #5860, #27787 ) ;
#60280 = EDGE_CURVE ( 'NONE', #34023, #16156, #33357, .T. ) ;
#60281 = ADVANCED_FACE ( 'NONE', ( #52101 ), #35832, .F. ) ;
#60282 = ORIENTED_EDGE ( 'NONE', *, *, #27800, .F. ) ;
#60283 = CIRCLE ( 'NONE', #29802, 0.3999999999993835154 ) ;
#60284 = CARTESIAN_POINT ( 'NONE',  ( 17.00000000000000000, -15.50000000000000000, -14.50000000000000000 ) ) ;
#60285 = CARTESIAN_POINT ( 'NONE',  ( 49.00000000000000000, -0.1999999999911430404, -8.864436962241481021E-12 ) ) ;
#60286 = PLANE ( 'NONE',  #16682 ) ;
#60287 = DIRECTION ( 'NONE',  ( 1.000000000000000000, -0.000000000000000000, 0.000000000000000000 ) ) ;
#60288 = CARTESIAN_POINT ( 'NONE',  ( 6.006483450353379716, -6.006483450353490738, 455.0000000000000568 ) ) ;
#60289 = FACE_OUTER_BOUND ( 'NONE', #49683, .T. ) ;
#60291 = EDGE_CURVE ( 'NONE', #33734, #66887, #8603, .T. ) ;
#60290 = CARTESIAN_POINT ( 'NONE',  ( -25.50000000000000355, -15.50000000000000000, 22.50000000000000000 ) ) ;
#60292 = FACE_OUTER_BOUND ( 'NONE', #63203, .T. ) ;
#60293 = VECTOR ( 'NONE', #25805, 1000.000000000000000 ) ;
#60294 = AXIS2_PLACEMENT_3D ( 'NONE', #40056, #13201, #7884 ) ;
#60295 = ORIENTED_EDGE ( 'NONE', *, *, #33719, .F. ) ;
#60296 = LINE ( 'NONE', #38402, #25860 ) ;
#60297 = CARTESIAN_POINT ( 'NONE',  ( -30.00000000000000000, -11.50000000000000000, -15.00000000000000000 ) ) ;
#60298 = DIRECTION ( 'NONE',  ( -1.836970198721029934E-16, 1.836970198721036590E-16, -1.000000000000000000 ) ) ;
#60299 = FACE_OUTER_BOUND ( 'NONE', #20533, .T. ) ;
#60300 = AXIS2_PLACEMENT_3D ( 'NONE', #37836, #54100, #64029 ) ;
#60301 = VECTOR ( 'NONE', #42233, 1000.000000000000114 ) ;
#60302 = VERTEX_POINT ( 'NONE', #19562 ) ;
#60303 = AXIS2_PLACEMENT_3D ( 'NONE', #19505, #67957, #30470 ) ;
#60304 = DIRECTION ( 'NONE',  ( 0.000000000000000000, 0.000000000000000000, -1.000000000000000000 ) ) ;
#60305 = DIRECTION ( 'NONE',  ( 1.000000000000000000, 0.000000000000000000, 0.000000000000000000 ) ) ;
#60306 = LINE ( 'NONE', #18215, #22103 ) ;
#60307 = AXIS2_PLACEMENT_3D ( 'NONE', #27226, #38189, #59738 ) ;
#60308 = FACE_OUTER_BOUND ( 'NONE', #9469, .T. ) ;
#60309 = CARTESIAN_POINT ( 'NONE',  ( -2.989207322240233555, -6.872275254348434892, 54.00000000000000711 ) ) ;
#60310 = ORIENTED_EDGE ( 'NONE', *, *, #65282, .F. ) ;
#60311 = VECTOR ( 'NONE', #23577, 1000.000000000000000 ) ;
#60312 = ORIENTED_EDGE ( 'NONE', *, *, #56616, .T. ) ;
#60313 = CARTESIAN_POINT ( 'NONE',  ( 47.00000000000000000, -0.7500000000000000000, -4.943429983321300014 ) ) ;
#60314 = DIRECTION ( 'NONE',  ( -0.4285714285711678118, 0.000000000000000000, -0.9035079029053749711 ) ) ;
#60315 = VERTEX_POINT ( 'NONE', #58104 ) ;
#60316 = DIRECTION ( 'NONE',  ( 0.000000000000000000, 0.000000000000000000, -1.000000000000000000 ) ) ;
#60317 = ORIENTED_EDGE ( 'NONE', *, *, #52267, .T. ) ;
#60318 = ADVANCED_FACE ( 'NONE', ( #9674 ), #20966, .F. ) ;
#60319 = CARTESIAN_POINT ( 'NONE',  ( 7.606483450353373144, 11.31351654964662323, 195.0000000000000284 ) ) ;
#60320 = ORIENTED_EDGE ( 'NONE', *, *, #14167, .T. ) ;
#60321 = EDGE_LOOP ( 'NONE', ( #2785, #62758, #8526, #8748 ) ) ;
#60322 = CYLINDRICAL_SURFACE ( 'NONE', #45295, 2.204799999999998761 ) ;
#60323 = VERTEX_POINT ( 'NONE', #4382 ) ;
#60324 = CARTESIAN_POINT ( 'NONE',  ( -6.817976262117261044, 9.722976262117182245, 54.00000000000000711 ) ) ;
#60325 = DIRECTION ( 'NONE',  ( -1.836970198721029934E-16, 1.836970198721036344E-16, -1.000000000000000000 ) ) ;
#60326 = CARTESIAN_POINT ( 'NONE',  ( 7.000000000000000000, -23.65000000000000568, 12.40000000000000213 ) ) ;
#60327 = ORIENTED_EDGE ( 'NONE', *, *, #49266, .T. ) ;
#60328 = ORIENTED_EDGE ( 'NONE', *, *, #57807, .T. ) ;
#60329 = DIRECTION ( 'NONE',  ( 9.912705577010336396E-15, 1.000000000000000000, 0.000000000000000000 ) ) ;
#60330 = CARTESIAN_POINT ( 'NONE',  ( -7.250000000000001776, -7.249999999999998224, -12.50000000000000000 ) ) ;
#60331 = EDGE_CURVE ( 'NONE', #51859, #14190, #62697, .T. ) ;
#60332 = VERTEX_POINT ( 'NONE', #47491 ) ;
#60333 = CIRCLE ( 'NONE', #29856, 4.500000000000190958 ) ;
#60334 = EDGE_LOOP ( 'NONE', ( #6922, #39701, #8003, #46664, #42778, #35179, #68310, #15566 ) ) ;
#60335 = ORIENTED_EDGE ( 'NONE', *, *, #6856, .T. ) ;
#60336 = EDGE_CURVE ( 'NONE', #2927, #44960, #53172, .T. ) ;
#60337 = FACE_OUTER_BOUND ( 'NONE', #16948, .T. ) ;
#60339 = ORIENTED_EDGE ( 'NONE', *, *, #67006, .F. ) ;
#60338 = FACE_OUTER_BOUND ( 'NONE', #57251, .T. ) ;
#60340 = CARTESIAN_POINT ( 'NONE',  ( 49.00000000000000000, -0.1999999999911795112, 8.826273045769999343E-12 ) ) ;
#60341 = VECTOR ( 'NONE', #34818, 1000.000000000000000 ) ;
#60342 = AXIS2_PLACEMENT_3D ( 'NONE', #49237, #33310, #10359 ) ;
#60343 = CARTESIAN_POINT ( 'NONE',  ( 11.50000000000000000, -11.70000000000012008, -10.70000000000011831 ) ) ;
#60344 = ORIENTED_EDGE ( 'NONE', *, *, #66314, .F. ) ;
#60345 = ORIENTED_EDGE ( 'NONE', *, *, #36674, .T. ) ;
#60346 = VECTOR ( 'NONE', #29699, 1000.000000000000114 ) ;
#60347 = AXIS2_PLACEMENT_3D ( 'NONE', #44622, #67255, #18810 ) ;
#60348 = DIRECTION ( 'NONE',  ( 1.000000000000000000, 0.000000000000000000, 0.000000000000000000 ) ) ;
#60349 = CYLINDRICAL_SURFACE ( 'NONE', #19994, 1.399999999999999245 ) ;
#60350 = EDGE_CURVE ( 'NONE', #46964, #42683, #69058, .T. ) ;
#60351 = AXIS2_PLACEMENT_3D ( 'NONE', #36034, #57604, #47697 ) ;
#60352 = LINE ( 'NONE', #44434, #66249 ) ;
#60353 = LINE ( 'NONE', #8000, #55015 ) ;
#60354 = ADVANCED_FACE ( 'NONE', ( #42537 ), #20611, .F. ) ;
#60355 = EDGE_CURVE ( 'NONE', #13793, #47124, #42181, .T. ) ;
#60357 = ORIENTED_EDGE ( 'NONE', *, *, #26431, .F. ) ;
#60356 = LINE ( 'NONE', #27856, #59117 ) ;
#60358 = EDGE_LOOP ( 'NONE', ( #2047, #24898, #36148, #54247 ) ) ;
#60359 = VECTOR ( 'NONE', #60416, 1000.000000000000000 ) ;
#60360 = DIRECTION ( 'NONE',  ( -5.981805089575196197E-17, -1.000000000000000000, 0.000000000000000000 ) ) ;
#60361 = DIRECTION ( 'NONE',  ( 0.000000000000000000, 0.000000000000000000, 1.000000000000000000 ) ) ;
#60362 = EDGE_CURVE ( 'NONE', #21951, #50851, #68725, .T. ) ;
#60363 = FACE_OUTER_BOUND ( 'NONE', #54264, .T. ) ;
#60364 = DIRECTION ( 'NONE',  ( 0.000000000000000000, 0.7096009616570518874, 0.7046037717862339012 ) ) ;
#60365 = CARTESIAN_POINT ( 'NONE',  ( 7.811466277050743479, 4.727349090213326832, 455.0000000000000568 ) ) ;
#60366 = EDGE_CURVE ( 'NONE', #36688, #29870, #3307, .T. ) ;
#60367 = ORIENTED_EDGE ( 'NONE', *, *, #54455, .F. ) ;
#60368 = DIRECTION ( 'NONE',  ( 1.000000000000000000, -5.981805089575196197E-17, 0.000000000000000000 ) ) ;
#60369 = DIRECTION ( 'NONE',  ( 0.000000000000000000, -0.6787500000000000755, -0.7343694148723788340 ) ) ;
#60371 = EDGE_CURVE ( 'NONE', #60571, #18478, #16404, .T. ) ;
#60370 = DIRECTION ( 'NONE',  ( 0.000000000000000000, 0.000000000000000000, -1.000000000000000000 ) ) ;
#60372 = FACE_OUTER_BOUND ( 'NONE', #14608, .T. ) ;
#60373 = DIRECTION ( 'NONE',  ( 1.000000000000000000, -8.903847840905249551E-15, 1.836970198721013664E-16 ) ) ;
#60374 = CARTESIAN_POINT ( 'NONE',  ( 0.9555237378828180805, 9.915476262117216777, 54.00000000000000711 ) ) ;
#60375 = CARTESIAN_POINT ( 'NONE',  ( 49.00000000000000000, -21.00000000000000000, 13.86939075806900057 ) ) ;
#60376 = DIRECTION ( 'NONE',  ( 0.000000000000000000, 1.000000000000000000, 0.000000000000000000 ) ) ;
#60377 = VERTEX_POINT ( 'NONE', #19918 ) ;
#60378 = CARTESIAN_POINT ( 'NONE',  ( -30.00000000000000000, -17.14999999999999858, 27.00000000000000000 ) ) ;
#60379 = DIRECTION ( 'NONE',  ( -0.000000000000000000, 3.673940397442059868E-16, -1.000000000000000000 ) ) ;
#60380 = EDGE_CURVE ( 'NONE', #17866, #9016, #14613, .T. ) ;
#60381 = VECTOR ( 'NONE', #63376, 1000.000000000000000 ) ;
#60382 = VERTEX_POINT ( 'NONE', #10707 ) ;
#60383 = CARTESIAN_POINT ( 'NONE',  ( 181.4833316329832940, 5.000000000000000000, 316.5239988703752942 ) ) ;
#60384 = CARTESIAN_POINT ( 'NONE',  ( 4.740315990920143108, 4.188533722949256521, 195.0000000000000284 ) ) ;
#60385 = FACE_OUTER_BOUND ( 'NONE', #56422, .T. ) ;
#60386 = DIRECTION ( 'NONE',  ( 1.000000000000000000, 2.135044278125301343E-15, -0.000000000000000000 ) ) ;
#60387 = CARTESIAN_POINT ( 'NONE',  ( 6.849523737882817542, -10.50702373788281463, 26.00000000000000000 ) ) ;
#60388 = LINE ( 'NONE', #16930, #43307 ) ;
#60389 = VECTOR ( 'NONE', #395, 1000.000000000000114 ) ;
#60390 = VECTOR ( 'NONE', #67574, 1000.000000000000114 ) ;
#60391 = EDGE_LOOP ( 'NONE', ( #17383, #47254, #54594, #25761 ) ) ;
#60392 = AXIS2_PLACEMENT_3D ( 'NONE', #15587, #26528, #42435 ) ;
#60393 = DIRECTION ( 'NONE',  ( 0.000000000000000000, 0.000000000000000000, 1.000000000000000000 ) ) ;
#60394 = EDGE_CURVE ( 'NONE', #34404, #18663, #22018, .T. ) ;
#60395 = ORIENTED_EDGE ( 'NONE', *, *, #22383, .F. ) ;
#60396 = DIRECTION ( 'NONE',  ( 1.000000000000000000, -3.491481338843133355E-15, -1.836970198721036344E-16 ) ) ;
#60397 = VECTOR ( 'NONE', #10870, 1000.000000000000000 ) ;
#60398 = VECTOR ( 'NONE', #38838, 1000.000000000000000 ) ;
#60399 = EDGE_CURVE ( 'NONE', #44650, #60071, #7388, .T. ) ;
#60400 = CARTESIAN_POINT ( 'NONE',  ( -11.07551654964677290, -10.20488345035332500, 195.0000000000000284 ) ) ;
#60401 = VECTOR ( 'NONE', #3650, 1000.000000000000000 ) ;
#60402 = FACE_OUTER_BOUND ( 'NONE', #12184, .T. ) ;
#60403 = VERTEX_POINT ( 'NONE', #38290 ) ;
#60404 = ORIENTED_EDGE ( 'NONE', *, *, #61407, .T. ) ;
#60405 = LINE ( 'NONE', #66057, #18150 ) ;
#60406 = VERTEX_POINT ( 'NONE', #65835 ) ;
#60407 = EDGE_CURVE ( 'NONE', #62060, #60909, #27330, .T. ) ;
#60408 = ORIENTED_EDGE ( 'NONE', *, *, #1661, .F. ) ;
#60409 = DIRECTION ( 'NONE',  ( 0.000000000000000000, -0.000000000000000000, 1.000000000000000000 ) ) ;
#60410 = CARTESIAN_POINT ( 'NONE',  ( 283.0000000000000568, -40.30000000000000426, -8.900000000000000355 ) ) ;
#60411 = VECTOR ( 'NONE', #30648, 1000.000000000000000 ) ;
#60412 = DIRECTION ( 'NONE',  ( 1.000000000000000000, 0.000000000000000000, 0.000000000000000000 ) ) ;
#60413 = ORIENTED_EDGE ( 'NONE', *, *, #2413, .F. ) ;
#60414 = MECHANICAL_DESIGN_GEOMETRIC_PRESENTATION_REPRESENTATION (  '', ( #59271 ), #57041 ) ;
#60415 = DIRECTION ( 'NONE',  ( 0.000000000000000000, 0.000000000000000000, 1.000000000000000000 ) ) ;
#60417 = CARTESIAN_POINT ( 'NONE',  ( 25.90000000000000213, 0.000000000000000000, 0.000000000000000000 ) ) ;
#60416 = DIRECTION ( 'NONE',  ( 0.000000000000000000, 0.000000000000000000, 1.000000000000000000 ) ) ;
#60418 = VERTEX_POINT ( 'NONE', #5430 ) ;
#60420 = ORIENTED_EDGE ( 'NONE', *, *, #68697, .F. ) ;
#60419 = CARTESIAN_POINT ( 'NONE',  ( -1.466476262117230034, 9.390476262117152473, 26.00000000000000711 ) ) ;
#60421 = ORIENTED_EDGE ( 'NONE', *, *, #67789, .T. ) ;
#60422 = DIRECTION ( 'NONE',  ( 1.000000000000000000, 0.000000000000000000, 0.000000000000000000 ) ) ;
#60423 = EDGE_CURVE ( 'NONE', #18487, #31408, #32280, .T. ) ;
#60424 = FACE_OUTER_BOUND ( 'NONE', #12820, .T. ) ;
#60425 = LINE ( 'NONE', #12323, #60749 ) ;
#60426 = ORIENTED_EDGE ( 'NONE', *, *, #36622, .F. ) ;
#60427 = EDGE_CURVE ( 'NONE', #61728, #56196, #55957, .T. ) ;
#60428 = ORIENTED_EDGE ( 'NONE', *, *, #29069, .T. ) ;
#60429 = EDGE_CURVE ( 'NONE', #48626, #18593, #60501, .T. ) ;
#60430 = CYLINDRICAL_SURFACE ( 'NONE', #61754, 3.500000000000003109 ) ;
#60431 = DIRECTION ( 'NONE',  ( 0.5773502691896256200, 0.5773502691896259531, 0.5773502691896256200 ) ) ;
#60432 = EDGE_CURVE ( 'NONE', #2395, #17328, #16722, .T. ) ;
#60433 = VECTOR ( 'NONE', #5809, 1000.000000000000000 ) ;
#60434 = EDGE_CURVE ( 'NONE', #25825, #35692, #59841, .T. ) ;
#60435 = ADVANCED_FACE ( 'NONE', ( #32971, #53863 ), #37941, .F. ) ;
#60436 = EDGE_LOOP ( 'NONE', ( #25929, #12291, #53192, #56852 ) ) ;
#60437 = CARTESIAN_POINT ( 'NONE',  ( 7.250000000000004441, 7.450000000000001954, -13.50000000000000178 ) ) ;
#60438 = DIRECTION ( 'NONE',  ( -1.000000000000000000, 0.000000000000000000, 0.000000000000000000 ) ) ;
#60439 = CIRCLE ( 'NONE', #31264, 1.000000000000000000 ) ;
#60440 = DIRECTION ( 'NONE',  ( 1.000000000000000000, -7.808916176531286882E-15, -2.868949260119708725E-30 ) ) ;
#60441 = VERTEX_POINT ( 'NONE', #26983 ) ;
#60442 = EDGE_CURVE ( 'NONE', #8699, #18454, #68442, .T. ) ;
#60443 = CIRCLE ( 'NONE', #32250, 0.5000000000009302559 ) ;
#60444 = VECTOR ( 'NONE', #66722, 1000.000000000000000 ) ;
#60445 = VECTOR ( 'NONE', #4536, 1000.000000000000000 ) ;
#60446 = CARTESIAN_POINT ( 'NONE',  ( 4.396432944014527777, -8.406483450353478659, 455.0000000000000568 ) ) ;
#60447 = EDGE_CURVE ( 'NONE', #16870, #19628, #48541, .T. ) ;
#60448 = LINE ( 'NONE', #43849, #14777 ) ;
#60450 = ORIENTED_EDGE ( 'NONE', *, *, #68591, .T. ) ;
#60449 =( NAMED_UNIT ( * ) PLANE_ANGLE_UNIT ( ) SI_UNIT ( $, .RADIAN. ) );
#60452 = ORIENTED_EDGE ( 'NONE', *, *, #57023, .F. ) ;
#60451 = CARTESIAN_POINT ( 'NONE',  ( -6.822336235477446387, 4.135079735113102117, 54.00000000000000711 ) ) ;
#60453 = EDGE_CURVE ( 'NONE', #36902, #58100, #22373, .T. ) ;
#60454 = LINE ( 'NONE', #17675, #59609 ) ;
#60455 = STYLED_ITEM ( 'NONE', ( #56680 ), #67577 ) ;
#60456 = DIRECTION ( 'NONE',  ( -1.000000000000000000, 0.000000000000000000, 0.000000000000000000 ) ) ;
#60457 = FACE_OUTER_BOUND ( 'NONE', #10700, .T. ) ;
#60458 = DIRECTION ( 'NONE',  ( -1.000000000000000000, 0.000000000000000000, 0.000000000000000000 ) ) ;
#60459 = CARTESIAN_POINT ( 'NONE',  ( 15.90000000000000036, 0.000000000000000000, 8.619743980008982554E-16 ) ) ;
#60460 = AXIS2_PLACEMENT_3D ( 'NONE', #19302, #45119, #18964 ) ;
#60461 = DIRECTION ( 'NONE',  ( -1.260948829465469904E-14, -1.000000000000000000, -1.836970198721033632E-16 ) ) ;
#60462 = EDGE_CURVE ( 'NONE', #42050, #20416, #42881, .T. ) ;
#60463 = ORIENTED_EDGE ( 'NONE', *, *, #53325, .F. ) ;
#60464 = CARTESIAN_POINT ( 'NONE',  ( 275.0000000000000000, -27.13000000000000611, 15.49999999999930012 ) ) ;
#60466 = ADVANCED_FACE ( 'NONE', ( #38628 ), #5060, .F. ) ;
#60465 = DIRECTION ( 'NONE',  ( 1.000000000000000000, -0.000000000000000000, -0.000000000000000000 ) ) ;
#60468 = ORIENTED_EDGE ( 'NONE', *, *, #31977, .T. ) ;
#60467 = CARTESIAN_POINT ( 'NONE',  ( 11.32648345035337734, -7.606483450353397124, 195.0000000000000284 ) ) ;
#60469 = VECTOR ( 'NONE', #64500, 1000.000000000000000 ) ;
#60470 = DIRECTION ( 'NONE',  ( 1.836970198721029934E-16, 1.836970198721010706E-16, -1.000000000000000000 ) ) ;
#60471 = CIRCLE ( 'NONE', #49183, 1.224999999999998757 ) ;
#60472 = DIRECTION ( 'NONE',  ( -1.000000000000000000, 0.000000000000000000, 0.000000000000000000 ) ) ;
#60473 = ORIENTED_EDGE ( 'NONE', *, *, #65625, .T. ) ;
#60474 = CARTESIAN_POINT ( 'NONE',  ( 10.62249899919925866, -21.00000000000000000, 17.50000000000000000 ) ) ;
#60475 = CARTESIAN_POINT ( 'NONE',  ( 46.39999999999999858, 33.00000000000000000, 0.7500000000000000000 ) ) ;
#60476 = EDGE_CURVE ( 'NONE', #67341, #59636, #45812, .T. ) ;
#60477 = ORIENTED_EDGE ( 'NONE', *, *, #54809, .F. ) ;
#60478 = DIRECTION ( 'NONE',  ( 1.000000000000000000, 0.000000000000000000, 0.000000000000000000 ) ) ;
#60479 = CARTESIAN_POINT ( 'NONE',  ( -6.331612867284154511, 8.393516549646601987, 195.0000000000000284 ) ) ;
#60480 = FACE_OUTER_BOUND ( 'NONE', #16368, .T. ) ;
#60481 = LINE ( 'NONE', #17705, #16158 ) ;
#60482 = ORIENTED_EDGE ( 'NONE', *, *, #5561, .F. ) ;
#60483 = CARTESIAN_POINT ( 'NONE',  ( -8.393516549646712122, 6.331612867284047041, 455.0000000000000568 ) ) ;
#60484 = ORIENTED_EDGE ( 'NONE', *, *, #57820, .F. ) ;
#60485 = AXIS2_PLACEMENT_3D ( 'NONE', #9417, #68817, #64564 ) ;
#60486 = VERTEX_POINT ( 'NONE', #37246 ) ;
#60487 = DIRECTION ( 'NONE',  ( -1.000000000000000000, 0.000000000000000000, 0.000000000000000000 ) ) ;
#60488 = DIRECTION ( 'NONE',  ( 0.000000000000000000, 0.000000000000000000, -1.000000000000000000 ) ) ;
#60489 = VECTOR ( 'NONE', #23961, 1000.000000000000000 ) ;
#60490 = EDGE_CURVE ( 'NONE', #28651, #36435, #6301, .T. ) ;
#60491 = PLANE ( 'NONE',  #37765 ) ;
#60492 = LINE ( 'NONE', #52246, #10355 ) ;
#60493 = ORIENTED_EDGE ( 'NONE', *, *, #32241, .T. ) ;
#60494 = ORIENTED_EDGE ( 'NONE', *, *, #53426, .T. ) ;
#60496 = ORIENTED_EDGE ( 'NONE', *, *, #13414, .F. ) ;
#60495 = DIRECTION ( 'NONE',  ( 0.000000000000000000, 0.000000000000000000, -1.000000000000000000 ) ) ;
#60497 = EDGE_LOOP ( 'NONE', ( #11670, #35537, #8862, #30672 ) ) ;
#60498 = EDGE_CURVE ( 'NONE', #42074, #41827, #26631, .T. ) ;
#60499 = AXIS2_PLACEMENT_3D ( 'NONE', #37946, #15683, #43237 ) ;
#60500 = VECTOR ( 'NONE', #41785, 1000.000000000000000 ) ;
#60501 = CIRCLE ( 'NONE', #42446, 1.000000000000000888 ) ;
#60502 = CARTESIAN_POINT ( 'NONE',  ( -9.791916549646712653, 10.19191654964664018, 455.0000000000000568 ) ) ;
#60503 = CARTESIAN_POINT ( 'NONE',  ( -11.77351654964669336, -4.186483450353275515, 195.0000000000000284 ) ) ;
#60504 = CARTESIAN_POINT ( 'NONE',  ( -8.566576262117260754, 8.916576262117214213, 54.00000000000000711 ) ) ;
#60505 = EDGE_CURVE ( 'NONE', #53865, #50705, #36807, .T. ) ;
#60506 = AXIS2_PLACEMENT_3D ( 'NONE', #52194, #30287, #51852 ) ;
#60507 = AXIS2_PLACEMENT_3D ( 'NONE', #56157, #8043, #2402 ) ;
#60508 = VECTOR ( 'NONE', #44239, 1000.000000000000114 ) ;
#60510 = DIRECTION ( 'NONE',  ( -0.000000000000000000, -0.000000000000000000, -1.000000000000000000 ) ) ;
#60509 = PLANE ( 'NONE',  #41145 ) ;
#60511 = ORIENTED_EDGE ( 'NONE', *, *, #60205, .F. ) ;
#60512 = ADVANCED_FACE ( 'NONE', ( #67222 ), #18415, .T. ) ;
#60514 = ORIENTED_EDGE ( 'NONE', *, *, #1288, .F. ) ;
#60513 = CARTESIAN_POINT ( 'NONE',  ( 27.00000000000000000, 0.000000000000000000, -2.458500000000000796 ) ) ;
#60515 = ORIENTED_EDGE ( 'NONE', *, *, #41851, .T. ) ;
#60516 = ORIENTED_EDGE ( 'NONE', *, *, #63197, .T. ) ;
#60517 = CIRCLE ( 'NONE', #41332, 0.3999999999993817390 ) ;
#60518 = EDGE_CURVE ( 'NONE', #39018, #66073, #55574, .T. ) ;
#60519 = CARTESIAN_POINT ( 'NONE',  ( 41.09999999999999432, 20.60000000000000142, -13.86939075806900057 ) ) ;
#60520 = COLOUR_RGB ( '', 0.72549020, 0.75294118, 0.79215686) ;
#60521 = DIRECTION ( 'NONE',  ( 1.000000000000000000, -0.000000000000000000, 0.000000000000000000 ) ) ;
#60522 = DIRECTION ( 'NONE',  ( -1.000000000000000000, 1.254221251785257731E-14, 1.836970198721053107E-16 ) ) ;
#60523 = ORIENTED_EDGE ( 'NONE', *, *, #10437, .F. ) ;
#60524 = ORIENTED_EDGE ( 'NONE', *, *, #32301, .T. ) ;
#60525 = VECTOR ( 'NONE', #8450, 1000.000000000000000 ) ;
#60526 = CARTESIAN_POINT ( 'NONE',  ( 36.90000000000000568, 0.000000000000000000, 3.016910393003143647E-15 ) ) ;
#60527 = CARTESIAN_POINT ( 'NONE',  ( -3.650476262117221093, 10.49297626211717116, 54.00000000000000711 ) ) ;
#60528 = ORIENTED_EDGE ( 'NONE', *, *, #62482, .T. ) ;
#60529 = EDGE_CURVE ( 'NONE', #9740, #12989, #33659, .T. ) ;
#60530 = ORIENTED_EDGE ( 'NONE', *, *, #30172, .F. ) ;
#60531 = CARTESIAN_POINT ( 'NONE',  ( 41.09999999999999432, -21.00000000000000000, 13.86939075806900057 ) ) ;
#60532 = DIRECTION ( 'NONE',  ( -1.836970198721029934E-16, 1.836970198721036344E-16, -1.000000000000000000 ) ) ;
#60533 = ORIENTED_EDGE ( 'NONE', *, *, #10802, .F. ) ;
#60534 = CARTESIAN_POINT ( 'NONE',  ( -6.606374702650259501, -7.265214908726163046, 455.0000000000000568 ) ) ;
#60535 = AXIS2_PLACEMENT_3D ( 'NONE', #64838, #22044, #16048 ) ;
#60537 = ORIENTED_EDGE ( 'NONE', *, *, #57617, .T. ) ;
#60536 = CARTESIAN_POINT ( 'NONE',  ( -10.19191654964671301, 9.791916549646639822, 455.0000000000000568 ) ) ;
#60538 = VERTEX_POINT ( 'NONE', #12082 ) ;
#60539 = CARTESIAN_POINT ( 'NONE',  ( -4.734785091273957747, 5.380658396643156038, 455.0000000000000568 ) ) ;
#60540 = DIRECTION ( 'NONE',  ( 0.000000000000000000, -0.7071067811865460184, -0.7071067811865489050 ) ) ;
#60541 = CIRCLE ( 'NONE', #39093, 3.499999999999056310 ) ;
#60542 = LINE ( 'NONE', #17404, #8029 ) ;
#60543 = CARTESIAN_POINT ( 'NONE',  ( -9.722976262117237312, 7.605476262117214503, 26.00000000000000711 ) ) ;
#60544 = DIRECTION ( 'NONE',  ( -1.000000000000000000, 0.000000000000000000, 0.000000000000000000 ) ) ;
#60545 = FACE_OUTER_BOUND ( 'NONE', #24107, .T. ) ;
#60546 = VECTOR ( 'NONE', #49298, 1000.000000000000000 ) ;
#60547 = EDGE_CURVE ( 'NONE', #22546, #45122, #2866, .T. ) ;
#60548 = ORIENTED_EDGE ( 'NONE', *, *, #65195, .F. ) ;
#60549 = CARTESIAN_POINT ( 'NONE',  ( 10.50000000000000178, 9.690000000000001279, 0.000000000000000000 ) ) ;
#60551 = ORIENTED_EDGE ( 'NONE', *, *, #46094, .T. ) ;
#60550 = EDGE_CURVE ( 'NONE', #17050, #1369, #24082, .T. ) ;
#60552 = AXIS2_PLACEMENT_3D ( 'NONE', #52472, #25608, #47171 ) ;
#60553 = AXIS2_PLACEMENT_3D ( 'NONE', #68314, #68675, #14928 ) ;
#60555 = DIRECTION ( 'NONE',  ( 0.000000000000000000, -1.000000000000000000, 0.000000000000000000 ) ) ;
#60554 = VECTOR ( 'NONE', #26541, 1000.000000000000000 ) ;
#60556 = LINE ( 'NONE', #139, #10885 ) ;
#60557 = CARTESIAN_POINT ( 'NONE',  ( 30.00000000000000000, -5.200000000000001066, 26.25000000000000000 ) ) ;
#60558 = DIRECTION ( 'NONE',  ( 0.000000000000000000, 1.000000000000000000, 0.000000000000000000 ) ) ;
#60559 = AXIS2_PLACEMENT_3D ( 'NONE', #5783, #32300, #59523 ) ;
#60560 = AXIS2_PLACEMENT_3D ( 'NONE', #23539, #18577, #23191 ) ;
#60561 = CIRCLE ( 'NONE', #1806, 0.3500000000009988455 ) ;
#60562 = FACE_OUTER_BOUND ( 'NONE', #57115, .T. ) ;
#60563 = ORIENTED_EDGE ( 'NONE', *, *, #24043, .F. ) ;
#60564 = ORIENTED_EDGE ( 'NONE', *, *, #3887, .T. ) ;
#60565 = VECTOR ( 'NONE', #37509, 1000.000000000000000 ) ;
#60566 = DIRECTION ( 'NONE',  ( 1.000000000000000000, 2.135044278125301343E-15, -0.000000000000000000 ) ) ;
#60567 = DIRECTION ( 'NONE',  ( 0.000000000000000000, 0.000000000000000000, -1.000000000000000000 ) ) ;
#60568 = VECTOR ( 'NONE', #10033, 1000.000000000000000 ) ;
#60569 = VERTEX_POINT ( 'NONE', #55918 ) ;
#60570 = DIRECTION ( 'NONE',  ( -0.6414496315691420314, 0.7671651518153128624, 2.587583378555127804E-16 ) ) ;
#60571 = VERTEX_POINT ( 'NONE', #46005 ) ;
#60572 = ORIENTED_EDGE ( 'NONE', *, *, #34163, .T. ) ;
#60573 = DIRECTION ( 'NONE',  ( 0.000000000000000000, 1.000000000000000000, 0.000000000000000000 ) ) ;
#60574 = LINE ( 'NONE', #66233, #16178 ) ;
#60575 = ORIENTED_EDGE ( 'NONE', *, *, #54644, .T. ) ;
#60576 = LINE ( 'NONE', #55285, #52536 ) ;
#60577 = CARTESIAN_POINT ( 'NONE',  ( 30.00000000000000000, -13.79999999999979998, 17.30000000000000071 ) ) ;
#60578 = CARTESIAN_POINT ( 'NONE',  ( 9.912023737882782015, 3.667976262117150998, 54.00000000000000711 ) ) ;
#60579 = CYLINDRICAL_SURFACE ( 'NONE', #39642, 0.3999999999999993006 ) ;
#60580 = ORIENTED_EDGE ( 'NONE', *, *, #46564, .F. ) ;
#60582 = EDGE_LOOP ( 'NONE', ( #47465, #68025, #11879, #60766 ) ) ;
#60581 = FACE_OUTER_BOUND ( 'NONE', #34683, .T. ) ;
#60583 = ADVANCED_FACE ( 'NONE', ( #61202 ), #61916, .F. ) ;
#60584 = CARTESIAN_POINT ( 'NONE',  ( 24.00000000000000000, -17.50000000000000000, -19.33772233983200195 ) ) ;
#60585 = DIRECTION ( 'NONE',  ( -1.000000000000000000, 0.000000000000000000, 0.000000000000000000 ) ) ;
#60586 = DIRECTION ( 'NONE',  ( 0.000000000000000000, 0.000000000000000000, -1.000000000000000000 ) ) ;
#60587 = CARTESIAN_POINT ( 'NONE',  ( -1.077516549646676092, 10.73351654964656454, 455.0000000000000568 ) ) ;
#60588 = ORIENTED_EDGE ( 'NONE', *, *, #5698, .T. ) ;
#60589 = VECTOR ( 'NONE', #64747, 1000.000000000000000 ) ;
#60590 = EDGE_CURVE ( 'NONE', #54499, #63139, #15348, .T. ) ;
#60591 = DIRECTION ( 'NONE',  ( -1.000000000000000000, 0.000000000000000000, 0.000000000000000000 ) ) ;
#60592 = CARTESIAN_POINT ( 'NONE',  ( 51.65933123007250316, 4.485835665191191701, 7.173814858237198427E-17 ) ) ;
#60593 = AXIS2_PLACEMENT_3D ( 'NONE', #63037, #30859, #14592 ) ;
#60594 = EDGE_CURVE ( 'NONE', #62987, #65652, #38862, .T. ) ;
#60595 = VERTEX_POINT ( 'NONE', #50263 ) ;
#60596 = EDGE_LOOP ( 'NONE', ( #40245, #34674 ) ) ;
#60597 = EDGE_CURVE ( 'NONE', #15946, #62916, #56612, .T. ) ;
#60598 = VECTOR ( 'NONE', #33926, 1000.000000000000000 ) ;
#60599 = VECTOR ( 'NONE', #55926, 1000.000000000000114 ) ;
#60600 = ORIENTED_EDGE ( 'NONE', *, *, #50287, .T. ) ;
#60601 = DIRECTION ( 'NONE',  ( -0.5000000000000004441, 0.8660254037844383745, 3.181725716174720005E-16 ) ) ;
#60602 = EDGE_CURVE ( 'NONE', #17661, #5817, #34686, .T. ) ;
#60603 = EDGE_CURVE ( 'NONE', #14932, #40754, #1823, .T. ) ;
#60604 = CARTESIAN_POINT ( 'NONE',  ( 6.789561617636943325, -7.408280051175178293, 54.00000000000000711 ) ) ;
#60605 = DIRECTION ( 'NONE',  ( 1.836970198721029934E-16, 1.836970198721010706E-16, -1.000000000000000000 ) ) ;
#60606 = VECTOR ( 'NONE', #43004, 1000.000000000000000 ) ;
#60607 = AXIS2_PLACEMENT_3D ( 'NONE', #26461, #16544, #53686 ) ;
#60608 = EDGE_CURVE ( 'NONE', #60107, #4446, #34327, .T. ) ;
#60609 = ORIENTED_EDGE ( 'NONE', *, *, #39987, .T. ) ;
#60610 = ORIENTED_EDGE ( 'NONE', *, *, #23485, .F. ) ;
#60611 = ORIENTED_EDGE ( 'NONE', *, *, #64810, .T. ) ;
#60612 = CARTESIAN_POINT ( 'NONE',  ( 2.706483450353350584, -10.09643294401453595, 195.0000000000000284 ) ) ;
#60613 = VECTOR ( 'NONE', #31181, 1000.000000000000000 ) ;
#60614 = AXIS2_PLACEMENT_3D ( 'NONE', #3048, #31335, #52902 ) ;
#60615 = ORIENTED_EDGE ( 'NONE', *, *, #37981, .T. ) ;
#60616 = ORIENTED_EDGE ( 'NONE', *, *, #54058, .F. ) ;
#60617 = ORIENTED_EDGE ( 'NONE', *, *, #66230, .T. ) ;
#60618 = ORIENTED_EDGE ( 'NONE', *, *, #60038, .F. ) ;
#60619 = CARTESIAN_POINT ( 'NONE',  ( -4.135079735113166954, 3.663616288757006512, 26.00000000000000711 ) ) ;
#60621 = ORIENTED_EDGE ( 'NONE', *, *, #59726, .T. ) ;
#60620 = CARTESIAN_POINT ( 'NONE',  ( 7.826483450353380000, -12.00648345035349251, 455.0000000000000568 ) ) ;
#60622 = FACE_OUTER_BOUND ( 'NONE', #28481, .T. ) ;
#60623 = PRODUCT_DEFINITION_SHAPE ( 'NONE', 'NONE',  #69989 ) ;
#60624 = VECTOR ( 'NONE', #49851, 1000.000000000000000 ) ;
#60625 = CARTESIAN_POINT ( 'NONE',  ( -11.00000000000000000, -10.85999999999999943, -9.000000000000001776 ) ) ;
#60626 = CARTESIAN_POINT ( 'NONE',  ( -6.350872789121327244, 3.663616288756986084, 26.00000000000000711 ) ) ;
#60627 = EDGE_LOOP ( 'NONE', ( #48770, #5864, #10251, #68709 ) ) ;
#60628 = DIRECTION ( 'NONE',  ( -1.000000000000000000, 0.000000000000000000, 0.000000000000000000 ) ) ;
#60629 = DIRECTION ( 'NONE',  ( 1.000000000000000000, 0.000000000000000000, 0.000000000000000000 ) ) ;
#60630 = DIRECTION ( 'NONE',  ( 0.000000000000000000, 0.000000000000000000, -1.000000000000000000 ) ) ;
#60631 = ORIENTED_EDGE ( 'NONE', *, *, #58515, .T. ) ;
#60632 = CARTESIAN_POINT ( 'NONE',  ( 40.90000000000000568, -16.96999999999999886, -21.00000000000000000 ) ) ;
#60633 = EDGE_CURVE ( 'NONE', #41307, #37678, #66182, .T. ) ;
#60634 = CARTESIAN_POINT ( 'NONE',  ( 11.75000000000000000, -5.000000000000000000, 11.75000000000000000 ) ) ;
#60635 = DIRECTION ( 'NONE',  ( 0.000000000000000000, 0.000000000000000000, -1.000000000000000000 ) ) ;
#60636 = VECTOR ( 'NONE', #25090, 1000.000000000000000 ) ;
#60637 = ORIENTED_EDGE ( 'NONE', *, *, #33808, .T. ) ;
#60638 = ADVANCED_FACE ( 'NONE', ( #8165 ), #50615, .F. ) ;
#60639 = DIRECTION ( 'NONE',  ( 0.000000000000000000, 0.000000000000000000, -1.000000000000000000 ) ) ;
#60640 = EDGE_CURVE ( 'NONE', #47184, #55467, #26656, .T. ) ;
#60641 = CARTESIAN_POINT ( 'NONE',  ( 2.369523737882811787, 9.547976262117209956, 26.00000000000000711 ) ) ;
#60642 = LINE ( 'NONE', #50377, #47214 ) ;
#60643 = EDGE_CURVE ( 'NONE', #9302, #42510, #7814, .T. ) ;
#60644 = ORIENTED_EDGE ( 'NONE', *, *, #31555, .T. ) ;
#60645 = CIRCLE ( 'NONE', #31353, 4.500000000000191847 ) ;
#60646 = VECTOR ( 'NONE', #63534, 1000.000000000000000 ) ;
#60647 = AXIS2_PLACEMENT_3D ( 'NONE', #12604, #18613, #34521 ) ;
#60648 = FACE_OUTER_BOUND ( 'NONE', #54802, .T. ) ;
#60649 = DIRECTION ( 'NONE',  ( -0.000000000000000000, 1.000000000000000000, -0.000000000000000000 ) ) ;
#60650 = CARTESIAN_POINT ( 'NONE',  ( -6.467976262117258734, 5.242976262117182706, 54.00000000000000711 ) ) ;
#60651 = DIRECTION ( 'NONE',  ( 0.000000000000000000, 0.000000000000000000, 1.000000000000000000 ) ) ;
#60652 = CYLINDRICAL_SURFACE ( 'NONE', #33411, 0.1749999999999980738 ) ;
#60653 = AXIS2_PLACEMENT_3D ( 'NONE', #4120, #69153, #20711 ) ;
#60654 =( GEOMETRIC_REPRESENTATION_CONTEXT ( 3 ) GLOBAL_UNCERTAINTY_ASSIGNED_CONTEXT ( ( #33053 ) ) GLOBAL_UNIT_ASSIGNED_CONTEXT ( ( #41824, #3652, #63755 ) ) REPRESENTATION_CONTEXT ( 'NONE', 'WORKASPACE' ) );
#60655 = ORIENTED_EDGE ( 'NONE', *, *, #13190, .T. ) ;
#60656 = DIRECTION ( 'NONE',  ( 0.000000000000000000, 0.000000000000000000, -1.000000000000000000 ) ) ;
#60657 = CARTESIAN_POINT ( 'NONE',  ( 275.0000000000000000, -26.28355339059299922, 9.766446609406699508 ) ) ;
#60658 = CARTESIAN_POINT ( 'NONE',  ( -7.603567055985545942, 8.393516549646601987, 195.0000000000000284 ) ) ;
#60659 = VECTOR ( 'NONE', #22481, 1000.000000000000000 ) ;
#60660 = CARTESIAN_POINT ( 'NONE',  ( 9.689999999999999503, -10.50000000000000178, 0.000000000000000000 ) ) ;
#60661 = CIRCLE ( 'NONE', #49377, 5.000000000000000000 ) ;
#60662 = CARTESIAN_POINT ( 'NONE',  ( 11.48848345035334617, -10.20488345035352928, 455.0000000000000568 ) ) ;
#60663 = VERTEX_POINT ( 'NONE', #45639 ) ;
#60664 = CARTESIAN_POINT ( 'NONE',  ( -8.250000000000001776, 0.000000000000000000, -15.50000000000000000 ) ) ;
#60665 = DIRECTION ( 'NONE',  ( -0.000000000000000000, -0.000000000000000000, -1.000000000000000000 ) ) ;
#60666 = PLANE ( 'NONE',  #40137 ) ;
#60667 = CARTESIAN_POINT ( 'NONE',  ( 7.000000000000000000, -21.00000000000000000, 0.000000000000000000 ) ) ;
#60668 = CARTESIAN_POINT ( 'NONE',  ( 9.690000000000001279, 9.750000000000000000, -4.250000000000000000 ) ) ;
#60669 = ORIENTED_EDGE ( 'NONE', *, *, #19091, .F. ) ;
#60670 = VECTOR ( 'NONE', #1082, 1000.000000000000000 ) ;
#60671 = ADVANCED_FACE ( 'NONE', ( #29733 ), #30448, .T. ) ;
#60672 = DIRECTION ( 'NONE',  ( 0.000000000000000000, 1.000000000000000000, 0.000000000000000000 ) ) ;
#60673 = CARTESIAN_POINT ( 'NONE',  ( -7.250000000000001776, -7.249999999999998224, -16.00000000000000000 ) ) ;
#60674 = ORIENTED_EDGE ( 'NONE', *, *, #52524, .T. ) ;
#60675 = CARTESIAN_POINT ( 'NONE',  ( 25.50000000000000355, -5.200000000000001066, -22.50000000000000000 ) ) ;
#60676 = ORIENTED_EDGE ( 'NONE', *, *, #10519, .T. ) ;
#60677 = CARTESIAN_POINT ( 'NONE',  ( -2.355476262117320640, -9.562023737882825003, 26.00000000000000711 ) ) ;
#60678 = ORIENTED_EDGE ( 'NONE', *, *, #26974, .F. ) ;
#60679 = ORIENTED_EDGE ( 'NONE', *, *, #50464, .T. ) ;
#60680 = CARTESIAN_POINT ( 'NONE',  ( -2.693516549646827851, -10.92648345035345692, 455.0000000000000568 ) ) ;
#60681 = ADVANCED_FACE ( 'NONE', ( #62974 ), #14530, .F. ) ;
#60682 = DIRECTION ( 'NONE',  ( 0.000000000000000000, 0.000000000000000000, -1.000000000000000000 ) ) ;
#60683 = FACE_OUTER_BOUND ( 'NONE', #18382, .T. ) ;
#60684 = CARTESIAN_POINT ( 'NONE',  ( 283.0000000000000568, -31.30000000000000071, 8.400000000000000355 ) ) ;
#60685 = ADVANCED_FACE ( 'NONE', ( #62260 ), #3579, .F. ) ;
#60686 = VECTOR ( 'NONE', #13516, 1000.000000000000000 ) ;
#60687 = ORIENTED_EDGE ( 'NONE', *, *, #33224, .T. ) ;
#60688 = ORIENTED_EDGE ( 'NONE', *, *, #55040, .T. ) ;
#60689 = FACE_OUTER_BOUND ( 'NONE', #69242, .T. ) ;
#60690 = DIRECTION ( 'NONE',  ( 1.000000000000000000, 0.000000000000000000, 0.000000000000000000 ) ) ;
#60691 = VERTEX_POINT ( 'NONE', #9580 ) ;
#60692 = EDGE_LOOP ( 'NONE', ( #52416, #64489, #42265, #49415 ) ) ;
#60693 = EDGE_LOOP ( 'NONE', ( #2600, #50343, #27480, #65681 ) ) ;
#60694 = AXIS2_PLACEMENT_3D ( 'NONE', #20109, #4211, #14459 ) ;
#60695 = VECTOR ( 'NONE', #49364, 1000.000000000000000 ) ;
#60696 = CIRCLE ( 'NONE', #6508, 0.5249999999999994671 ) ;
#60697 = CARTESIAN_POINT ( 'NONE',  ( 49.00000000000000000, -21.00000000000000000, 13.86939075806900057 ) ) ;
#60698 = CARTESIAN_POINT ( 'NONE',  ( -6.350872789121319251, -3.677663764522589140, 54.00000000000000711 ) ) ;
#60700 = ORIENTED_EDGE ( 'NONE', *, *, #66491, .F. ) ;
#60699 = LINE ( 'NONE', #13298, #65407 ) ;
#60701 = AXIS2_PLACEMENT_3D ( 'NONE', #42846, #15982, #59112 ) ;
#60702 = VECTOR ( 'NONE', #10716, 1000.000000000000000 ) ;
#60703 = CARTESIAN_POINT ( 'NONE',  ( 8.000000000000000000, 7.281754163448145079, -1.000000000000000000 ) ) ;
#60704 = DIRECTION ( 'NONE',  ( 0.7142857142857395036, 0.000000000000000000, 0.6998542122237394469 ) ) ;
#60705 = EDGE_LOOP ( 'NONE', ( #4753, #5463, #38993, #49151 ) ) ;
#60706 = ORIENTED_EDGE ( 'NONE', *, *, #14348, .T. ) ;
#60707 = AXIS2_PLACEMENT_3D ( 'NONE', #49274, #5794, #38314 ) ;
#60708 = CARTESIAN_POINT ( 'NONE',  ( 11.18999999999999950, 11.18999999999999950, -5.000000000000000000 ) ) ;
#60709 = DIRECTION ( 'NONE',  ( -0.6414496315691698980, -0.7671651518152895477, -2.587583378555116957E-16 ) ) ;
#60710 = LINE ( 'NONE', #23223, #10056 ) ;
#60711 = AXIS2_PLACEMENT_3D ( 'NONE', #44794, #12610, #12262 ) ;
#60712 = DIRECTION ( 'NONE',  ( -1.000000000000000000, 0.000000000000000000, 0.000000000000000000 ) ) ;
#60713 = DIRECTION ( 'NONE',  ( -1.836970198721029934E-16, 1.836970198721036344E-16, -1.000000000000000000 ) ) ;
#60715 = VERTEX_POINT ( 'NONE', #9231 ) ;
#60714 = LINE ( 'NONE', #22550, #43315 ) ;
#60716 = ORIENTED_EDGE ( 'NONE', *, *, #60362, .F. ) ;
#60717 = ADVANCED_FACE ( 'NONE', ( #30797 ), #35742, .F. ) ;
#60718 = LINE ( 'NONE', #21853, #29446 ) ;
#60719 = CARTESIAN_POINT ( 'NONE',  ( 49.00000000000000000, 0.000000000000000000, 0.000000000000000000 ) ) ;
#60720 = CYLINDRICAL_SURFACE ( 'NONE', #20043, 4.000000000000000000 ) ;
#60721 = PLANE ( 'NONE',  #41899 ) ;
#60722 = EDGE_CURVE ( 'NONE', #43786, #1825, #41746, .T. ) ;
#60723 = CARTESIAN_POINT ( 'NONE',  ( 9.306483450353379538, -10.92648345035348534, 455.0000000000000568 ) ) ;
#60724 = EDGE_LOOP ( 'NONE', ( #30432, #7742, #3223, #61188 ) ) ;
#60725 = DIRECTION ( 'NONE',  ( -1.836970198721029934E-16, 1.836970198721036590E-16, -1.000000000000000000 ) ) ;
#60726 = CARTESIAN_POINT ( 'NONE',  ( 17.00000000000000000, -17.50000000000000000, 19.33772233983200195 ) ) ;
#60727 = DIRECTION ( 'NONE',  ( 1.836970198721029934E-16, 1.836970198721010706E-16, -1.000000000000000000 ) ) ;
#60728 = VECTOR ( 'NONE', #3617, 1000.000000000000000 ) ;
#60729 = DIRECTION ( 'NONE',  ( -1.000000000000000000, 0.000000000000000000, 0.000000000000000000 ) ) ;
#60730 = CARTESIAN_POINT ( 'NONE',  ( -24.00000000000000000, -15.50000000000000000, -19.33772233983200195 ) ) ;
#60731 = CARTESIAN_POINT ( 'NONE',  ( 0.9555237378827876604, -9.404523737882790613, 54.00000000000000711 ) ) ;
#60732 = EDGE_LOOP ( 'NONE', ( #4709, #45113, #3795, #66949 ) ) ;
#60733 = DIRECTION ( 'NONE',  ( 0.000000000000000000, -0.7071067811865475727, 0.7071067811865475727 ) ) ;
#60734 = DIRECTION ( 'NONE',  ( 0.000000000000000000, 0.000000000000000000, -1.000000000000000000 ) ) ;
#60735 = ORIENTED_EDGE ( 'NONE', *, *, #5356, .F. ) ;
#60736 = CARTESIAN_POINT ( 'NONE',  ( 1.090483450353343819, -10.74648345035335772, 195.0000000000000284 ) ) ;
#60737 = DIRECTION ( 'NONE',  ( -1.000000000000000000, 0.000000000000000000, 0.000000000000000000 ) ) ;
#60738 = DIRECTION ( 'NONE',  ( 1.334402673828312846E-16, 1.000000000000000000, 0.000000000000000000 ) ) ;
#60739 = EDGE_CURVE ( 'NONE', #38230, #67348, #20185, .T. ) ;
#60740 = CARTESIAN_POINT ( 'NONE',  ( 7.450000000000004619, -1.336933437520057563E-15, -11.00000000000000000 ) ) ;
#60741 = CARTESIAN_POINT ( 'NONE',  ( 9.690000000000001279, 8.750000000000000000, -7.000000000000000000 ) ) ;
#60742 = ORIENTED_EDGE ( 'NONE', *, *, #12930, .T. ) ;
#60743 = AXIS2_PLACEMENT_3D ( 'NONE', #16601, #59379, #331 ) ;
#60744 = LINE ( 'NONE', #1359, #11539 ) ;
#60745 = VERTEX_POINT ( 'NONE', #19828 ) ;
#60746 = DIRECTION ( 'NONE',  ( 0.000000000000000000, 1.000000000000000000, 0.000000000000000000 ) ) ;
#60747 = VERTEX_POINT ( 'NONE', #25143 ) ;
#60748 = CARTESIAN_POINT ( 'NONE',  ( -11.31351654964679021, -7.806483450353372433, 455.0000000000000568 ) ) ;
#60749 = VECTOR ( 'NONE', #43834, 1000.000000000000000 ) ;
#60750 = CIRCLE ( 'NONE', #36914, 2.458500000000000796 ) ;
#60751 = LINE ( 'NONE', #23274, #42350 ) ;
#60752 = LINE ( 'NONE', #12299, #28848 ) ;
#60753 = ORIENTED_EDGE ( 'NONE', *, *, #17652, .F. ) ;
#60754 = ORIENTED_EDGE ( 'NONE', *, *, #56597, .T. ) ;
#60755 = CARTESIAN_POINT ( 'NONE',  ( -11.00000000000000000, -5.599999999999999645, -9.000000000000001776 ) ) ;
#60756 = ORIENTED_EDGE ( 'NONE', *, *, #69077, .F. ) ;
#60757 = EDGE_LOOP ( 'NONE', ( #3494, #25217, #50780, #36976 ) ) ;
#60758 = EDGE_CURVE ( 'NONE', #57901, #4860, #14222, .T. ) ;
#60759 = CIRCLE ( 'NONE', #57390, 1.929199999999998916 ) ;
#60760 = PRODUCT_DEFINITION_CONTEXT ( 'detailed design', #39479, 'design' ) ;
#60761 = CARTESIAN_POINT ( 'NONE',  ( -7.603567055985637424, -8.606483450353410447, 455.0000000000000568 ) ) ;
#60762 = CARTESIAN_POINT ( 'NONE',  ( 7.811466277050743479, 4.727349090213326832, 455.0000000000000568 ) ) ;
#60763 = CARTESIAN_POINT ( 'NONE',  ( -9.390476262117209316, -1.480523737882732060, 54.00000000000000711 ) ) ;
#60764 = EDGE_CURVE ( 'NONE', #60323, #5255, #51472, .T. ) ;
#60765 = EDGE_CURVE ( 'NONE', #46144, #2815, #18701, .T. ) ;
#60766 = ORIENTED_EDGE ( 'NONE', *, *, #45631, .T. ) ;
#60767 = LINE ( 'NONE', #34924, #19882 ) ;
#60769 = CARTESIAN_POINT ( 'NONE',  ( 0.000000000000000000, 0.000000000000000000, -19.00000000000000000 ) ) ;
#60768 = DIRECTION ( 'NONE',  ( 0.000000000000000000, 1.000000000000000000, 0.000000000000000000 ) ) ;
#60770 = ORIENTED_EDGE ( 'NONE', *, *, #6103, .T. ) ;
#60773 = EDGE_LOOP ( 'NONE', ( #2208, #58266, #49117, #17194 ) ) ;
#60772 = ADVANCED_FACE ( 'NONE', ( #67582 ), #14888, .F. ) ;
#60771 = CARTESIAN_POINT ( 'NONE',  ( 4.155633711806658859, -4.720772854004808394, 54.00000000000000711 ) ) ;
#60774 = EDGE_LOOP ( 'NONE', ( #67113, #36784, #17500, #1392 ) ) ;
#60775 = DIRECTION ( 'NONE',  ( 1.000000000000000000, 0.000000000000000000, 0.000000000000000000 ) ) ;
#60776 = ADVANCED_FACE ( 'NONE', ( #57313 ), #68274, .F. ) ;
#60777 = EDGE_CURVE ( 'NONE', #16435, #28094, #32309, .T. ) ;
#60778 = DIRECTION ( 'NONE',  ( -1.000000000000000000, -0.000000000000000000, -0.000000000000000000 ) ) ;
#60779 = EDGE_CURVE ( 'NONE', #11224, #1993, #63683, .T. ) ;
#60780 = VERTEX_POINT ( 'NONE', #58015 ) ;
#60781 = DIRECTION ( 'NONE',  ( -1.000000000000000000, 0.000000000000000000, 0.000000000000000000 ) ) ;
#60782 = ORIENTED_EDGE ( 'NONE', *, *, #61834, .F. ) ;
#60783 = ORIENTED_EDGE ( 'NONE', *, *, #41904, .T. ) ;
#60784 = FACE_OUTER_BOUND ( 'NONE', #60391, .T. ) ;
#60785 = DIRECTION ( 'NONE',  ( 0.000000000000000000, 0.000000000000000000, 1.000000000000000000 ) ) ;
#60786 = ORIENTED_EDGE ( 'NONE', *, *, #33339, .T. ) ;
#60787 = DIRECTION ( 'NONE',  ( -1.000000000000000000, 0.000000000000000000, 0.000000000000000000 ) ) ;
#60788 = CARTESIAN_POINT ( 'NONE',  ( 8.900000000000005684, 20.60000000000000142, 13.86939075806899702 ) ) ;
#60789 = CARTESIAN_POINT ( 'NONE',  ( 0.000000000000000000, 0.000000000000000000, 0.000000000000000000 ) ) ;
#60790 = ORIENTED_EDGE ( 'NONE', *, *, #68385, .F. ) ;
#60791 = CIRCLE ( 'NONE', #40504, 0.2000000000000005107 ) ;
#60792 = DIRECTION ( 'NONE',  ( 8.728482790395504563E-15, 1.000000000000000000, 3.673940397442059868E-16 ) ) ;
#60793 = CARTESIAN_POINT ( 'NONE',  ( -9.942044687070568543, 2.752095193409294982, 455.0000000000000568 ) ) ;
#60795 = EDGE_LOOP ( 'NONE', ( #40325, #43930, #42608, #29615, #32795, #65533, #30921, #13579, #29424, #13168, #9627, #55113, #64606, #15314, #58467, #6541, #2142, #24729 ) ) ;
#60794 = FILL_AREA_STYLE_COLOUR ( '', #41975 ) ;
#60797 = ORIENTED_EDGE ( 'NONE', *, *, #6885, .T. ) ;
#60796 = PLANE ( 'NONE',  #9789 ) ;
#60798 = CARTESIAN_POINT ( 'NONE',  ( 30.00000000000000000, -14.33999999999999986, 14.50000000000000000 ) ) ;
#60799 = CIRCLE ( 'NONE', #44997, 0.9999999999999991118 ) ;
#60800 = CARTESIAN_POINT ( 'NONE',  ( -11.00000000000000000, -12.00000000000000000, -12.20000000000000107 ) ) ;
#60801 = DIRECTION ( 'NONE',  ( 0.4999999999999827360, 0.000000000000000000, 0.8660254037844485886 ) ) ;
#60802 = DIRECTION ( 'NONE',  ( -1.000000000000000000, 0.000000000000000000, 0.000000000000000000 ) ) ;
#60803 = CARTESIAN_POINT ( 'NONE',  ( 7.500000000000000000, -20.40000000000000213, -20.00000000000000000 ) ) ;
#60804 = ORIENTED_EDGE ( 'NONE', *, *, #6291, .F. ) ;
#60805 = DIRECTION ( 'NONE',  ( 0.000000000000000000, 1.000000000000000000, 0.000000000000000000 ) ) ;
#60806 = DIRECTION ( 'NONE',  ( 1.836970198721029934E-16, 1.836970198721010706E-16, -1.000000000000000000 ) ) ;
#60807 = SURFACE_STYLE_FILL_AREA ( #39247 ) ;
#60808 = VECTOR ( 'NONE', #42570, 1000.000000000000000 ) ;
#60810 = ORIENTED_EDGE ( 'NONE', *, *, #39808, .T. ) ;
#60809 = DIRECTION ( 'NONE',  ( 0.000000000000000000, 1.000000000000000000, 0.000000000000000000 ) ) ;
#60811 = CARTESIAN_POINT ( 'NONE',  ( 6.749999999999996447, -7.348062532928000934, 0.000000000000000000 ) ) ;
#60812 = DIRECTION ( 'NONE',  ( 1.000000000000000000, -8.339399738404102667E-15, 0.000000000000000000 ) ) ;
#60813 = EDGE_CURVE ( 'NONE', #7192, #33956, #68388, .T. ) ;
#60814 = ORIENTED_EDGE ( 'NONE', *, *, #21771, .F. ) ;
#60815 = DIRECTION ( 'NONE',  ( 0.000000000000000000, 0.000000000000000000, 1.000000000000000000 ) ) ;
#60816 = DIRECTION ( 'NONE',  ( 0.000000000000000000, -1.000000000000000000, 0.000000000000000000 ) ) ;
#60817 = ORIENTED_EDGE ( 'NONE', *, *, #27543, .T. ) ;
#60818 = DIRECTION ( 'NONE',  ( -1.000000000000000000, 0.000000000000000000, 0.000000000000000000 ) ) ;
#60819 = DIRECTION ( 'NONE',  ( 0.000000000000000000, -0.7071067811865474617, -0.7071067811865474617 ) ) ;
#60820 = FACE_OUTER_BOUND ( 'NONE', #18252, .T. ) ;
#60821 = EDGE_CURVE ( 'NONE', #10719, #50834, #31163, .T. ) ;
#60822 = DIRECTION ( 'NONE',  ( -1.000000000000000000, 8.339399738404101090E-15, -1.836970198721014896E-16 ) ) ;
#60823 = CARTESIAN_POINT ( 'NONE',  ( -9.689726262117330791, -10.05377373788272699, 54.00000000000000711 ) ) ;
#60824 = ORIENTED_EDGE ( 'NONE', *, *, #22186, .F. ) ;
#60825 = LINE ( 'NONE', #66824, #37318 ) ;
#60826 = VERTEX_POINT ( 'NONE', #68974 ) ;
#60827 = EDGE_CURVE ( 'NONE', #23822, #4107, #36860, .T. ) ;
#60828 = ORIENTED_EDGE ( 'NONE', *, *, #3804, .F. ) ;
#60829 = DIRECTION ( 'NONE',  ( 0.000000000000000000, 1.000000000000000000, 0.000000000000000000 ) ) ;
#60830 = DIRECTION ( 'NONE',  ( 0.6414496315691526895, 0.7671651518153038696, 2.587583378555111534E-16 ) ) ;
#60831 = EDGE_CURVE ( 'NONE', #21103, #51919, #6358, .T. ) ;
#60832 = CIRCLE ( 'NONE', #30364, 0.5250000000000003553 ) ;
#60833 = CARTESIAN_POINT ( 'NONE',  ( 7.811466277050727491, 7.259684009079840905, 195.0000000000000284 ) ) ;
#60834 = LINE ( 'NONE', #44927, #5852 ) ;
#60835 = EDGE_LOOP ( 'NONE', ( #42319, #9759, #49331, #9757 ) ) ;
#60836 = VERTEX_POINT ( 'NONE', #64377 ) ;
#60837 = FACE_OUTER_BOUND ( 'NONE', #10714, .T. ) ;
#60838 = ORIENTED_EDGE ( 'NONE', *, *, #47993, .T. ) ;
#60839 = VECTOR ( 'NONE', #18392, 1000.000000000000000 ) ;
#60840 = CYLINDRICAL_SURFACE ( 'NONE', #13450, 2.000000000000001776 ) ;
#60841 = DIRECTION ( 'NONE',  ( 2.478176394252584099E-15, 1.000000000000000000, 0.000000000000000000 ) ) ;
#60842 = EDGE_CURVE ( 'NONE', #18752, #53516, #21928, .T. ) ;
#60843 = DIRECTION ( 'NONE',  ( -1.836970198721029934E-16, 1.836970198721036590E-16, -1.000000000000000000 ) ) ;
#60844 = AXIS2_PLACEMENT_3D ( 'NONE', #32995, #4402, #48226 ) ;
#60845 = DIRECTION ( 'NONE',  ( -1.836970198721029934E-16, 1.836970198721036590E-16, -1.000000000000000000 ) ) ;
#60847 = CARTESIAN_POINT ( 'NONE',  ( -10.03972626211722918, 8.916576262117214213, 26.00000000000000711 ) ) ;
#60846 = CARTESIAN_POINT ( 'NONE',  ( 3.724485858128685045, 7.394232575409559693, 54.00000000000000711 ) ) ;
#60848 = VERTEX_POINT ( 'NONE', #43482 ) ;
#60850 = ORIENTED_EDGE ( 'NONE', *, *, #21381, .T. ) ;
#60849 = CARTESIAN_POINT ( 'NONE',  ( 9.690000000000001279, -9.750000000000001776, -7.000000000000000000 ) ) ;
#60851 = ORIENTED_EDGE ( 'NONE', *, *, #66650, .F. ) ;
#60852 = ORIENTED_EDGE ( 'NONE', *, *, #17026, .F. ) ;
#60853 = CIRCLE ( 'NONE', #26012, 0.1999999999999996503 ) ;
#60854 = EDGE_CURVE ( 'NONE', #18237, #46721, #15932, .T. ) ;
#60855 = CARTESIAN_POINT ( 'NONE',  ( -0.9414762621173243806, -9.929523737882846035, 26.00000000000000711 ) ) ;
#60856 = EDGE_CURVE ( 'NONE', #16696, #9744, #15600, .T. ) ;
#60858 = VECTOR ( 'NONE', #50446, 1000.000000000000000 ) ;
#60857 = CIRCLE ( 'NONE', #30387, 0.1999999999999987899 ) ;
#60859 = DIRECTION ( 'NONE',  ( -0.000000000000000000, -0.000000000000000000, -1.000000000000000000 ) ) ;
#60860 = PLANE ( 'NONE',  #43285 ) ;
#60861 = EDGE_LOOP ( 'NONE', ( #38275, #31279, #69129, #6893 ) ) ;
#60862 = ORIENTED_EDGE ( 'NONE', *, *, #5396, .F. ) ;
#60863 = VECTOR ( 'NONE', #47086, 1000.000000000000114 ) ;
#60864 = DIRECTION ( 'NONE',  ( -0.000000000000000000, -0.000000000000000000, 1.000000000000000000 ) ) ;
#60865 = DIRECTION ( 'NONE',  ( 1.000000000000000000, 0.000000000000000000, 0.000000000000000000 ) ) ;
#60866 = EDGE_CURVE ( 'NONE', #44584, #24243, #21245, .T. ) ;
#60867 = EDGE_LOOP ( 'NONE', ( #25661, #22013, #57286, #1698, #41634, #67632, #42964, #14700 ) ) ;
#60868 = ORIENTED_EDGE ( 'NONE', *, *, #8705, .F. ) ;
#60869 = FACE_OUTER_BOUND ( 'NONE', #66866, .T. ) ;
#60870 = DIRECTION ( 'NONE',  ( 0.000000000000000000, -1.000000000000000000, 0.000000000000000000 ) ) ;
#60871 = ORIENTED_EDGE ( 'NONE', *, *, #52684, .F. ) ;
#60872 = CARTESIAN_POINT ( 'NONE',  ( 8.250000000000005329, -7.249999999999998224, -26.00000000000001066 ) ) ;
#60873 = ORIENTED_EDGE ( 'NONE', *, *, #50905, .T. ) ;
#60874 = ORIENTED_EDGE ( 'NONE', *, *, #26377, .T. ) ;
#60875 = CARTESIAN_POINT ( 'NONE',  ( -11.99351654964674374, -4.186483450353318148, 455.0000000000000568 ) ) ;
#60876 = DIRECTION ( 'NONE',  ( -0.000000000000000000, 3.673940397442059868E-16, -1.000000000000000000 ) ) ;
#60877 = DIRECTION ( 'NONE',  ( 0.000000000000000000, 0.000000000000000000, 1.000000000000000000 ) ) ;
#60878 = PLANE ( 'NONE',  #50709 ) ;
#60879 = DIRECTION ( 'NONE',  ( 0.000000000000000000, 0.000000000000000000, -1.000000000000000000 ) ) ;
#60880 = AXIS2_PLACEMENT_3D ( 'NONE', #49534, #405, #21965 ) ;
#60881 = EDGE_CURVE ( 'NONE', #38679, #24526, #4974, .T. ) ;
#60882 = CARTESIAN_POINT ( 'NONE',  ( 7.450000000000004619, -1.336933437520057563E-15, -8.500000000000000000 ) ) ;
#60883 = ORIENTED_EDGE ( 'NONE', *, *, #65234, .F. ) ;
#60884 = DIRECTION ( 'NONE',  ( 0.000000000000000000, 0.000000000000000000, -1.000000000000000000 ) ) ;
#60885 = VECTOR ( 'NONE', #4615, 1000.000000000000000 ) ;
#60886 = EDGE_CURVE ( 'NONE', #46437, #42264, #16273, .T. ) ;
#60888 = VERTEX_POINT ( 'NONE', #11644 ) ;
#60887 = FACE_OUTER_BOUND ( 'NONE', #56533, .T. ) ;
#60889 = CARTESIAN_POINT ( 'NONE',  ( -11.00000000000000000, -5.200000000000001066, 60.00000000000000000 ) ) ;
#60890 = CARTESIAN_POINT ( 'NONE',  ( 0.000000000000000000, 0.000000000000000000, 0.000000000000000000 ) ) ;
#60892 = EDGE_CURVE ( 'NONE', #20669, #3213, #20880, .T. ) ;
#60891 = DIRECTION ( 'NONE',  ( 0.000000000000000000, -1.000000000000000000, 0.000000000000000000 ) ) ;
#60893 = CARTESIAN_POINT ( 'NONE',  ( 29.50000000000000355, -11.50000000000000000, -11.00000000000000000 ) ) ;
#60894 = VECTOR ( 'NONE', #10306, 1000.000000000000000 ) ;
#60895 = DIRECTION ( 'NONE',  ( -1.000000000000000000, 0.000000000000000000, 0.000000000000000000 ) ) ;
#60896 = EDGE_CURVE ( 'NONE', #46781, #30509, #7499, .T. ) ;
#60897 = ORIENTED_EDGE ( 'NONE', *, *, #26200, .T. ) ;
#60898 = ORIENTED_EDGE ( 'NONE', *, *, #59723, .T. ) ;
#60899 = VECTOR ( 'NONE', #26380, 1000.000000000000000 ) ;
#60900 = DIRECTION ( 'NONE',  ( 1.047444401652939849E-14, 1.000000000000000000, 0.000000000000000000 ) ) ;
#60901 = EDGE_CURVE ( 'NONE', #58346, #17426, #19931, .T. ) ;
#60902 = DIRECTION ( 'NONE',  ( -1.000000000000000000, 0.000000000000000000, 0.000000000000000000 ) ) ;
#60903 = VECTOR ( 'NONE', #54245, 1000.000000000000000 ) ;
#60904 = LINE ( 'NONE', #13519, #3845 ) ;
#60905 = ORIENTED_EDGE ( 'NONE', *, *, #5604, .T. ) ;
#60906 = CARTESIAN_POINT ( 'NONE',  ( 39.00000000000000000, -14.48845687959340012, -21.00000000000000000 ) ) ;
#60907 = VERTEX_POINT ( 'NONE', #48112 ) ;
#60908 = EDGE_CURVE ( 'NONE', #28990, #62386, #53773, .T. ) ;
#60909 = VERTEX_POINT ( 'NONE', #10618 ) ;
#60910 = EDGE_CURVE ( 'NONE', #42070, #34855, #723, .T. ) ;
#60911 = CYLINDRICAL_SURFACE ( 'NONE', #15504, 4.000000000000000000 ) ;
#60912 = AXIS2_PLACEMENT_3D ( 'NONE', #4874, #15825, #69917 ) ;
#60913 = CARTESIAN_POINT ( 'NONE',  ( 290.0000000000000000, 4.898587196589412829E-16, 4.000000000000000000 ) ) ;
#60914 = VERTEX_POINT ( 'NONE', #54800 ) ;
#60915 = PLANE ( 'NONE',  #57007 ) ;
#60916 = ADVANCED_FACE ( 'NONE', ( #48455 ), #48807, .F. ) ;
#60917 = EDGE_CURVE ( 'NONE', #49993, #57359, #21584, .T. ) ;
#60918 = DIRECTION ( 'NONE',  ( 0.000000000000000000, 3.673940397442059868E-16, -1.000000000000000000 ) ) ;
#60919 = ORIENTED_EDGE ( 'NONE', *, *, #53131, .F. ) ;
#60921 = ORIENTED_EDGE ( 'NONE', *, *, #52477, .F. ) ;
#60920 = CARTESIAN_POINT ( 'NONE',  ( 7.450000000000004619, -1.336933437520057563E-15, -14.00000000000000000 ) ) ;
#60922 = EDGE_CURVE ( 'NONE', #41506, #16868, #64716, .T. ) ;
#60923 = PLANE ( 'NONE',  #59698 ) ;
#60924 = DIRECTION ( 'NONE',  ( -1.000000000000000000, 0.000000000000000000, 0.000000000000000000 ) ) ;
#60925 = PLANE ( 'NONE',  #44729 ) ;
#60926 = DIRECTION ( 'NONE',  ( 0.000000000000000000, 1.000000000000000000, 0.000000000000000000 ) ) ;
#60927 = ORIENTED_EDGE ( 'NONE', *, *, #38462, .F. ) ;
#60928 = CARTESIAN_POINT ( 'NONE',  ( 275.0000000000000000, -42.00000000000000000, -15.00000000000000000 ) ) ;
#60929 = EDGE_CURVE ( 'NONE', #64997, #3474, #8616, .T. ) ;
#60930 = DIRECTION ( 'NONE',  ( -8.802523127157697409E-15, -1.000000000000000000, -1.836970198721026976E-16 ) ) ;
#60931 = ORIENTED_EDGE ( 'NONE', *, *, #7810, .T. ) ;
#60932 = ORIENTED_EDGE ( 'NONE', *, *, #53528, .F. ) ;
#60933 = ORIENTED_EDGE ( 'NONE', *, *, #16792, .F. ) ;
#60934 = LINE ( 'NONE', #27737, #51326 ) ;
#60935 = EDGE_CURVE ( 'NONE', #6091, #36263, #10977, .T. ) ;
#60936 = DIRECTION ( 'NONE',  ( 0.7671651518152985405, 0.6414496315691592399, -2.309356642088639737E-17 ) ) ;
#60937 = AXIS2_PLACEMENT_3D ( 'NONE', #26335, #58531, #58873 ) ;
#60938 = CIRCLE ( 'NONE', #14673, 0.5999999999999989786 ) ;
#60939 = DIRECTION ( 'NONE',  ( -1.000000000000000000, 0.000000000000000000, 0.000000000000000000 ) ) ;
#60940 = EDGE_CURVE ( 'NONE', #9679, #57901, #27245, .T. ) ;
#60941 = VECTOR ( 'NONE', #55781, 1000.000000000000000 ) ;
#60942 = ORIENTED_EDGE ( 'NONE', *, *, #50117, .T. ) ;
#60943 = ORIENTED_EDGE ( 'NONE', *, *, #24346, .T. ) ;
#60944 = VERTEX_POINT ( 'NONE', #58724 ) ;
#60945 = CARTESIAN_POINT ( 'NONE',  ( -14.25000000000000000, -2.500000000000000000, 21.77831216351300014 ) ) ;
#60946 = ORIENTED_EDGE ( 'NONE', *, *, #56244, .F. ) ;
#60947 = ORIENTED_EDGE ( 'NONE', *, *, #9528, .F. ) ;
#60948 = ORIENTED_EDGE ( 'NONE', *, *, #37064, .T. ) ;
#60949 = VECTOR ( 'NONE', #20491, 1000.000000000000114 ) ;
#60950 = ORIENTED_EDGE ( 'NONE', *, *, #2596, .F. ) ;
#60951 = DIRECTION ( 'NONE',  ( 0.000000000000000000, 0.7071067811865474617, 0.7071067811865474617 ) ) ;
#60953 = ORIENTED_EDGE ( 'NONE', *, *, #21582, .T. ) ;
#60952 = CARTESIAN_POINT ( 'NONE',  ( -7.360529556226213473E-16, 5.657408540444995637, 0.000000000000000000 ) ) ;
#60954 = CARTESIAN_POINT ( 'NONE',  ( 11.78648345035337819, -7.606483450353493936, 455.0000000000000568 ) ) ;
#60955 = CARTESIAN_POINT ( 'NONE',  ( -8.566576262117260754, 9.689726262117185129, 54.00000000000000711 ) ) ;
#60956 = CYLINDRICAL_SURFACE ( 'NONE', #20028, 0.5999999999999998668 ) ;
#60958 = ORIENTED_EDGE ( 'NONE', *, *, #38661, .F. ) ;
#60957 = FACE_OUTER_BOUND ( 'NONE', #11807, .T. ) ;
#60959 = VECTOR ( 'NONE', #26649, 1000.000000000000000 ) ;
#60960 = VECTOR ( 'NONE', #18954, 1000.000000000000000 ) ;
#60961 = DIRECTION ( 'NONE',  ( 1.000000000000000000, 0.000000000000000000, 0.000000000000000000 ) ) ;
#60962 = CARTESIAN_POINT ( 'NONE',  ( 28.00000000000000000, -16.64230188589300141, 14.64519951917099583 ) ) ;
#60963 = CARTESIAN_POINT ( 'NONE',  ( -8.250000000000001776, -7.249999999999998224, -22.50000000000000000 ) ) ;
#60964 = ORIENTED_EDGE ( 'NONE', *, *, #21532, .T. ) ;
#60965 = DIRECTION ( 'NONE',  ( 1.000000000000000000, -0.000000000000000000, 0.000000000000000000 ) ) ;
#60966 = EDGE_CURVE ( 'NONE', #39317, #44931, #56526, .T. ) ;
#60967 = CARTESIAN_POINT ( 'NONE',  ( 0.000000000000000000, 8.250000000000001776, -24.00000000000000000 ) ) ;
#60968 = LINE ( 'NONE', #68037, #5187 ) ;
#60969 = VERTEX_POINT ( 'NONE', #6694 ) ;
#60971 = EDGE_CURVE ( 'NONE', #65126, #11924, #34248, .T. ) ;
#60970 = DIRECTION ( 'NONE',  ( -0.7071067811865474617, 0.7071067811865474617, 2.597868168706479611E-16 ) ) ;
#60972 = DIRECTION ( 'NONE',  ( -2.891205793294683355E-15, -1.000000000000000000, 0.000000000000000000 ) ) ;
#60973 = DIRECTION ( 'NONE',  ( -1.000000000000000000, 1.047444401652940007E-14, -1.836970198721010706E-16 ) ) ;
#60974 = ADVANCED_FACE ( 'NONE', ( #23310 ), #44867, .F. ) ;
#60975 = EDGE_CURVE ( 'NONE', #16609, #23148, #63955, .T. ) ;
#60976 = ORIENTED_EDGE ( 'NONE', *, *, #18116, .F. ) ;
#60977 = DIRECTION ( 'NONE',  ( 0.000000000000000000, 0.000000000000000000, 1.000000000000000000 ) ) ;
#60978 = EDGE_CURVE ( 'NONE', #48159, #36748, #18758, .T. ) ;
#60979 = ADVANCED_FACE ( 'NONE', ( #7035 ), #27928, .T. ) ;
#60980 = DIRECTION ( 'NONE',  ( 0.7671651518153173033, 0.6414496315691367023, 2.587583378555109069E-16 ) ) ;
#60981 = CIRCLE ( 'NONE', #6827, 24.99999999998784972 ) ;
#60982 = DIRECTION ( 'NONE',  ( -1.047444401652939849E-14, -1.000000000000000000, 0.000000000000000000 ) ) ;
#60983 = CARTESIAN_POINT ( 'NONE',  ( 7.250000000000005329, -7.249999999999998224, -26.00000000000001066 ) ) ;
#60984 = CIRCLE ( 'NONE', #44092, 0.3499999999999996447 ) ;
#60985 = ORIENTED_EDGE ( 'NONE', *, *, #25157, .T. ) ;
#60986 = CARTESIAN_POINT ( 'NONE',  ( -7.250000000000000888, 8.250000000000001776, -17.00000000000000000 ) ) ;
#60987 = DIRECTION ( 'NONE',  ( 0.000000000000000000, -3.673940397442059868E-16, 1.000000000000000000 ) ) ;
#60988 = CARTESIAN_POINT ( 'NONE',  ( 39.00000000000000000, 0.000000000000000000, 0.000000000000000000 ) ) ;
#60989 = AXIS2_PLACEMENT_3D ( 'NONE', #27434, #59952, #59619 ) ;
#60990 = LINE ( 'NONE', #941, #53873 ) ;
#60991 = DIRECTION ( 'NONE',  ( 1.000000000000000000, 0.000000000000000000, 0.000000000000000000 ) ) ;
#60992 = EDGE_LOOP ( 'NONE', ( #60958, #67396 ) ) ;
#60993 = LINE ( 'NONE', #50042, #42283 ) ;
#60994 = DIRECTION ( 'NONE',  ( 0.000000000000000000, 0.000000000000000000, 1.000000000000000000 ) ) ;
#60995 = DIRECTION ( 'NONE',  ( -1.836970198721029934E-16, 1.836970198721036344E-16, -1.000000000000000000 ) ) ;
#60996 = VECTOR ( 'NONE', #53299, 1000.000000000000114 ) ;
#60997 = DIRECTION ( 'NONE',  ( 0.000000000000000000, 3.673940397442059868E-16, -1.000000000000000000 ) ) ;
#60998 = CARTESIAN_POINT ( 'NONE',  ( -9.722976262117244417, -3.682023737882722081, 26.00000000000000000 ) ) ;
#60999 = CIRCLE ( 'NONE', #59912, 1.000000000000001776 ) ;
#61000 = ORIENTED_EDGE ( 'NONE', *, *, #45672, .F. ) ;
#61001 = VERTEX_POINT ( 'NONE', #29291 ) ;
#61002 = CARTESIAN_POINT ( 'NONE',  ( 4.456444791733522252E-16, 7.450000000000002842, -22.00000000000000000 ) ) ;
#61003 = DIRECTION ( 'NONE',  ( -1.000000000000000000, 0.000000000000000000, 0.000000000000000000 ) ) ;
#61004 = ORIENTED_EDGE ( 'NONE', *, *, #5608, .F. ) ;
#61005 = VECTOR ( 'NONE', #60802, 1000.000000000000000 ) ;
#61006 = VECTOR ( 'NONE', #2953, 1000.000000000000000 ) ;
#61007 = DIRECTION ( 'NONE',  ( 0.000000000000000000, -1.000000000000000000, 0.000000000000000000 ) ) ;
#61008 = EDGE_LOOP ( 'NONE', ( #46361, #58017, #52551, #33012 ) ) ;
#61009 = DIRECTION ( 'NONE',  ( 1.000000000000000000, 0.000000000000000000, 0.000000000000000000 ) ) ;
#61010 = EDGE_LOOP ( 'NONE', ( #34210, #5749, #8130, #37534, #25104, #30774, #51186, #59804, #3741, #61035, #17239, #10738, #2069, #64718, #42324, #39028, #63267, #25201 ) ) ;
#61011 = ORIENTED_EDGE ( 'NONE', *, *, #10184, .F. ) ;
#61012 = DIRECTION ( 'NONE',  ( 1.000000000000000000, -1.047444401652940007E-14, 1.836970198721010706E-16 ) ) ;
#61013 = PLANE ( 'NONE',  #18444 ) ;
#61014 = DIRECTION ( 'NONE',  ( 1.000000000000000000, 0.000000000000000000, 0.000000000000000000 ) ) ;
#61016 = EDGE_CURVE ( 'NONE', #27989, #65011, #18692, .T. ) ;
#61015 = DIRECTION ( 'NONE',  ( 0.000000000000000000, 0.000000000000000000, -1.000000000000000000 ) ) ;
#61017 = VECTOR ( 'NONE', #23640, 1000.000000000000000 ) ;
#61018 = EDGE_LOOP ( 'NONE', ( #48201, #67734, #58433, #69863, #27954, #36873, #15411, #36479 ) ) ;
#61020 = EDGE_CURVE ( 'NONE', #40017, #31832, #40264, .T. ) ;
#61019 = ORIENTED_EDGE ( 'NONE', *, *, #9945, .T. ) ;
#61021 = DIRECTION ( 'NONE',  ( -1.000000000000000000, 0.000000000000000000, 0.000000000000000000 ) ) ;
#61022 = PLANE ( 'NONE',  #18060 ) ;
#61023 = VERTEX_POINT ( 'NONE', #22960 ) ;
#61024 = ORIENTED_EDGE ( 'NONE', *, *, #39260, .T. ) ;
#61025 = ORIENTED_EDGE ( 'NONE', *, *, #63656, .T. ) ;
#61026 = CARTESIAN_POINT ( 'NONE',  ( 152.0064834503532722, -29.01119750012554377, 0.000000000000000000 ) ) ;
#61027 = CIRCLE ( 'NONE', #2343, 4.000000000000000888 ) ;
#61029 = ORIENTED_EDGE ( 'NONE', *, *, #28756, .T. ) ;
#61028 = CARTESIAN_POINT ( 'NONE',  ( 283.0000000000000568, -30.80000000000000071, 12.20000000000000107 ) ) ;
#61030 = DIRECTION ( 'NONE',  ( 1.000000000000000000, -0.000000000000000000, -0.000000000000000000 ) ) ;
#61031 = AXIS2_PLACEMENT_3D ( 'NONE', #20319, #47884, #41884 ) ;
#61032 = CARTESIAN_POINT ( 'NONE',  ( 4.206483450353343478, -11.12648345035347575, 455.0000000000000568 ) ) ;
#61033 = EDGE_LOOP ( 'NONE', ( #63183, #18441, #42874, #29431 ) ) ;
#61034 = VECTOR ( 'NONE', #47708, 1000.000000000000000 ) ;
#61035 = ORIENTED_EDGE ( 'NONE', *, *, #10823, .F. ) ;
#61036 = VECTOR ( 'NONE', #59280, 1000.000000000000000 ) ;
#61037 = VECTOR ( 'NONE', #61432, 1000.000000000000000 ) ;
#61038 = CARTESIAN_POINT ( 'NONE',  ( 7.250000000000005329, -8.249999999999998224, -9.500000000000001776 ) ) ;
#61039 = CARTESIAN_POINT ( 'NONE',  ( 275.0000000000000000, -30.45000000000094786, -14.49999999999906031 ) ) ;
#61040 = CARTESIAN_POINT ( 'NONE',  ( 10.31889768521802253, -20.65270074880750428, -17.15270074880750428 ) ) ;
#61041 = VECTOR ( 'NONE', #16423, 1000.000000000000000 ) ;
#61042 = ADVANCED_FACE ( 'NONE', ( #65751 ), #55148, .T. ) ;
#61043 = FILL_AREA_STYLE_COLOUR ( '', #18850 ) ;
#61044 = CYLINDRICAL_SURFACE ( 'NONE', #58457, 1.000000000000000000 ) ;
#61046 = ORIENTED_EDGE ( 'NONE', *, *, #27990, .F. ) ;
#61045 =( NAMED_UNIT ( * ) PLANE_ANGLE_UNIT ( ) SI_UNIT ( $, .RADIAN. ) );
#61047 = VERTEX_POINT ( 'NONE', #28958 ) ;
#61048 = PLANE ( 'NONE',  #38867 ) ;
#61049 = CARTESIAN_POINT ( 'NONE',  ( 9.737023737882815055, -7.969523737882825642, 54.00000000000000711 ) ) ;
#61050 = PLANE ( 'NONE',  #69783 ) ;
#61051 = ADVANCED_FACE ( 'NONE', ( #44511 ), #50532, .F. ) ;
#61052 = EDGE_CURVE ( 'NONE', #50228, #31960, #22625, .T. ) ;
#61053 = DIRECTION ( 'NONE',  ( -1.000000000000000000, 0.000000000000000000, 0.000000000000000000 ) ) ;
#61054 = CARTESIAN_POINT ( 'NONE',  ( 8.612468434717188259, 1.991476262117162888, 54.00000000000000711 ) ) ;
#61056 = VERTEX_POINT ( 'NONE', #12675 ) ;
#61055 = EDGE_CURVE ( 'NONE', #20187, #55919, #17657, .T. ) ;
#61057 = DIRECTION ( 'NONE',  ( 0.000000000000000000, 0.000000000000000000, 1.000000000000000000 ) ) ;
#61058 = EDGE_CURVE ( 'NONE', #33875, #6182, #58298, .T. ) ;
#61059 = DIRECTION ( 'NONE',  ( 0.000000000000000000, -0.1249999999999996531, -0.9921567416492215186 ) ) ;
#61060 = LINE ( 'NONE', #34183, #31175 ) ;
#61061 = DIRECTION ( 'NONE',  ( -1.836970198721029934E-16, 1.836970198721036344E-16, -1.000000000000000000 ) ) ;
#61062 = EDGE_CURVE ( 'NONE', #8558, #69064, #23646, .T. ) ;
#61063 = VECTOR ( 'NONE', #27148, 1000.000000000000000 ) ;
#61064 = CARTESIAN_POINT ( 'NONE',  ( 0.000000000000000000, -5.000000000000000000, 0.000000000000000000 ) ) ;
#61065 = DIRECTION ( 'NONE',  ( 0.000000000000000000, -1.000000000000000000, 0.000000000000000000 ) ) ;
#61066 = DIRECTION ( 'NONE',  ( -0.000000000000000000, 1.000000000000000000, -0.000000000000000000 ) ) ;
#61067 = VERTEX_POINT ( 'NONE', #11990 ) ;
#61068 = LINE ( 'NONE', #23592, #32101 ) ;
#61069 = LINE ( 'NONE', #11938, #14835 ) ;
#61070 = ORIENTED_EDGE ( 'NONE', *, *, #35697, .F. ) ;
#61071 = CARTESIAN_POINT ( 'NONE',  ( -3.710438382363177912, -7.408280051175174741, 54.00000000000000711 ) ) ;
#61072 = DIRECTION ( 'NONE',  ( -1.794541526872559352E-16, -1.000000000000000000, 0.000000000000000000 ) ) ;
#61073 = DIRECTION ( 'NONE',  ( -0.000000000000000000, -0.000000000000000000, 1.000000000000000000 ) ) ;
#61074 = CARTESIAN_POINT ( 'NONE',  ( -10.08346604330787777, 9.293516549646602343, 455.0000000000000568 ) ) ;
#61075 = DIRECTION ( 'NONE',  ( 0.000000000000000000, 0.000000000000000000, 1.000000000000000000 ) ) ;
#61076 = AXIS2_PLACEMENT_3D ( 'NONE', #50976, #50278, #2883 ) ;
#61077 = ORIENTED_EDGE ( 'NONE', *, *, #41158, .T. ) ;
#61078 = CARTESIAN_POINT ( 'NONE',  ( -8.250000000000001776, 0.000000000000000000, -8.000000000000000000 ) ) ;
#61079 = VECTOR ( 'NONE', #66536, 1000.000000000000000 ) ;
#61080 = ORIENTED_EDGE ( 'NONE', *, *, #60764, .F. ) ;
#61081 = DIRECTION ( 'NONE',  ( 0.000000000000000000, 0.000000000000000000, -1.000000000000000000 ) ) ;
#61082 = EDGE_LOOP ( 'NONE', ( #46149, #37540, #15993, #15480 ) ) ;
#61083 = AXIS2_PLACEMENT_3D ( 'NONE', #68929, #15192, #36762 ) ;
#61084 = DIRECTION ( 'NONE',  ( 1.000000000000000000, 0.000000000000000000, 0.000000000000000000 ) ) ;
#61085 = AXIS2_PLACEMENT_3D ( 'NONE', #56666, #19530, #52065 ) ;
#61086 = VECTOR ( 'NONE', #18230, 1000.000000000000000 ) ;
#61087 = CARTESIAN_POINT ( 'NONE',  ( -7.813516549646836395, -11.78648345035340661, 455.0000000000000568 ) ) ;
#61088 = DIRECTION ( 'NONE',  ( 0.000000000000000000, 1.000000000000000000, 0.000000000000000000 ) ) ;
#61089 = ORIENTED_EDGE ( 'NONE', *, *, #23731, .T. ) ;
#61090 = ORIENTED_EDGE ( 'NONE', *, *, #21737, .T. ) ;
#61091 = LINE ( 'NONE', #44483, #64607 ) ;
#61092 = ORIENTED_EDGE ( 'NONE', *, *, #68283, .F. ) ;
#61093 = CIRCLE ( 'NONE', #22760, 4.000000000000000888 ) ;
#61094 = VERTEX_POINT ( 'NONE', #33573 ) ;
#61095 = DIRECTION ( 'NONE',  ( -1.836970198721029934E-16, -1.836970198721010706E-16, 1.000000000000000000 ) ) ;
#61096 = CARTESIAN_POINT ( 'NONE',  ( 0.000000000000000000, -7.449999999999998401, -25.00000000000000000 ) ) ;
#61097 = CARTESIAN_POINT ( 'NONE',  ( 175.4206970127264356, -30.42541106249864669, 5.000000000000000000 ) ) ;
#61098 = VECTOR ( 'NONE', #51948, 999.9999999999998863 ) ;
#61099 = EDGE_LOOP ( 'NONE', ( #41211, #11470, #39439, #26108 ) ) ;
#61100 = EDGE_CURVE ( 'NONE', #10947, #35367, #7729, .T. ) ;
#61101 = EDGE_CURVE ( 'NONE', #14586, #20510, #61468, .T. ) ;
#61102 = CARTESIAN_POINT ( 'NONE',  ( -10.91351654964670814, 9.093516549646603053, 195.0000000000000284 ) ) ;
#61103 = ADVANCED_FACE ( 'NONE', ( #23996, #35287 ), #30362, .F. ) ;
#61105 = DIRECTION ( 'NONE',  ( 1.836970198721029934E-16, 1.836970198721010706E-16, -1.000000000000000000 ) ) ;
#61104 = FACE_OUTER_BOUND ( 'NONE', #48492, .T. ) ;
#61106 = ORIENTED_EDGE ( 'NONE', *, *, #12518, .F. ) ;
#61108 = EDGE_LOOP ( 'NONE', ( #8320, #37724, #32621, #61165, #18734, #59878 ) ) ;
#61107 = CARTESIAN_POINT ( 'NONE',  ( 283.0000000000000568, -32.95000000000000284, -7.700000000000000178 ) ) ;
#61109 = ORIENTED_EDGE ( 'NONE', *, *, #148, .T. ) ;
#61110 = EDGE_CURVE ( 'NONE', #58198, #9849, #62890, .T. ) ;
#61111 = DIRECTION ( 'NONE',  ( 1.000000000000000000, 0.000000000000000000, 0.000000000000000000 ) ) ;
#61112 = DIRECTION ( 'NONE',  ( 0.7071067811865470176, 0.000000000000000000, 0.7071067811865480168 ) ) ;
#61113 = ORIENTED_EDGE ( 'NONE', *, *, #11588, .T. ) ;
#61114 = LINE ( 'NONE', #16969, #25801 ) ;
#61115 = CARTESIAN_POINT ( 'NONE',  ( 10.00000000000000000, -18.00000000000000355, -21.00000000000000000 ) ) ;
#61116 = EDGE_LOOP ( 'NONE', ( #30368, #43015, #9895, #37590, #19265, #10631, #33985, #27507 ) ) ;
#61117 = ORIENTED_EDGE ( 'NONE', *, *, #35645, .T. ) ;
#61118 = CARTESIAN_POINT ( 'NONE',  ( 35.89999999999999858, 13.66939075806899240, -20.79999999999999361 ) ) ;
#61119 = DIRECTION ( 'NONE',  ( 0.000000000000000000, 0.000000000000000000, 1.000000000000000000 ) ) ;
#61120 = VERTEX_POINT ( 'NONE', #25059 ) ;
#61121 = CARTESIAN_POINT ( 'NONE',  ( 8.250000000000005329, -7.249999999999998224, -12.00000000000000000 ) ) ;
#61122 = DIRECTION ( 'NONE',  ( 0.000000000000000000, 0.000000000000000000, -1.000000000000000000 ) ) ;
#61123 = LINE ( 'NONE', #1738, #40704 ) ;
#61124 = AXIS2_PLACEMENT_3D ( 'NONE', #64827, #16380, #53527 ) ;
#61125 = ORIENTED_EDGE ( 'NONE', *, *, #48561, .F. ) ;
#61126 = VECTOR ( 'NONE', #16649, 1000.000000000000000 ) ;
#61127 = FACE_OUTER_BOUND ( 'NONE', #45605, .T. ) ;
#61128 = LINE ( 'NONE', #6030, #5756 ) ;
#61129 = EDGE_LOOP ( 'NONE', ( #11473, #42958, #45724, #47865 ) ) ;
#61131 = VERTEX_POINT ( 'NONE', #24352 ) ;
#61130 = DIRECTION ( 'NONE',  ( 1.000000000000000000, -1.047444401652940007E-14, 1.836970198721010706E-16 ) ) ;
#61132 = PLANE ( 'NONE',  #16716 ) ;
#61133 = CARTESIAN_POINT ( 'NONE',  ( -7.250000000000001776, -7.249999999999998224, -9.000000000000001776 ) ) ;
#61134 = DIRECTION ( 'NONE',  ( -0.000000000000000000, -0.000000000000000000, -1.000000000000000000 ) ) ;
#61135 = AXIS2_PLACEMENT_3D ( 'NONE', #5027, #26593, #32244 ) ;
#61136 = CLOSED_SHELL ( 'NONE', ( #42737, #7370, #37949, #20634, #108, #44475, #277, #53759, #52643, #15279, #36466, #14830, #33381, #55789 ) ) ;
#61137 = LINE ( 'NONE', #7401, #6806 ) ;
#61138 = DIRECTION ( 'NONE',  ( 0.000000000000000000, 0.000000000000000000, 1.000000000000000000 ) ) ;
#61139 = EDGE_LOOP ( 'NONE', ( #31632, #69525, #52826, #60618 ) ) ;
#61140 = DIRECTION ( 'NONE',  ( -1.836970198721029934E-16, -1.836970198721010706E-16, 1.000000000000000000 ) ) ;
#61141 = CARTESIAN_POINT ( 'NONE',  ( 7.450000000000004619, -1.336933437520057563E-15, -9.500000000000001776 ) ) ;
#61142 = AXIS2_PLACEMENT_3D ( 'NONE', #68246, #36065, #57637 ) ;
#61143 = ADVANCED_FACE ( 'NONE', ( #29648 ), #2780, .T. ) ;
#61144 = DIRECTION ( 'NONE',  ( 4.121462285523434458E-16, 1.000000000000000000, 0.000000000000000000 ) ) ;
#61146 = ORIENTED_EDGE ( 'NONE', *, *, #41686, .F. ) ;
#61145 = DIRECTION ( 'NONE',  ( -1.000000000000000000, 0.000000000000000000, 0.000000000000000000 ) ) ;
#61147 = DIRECTION ( 'NONE',  ( -1.000000000000000000, 0.000000000000000000, 0.000000000000000000 ) ) ;
#61148 = EDGE_CURVE ( 'NONE', #27390, #54230, #25775, .T. ) ;
#61149 = ADVANCED_FACE ( 'NONE', ( #51932 ), #19734, .F. ) ;
#61150 = CARTESIAN_POINT ( 'NONE',  ( -9.547976262117254365, 8.130476262117182884, 54.00000000000000711 ) ) ;
#61151 = CIRCLE ( 'NONE', #9248, 3.499999999999999556 ) ;
#61152 = EDGE_CURVE ( 'NONE', #49332, #21330, #45924, .T. ) ;
#61153 = ORIENTED_EDGE ( 'NONE', *, *, #63559, .T. ) ;
#61154 = CYLINDRICAL_SURFACE ( 'NONE', #44432, 24.99999999998789946 ) ;
#61155 = CARTESIAN_POINT ( 'NONE',  ( 6.501044194225443995, 2.617976262117186703, 54.00000000000000711 ) ) ;
#61156 = VERTEX_POINT ( 'NONE', #24705 ) ;
#61157 = DIRECTION ( 'NONE',  ( -0.9583148474998870459, 0.000000000000000000, 0.2857142857143623593 ) ) ;
#61158 = CARTESIAN_POINT ( 'NONE',  ( 29.50000000000000355, -15.97213595500069871, 14.50000000000000000 ) ) ;
#61159 = FILL_AREA_STYLE ('',( #13434 ) ) ;
#61160 = APPLICATION_CONTEXT ( 'automotive_design' ) ;
#61161 = ADVANCED_FACE ( 'NONE', ( #20450 ), #34539, .T. ) ;
#61162 = LINE ( 'NONE', #16681, #47396 ) ;
#61163 = EDGE_CURVE ( 'NONE', #51833, #63119, #62174, .T. ) ;
#61164 = CARTESIAN_POINT ( 'NONE',  ( 15.00000000000000000, -26.42999999999999972, 5.874955318979029784 ) ) ;
#61165 = ORIENTED_EDGE ( 'NONE', *, *, #60056, .T. ) ;
#61166 = VECTOR ( 'NONE', #14624, 1000.000000000000000 ) ;
#61167 = PLANE ( 'NONE',  #67775 ) ;
#61168 = ORIENTED_EDGE ( 'NONE', *, *, #21922, .T. ) ;
#61169 = VERTEX_POINT ( 'NONE', #46965 ) ;
#61170 = DIRECTION ( 'NONE',  ( 0.000000000000000000, 0.000000000000000000, -1.000000000000000000 ) ) ;
#61171 = AXIS2_PLACEMENT_3D ( 'NONE', #49451, #5622, #1015 ) ;
#61172 = DIRECTION ( 'NONE',  ( -0.7071067811865474617, 0.7071067811865474617, -0.000000000000000000 ) ) ;
#61173 = DIRECTION ( 'NONE',  ( 0.000000000000000000, 0.000000000000000000, 1.000000000000000000 ) ) ;
#61174 = ORIENTED_EDGE ( 'NONE', *, *, #7745, .T. ) ;
#61175 = ORIENTED_EDGE ( 'NONE', *, *, #65569, .F. ) ;
#61176 = VECTOR ( 'NONE', #36108, 1000.000000000000000 ) ;
#61177 = CYLINDRICAL_SURFACE ( 'NONE', #65714, 0.1999999999999996503 ) ;
#61178 = ORIENTED_EDGE ( 'NONE', *, *, #7188, .F. ) ;
#61179 = DIRECTION ( 'NONE',  ( 1.000000000000000000, 0.000000000000000000, 0.000000000000000000 ) ) ;
#61180 = CARTESIAN_POINT ( 'NONE',  ( -7.250000000000000888, 7.250000000000001776, -14.50000000000000000 ) ) ;
#61181 = LINE ( 'NONE', #12739, #6009 ) ;
#61182 = CARTESIAN_POINT ( 'NONE',  ( -11.00000000000000000, -11.10796162543699950, -9.102987789146602893 ) ) ;
#61184 = DIRECTION ( 'NONE',  ( 0.000000000000000000, 0.000000000000000000, -1.000000000000000000 ) ) ;
#61183 = CARTESIAN_POINT ( 'NONE',  ( -16.89194109070750116, -5.000000000000000000, 26.25000000000000000 ) ) ;
#61185 = EDGE_LOOP ( 'NONE', ( #33019, #20485, #22350, #37890 ) ) ;
#61187 = ORIENTED_EDGE ( 'NONE', *, *, #23731, .F. ) ;
#61186 = LINE ( 'NONE', #60849, #2497 ) ;
#61188 = ORIENTED_EDGE ( 'NONE', *, *, #9838, .T. ) ;
#61189 = ORIENTED_EDGE ( 'NONE', *, *, #32325, .F. ) ;
#61190 = CIRCLE ( 'NONE', #17147, 24.99999999998785327 ) ;
#61191 = EDGE_CURVE ( 'NONE', #12812, #51717, #19049, .T. ) ;
#61192 = DIRECTION ( 'NONE',  ( -0.000000000000000000, -0.000000000000000000, -1.000000000000000000 ) ) ;
#61193 = AXIS2_PLACEMENT_3D ( 'NONE', #2405, #28579, #33877 ) ;
#61194 = CARTESIAN_POINT ( 'NONE',  ( -7.415254214038309755, -3.606483450353353160, 195.0000000000000284 ) ) ;
#61195 = CIRCLE ( 'NONE', #33011, 24.99999999998789946 ) ;
#61196 = FACE_OUTER_BOUND ( 'NONE', #48705, .T. ) ;
#61197 = VERTEX_POINT ( 'NONE', #3840 ) ;
#61198 = ORIENTED_EDGE ( 'NONE', *, *, #15425, .F. ) ;
#61199 = VECTOR ( 'NONE', #54063, 1000.000000000000000 ) ;
#61200 = EDGE_CURVE ( 'NONE', #31506, #20448, #3496, .T. ) ;
#61201 = DIRECTION ( 'NONE',  ( 0.000000000000000000, 0.000000000000000000, -1.000000000000000000 ) ) ;
#61202 = FACE_OUTER_BOUND ( 'NONE', #32706, .T. ) ;
#61203 = ORIENTED_EDGE ( 'NONE', *, *, #18107, .F. ) ;
#61204 = ORIENTED_EDGE ( 'NONE', *, *, #15147, .F. ) ;
#61205 = LINE ( 'NONE', #60531, #45201 ) ;
#61206 = ADVANCED_FACE ( 'NONE', ( #51584 ), #30003, .T. ) ;
#61207 = DIRECTION ( 'NONE',  ( 1.000000000000000000, 0.000000000000000000, 0.000000000000000000 ) ) ;
#61208 = ORIENTED_EDGE ( 'NONE', *, *, #37152, .T. ) ;
#61209 = DIRECTION ( 'NONE',  ( -1.836970198721029934E-16, 1.836970198721036344E-16, -1.000000000000000000 ) ) ;
#61211 = VERTEX_POINT ( 'NONE', #67841 ) ;
#61210 = CARTESIAN_POINT ( 'NONE',  ( 12.00648345035338060, -4.186483450353396307, 195.0000000000000284 ) ) ;
#61212 = VERTEX_POINT ( 'NONE', #40612 ) ;
#61213 = LINE ( 'NONE', #1488, #67180 ) ;
#61214 = CARTESIAN_POINT ( 'NONE',  ( 7.250000000000005329, 7.250000000000000888, -14.00000000000000000 ) ) ;
#61215 = DIRECTION ( 'NONE',  ( 0.000000000000000000, 1.000000000000000000, 0.000000000000000000 ) ) ;
#61216 = AXIS2_PLACEMENT_3D ( 'NONE', #24580, #40830, #28812 ) ;
#61217 = CARTESIAN_POINT ( 'NONE',  ( -7.250000000000000888, 7.250000000000001776, -12.00000000000000000 ) ) ;
#61218 = EDGE_CURVE ( 'NONE', #58489, #2756, #62827, .T. ) ;
#61219 = CARTESIAN_POINT ( 'NONE',  ( -7.450000000000001954, 7.250000000000000000, -7.500000000000000000 ) ) ;
#61220 = DIRECTION ( 'NONE',  ( -0.000000000000000000, -0.000000000000000000, -1.000000000000000000 ) ) ;
#61221 = CYLINDRICAL_SURFACE ( 'NONE', #8934, 24.99999999998794920 ) ;
#61222 = AXIS2_PLACEMENT_3D ( 'NONE', #26133, #42378, #63967 ) ;
#61223 = ORIENTED_EDGE ( 'NONE', *, *, #51903, .T. ) ;
#61224 = CARTESIAN_POINT ( 'NONE',  ( -17.00000000000000000, -16.64230188589300141, 14.64519951917099583 ) ) ;
#61226 = EDGE_LOOP ( 'NONE', ( #12956, #28249 ) ) ;
#61225 = DIRECTION ( 'NONE',  ( 0.000000000000000000, 0.000000000000000000, 1.000000000000000000 ) ) ;
#61227 = DIRECTION ( 'NONE',  ( 0.000000000000000000, 1.000000000000000000, 0.000000000000000000 ) ) ;
#61228 = CARTESIAN_POINT ( 'NONE',  ( 7.000000000000000000, -21.00000000000000000, 0.000000000000000000 ) ) ;
#61229 = ADVANCED_FACE ( 'NONE', ( #14091 ), #35646, .T. ) ;
#61230 = CARTESIAN_POINT ( 'NONE',  ( 0.000000000000000000, 8.250000000000001776, -9.000000000000001776 ) ) ;
#61231 = CARTESIAN_POINT ( 'NONE',  ( 49.00000000000000000, -0.2000000000089119934, 8.909539772616881237E-12 ) ) ;
#61232 = LINE ( 'NONE', #66558, #54077 ) ;
#61233 = EDGE_CURVE ( 'NONE', #64674, #68234, #56871, .T. ) ;
#61234 = VERTEX_POINT ( 'NONE', #19392 ) ;
#61235 = VECTOR ( 'NONE', #23465, 1000.000000000000000 ) ;
#61236 = ORIENTED_EDGE ( 'NONE', *, *, #63433, .T. ) ;
#61237 = CARTESIAN_POINT ( 'NONE',  ( -8.593516549646711411, 7.603567055985436696, 455.0000000000000568 ) ) ;
#61238 = ADVANCED_FACE ( 'NONE', ( #40957, #52641 ), #4208, .T. ) ;
#61239 = DIRECTION ( 'NONE',  ( -1.836970198721029934E-16, 1.836970198721036590E-16, -1.000000000000000000 ) ) ;
#61240 = ADVANCED_FACE ( 'NONE', ( #48023 ), #21841, .F. ) ;
#61241 = FACE_OUTER_BOUND ( 'NONE', #62695, .T. ) ;
#61242 = ORIENTED_EDGE ( 'NONE', *, *, #23005, .F. ) ;
#61243 = DIRECTION ( 'NONE',  ( 0.000000000000000000, -0.9239212585478300266, -0.3825826812643171038 ) ) ;
#61244 = EDGE_LOOP ( 'NONE', ( #35035, #23824, #49882, #30764 ) ) ;
#61245 = ORIENTED_EDGE ( 'NONE', *, *, #40947, .F. ) ;
#61246 = AXIS2_PLACEMENT_3D ( 'NONE', #41611, #41962, #26063 ) ;
#61247 = CYLINDRICAL_SURFACE ( 'NONE', #24522, 0.1749999999999980738 ) ;
#61248 = FACE_OUTER_BOUND ( 'NONE', #59717, .T. ) ;
#61249 = ORIENTED_EDGE ( 'NONE', *, *, #41609, .T. ) ;
#61250 = PLANE ( 'NONE',  #61535 ) ;
#61251 = VECTOR ( 'NONE', #8203, 1000.000000000000000 ) ;
#61252 = EDGE_CURVE ( 'NONE', #32206, #14663, #42366, .T. ) ;
#61253 = PLANE ( 'NONE',  #15154 ) ;
#61254 = VECTOR ( 'NONE', #20125, 1000.000000000000000 ) ;
#61255 = DIRECTION ( 'NONE',  ( -1.836970198721029934E-16, 1.836970198721036344E-16, -1.000000000000000000 ) ) ;
#61256 = ORIENTED_EDGE ( 'NONE', *, *, #41200, .T. ) ;
#61258 = ORIENTED_EDGE ( 'NONE', *, *, #19390, .T. ) ;
#61257 = CYLINDRICAL_SURFACE ( 'NONE', #14798, 1.399999999999999245 ) ;
#61259 = ORIENTED_EDGE ( 'NONE', *, *, #29497, .T. ) ;
#61260 = LINE ( 'NONE', #55294, #35969 ) ;
#61261 = DIRECTION ( 'NONE',  ( 0.000000000000000000, 0.000000000000000000, 1.000000000000000000 ) ) ;
#61262 = FACE_OUTER_BOUND ( 'NONE', #3238, .T. ) ;
#61263 = EDGE_CURVE ( 'NONE', #26074, #19113, #32470, .T. ) ;
#61264 = PLANE ( 'NONE',  #11584 ) ;
#61265 = SURFACE_STYLE_FILL_AREA ( #19198 ) ;
#61266 = CARTESIAN_POINT ( 'NONE',  ( -8.916576262117361651, -10.05377373788273587, 54.00000000000000711 ) ) ;
#61267 = CIRCLE ( 'NONE', #69225, 0.1749999999999998224 ) ;
#61268 = ORIENTED_EDGE ( 'NONE', *, *, #50607, .T. ) ;
#61269 = EDGE_LOOP ( 'NONE', ( #32395, #54427 ) ) ;
#61270 = EDGE_CURVE ( 'NONE', #21681, #49752, #61705, .T. ) ;
#61271 = VERTEX_POINT ( 'NONE', #21495 ) ;
#61272 = DIRECTION ( 'NONE',  ( 0.000000000000000000, 1.000000000000000000, 0.000000000000000000 ) ) ;
#61273 = CARTESIAN_POINT ( 'NONE',  ( -29.50000000000000355, -11.50000000000000000, 15.00000000000000000 ) ) ;
#61274 = EDGE_CURVE ( 'NONE', #64371, #5737, #32109, .T. ) ;
#61275 = CARTESIAN_POINT ( 'NONE',  ( 0.000000000000000000, 8.250000000000001776, -15.00000000000000000 ) ) ;
#61276 = ORIENTED_EDGE ( 'NONE', *, *, #4287, .T. ) ;
#61277 = VERTEX_POINT ( 'NONE', #37079 ) ;
#61278 = ORIENTED_EDGE ( 'NONE', *, *, #49483, .F. ) ;
#61279 = EDGE_CURVE ( 'NONE', #50319, #10944, #38068, .T. ) ;
#61280 = DIRECTION ( 'NONE',  ( 0.000000000000000000, 1.000000000000000000, 0.000000000000000000 ) ) ;
#61281 = ORIENTED_EDGE ( 'NONE', *, *, #2982, .F. ) ;
#61282 = EDGE_CURVE ( 'NONE', #59628, #28450, #65122, .T. ) ;
#61283 = ORIENTED_EDGE ( 'NONE', *, *, #15769, .T. ) ;
#61284 = VERTEX_POINT ( 'NONE', #59325 ) ;
#61285 = VERTEX_POINT ( 'NONE', #10887 ) ;
#61286 = DIRECTION ( 'NONE',  ( -1.000000000000000000, 0.000000000000000000, 0.000000000000000000 ) ) ;
#61287 = ADVANCED_FACE ( 'NONE', ( #10537 ), #54039, .F. ) ;
#61289 = ORIENTED_EDGE ( 'NONE', *, *, #44149, .T. ) ;
#61288 = CARTESIAN_POINT ( 'NONE',  ( 10.92648345035337343, -2.706483450353395437, 195.0000000000000284 ) ) ;
#61290 = DIRECTION ( 'NONE',  ( 0.000000000000000000, -3.673940397442059868E-16, 1.000000000000000000 ) ) ;
#61292 = DIRECTION ( 'NONE',  ( 1.060575238724893480E-16, 0.5000000000000189848, -0.8660254037844277164 ) ) ;
#61291 = CIRCLE ( 'NONE', #55662, 1.399999999999998579 ) ;
#61293 = DIRECTION ( 'NONE',  ( 0.000000000000000000, -1.000000000000000000, 0.000000000000000000 ) ) ;
#61294 = ADVANCED_FACE ( 'NONE', ( #59677 ), #11226, .T. ) ;
#61296 = ORIENTED_EDGE ( 'NONE', *, *, #6561, .F. ) ;
#61295 = DIRECTION ( 'NONE',  ( -3.596772705736694889E-15, -1.000000000000000000, 0.000000000000000000 ) ) ;
#61297 = EDGE_CURVE ( 'NONE', #59237, #22525, #58287, .T. ) ;
#61299 = VERTEX_POINT ( 'NONE', #52995 ) ;
#61298 = AXIS2_PLACEMENT_3D ( 'NONE', #52141, #10065, #8996 ) ;
#61300 = AXIS2_PLACEMENT_3D ( 'NONE', #51537, #3100, #46217 ) ;
#61301 = ADVANCED_FACE ( 'NONE', ( #26819 ), #4891, .T. ) ;
#61302 = DIRECTION ( 'NONE',  ( -1.000000000000000000, 0.000000000000000000, 0.000000000000000000 ) ) ;
#61303 = ADVANCED_FACE ( 'NONE', ( #48719, #279 ), #64291, .T. ) ;
#61304 = EDGE_CURVE ( 'NONE', #17425, #40699, #52710, .T. ) ;
#61305 = DIRECTION ( 'NONE',  ( -1.000000000000000000, 0.000000000000000000, 0.000000000000000000 ) ) ;
#61306 = DIRECTION ( 'NONE',  ( 0.000000000000000000, 0.000000000000000000, 1.000000000000000000 ) ) ;
#61307 = COLOUR_RGB ( '', 0.31764706, 0.68627451, 0.89019608) ;
#61308 = VECTOR ( 'NONE', #23238, 1000.000000000000000 ) ;
#61309 = EDGE_LOOP ( 'NONE', ( #55608, #33876 ) ) ;
#61310 = CARTESIAN_POINT ( 'NONE',  ( 276.8000000000000682, -25.60000000000000142, -17.60000000000000142 ) ) ;
#61311 = EDGE_CURVE ( 'NONE', #18067, #59587, #6365, .T. ) ;
#61312 = CARTESIAN_POINT ( 'NONE',  ( 0.000000000000000000, -7.449999999999998401, -16.50000000000000000 ) ) ;
#61313 = VECTOR ( 'NONE', #1397, 1000.000000000000000 ) ;
#61314 = CYLINDRICAL_SURFACE ( 'NONE', #40180, 1.000000000000001776 ) ;
#61315 = ADVANCED_FACE ( 'NONE', ( #25 ), #60093, .T. ) ;
#61316 = EDGE_LOOP ( 'NONE', ( #40809, #30401, #47892, #57393 ) ) ;
#61317 = FACE_OUTER_BOUND ( 'NONE', #11411, .T. ) ;
#61318 = EDGE_CURVE ( 'NONE', #17506, #64534, #64376, .T. ) ;
#61319 = FACE_BOUND ( 'NONE', #19463, .T. ) ;
#61320 = LINE ( 'NONE', #12875, #41588 ) ;
#61321 = AXIS2_PLACEMENT_3D ( 'NONE', #41452, #41092, #25903 ) ;
#61322 = ORIENTED_EDGE ( 'NONE', *, *, #46608, .T. ) ;
#61323 = CARTESIAN_POINT ( 'NONE',  ( -6.858227778582841161, -3.003254798005709603, 26.00000000000000711 ) ) ;
#61324 = CIRCLE ( 'NONE', #57971, 0.1999999999999996503 ) ;
#61325 = EDGE_CURVE ( 'NONE', #22300, #56770, #21583, .T. ) ;
#61326 = CARTESIAN_POINT ( 'NONE',  ( 283.0000000000000568, -29.94999999999999929, -14.50000000000000000 ) ) ;
#61327 = CARTESIAN_POINT ( 'NONE',  ( 6.344579767990853547, 8.393516549646580671, 455.0000000000000568 ) ) ;
#61328 = ADVANCED_FACE ( 'NONE', ( #15598 ), #42794, .F. ) ;
#61329 = EDGE_LOOP ( 'NONE', ( #43420, #6278, #66506, #44310 ) ) ;
#61330 = DIRECTION ( 'NONE',  ( 1.000000000000000000, -3.491481338843133355E-15, -1.836970198721036344E-16 ) ) ;
#61331 = CARTESIAN_POINT ( 'NONE',  ( -0.9414762621172249046, 9.915476262117151052, 54.00000000000000711 ) ) ;
#61332 = CARTESIAN_POINT ( 'NONE',  ( 10.31452373788280497, 6.642976262117183062, 54.00000000000000711 ) ) ;
#61333 = FACE_OUTER_BOUND ( 'NONE', #62859, .T. ) ;
#61334 = DIRECTION ( 'NONE',  ( 0.000000000000000000, 0.000000000000000000, 1.000000000000000000 ) ) ;
#61335 = EDGE_LOOP ( 'NONE', ( #44800, #63644, #1724, #42636 ) ) ;
#61336 = PLANE ( 'NONE',  #62616 ) ;
#61337 = LINE ( 'NONE', #12895, #19209 ) ;
#61338 = CARTESIAN_POINT ( 'NONE',  ( 7.250000000000005329, -7.249999999999998224, -17.50000000000000000 ) ) ;
#61339 = CYLINDRICAL_SURFACE ( 'NONE', #4908, 0.1999999999999987899 ) ;
#61340 = FACE_OUTER_BOUND ( 'NONE', #42965, .T. ) ;
#61341 = ORIENTED_EDGE ( 'NONE', *, *, #24085, .T. ) ;
#61343 = ORIENTED_EDGE ( 'NONE', *, *, #44487, .T. ) ;
#61342 = CARTESIAN_POINT ( 'NONE',  ( 12.00648345035341968, 11.18071654964654726, 455.0000000000000568 ) ) ;
#61344 = AXIS2_PLACEMENT_3D ( 'NONE', #47786, #68311, #20215 ) ;
#61345 = AXIS2_PLACEMENT_3D ( 'NONE', #39116, #257, #54696 ) ;
#61346 = LINE ( 'NONE', #61002, #50743 ) ;
#61347 = DIRECTION ( 'NONE',  ( -1.000000000000000000, 0.000000000000000000, 0.000000000000000000 ) ) ;
#61348 = ORIENTED_EDGE ( 'NONE', *, *, #9247, .T. ) ;
#61349 = VECTOR ( 'NONE', #27536, 1000.000000000000227 ) ;
#61350 = CARTESIAN_POINT ( 'NONE',  ( -7.290476262117262962, 9.722976262117180468, 54.00000000000000711 ) ) ;
#61351 = AXIS2_PLACEMENT_3D ( 'NONE', #22366, #60521, #11389 ) ;
#61352 = ORIENTED_EDGE ( 'NONE', *, *, #13761, .T. ) ;
#61353 = DIRECTION ( 'NONE',  ( 0.000000000000000000, 0.000000000000000000, 1.000000000000000000 ) ) ;
#61355 = EDGE_LOOP ( 'NONE', ( #21365, #20874, #9392, #10873 ) ) ;
#61354 = AXIS2_PLACEMENT_3D ( 'NONE', #4129, #51145, #13667 ) ;
#61356 = CIRCLE ( 'NONE', #28612, 24.99999999998794920 ) ;
#61357 = ORIENTED_EDGE ( 'NONE', *, *, #26576, .T. ) ;
#61358 = FACE_OUTER_BOUND ( 'NONE', #27921, .T. ) ;
#61359 = CARTESIAN_POINT ( 'NONE',  ( 41.09999999999999432, -14.48845687959340012, 21.00000000000000000 ) ) ;
#61360 = ADVANCED_FACE ( 'NONE', ( #59756 ), #5339, .F. ) ;
#61361 = FACE_OUTER_BOUND ( 'NONE', #28941, .T. ) ;
#61362 = FACE_OUTER_BOUND ( 'NONE', #59037, .T. ) ;
#61363 = ORIENTED_EDGE ( 'NONE', *, *, #5698, .F. ) ;
#61364 = ORIENTED_EDGE ( 'NONE', *, *, #69401, .T. ) ;
#61365 = EDGE_CURVE ( 'NONE', #43477, #9283, #26899, .T. ) ;
#61366 = CARTESIAN_POINT ( 'NONE',  ( 15.50000000000000000, -15.50000000000000000, -22.50000000000000000 ) ) ;
#61367 = DIRECTION ( 'NONE',  ( 0.000000000000000000, 0.000000000000000000, -1.000000000000000000 ) ) ;
#61368 = VERTEX_POINT ( 'NONE', #10976 ) ;
#61369 = EDGE_CURVE ( 'NONE', #34713, #17836, #38542, .T. ) ;
#61370 = ORIENTED_EDGE ( 'NONE', *, *, #26124, .F. ) ;
#61371 = ORIENTED_EDGE ( 'NONE', *, *, #55404, .F. ) ;
#61372 = DIRECTION ( 'NONE',  ( 0.000000000000000000, 1.000000000000000000, 0.000000000000000000 ) ) ;
#61373 = ADVANCED_FACE ( 'NONE', ( #11309, #37847 ), #69322, .T. ) ;
#61375 = ORIENTED_EDGE ( 'NONE', *, *, #59894, .F. ) ;
#61374 = DIRECTION ( 'NONE',  ( 0.000000000000000000, 0.000000000000000000, 1.000000000000000000 ) ) ;
#61376 = CARTESIAN_POINT ( 'NONE',  ( -9.915476262117259409, 0.9414762621171833823, 54.00000000000000711 ) ) ;
#61377 = CARTESIAN_POINT ( 'NONE',  ( -7.250000000000000000, -7.449999999999998401, -8.500000000000000000 ) ) ;
#61378 = ORIENTED_EDGE ( 'NONE', *, *, #45580, .T. ) ;
#61379 = ORIENTED_EDGE ( 'NONE', *, *, #62749, .T. ) ;
#61380 = EDGE_CURVE ( 'NONE', #58636, #44788, #32552, .T. ) ;
#61381 = DIRECTION ( 'NONE',  ( 0.000000000000000000, -0.9938079899998859545, -0.1111111111112941946 ) ) ;
#61382 = FACE_OUTER_BOUND ( 'NONE', #63137, .T. ) ;
#61383 = CARTESIAN_POINT ( 'NONE',  ( 280.0000000000000000, -20.40000000000000213, 20.00000000000000000 ) ) ;
#61384 = VECTOR ( 'NONE', #3527, 1000.000000000000000 ) ;
#61385 = VECTOR ( 'NONE', #63484, 1000.000000000000000 ) ;
#61386 = PLANE ( 'NONE',  #13023 ) ;
#61387 = DIRECTION ( 'NONE',  ( -0.3479852726768748461, 0.000000000000000000, 0.9375000000000006661 ) ) ;
#61389 = ORIENTED_EDGE ( 'NONE', *, *, #16062, .F. ) ;
#61388 = DIRECTION ( 'NONE',  ( 0.000000000000000000, -0.7071067811865474617, -0.7071067811865474617 ) ) ;
#61390 = ORIENTED_EDGE ( 'NONE', *, *, #32864, .F. ) ;
#61391 = CARTESIAN_POINT ( 'NONE',  ( 111.9257688011041836, 10.00000000000000000, 281.4830310981151911 ) ) ;
#61392 = AXIS2_PLACEMENT_3D ( 'NONE', #69375, #30494, #58777 ) ;
#61394 = CIRCLE ( 'NONE', #8314, 1.224999999999998757 ) ;
#61393 = DIRECTION ( 'NONE',  ( 0.000000000000000000, 0.000000000000000000, -1.000000000000000000 ) ) ;
#61395 = DIRECTION ( 'NONE',  ( -3.016910393003147986E-15, 1.000000000000000000, 3.673940397442059868E-16 ) ) ;
#61396 = AXIS2_PLACEMENT_3D ( 'NONE', #53838, #38938, #60841 ) ;
#61397 = VECTOR ( 'NONE', #20223, 999.9999999999998863 ) ;
#61398 = LINE ( 'NONE', #55431, #25195 ) ;
#61399 = VERTEX_POINT ( 'NONE', #64039 ) ;
#61400 = DIRECTION ( 'NONE',  ( -1.000000000000000000, 0.000000000000000000, 0.000000000000000000 ) ) ;
#61401 = FACE_OUTER_BOUND ( 'NONE', #63427, .T. ) ;
#61402 = EDGE_CURVE ( 'NONE', #26427, #59671, #69666, .T. ) ;
#61403 = DIRECTION ( 'NONE',  ( 0.000000000000000000, 0.000000000000000000, -1.000000000000000000 ) ) ;
#61404 = CARTESIAN_POINT ( 'NONE',  ( 11.48848345035342078, 11.07551654964652599, 455.0000000000000568 ) ) ;
#61405 = EDGE_CURVE ( 'NONE', #32707, #29553, #19982, .T. ) ;
#61406 = DIRECTION ( 'NONE',  ( 1.000000000000000000, -0.000000000000000000, 0.000000000000000000 ) ) ;
#61407 = EDGE_CURVE ( 'NONE', #26866, #50489, #66260, .T. ) ;
#61408 = LINE ( 'NONE', #14400, #35253 ) ;
#61409 = CIRCLE ( 'NONE', #46746, 0.9999999999999991118 ) ;
#61410 = DIRECTION ( 'NONE',  ( -3.491481338843133355E-15, -1.000000000000000000, -1.836970198721029934E-16 ) ) ;
#61411 = ORIENTED_EDGE ( 'NONE', *, *, #24633, .F. ) ;
#61412 = DIRECTION ( 'NONE',  ( 0.000000000000000000, 1.000000000000000000, 0.000000000000000000 ) ) ;
#61413 = LINE ( 'NONE', #39846, #48699 ) ;
#61414 = VERTEX_POINT ( 'NONE', #10278 ) ;
#61415 = DIRECTION ( 'NONE',  ( 0.000000000000000000, 0.000000000000000000, 1.000000000000000000 ) ) ;
#61416 = FACE_OUTER_BOUND ( 'NONE', #16931, .T. ) ;
#61417 = CARTESIAN_POINT ( 'NONE',  ( -23.48000000000000043, -15.50000000000000000, -26.00000000000000355 ) ) ;
#61418 = CARTESIAN_POINT ( 'NONE',  ( -29.50000000000000355, -12.00000000000000000, -11.03137303340310282 ) ) ;
#61419 = DIRECTION ( 'NONE',  ( -1.000000000000000000, 0.000000000000000000, 0.000000000000000000 ) ) ;
#61420 = ORIENTED_EDGE ( 'NONE', *, *, #30749, .T. ) ;
#61421 = LINE ( 'NONE', #33867, #29605 ) ;
#61422 = ORIENTED_EDGE ( 'NONE', *, *, #67251, .T. ) ;
#61423 = CARTESIAN_POINT ( 'NONE',  ( -9.404046420174124066, 1.853252480934674873, 455.0000000000000568 ) ) ;
#61424 = ORIENTED_EDGE ( 'NONE', *, *, #48362, .T. ) ;
#61425 = VECTOR ( 'NONE', #63805, 1000.000000000000000 ) ;
#61426 = DIRECTION ( 'NONE',  ( -1.000000000000000000, 0.000000000000000000, 0.000000000000000000 ) ) ;
#61427 = AXIS2_PLACEMENT_3D ( 'NONE', #25450, #8830, #3535 ) ;
#61428 = CARTESIAN_POINT ( 'NONE',  ( 7.532023737882817649, -3.848229544836335947, 26.00000000000000711 ) ) ;
#61429 = FACE_OUTER_BOUND ( 'NONE', #44667, .T. ) ;
#61430 = VERTEX_POINT ( 'NONE', #21927 ) ;
#61431 = VERTEX_POINT ( 'NONE', #16973 ) ;
#61432 = DIRECTION ( 'NONE',  ( -1.356437060717832013E-15, -1.000000000000000000, -1.836970198721033878E-16 ) ) ;
#61433 = EDGE_LOOP ( 'NONE', ( #43692, #48141, #52901, #43233 ) ) ;
#61434 = EDGE_LOOP ( 'NONE', ( #4558, #13964, #38936, #47424 ) ) ;
#61435 = EDGE_CURVE ( 'NONE', #48126, #42371, #36912, .T. ) ;
#61436 = LINE ( 'NONE', #2751, #41722 ) ;
#61437 = CYLINDRICAL_SURFACE ( 'NONE', #20086, 1.000000000000000000 ) ;
#61438 = VECTOR ( 'NONE', #65621, 1000.000000000000000 ) ;
#61439 = VECTOR ( 'NONE', #17737, 1000.000000000000114 ) ;
#61440 = CARTESIAN_POINT ( 'NONE',  ( 38.90000000000000568, 13.66939075806899240, -20.79999999999999361 ) ) ;
#61441 = EDGE_LOOP ( 'NONE', ( #52275, #34111, #16462, #346, #17203, #53232, #62725 ) ) ;
#61442 = EDGE_CURVE ( 'NONE', #14683, #23727, #54799, .T. ) ;
#61443 = FACE_OUTER_BOUND ( 'NONE', #67287, .T. ) ;
#61445 = CARTESIAN_POINT ( 'NONE',  ( 11.32648345035337734, -7.606483450353492159, 455.0000000000000568 ) ) ;
#61444 = CARTESIAN_POINT ( 'NONE',  ( 25.50000000000000355, 0.000000000000000000, 20.24999999999999645 ) ) ;
#61446 = VECTOR ( 'NONE', #63670, 1000.000000000000000 ) ;
#61447 =( GEOMETRIC_REPRESENTATION_CONTEXT ( 3 ) GLOBAL_UNCERTAINTY_ASSIGNED_CONTEXT ( ( #52909 ) ) GLOBAL_UNIT_ASSIGNED_CONTEXT ( ( #33960, #62229, #12730 ) ) REPRESENTATION_CONTEXT ( 'NONE', 'WORKASPACE' ) );
#61449 = ORIENTED_EDGE ( 'NONE', *, *, #12636, .T. ) ;
#61448 = AXIS2_PLACEMENT_3D ( 'NONE', #44982, #60555, #38651 ) ;
#61451 = ORIENTED_EDGE ( 'NONE', *, *, #52313, .F. ) ;
#61450 = CARTESIAN_POINT ( 'NONE',  ( 15.90000000000000036, -0.000000000000000000, -20.80000000000000426 ) ) ;
#61452 = EDGE_CURVE ( 'NONE', #13815, #25255, #33228, .T. ) ;
#61453 = ORIENTED_EDGE ( 'NONE', *, *, #53715, .T. ) ;
#61454 = EDGE_CURVE ( 'NONE', #13193, #45555, #21093, .T. ) ;
#61455 = DIRECTION ( 'NONE',  ( 1.000000000000000000, 0.000000000000000000, 0.000000000000000000 ) ) ;
#61456 = VECTOR ( 'NONE', #45534, 1000.000000000000000 ) ;
#61457 = EDGE_CURVE ( 'NONE', #16734, #15307, #8672, .T. ) ;
#61458 = EDGE_CURVE ( 'NONE', #42896, #55318, #44510, .T. ) ;
#61459 = CARTESIAN_POINT ( 'NONE',  ( 10.20488345035338007, -11.08848345035349325, 455.0000000000000568 ) ) ;
#61460 = ORIENTED_EDGE ( 'NONE', *, *, #34098, .T. ) ;
#61461 = CARTESIAN_POINT ( 'NONE',  ( -7.249999999999995559, 8.250000000000001776, -5.000000000000000000 ) ) ;
#61462 = ADVANCED_FACE ( 'NONE', ( #34604 ), #22958, .F. ) ;
#61463 = DIRECTION ( 'NONE',  ( 1.000000000000000000, 0.000000000000000000, 0.000000000000000000 ) ) ;
#61464 = VERTEX_POINT ( 'NONE', #44866 ) ;
#61465 = ORIENTED_EDGE ( 'NONE', *, *, #31572, .T. ) ;
#61466 = CIRCLE ( 'NONE', #26525, 0.5000000000009372503 ) ;
#61467 = CARTESIAN_POINT ( 'NONE',  ( 2.906483450353420039, 10.91351654964658913, 455.0000000000000568 ) ) ;
#61468 = LINE ( 'NONE', #13026, #715 ) ;
#61469 = ORIENTED_EDGE ( 'NONE', *, *, #759, .T. ) ;
#61470 = FACE_OUTER_BOUND ( 'NONE', #51377, .T. ) ;
#61471 = PLANE ( 'NONE',  #47054 ) ;
#61472 = FACE_BOUND ( 'NONE', #24302, .T. ) ;
#61473 = ORIENTED_EDGE ( 'NONE', *, *, #63353, .F. ) ;
#61474 = CARTESIAN_POINT ( 'NONE',  ( -7.250000000000000000, -7.449999999999998401, -10.50000000000000000 ) ) ;
#61475 = DIRECTION ( 'NONE',  ( -0.000000000000000000, -0.000000000000000000, -1.000000000000000000 ) ) ;
#61477 = ORIENTED_EDGE ( 'NONE', *, *, #21421, .F. ) ;
#61476 = DIRECTION ( 'NONE',  ( 3.491481338843133355E-15, 1.000000000000000000, 1.836970198721029934E-16 ) ) ;
#61479 = ORIENTED_EDGE ( 'NONE', *, *, #5361, .T. ) ;
#61478 = DIRECTION ( 'NONE',  ( -1.000000000000000000, 0.000000000000000000, 0.000000000000000000 ) ) ;
#61480 = CARTESIAN_POINT ( 'NONE',  ( 8.711985858128693749, -8.093267424590470327, 54.00000000000000711 ) ) ;
#61481 = CARTESIAN_POINT ( 'NONE',  ( -8.227189898828745740, 1.620245201994245487, 54.00000000000000711 ) ) ;
#61482 = AXIS2_PLACEMENT_3D ( 'NONE', #10490, #54333, #47976 ) ;
#61483 = LINE ( 'NONE', #56544, #35842 ) ;
#61484 = CARTESIAN_POINT ( 'NONE',  ( 30.00000000000000000, -17.14999999999900027, -26.64999999999900027 ) ) ;
#61485 = DIRECTION ( 'NONE',  ( 0.000000000000000000, 0.000000000000000000, 1.000000000000000000 ) ) ;
#61486 = VERTEX_POINT ( 'NONE', #39221 ) ;
#61487 = DIRECTION ( 'NONE',  ( 0.3479852726768751237, 0.000000000000000000, -0.9375000000000004441 ) ) ;
#61488 = DIRECTION ( 'NONE',  ( -1.000000000000000000, 3.016910393003147986E-15, 0.000000000000000000 ) ) ;
#61489 = DIRECTION ( 'NONE',  ( 0.000000000000000000, -1.000000000000000000, 0.000000000000000000 ) ) ;
#61491 = ORIENTED_EDGE ( 'NONE', *, *, #23918, .F. ) ;
#61490 = DIRECTION ( 'NONE',  ( 0.000000000000000000, 0.000000000000000000, -1.000000000000000000 ) ) ;
#61492 = ADVANCED_FACE ( 'NONE', ( #11989 ), #28957, .F. ) ;
#61493 = VECTOR ( 'NONE', #1419, 1000.000000000000000 ) ;
#61494 = CIRCLE ( 'NONE', #31038, 9.300000000000002487 ) ;
#61495 = DIRECTION ( 'NONE',  ( 0.000000000000000000, 1.000000000000000000, 0.000000000000000000 ) ) ;
#61496 = EDGE_CURVE ( 'NONE', #55024, #29674, #53874, .T. ) ;
#61497 = CARTESIAN_POINT ( 'NONE',  ( -4.193516549646831848, -11.12648345035344377, 455.0000000000000568 ) ) ;
#61498 = ADVANCED_FACE ( 'NONE', ( #60784 ), #55147, .F. ) ;
#61499 = VECTOR ( 'NONE', #64007, 1000.000000000000114 ) ;
#61500 = ORIENTED_EDGE ( 'NONE', *, *, #58200, .T. ) ;
#61501 = CARTESIAN_POINT ( 'NONE',  ( 6.849523737882817542, -10.31452373788282095, 54.00000000000000711 ) ) ;
#61502 = CARTESIAN_POINT ( 'NONE',  ( 282.6457513110646005, -25.50000000000000355, -17.00000000000000000 ) ) ;
#61504 = VERTEX_POINT ( 'NONE', #61118 ) ;
#61503 = ADVANCED_FACE ( 'NONE', ( #12327 ), #65750, .F. ) ;
#61505 = DIRECTION ( 'NONE',  ( 0.000000000000000000, -0.9921567416492215186, 0.1249999999999996531 ) ) ;
#61506 = CARTESIAN_POINT ( 'NONE',  ( 11.90000000000000036, 20.60000000000000142, -13.86939075806900057 ) ) ;
#61507 = VECTOR ( 'NONE', #29120, 1000.000000000000114 ) ;
#61508 = CARTESIAN_POINT ( 'NONE',  ( -7.450000000000001954, -7.249999999999998224, -23.50000000000000000 ) ) ;
#61509 = DIRECTION ( 'NONE',  ( 0.000000000000000000, 0.7046037717862339012, 0.7096009616570518874 ) ) ;
#61510 = LINE ( 'NONE', #22666, #37668 ) ;
#61511 = VECTOR ( 'NONE', #66305, 1000.000000000000000 ) ;
#61512 = EDGE_LOOP ( 'NONE', ( #11121, #61625, #56902, #57742 ) ) ;
#61513 = DIRECTION ( 'NONE',  ( 0.000000000000000000, 1.000000000000000000, 0.000000000000000000 ) ) ;
#61514 = EDGE_LOOP ( 'NONE', ( #28852, #2629, #43745, #59531 ) ) ;
#61515 = ORIENTED_EDGE ( 'NONE', *, *, #60758, .F. ) ;
#61516 = VECTOR ( 'NONE', #8351, 1000.000000000000000 ) ;
#61517 = DIRECTION ( 'NONE',  ( 1.836970198721029934E-16, 1.836970198721010706E-16, -1.000000000000000000 ) ) ;
#61518 = DIRECTION ( 'NONE',  ( 0.000000000000000000, 1.000000000000000000, 0.000000000000000000 ) ) ;
#61520 = CARTESIAN_POINT ( 'NONE',  ( 18.85410196625000268, -15.50000000000000000, 21.50000000000000000 ) ) ;
#61519 = DIRECTION ( 'NONE',  ( 0.000000000000000000, 0.000000000000000000, 1.000000000000000000 ) ) ;
#61521 = ORIENTED_EDGE ( 'NONE', *, *, #15383, .F. ) ;
#61522 = EDGE_LOOP ( 'NONE', ( #36662, #47383, #35932, #28410, #57028 ) ) ;
#61523 = CARTESIAN_POINT ( 'NONE',  ( -25.50000000000000355, -5.578999999999999737, -24.12099999999999511 ) ) ;
#61524 = AXIS2_PLACEMENT_3D ( 'NONE', #35945, #57852, #52567 ) ;
#61525 = ORIENTED_EDGE ( 'NONE', *, *, #41037, .F. ) ;
#61526 = CARTESIAN_POINT ( 'NONE',  ( 4.396432944014577515, 8.593516549646585290, 455.0000000000000568 ) ) ;
#61527 = LINE ( 'NONE', #55894, #41082 ) ;
#61528 = LINE ( 'NONE', #23714, #11636 ) ;
#61529 = DIRECTION ( 'NONE',  ( 0.000000000000000000, 0.000000000000000000, -1.000000000000000000 ) ) ;
#61531 = CARTESIAN_POINT ( 'NONE',  ( 9.899999999999998579, -21.00000000000000000, 13.86939075806900057 ) ) ;
#61530 = DIRECTION ( 'NONE',  ( -0.000000000000000000, -0.000000000000000000, -1.000000000000000000 ) ) ;
#61532 = ORIENTED_EDGE ( 'NONE', *, *, #15914, .T. ) ;
#61534 = ORIENTED_EDGE ( 'NONE', *, *, #39349, .T. ) ;
#61533 = CARTESIAN_POINT ( 'NONE',  ( 283.0000000000000568, -53.81370849898476649, -17.35424868893542438 ) ) ;
#61535 = AXIS2_PLACEMENT_3D ( 'NONE', #24141, #34374, #45343 ) ;
#61536 = ORIENTED_EDGE ( 'NONE', *, *, #52887, .T. ) ;
#61537 = ORIENTED_EDGE ( 'NONE', *, *, #34771, .T. ) ;
#61538 = AXIS2_PLACEMENT_3D ( 'NONE', #53380, #53033, #43437 ) ;
#61539 = EDGE_CURVE ( 'NONE', #49372, #69377, #1731, .T. ) ;
#61540 = FACE_OUTER_BOUND ( 'NONE', #68967, .T. ) ;
#61541 = VECTOR ( 'NONE', #16103, 1000.000000000000000 ) ;
#61542 = VECTOR ( 'NONE', #59699, 1000.000000000000000 ) ;
#61544 = DIRECTION ( 'NONE',  ( 0.000000000000000000, 0.000000000000000000, 1.000000000000000000 ) ) ;
#61543 = VECTOR ( 'NONE', #11895, 1000.000000000000000 ) ;
#61545 = EDGE_CURVE ( 'NONE', #42371, #50215, #2435, .T. ) ;
#61546 = AXIS2_PLACEMENT_3D ( 'NONE', #47739, #25837, #68964 ) ;
#61547 = VERTEX_POINT ( 'NONE', #40263 ) ;
#61548 = ORIENTED_EDGE ( 'NONE', *, *, #27320, .T. ) ;
#61549 = VECTOR ( 'NONE', #69918, 1000.000000000000000 ) ;
#61550 = AXIS2_PLACEMENT_3D ( 'NONE', #3995, #68706, #14595 ) ;
#61551 = DIRECTION ( 'NONE',  ( -0.000000000000000000, 3.673940397442059868E-16, -1.000000000000000000 ) ) ;
#61552 = DIRECTION ( 'NONE',  ( 0.000000000000000000, 0.000000000000000000, -1.000000000000000000 ) ) ;
#61553 = EDGE_LOOP ( 'NONE', ( #56300, #3576, #63762, #1285 ) ) ;
#61554 = ORIENTED_EDGE ( 'NONE', *, *, #31104, .T. ) ;
#61555 = DIRECTION ( 'NONE',  ( -1.000000000000000000, 0.000000000000000000, 0.000000000000000000 ) ) ;
#61556 = CIRCLE ( 'NONE', #2820, 3.499999999999056310 ) ;
#61557 = DIRECTION ( 'NONE',  ( -1.000000000000000000, 5.120954910632640039E-15, 1.881408311965255020E-30 ) ) ;
#61558 = VERTEX_POINT ( 'NONE', #33906 ) ;
#61559 = AXIS2_PLACEMENT_3D ( 'NONE', #46471, #68048, #35872 ) ;
#61560 = CARTESIAN_POINT ( 'NONE',  ( -7.342976262117259623, 6.651770455163663165, 54.00000000000000711 ) ) ;
#61561 = LINE ( 'NONE', #41407, #4639 ) ;
#61563 = ORIENTED_EDGE ( 'NONE', *, *, #63829, .F. ) ;
#61562 = DIRECTION ( 'NONE',  ( 1.000000000000000000, 0.000000000000000000, 0.000000000000000000 ) ) ;
#61564 = VECTOR ( 'NONE', #30116, 1000.000000000000000 ) ;
#61565 = ORIENTED_EDGE ( 'NONE', *, *, #67090, .F. ) ;
#61566 = DIRECTION ( 'NONE',  ( 0.000000000000000000, 0.000000000000000000, 1.000000000000000000 ) ) ;
#61567 = DIRECTION ( 'NONE',  ( 1.000000000000000000, -5.626525616968433909E-15, -1.836970198721040534E-16 ) ) ;
#61568 = CARTESIAN_POINT ( 'NONE',  ( 2.544523737882785852, -9.737023737882799068, 54.00000000000000711 ) ) ;
#61569 = CARTESIAN_POINT ( 'NONE',  ( 4.186483450353423841, 11.99351654964658742, 455.0000000000000568 ) ) ;
#61570 = CARTESIAN_POINT ( 'NONE',  ( 14.25000000000000000, -2.500000000000000000, 21.77831216351300014 ) ) ;
#61571 = CARTESIAN_POINT ( 'NONE',  ( -11.18999999999999950, -11.18999999999999950, -5.000000000000000000 ) ) ;
#61572 = CARTESIAN_POINT ( 'NONE',  ( -6.822336235477446387, 6.350872789121265072, 54.00000000000000711 ) ) ;
#61573 = ORIENTED_EDGE ( 'NONE', *, *, #12518, .T. ) ;
#61574 = LINE ( 'NONE', #11756, #17938 ) ;
#61576 = ORIENTED_EDGE ( 'NONE', *, *, #36596, .T. ) ;
#61575 = DIRECTION ( 'NONE',  ( 0.000000000000000000, 1.000000000000000000, 0.000000000000000000 ) ) ;
#61577 = CARTESIAN_POINT ( 'NONE',  ( -16.75000000000000000, -2.500000000000000000, 21.77831216351300014 ) ) ;
#61578 = CARTESIAN_POINT ( 'NONE',  ( 4.622483450353394474, 3.593516549646586622, 455.0000000000000568 ) ) ;
#61579 = CIRCLE ( 'NONE', #16442, 1.399999999999998579 ) ;
#61580 = DIRECTION ( 'NONE',  ( 0.000000000000000000, -1.000000000000000000, 0.000000000000000000 ) ) ;
#61581 = PLANE ( 'NONE',  #27281 ) ;
#61582 = CYLINDRICAL_SURFACE ( 'NONE', #56271, 0.5000000000001374456 ) ;
#61583 = CIRCLE ( 'NONE', #41256, 4.000000000000000888 ) ;
#61584 = VERTEX_POINT ( 'NONE', #23995 ) ;
#61586 = ORIENTED_EDGE ( 'NONE', *, *, #17394, .F. ) ;
#61585 = EDGE_CURVE ( 'NONE', #29173, #36079, #61840, .T. ) ;
#61587 = VECTOR ( 'NONE', #6910, 1000.000000000000000 ) ;
#61588 = DIRECTION ( 'NONE',  ( -0.000000000000000000, -0.000000000000000000, -1.000000000000000000 ) ) ;
#61589 = DIRECTION ( 'NONE',  ( -0.000000000000000000, -0.000000000000000000, -1.000000000000000000 ) ) ;
#61590 = AXIS2_PLACEMENT_3D ( 'NONE', #9678, #31260, #52832 ) ;
#61591 = CIRCLE ( 'NONE', #4044, 2.250000000000001776 ) ;
#61592 = VECTOR ( 'NONE', #56265, 1000.000000000000000 ) ;
#61593 = DIRECTION ( 'NONE',  ( 1.000000000000000000, 0.000000000000000000, 0.000000000000000000 ) ) ;
#61594 = ORIENTED_EDGE ( 'NONE', *, *, #2097, .F. ) ;
#61595 = CARTESIAN_POINT ( 'NONE',  ( -7.450000000000001954, -7.249999999999998224, -25.00000000000000000 ) ) ;
#61596 = ORIENTED_EDGE ( 'NONE', *, *, #26840, .F. ) ;
#61597 = ORIENTED_EDGE ( 'NONE', *, *, #26010, .T. ) ;
#61598 = CARTESIAN_POINT ( 'NONE',  ( -15.50000000000000000, -0.1999999999999999556, 21.05000000000000071 ) ) ;
#61600 = DIRECTION ( 'NONE',  ( -0.000000000000000000, 0.000000000000000000, 1.000000000000000000 ) ) ;
#61599 = AXIS2_PLACEMENT_3D ( 'NONE', #22471, #44014, #60629 ) ;
#61601 = VECTOR ( 'NONE', #66414, 1000.000000000000000 ) ;
#61602 = AXIS2_PLACEMENT_3D ( 'NONE', #56250, #34671, #7794 ) ;
#61604 = ORIENTED_EDGE ( 'NONE', *, *, #47376, .F. ) ;
#61603 = ADVANCED_FACE ( 'NONE', ( #38872 ), #6693, .F. ) ;
#61605 = DIRECTION ( 'NONE',  ( -0.7071067811865401342, 0.7071067811865550112, 0.000000000000000000 ) ) ;
#61606 = AXIS2_PLACEMENT_3D ( 'NONE', #4541, #20445, #47664 ) ;
#61607 = CARTESIAN_POINT ( 'NONE',  ( -25.50000000000000355, 0.000000000000000000, 24.75000000000000000 ) ) ;
#61608 = ADVANCED_FACE ( 'NONE', ( #13390 ), #60430, .F. ) ;
#61609 = DIRECTION ( 'NONE',  ( 0.000000000000000000, 0.000000000000000000, -1.000000000000000000 ) ) ;
#61610 = ORIENTED_EDGE ( 'NONE', *, *, #62648, .F. ) ;
#61611 = EDGE_LOOP ( 'NONE', ( #67838, #14092, #34726, #56582 ) ) ;
#61613 = ORIENTED_EDGE ( 'NONE', *, *, #28667, .T. ) ;
#61612 = DIRECTION ( 'NONE',  ( -1.079558018506126467E-14, -1.000000000000000000, 0.000000000000000000 ) ) ;
#61614 = EDGE_LOOP ( 'NONE', ( #53204, #67724, #898, #8650 ) ) ;
#61615 = PRODUCT_DEFINITION_SHAPE ( 'NONE', 'NONE',  #18876 ) ;
#61616 = VECTOR ( 'NONE', #38496, 999.9999999999998863 ) ;
#61617 = DIRECTION ( 'NONE',  ( 0.000000000000000000, 1.000000000000000000, 0.000000000000000000 ) ) ;
#61618 = CARTESIAN_POINT ( 'NONE',  ( 9.899999999999998579, 20.60000000000000142, 13.86939075806899702 ) ) ;
#61619 = DIRECTION ( 'NONE',  ( 0.000000000000000000, 0.000000000000000000, 1.000000000000000000 ) ) ;
#61620 = CARTESIAN_POINT ( 'NONE',  ( 7.000000000000000000, -26.50000000000000000, 5.530822723609939651 ) ) ;
#61621 = AXIS2_PLACEMENT_3D ( 'NONE', #11582, #651, #32491 ) ;
#61622 = DIRECTION ( 'NONE',  ( 1.000000000000000000, 0.000000000000000000, 0.000000000000000000 ) ) ;
#61623 = CARTESIAN_POINT ( 'NONE',  ( 283.0000000000000568, -28.94999999999999929, -13.50000000000000000 ) ) ;
#61624 = EDGE_LOOP ( 'NONE', ( #45793, #12784, #58434, #62169 ) ) ;
#61625 = ORIENTED_EDGE ( 'NONE', *, *, #69075, .F. ) ;
#61626 = ORIENTED_EDGE ( 'NONE', *, *, #30749, .F. ) ;
#61627 = ORIENTED_EDGE ( 'NONE', *, *, #8385, .T. ) ;
#61628 = LINE ( 'NONE', #24162, #17507 ) ;
#61629 = FACE_OUTER_BOUND ( 'NONE', #17955, .T. ) ;
#61631 = EDGE_CURVE ( 'NONE', #47150, #53417, #39556, .T. ) ;
#61630 = CARTESIAN_POINT ( 'NONE',  ( -9.690000000000001279, -9.690000000000001279, 0.000000000000000000 ) ) ;
#61632 = DIRECTION ( 'NONE',  ( 0.000000000000000000, 0.000000000000000000, -1.000000000000000000 ) ) ;
#61633 = EDGE_CURVE ( 'NONE', #27877, #26707, #15505, .T. ) ;
#61634 = ORIENTED_EDGE ( 'NONE', *, *, #18671, .T. ) ;
#61635 = EDGE_LOOP ( 'NONE', ( #58772, #16996, #51146, #29830, #63136, #45110 ) ) ;
#61636 = EDGE_CURVE ( 'NONE', #16217, #22012, #53599, .T. ) ;
#61637 = VECTOR ( 'NONE', #30211, 1000.000000000000000 ) ;
#61638 = ORIENTED_EDGE ( 'NONE', *, *, #2086, .T. ) ;
#61639 = DIRECTION ( 'NONE',  ( 0.000000000000000000, 1.000000000000000000, 0.000000000000000000 ) ) ;
#61640 = ORIENTED_EDGE ( 'NONE', *, *, #36280, .F. ) ;
#61641 = ADVANCED_FACE ( 'NONE', ( #42976 ), #10111, .F. ) ;
#61642 = AXIS2_PLACEMENT_3D ( 'NONE', #56405, #56754, #2318 ) ;
#61643 = ORIENTED_EDGE ( 'NONE', *, *, #54541, .F. ) ;
#61645 = ORIENTED_EDGE ( 'NONE', *, *, #3397, .T. ) ;
#61644 = PRODUCT_DEFINITION ( 'UNKNOWN', '', #3124, #33201 ) ;
#61646 = ORIENTED_EDGE ( 'NONE', *, *, #34820, .T. ) ;
#61647 = AXIS2_PLACEMENT_3D ( 'NONE', #11106, #161, #11782 ) ;
#61648 = CARTESIAN_POINT ( 'NONE',  ( 7.450000000000003730, -7.249999999999997335, -22.00000000000000000 ) ) ;
#61649 = EDGE_CURVE ( 'NONE', #47806, #34716, #65173, .T. ) ;
#61651 = ORIENTED_EDGE ( 'NONE', *, *, #32474, .T. ) ;
#61650 = PLANE ( 'NONE',  #55956 ) ;
#61653 = ORIENTED_EDGE ( 'NONE', *, *, #60366, .F. ) ;
#61652 = EDGE_CURVE ( 'NONE', #25093, #58003, #56106, .T. ) ;
#61654 = CARTESIAN_POINT ( 'NONE',  ( 25.50000000000000355, -5.200000000000001066, 24.50000000000000000 ) ) ;
#61655 = CIRCLE ( 'NONE', #58296, 0.2000000000000005107 ) ;
#61656 = VECTOR ( 'NONE', #52779, 1000.000000000000000 ) ;
#61657 = AXIS2_PLACEMENT_3D ( 'NONE', #11310, #27, #37161 ) ;
#61658 = LINE ( 'NONE', #41141, #47613 ) ;
#61659 = DIRECTION ( 'NONE',  ( -1.000000000000000000, 0.000000000000000000, 0.000000000000000000 ) ) ;
#61661 = VERTEX_POINT ( 'NONE', #51218 ) ;
#61660 = DIRECTION ( 'NONE',  ( -0.000000000000000000, -0.000000000000000000, -1.000000000000000000 ) ) ;
#61662 = ORIENTED_EDGE ( 'NONE', *, *, #46039, .F. ) ;
#61663 = CIRCLE ( 'NONE', #9754, 0.2000000000000005107 ) ;
#61664 = AXIS2_PLACEMENT_3D ( 'NONE', #50599, #12400, #65817 ) ;
#61665 = VECTOR ( 'NONE', #6343, 1000.000000000000000 ) ;
#61666 = FACE_OUTER_BOUND ( 'NONE', #17364, .T. ) ;
#61667 = CARTESIAN_POINT ( 'NONE',  ( 19.90000000000000213, -21.00000000000000000, 13.86939075806900057 ) ) ;
#61668 = DIRECTION ( 'NONE',  ( -1.000000000000000000, 0.000000000000000000, 0.000000000000000000 ) ) ;
#61669 = VECTOR ( 'NONE', #26368, 1000.000000000000000 ) ;
#61670 = ORIENTED_EDGE ( 'NONE', *, *, #57219, .F. ) ;
#61671 = LINE ( 'NONE', #34795, #38267 ) ;
#61672 = DIRECTION ( 'NONE',  ( 1.000000000000000000, 0.000000000000000000, 0.000000000000000000 ) ) ;
#61673 = CARTESIAN_POINT ( 'NONE',  ( 7.450000000000003730, -7.249999999999997335, -16.50000000000000000 ) ) ;
#61674 = EDGE_CURVE ( 'NONE', #32938, #42459, #63513, .T. ) ;
#61675 = EDGE_LOOP ( 'NONE', ( #57040, #30055, #40920, #65414 ) ) ;
#61676 = DIRECTION ( 'NONE',  ( 0.000000000000000000, 0.000000000000000000, 1.000000000000000000 ) ) ;
#61677 = CARTESIAN_POINT ( 'NONE',  ( -29.50000000000000355, -12.00000000000000000, 10.52786404500095863 ) ) ;
#61678 = DIRECTION ( 'NONE',  ( 1.836970198721029934E-16, 1.836970198721010706E-16, -1.000000000000000000 ) ) ;
#61679 = EDGE_CURVE ( 'NONE', #44259, #39509, #53918, .T. ) ;
#61680 = ORIENTED_EDGE ( 'NONE', *, *, #49001, .T. ) ;
#61681 = DIRECTION ( 'NONE',  ( 1.000000000000000000, 0.000000000000000000, 0.000000000000000000 ) ) ;
#61682 = LINE ( 'NONE', #13248, #55925 ) ;
#61683 = LINE ( 'NONE', #41440, #60500 ) ;
#61684 = ORIENTED_EDGE ( 'NONE', *, *, #18278, .F. ) ;
#61685 = PLANE ( 'NONE',  #5614 ) ;
#61686 = DIRECTION ( 'NONE',  ( 0.000000000000000000, 1.000000000000000000, 0.000000000000000000 ) ) ;
#61687 = AXIS2_PLACEMENT_3D ( 'NONE', #50289, #29416, #23429 ) ;
#61688 = CARTESIAN_POINT ( 'NONE',  ( -8.250000000000001776, -8.249999999999998224, -26.00000000000001066 ) ) ;
#61689 = LINE ( 'NONE', #2304, #39148 ) ;
#61690 = LINE ( 'NONE', #19264, #13844 ) ;
#61691 = ORIENTED_EDGE ( 'NONE', *, *, #37552, .F. ) ;
#61692 = DIRECTION ( 'NONE',  ( -1.000000000000000000, 0.000000000000000000, 0.000000000000000000 ) ) ;
#61693 = CARTESIAN_POINT ( 'NONE',  ( 49.00000000000000000, -21.00000000000000000, 13.86939075806900057 ) ) ;
#61694 = DIRECTION ( 'NONE',  ( 0.000000000000000000, -3.673940397442059868E-16, 1.000000000000000000 ) ) ;
#61695 = AXIS2_PLACEMENT_3D ( 'NONE', #32898, #34260, #11657 ) ;
#61696 = VECTOR ( 'NONE', #41054, 1000.000000000000000 ) ;
#61697 = CARTESIAN_POINT ( 'NONE',  ( 0.5000000000000008882, -42.49999999999997868, -26.49999999999997868 ) ) ;
#61698 = EDGE_CURVE ( 'NONE', #68424, #49997, #40307, .T. ) ;
#61699 = CARTESIAN_POINT ( 'NONE',  ( 14.10805890929250062, -5.000000000000000000, 26.25000000000000000 ) ) ;
#61700 = ORIENTED_EDGE ( 'NONE', *, *, #21028, .F. ) ;
#61702 = VERTEX_POINT ( 'NONE', #47245 ) ;
#61701 = CARTESIAN_POINT ( 'NONE',  ( 8.750000000000005329, 7.250000000000000888, -26.00000000000001066 ) ) ;
#61703 = AXIS2_PLACEMENT_3D ( 'NONE', #52944, #59961, #55028 ) ;
#61704 = VECTOR ( 'NONE', #23259, 1000.000000000000000 ) ;
#61705 = CIRCLE ( 'NONE', #7549, 0.1749999999999998224 ) ;
#61706 = CARTESIAN_POINT ( 'NONE',  ( 49.00000000000000000, -21.00000000000000000, 13.86939075806900057 ) ) ;
#61707 = CYLINDRICAL_SURFACE ( 'NONE', #50344, 1.000000000000000000 ) ;
#61709 = ORIENTED_EDGE ( 'NONE', *, *, #38535, .F. ) ;
#61708 = EDGE_CURVE ( 'NONE', #33051, #55647, #25650, .T. ) ;
#61710 = EDGE_CURVE ( 'NONE', #53664, #47169, #47935, .T. ) ;
#61711 = AXIS2_PLACEMENT_3D ( 'NONE', #43858, #15954, #69706 ) ;
#61712 = AXIS2_PLACEMENT_3D ( 'NONE', #56771, #1627, #23901 ) ;
#61713 = CARTESIAN_POINT ( 'NONE',  ( 0.000000000000000000, 0.000000000000000000, 5.000000000000000000 ) ) ;
#61714 = EDGE_CURVE ( 'NONE', #50247, #21845, #16109, .T. ) ;
#61715 = ORIENTED_EDGE ( 'NONE', *, *, #5549, .F. ) ;
#61716 = EDGE_CURVE ( 'NONE', #51933, #11521, #13205, .T. ) ;
#61717 = ADVANCED_FACE ( 'NONE', ( #62172 ), #9408, .T. ) ;
#61718 = CARTESIAN_POINT ( 'NONE',  ( 275.0000000000000000, -26.50000000000000000, -9.080000000000000071 ) ) ;
#61719 = ORIENTED_EDGE ( 'NONE', *, *, #54409, .T. ) ;
#61720 = VERTEX_POINT ( 'NONE', #40611 ) ;
#61721 = FACE_OUTER_BOUND ( 'NONE', #29723, .T. ) ;
#61722 = CARTESIAN_POINT ( 'NONE',  ( 6.501044194225444883, 3.142976262117191943, 26.00000000000000711 ) ) ;
#61723 = ADVANCED_FACE ( 'NONE', ( #13737 ), #15065, .F. ) ;
#61724 = CARTESIAN_POINT ( 'NONE',  ( 36.90000000000000568, -21.00000000000001421, -13.86939075806900945 ) ) ;
#61725 = DIRECTION ( 'NONE',  ( 0.000000000000000000, 1.000000000000000000, 0.000000000000000000 ) ) ;
#61726 = VECTOR ( 'NONE', #46027, 1000.000000000000000 ) ;
#61727 = EDGE_CURVE ( 'NONE', #29478, #67299, #53258, .T. ) ;
#61728 = VERTEX_POINT ( 'NONE', #58902 ) ;
#61729 = ORIENTED_EDGE ( 'NONE', *, *, #6006, .T. ) ;
#61730 = FACE_OUTER_BOUND ( 'NONE', #54339, .T. ) ;
#61731 = EDGE_CURVE ( 'NONE', #24148, #68045, #69851, .T. ) ;
#61732 = CARTESIAN_POINT ( 'NONE',  ( 17.00000000000000000, -15.50000000000000000, -19.33772233983200195 ) ) ;
#61733 = ORIENTED_EDGE ( 'NONE', *, *, #12911, .T. ) ;
#61734 = ORIENTED_EDGE ( 'NONE', *, *, #12125, .T. ) ;
#61735 = ORIENTED_EDGE ( 'NONE', *, *, #11187, .T. ) ;
#61736 = CARTESIAN_POINT ( 'NONE',  ( 275.0000000000000000, -26.06132420600899735, 10.13999572156699891 ) ) ;
#61737 = EDGE_CURVE ( 'NONE', #61284, #27400, #21411, .T. ) ;
#61739 = VERTEX_POINT ( 'NONE', #15763 ) ;
#61738 = CARTESIAN_POINT ( 'NONE',  ( -9.897976262117248680, -3.682023737882723857, 54.00000000000000711 ) ) ;
#61740 = EDGE_CURVE ( 'NONE', #34997, #41893, #42626, .T. ) ;
#61741 = FACE_OUTER_BOUND ( 'NONE', #7231, .T. ) ;
#61742 = DIRECTION ( 'NONE',  ( 1.000000000000000000, -8.673617379884027583E-15, 0.000000000000000000 ) ) ;
#61743 = CIRCLE ( 'NONE', #19960, 0.1999999999999987899 ) ;
#61744 = ORIENTED_EDGE ( 'NONE', *, *, #49994, .T. ) ;
#61745 = ORIENTED_EDGE ( 'NONE', *, *, #37622, .F. ) ;
#61746 = CIRCLE ( 'NONE', #34634, 0.9999999999999991118 ) ;
#61747 = EDGE_CURVE ( 'NONE', #35441, #51919, #5158, .T. ) ;
#61748 = CARTESIAN_POINT ( 'NONE',  ( -14.25000000000000000, -2.500000000000000000, -21.77831216351300014 ) ) ;
#61749 = DIRECTION ( 'NONE',  ( 0.000000000000000000, 0.000000000000000000, 1.000000000000000000 ) ) ;
#61750 = VECTOR ( 'NONE', #20817, 1000.000000000000000 ) ;
#61751 = VECTOR ( 'NONE', #47331, 1000.000000000000000 ) ;
#61752 = CARTESIAN_POINT ( 'NONE',  ( 78.77321854994620765, 47.95351654967443977, 0.000000000000000000 ) ) ;
#61753 = VECTOR ( 'NONE', #32669, 1000.000000000000000 ) ;
#61754 = AXIS2_PLACEMENT_3D ( 'NONE', #55831, #1062, #7034 ) ;
#61755 = LINE ( 'NONE', #41230, #6341 ) ;
#61757 = CARTESIAN_POINT ( 'NONE',  ( 39.00000000000000000, 0.000000000000000000, 0.000000000000000000 ) ) ;
#61756 = AXIS2_PLACEMENT_3D ( 'NONE', #10696, #28944, #2077 ) ;
#61759 = ORIENTED_EDGE ( 'NONE', *, *, #10798, .T. ) ;
#61758 = CARTESIAN_POINT ( 'NONE',  ( 7.250000000000005329, 8.250000000000001776, -16.00000000000000000 ) ) ;
#61760 = ORIENTED_EDGE ( 'NONE', *, *, #44785, .T. ) ;
#61761 = CARTESIAN_POINT ( 'NONE',  ( 6.358413763958968623, -4.720772854004790631, 54.00000000000000711 ) ) ;
#61762 = DIRECTION ( 'NONE',  ( 1.000000000000000000, 0.000000000000000000, -0.000000000000000000 ) ) ;
#61763 = VECTOR ( 'NONE', #47420, 1000.000000000000000 ) ;
#61764 = AXIS2_PLACEMENT_3D ( 'NONE', #6671, #49123, #50508 ) ;
#61765 = LINE ( 'NONE', #68477, #19500 ) ;
#61766 = FACE_OUTER_BOUND ( 'NONE', #30965, .T. ) ;
#61767 = EDGE_CURVE ( 'NONE', #51203, #62359, #33546, .T. ) ;
#61768 = AXIS2_PLACEMENT_3D ( 'NONE', #6277, #27848, #17568 ) ;
#61769 = DIRECTION ( 'NONE',  ( -0.000000000000000000, -0.000000000000000000, 1.000000000000000000 ) ) ;
#61770 = EDGE_LOOP ( 'NONE', ( #23500, #37310, #11440, #15691 ) ) ;
#61771 = LINE ( 'NONE', #51155, #1946 ) ;
#61772 = DIRECTION ( 'NONE',  ( 0.000000000000000000, -0.2142857142857142738, -0.9767710236555245951 ) ) ;
#61773 = CARTESIAN_POINT ( 'NONE',  ( 8.250000000000005329, 0.000000000000000000, -12.00000000000000000 ) ) ;
#61774 = EDGE_CURVE ( 'NONE', #1311, #50458, #11145, .T. ) ;
#61775 = CARTESIAN_POINT ( 'NONE',  ( 32.89999999999999858, -21.00000000000000000, 13.86939075806900057 ) ) ;
#61776 = CIRCLE ( 'NONE', #40329, 2.215251240775983899 ) ;
#61777 = DIRECTION ( 'NONE',  ( 0.000000000000000000, 1.000000000000000000, 0.000000000000000000 ) ) ;
#61778 = DIRECTION ( 'NONE',  ( 3.540251991789408222E-15, 1.000000000000000000, 0.000000000000000000 ) ) ;
#61779 = EDGE_CURVE ( 'NONE', #47728, #10391, #6461, .T. ) ;
#61780 = CARTESIAN_POINT ( 'NONE',  ( -7.250000000000001776, -7.249999999999998224, -26.00000000000001066 ) ) ;
#61781 = VERTEX_POINT ( 'NONE', #5509 ) ;
#61782 = LINE ( 'NONE', #8020, #43340 ) ;
#61783 = ADVANCED_FACE ( 'NONE', ( #59241 ), #28105, .F. ) ;
#61784 = DIRECTION ( 'NONE',  ( 0.000000000000000000, -0.000000000000000000, 1.000000000000000000 ) ) ;
#61785 = VERTEX_POINT ( 'NONE', #60626 ) ;
#61786 = FACE_OUTER_BOUND ( 'NONE', #2299, .T. ) ;
#61787 = CARTESIAN_POINT ( 'NONE',  ( -7.250000000000000888, 8.250000000000001776, -23.50000000000000000 ) ) ;
#61788 = CARTESIAN_POINT ( 'NONE',  ( 30.00000000000000000, -13.54524521594299991, 17.53999999999999915 ) ) ;
#61789 = CYLINDRICAL_SURFACE ( 'NONE', #35305, 0.5249999999999994671 ) ;
#61790 = EDGE_CURVE ( 'NONE', #56837, #52982, #60269, .T. ) ;
#61791 = LINE ( 'NONE', #46565, #45196 ) ;
#61792 = VERTEX_POINT ( 'NONE', #33060 ) ;
#61793 = CARTESIAN_POINT ( 'NONE',  ( 30.00000000000000000, -11.50000000000100009, -15.00000000000084910 ) ) ;
#61794 = ORIENTED_EDGE ( 'NONE', *, *, #67992, .F. ) ;
#61795 = LINE ( 'NONE', #62133, #69542 ) ;
#61796 = COLOUR_RGB ( '', 0.09019608, 0.27058824, 0.51372549) ;
#61798 = ORIENTED_EDGE ( 'NONE', *, *, #28333, .T. ) ;
#61797 = EDGE_CURVE ( 'NONE', #14910, #10609, #32383, .T. ) ;
#61799 = CARTESIAN_POINT ( 'NONE',  ( -7.450000000000001954, -7.249999999999998224, -23.50000000000000000 ) ) ;
#61800 = EDGE_CURVE ( 'NONE', #53301, #48215, #12177, .T. ) ;
#61801 = VERTEX_POINT ( 'NONE', #66284 ) ;
#61802 = EDGE_CURVE ( 'NONE', #2806, #26623, #11825, .T. ) ;
#61803 = EDGE_CURVE ( 'NONE', #56322, #60944, #59596, .T. ) ;
#61804 = CARTESIAN_POINT ( 'NONE',  ( 17.00000000000000000, -16.28999999999999915, -14.50000000000000000 ) ) ;
#61805 = AXIS2_PLACEMENT_3D ( 'NONE', #10474, #32048, #53622 ) ;
#61806 = VECTOR ( 'NONE', #26384, 1000.000000000000000 ) ;
#61807 = CARTESIAN_POINT ( 'NONE',  ( 6.657023737882816761, 9.897976262117193613, 54.00000000000000711 ) ) ;
#61808 = ORIENTED_EDGE ( 'NONE', *, *, #16289, .F. ) ;
#61809 = ORIENTED_EDGE ( 'NONE', *, *, #27654, .F. ) ;
#61810 = DIRECTION ( 'NONE',  ( 0.000000000000000000, 0.000000000000000000, 1.000000000000000000 ) ) ;
#61811 = VERTEX_POINT ( 'NONE', #48634 ) ;
#61812 = EDGE_LOOP ( 'NONE', ( #23775, #1874, #54896, #35274, #1749 ) ) ;
#61813 = EDGE_CURVE ( 'NONE', #25655, #58150, #27065, .T. ) ;
#61814 = AXIS2_PLACEMENT_3D ( 'NONE', #33957, #60829, #12378 ) ;
#61815 = CIRCLE ( 'NONE', #69763, 3.499999999999999556 ) ;
#61816 = LINE ( 'NONE', #51556, #31653 ) ;
#61817 = DIRECTION ( 'NONE',  ( -6.508391731846281342E-15, -1.000000000000000000, -1.836970198721024757E-16 ) ) ;
#61818 = CARTESIAN_POINT ( 'NONE',  ( 7.250000000000005329, -7.249999999999998224, -17.00000000000000000 ) ) ;
#61819 = DIRECTION ( 'NONE',  ( 0.7071067811865475727, 0.7071067811865475727, 0.000000000000000000 ) ) ;
#61820 = VERTEX_POINT ( 'NONE', #64901 ) ;
#61821 = DIRECTION ( 'NONE',  ( 1.000000000000000000, 0.000000000000000000, 0.000000000000000000 ) ) ;
#61822 = VECTOR ( 'NONE', #4480, 1000.000000000000000 ) ;
#61823 = AXIS2_PLACEMENT_3D ( 'NONE', #62862, #14432, #57552 ) ;
#61825 = DIRECTION ( 'NONE',  ( -1.000000000000000000, 0.000000000000000000, 0.000000000000000000 ) ) ;
#61824 = FACE_OUTER_BOUND ( 'NONE', #64902, .T. ) ;
#61826 = ORIENTED_EDGE ( 'NONE', *, *, #34497, .T. ) ;
#61828 = ORIENTED_EDGE ( 'NONE', *, *, #6899, .F. ) ;
#61827 = CARTESIAN_POINT ( 'NONE',  ( 283.0000000000000568, -26.50000000000000000, -0.5000000000000000000 ) ) ;
#61829 = ORIENTED_EDGE ( 'NONE', *, *, #10169, .T. ) ;
#61830 = PRODUCT_CONTEXT ( 'NONE', #20094, 'mechanical' ) ;
#61831 = FACE_OUTER_BOUND ( 'NONE', #65513, .T. ) ;
#61832 = EDGE_CURVE ( 'NONE', #9816, #1141, #17144, .T. ) ;
#61833 = ORIENTED_EDGE ( 'NONE', *, *, #68188, .F. ) ;
#61834 = EDGE_CURVE ( 'NONE', #42657, #65388, #54998, .T. ) ;
#61835 = VECTOR ( 'NONE', #8008, 1000.000000000000000 ) ;
#61836 = CARTESIAN_POINT ( 'NONE',  ( 41.09999999999999432, 13.66939075806899950, 20.80000000000000426 ) ) ;
#61837 = FACE_OUTER_BOUND ( 'NONE', #19108, .T. ) ;
#61838 = ORIENTED_EDGE ( 'NONE', *, *, #42442, .F. ) ;
#61839 = EDGE_LOOP ( 'NONE', ( #18522, #4790, #1813, #48779 ) ) ;
#61840 = LINE ( 'NONE', #17301, #1907 ) ;
#61841 = DIRECTION ( 'NONE',  ( -1.000000000000000000, 0.000000000000000000, 0.000000000000000000 ) ) ;
#61842 = ORIENTED_EDGE ( 'NONE', *, *, #7943, .F. ) ;
#61843 = LINE ( 'NONE', #51934, #21145 ) ;
#61844 = DIRECTION ( 'NONE',  ( 1.000000000000000000, 0.000000000000000000, 0.000000000000000000 ) ) ;
#61845 = PLANE ( 'NONE',  #21538 ) ;
#61846 = EDGE_LOOP ( 'NONE', ( #8937, #44822, #51296, #33340 ) ) ;
#61847 = PLANE ( 'NONE',  #25642 ) ;
#61848 = CARTESIAN_POINT ( 'NONE',  ( -11.11351654964674118, -4.206483450353336373, 455.0000000000000568 ) ) ;
#61850 = ORIENTED_EDGE ( 'NONE', *, *, #43807, .T. ) ;
#61849 = CARTESIAN_POINT ( 'NONE',  ( 0.000000000000000000, -8.249999999999998224, -14.50000000000000000 ) ) ;
#61852 = ORIENTED_EDGE ( 'NONE', *, *, #59032, .T. ) ;
#61851 = LINE ( 'NONE', #51946, #16259 ) ;
#61853 = DIRECTION ( 'NONE',  ( 0.000000000000000000, 0.000000000000000000, 1.000000000000000000 ) ) ;
#61854 = CARTESIAN_POINT ( 'NONE',  ( 8.250000000000005329, 0.000000000000000000, -22.00000000000000000 ) ) ;
#61855 = DIRECTION ( 'NONE',  ( 0.000000000000000000, -1.000000000000000000, 0.000000000000000000 ) ) ;
#61856 = CARTESIAN_POINT ( 'NONE',  ( 3.664523737882781518, -10.31452373788279964, 26.00000000000000000 ) ) ;
#61857 = DIRECTION ( 'NONE',  ( -0.000000000000000000, -0.000000000000000000, -1.000000000000000000 ) ) ;
#61858 = ORIENTED_EDGE ( 'NONE', *, *, #58156, .T. ) ;
#61859 = DIRECTION ( 'NONE',  ( 1.000000000000000000, 0.000000000000000000, 0.000000000000000000 ) ) ;
#61860 = DIRECTION ( 'NONE',  ( 1.000000000000000000, 0.000000000000000000, 0.000000000000000000 ) ) ;
#61861 = LINE ( 'NONE', #13419, #53736 ) ;
#61862 = AXIS2_PLACEMENT_3D ( 'NONE', #10672, #57710, #30844 ) ;
#61863 = ADVANCED_FACE ( 'NONE', ( #65258, #543 ), #49666, .F. ) ;
#61865 = VERTEX_POINT ( 'NONE', #55331 ) ;
#61864 = CARTESIAN_POINT ( 'NONE',  ( 29.50000000000000355, -11.50000000000000000, -15.00000000000000000 ) ) ;
#61866 = CARTESIAN_POINT ( 'NONE',  ( 30.00000000000000000, -11.10796162543699950, 9.102987789146602893 ) ) ;
#61867 = DIRECTION ( 'NONE',  ( 0.4998444328988824181, 0.000000000000000000, -0.8661152018640445593 ) ) ;
#61868 = ADVANCED_FACE ( 'NONE', ( #28436 ), #27760, .T. ) ;
#61869 = VECTOR ( 'NONE', #22401, 1000.000000000000000 ) ;
#61870 = VECTOR ( 'NONE', #40506, 1000.000000000000000 ) ;
#61871 = EDGE_LOOP ( 'NONE', ( #64144, #34338, #9360, #47076, #28351, #26299, #58639, #11652 ) ) ;
#61872 = EDGE_LOOP ( 'NONE', ( #67177, #12491, #32339, #47740 ) ) ;
#61873 = CARTESIAN_POINT ( 'NONE',  ( 29.25000000000000000, -5.000000000000000000, -11.75000000000000000 ) ) ;
#61874 = EDGE_CURVE ( 'NONE', #51947, #26978, #1567, .T. ) ;
#61875 = FACE_OUTER_BOUND ( 'NONE', #48893, .T. ) ;
#61876 = ADVANCED_FACE ( 'NONE', ( #17483 ), #23132, .F. ) ;
#61877 = ORIENTED_EDGE ( 'NONE', *, *, #13082, .F. ) ;
#61878 = CARTESIAN_POINT ( 'NONE',  ( 3.157023737882809655, -6.501044194225480410, 54.00000000000000711 ) ) ;
#61879 = EDGE_CURVE ( 'NONE', #50336, #1385, #51625, .T. ) ;
#61880 = EDGE_CURVE ( 'NONE', #11348, #39584, #3323, .T. ) ;
#61881 = DIRECTION ( 'NONE',  ( 0.000000000000000000, 0.000000000000000000, -1.000000000000000000 ) ) ;
#61882 = CIRCLE ( 'NONE', #15625, 0.2000000000000005107 ) ;
#61883 = CARTESIAN_POINT ( 'NONE',  ( -9.234937905884079257, -9.955011587777201854, 195.0000000000000284 ) ) ;
#61884 = VERTEX_POINT ( 'NONE', #40800 ) ;
#61885 = DIRECTION ( 'NONE',  ( -0.7071067811865446862, -0.7071067811865503483, 0.000000000000000000 ) ) ;
#61886 = ORIENTED_EDGE ( 'NONE', *, *, #50946, .T. ) ;
#61887 = ORIENTED_EDGE ( 'NONE', *, *, #26224, .T. ) ;
#61888 = CARTESIAN_POINT ( 'NONE',  ( -3.142976262117261221, 4.031976262117183296, 54.00000000000000711 ) ) ;
#61889 = PLANE ( 'NONE',  #69385 ) ;
#61890 = ORIENTED_EDGE ( 'NONE', *, *, #27784, .T. ) ;
#61891 = VERTEX_POINT ( 'NONE', #29137 ) ;
#61892 = DIRECTION ( 'NONE',  ( -1.000000000000000000, 0.000000000000000000, 0.000000000000000000 ) ) ;
#61893 = ORIENTED_EDGE ( 'NONE', *, *, #52133, .F. ) ;
#61894 = CARTESIAN_POINT ( 'NONE',  ( 30.00000000000000000, -9.199999999999999289, -12.69999999999986073 ) ) ;
#61895 = LINE ( 'NONE', #56929, #66267 ) ;
#61896 = DIRECTION ( 'NONE',  ( -1.000000000000000000, 2.602085213965213008E-15, 0.000000000000000000 ) ) ;
#61897 = DIRECTION ( 'NONE',  ( -1.794541526872559352E-16, -1.000000000000000000, 0.000000000000000000 ) ) ;
#61898 = AXIS2_PLACEMENT_3D ( 'NONE', #44554, #2821, #45964 ) ;
#61899 = ORIENTED_EDGE ( 'NONE', *, *, #36202, .F. ) ;
#61900 = CARTESIAN_POINT ( 'NONE',  ( 0.000000000000000000, -7.449999999999998401, -20.50000000000000000 ) ) ;
#61902 = FACE_OUTER_BOUND ( 'NONE', #41638, .T. ) ;
#61901 = CARTESIAN_POINT ( 'NONE',  ( -9.547976262117304103, -8.144523737882758851, 54.00000000000000711 ) ) ;
#61903 = EDGE_LOOP ( 'NONE', ( #16193, #8293, #69726, #6728 ) ) ;
#61905 = ORIENTED_EDGE ( 'NONE', *, *, #20366, .F. ) ;
#61904 = CARTESIAN_POINT ( 'NONE',  ( 30.00000000000000000, -13.79999999999979998, 17.30000000000000071 ) ) ;
#61906 = ORIENTED_EDGE ( 'NONE', *, *, #27658, .F. ) ;
#61907 = ORIENTED_EDGE ( 'NONE', *, *, #3063, .F. ) ;
#61908 = DIRECTION ( 'NONE',  ( 0.000000000000000000, -0.7071067811865474617, 0.7071067811865474617 ) ) ;
#61909 = VECTOR ( 'NONE', #19445, 1000.000000000000000 ) ;
#61910 = EDGE_CURVE ( 'NONE', #43603, #44628, #17753, .T. ) ;
#61911 = CYLINDRICAL_SURFACE ( 'NONE', #62032, 1.000000000000000000 ) ;
#61912 = ORIENTED_EDGE ( 'NONE', *, *, #22895, .T. ) ;
#61913 = ORIENTED_EDGE ( 'NONE', *, *, #19685, .F. ) ;
#61914 = EDGE_CURVE ( 'NONE', #2063, #14714, #62932, .T. ) ;
#61915 = DIRECTION ( 'NONE',  ( 1.000000000000000000, 0.000000000000000000, 0.000000000000000000 ) ) ;
#61916 = PLANE ( 'NONE',  #50356 ) ;
#61917 = VERTEX_POINT ( 'NONE', #51765 ) ;
#61918 = ORIENTED_EDGE ( 'NONE', *, *, #64922, .F. ) ;
#61919 = CARTESIAN_POINT ( 'NONE',  ( 30.00000000000000000, -5.200000000000001066, -11.75000000000000000 ) ) ;
#61920 = CARTESIAN_POINT ( 'NONE',  ( -7.250000000000000888, 7.250000000000001776, -9.500000000000001776 ) ) ;
#61921 = EDGE_LOOP ( 'NONE', ( #34870, #2446, #23594, #4462 ) ) ;
#61922 = AXIS2_PLACEMENT_3D ( 'NONE', #67260, #60895, #13159 ) ;
#61923 = LINE ( 'NONE', #13481, #39144 ) ;
#61924 = LINE ( 'NONE', #3235, #29447 ) ;
#61926 = ORIENTED_EDGE ( 'NONE', *, *, #17746, .F. ) ;
#61925 = FILL_AREA_STYLE ('',( #2524 ) ) ;
#61927 = ORIENTED_EDGE ( 'NONE', *, *, #49921, .F. ) ;
#61928 = LINE ( 'NONE', #56629, #16994 ) ;
#61929 = DIRECTION ( 'NONE',  ( -1.000000000000000000, 0.000000000000000000, 0.000000000000000000 ) ) ;
#61930 = CARTESIAN_POINT ( 'NONE',  ( 8.250000000000005329, -7.249999999999998224, -17.50000000000000000 ) ) ;
#61931 = DIRECTION ( 'NONE',  ( 0.000000000000000000, 0.000000000000000000, 1.000000000000000000 ) ) ;
#61932 = CARTESIAN_POINT ( 'NONE',  ( -8.250000000000001776, -7.249999999999998224, -18.00000000000000000 ) ) ;
#61933 = CARTESIAN_POINT ( 'NONE',  ( 24.90000000000000213, -0.1999999999911430404, -8.864436962241481021E-12 ) ) ;
#61934 = DIRECTION ( 'NONE',  ( 1.000000000000000000, -0.000000000000000000, -0.000000000000000000 ) ) ;
#61935 = EDGE_LOOP ( 'NONE', ( #42616, #49551, #66604, #65657 ) ) ;
#61936 = DIRECTION ( 'NONE',  ( 0.000000000000000000, 0.000000000000000000, -1.000000000000000000 ) ) ;
#61938 = ORIENTED_EDGE ( 'NONE', *, *, #32681, .T. ) ;
#61937 = CARTESIAN_POINT ( 'NONE',  ( -7.250000000000000888, 7.450000000000003730, -22.00000000000000000 ) ) ;
#61939 = EDGE_CURVE ( 'NONE', #20854, #27061, #40449, .T. ) ;
#61940 = CARTESIAN_POINT ( 'NONE',  ( 30.90000000000000213, -21.00000000000000000, 13.86939075806900057 ) ) ;
#61941 = DIRECTION ( 'NONE',  ( 0.000000000000000000, 0.000000000000000000, -1.000000000000000000 ) ) ;
#61942 = DIRECTION ( 'NONE',  ( -1.836970198721029934E-16, 1.836970198721036590E-16, -1.000000000000000000 ) ) ;
#61943 = CARTESIAN_POINT ( 'NONE',  ( 10.05377373788281048, 8.916576262117187568, 26.00000000000000711 ) ) ;
#61944 = DIRECTION ( 'NONE',  ( 0.000000000000000000, 0.000000000000000000, -1.000000000000000000 ) ) ;
#61945 = ORIENTED_EDGE ( 'NONE', *, *, #3612, .T. ) ;
#61946 = CARTESIAN_POINT ( 'NONE',  ( -5.993516549646776603, -6.006483450353426790, 455.0000000000000568 ) ) ;
#61947 = VERTEX_POINT ( 'NONE', #45391 ) ;
#61948 = AXIS2_PLACEMENT_3D ( 'NONE', #20684, #30603, #36605 ) ;
#61949 = DIRECTION ( 'NONE',  ( 0.000000000000000000, 0.000000000000000000, 1.000000000000000000 ) ) ;
#61950 = EDGE_CURVE ( 'NONE', #55879, #29528, #35132, .T. ) ;
#61951 = ADVANCED_FACE ( 'NONE', ( #68023 ), #60956, .F. ) ;
#61952 = DIRECTION ( 'NONE',  ( -8.359604446858500663E-15, -1.000000000000000000, 0.000000000000000000 ) ) ;
#61953 = VECTOR ( 'NONE', #41629, 1000.000000000000000 ) ;
#61954 = DIRECTION ( 'NONE',  ( 0.000000000000000000, 0.000000000000000000, -1.000000000000000000 ) ) ;
#61955 = EDGE_CURVE ( 'NONE', #67535, #54832, #12857, .T. ) ;
#61956 = VERTEX_POINT ( 'NONE', #2971 ) ;
#61957 = CARTESIAN_POINT ( 'NONE',  ( 7.450000000000006395, 7.250000000000000888, -21.00000000000000000 ) ) ;
#61958 = ORIENTED_EDGE ( 'NONE', *, *, #49443, .F. ) ;
#61959 = VERTEX_POINT ( 'NONE', #67330 ) ;
#61960 = AXIS2_PLACEMENT_3D ( 'NONE', #13750, #19401, #50540 ) ;
#61961 = DIRECTION ( 'NONE',  ( 1.000000000000000000, 0.000000000000000000, 0.000000000000000000 ) ) ;
#61962 = DIRECTION ( 'NONE',  ( 0.000000000000000000, 3.673940397442059868E-16, -1.000000000000000000 ) ) ;
#61963 = ORIENTED_EDGE ( 'NONE', *, *, #7164, .T. ) ;
#61964 = DIRECTION ( 'NONE',  ( -0.000000000000000000, 1.000000000000000000, -0.000000000000000000 ) ) ;
#61965 = VECTOR ( 'NONE', #66370, 1000.000000000000000 ) ;
#61966 = DIRECTION ( 'NONE',  ( 0.000000000000000000, 0.000000000000000000, 1.000000000000000000 ) ) ;
#61967 = PLANE ( 'NONE',  #61085 ) ;
#61968 = EDGE_LOOP ( 'NONE', ( #66269, #31325, #21829, #63868 ) ) ;
#61969 = VERTEX_POINT ( 'NONE', #56710 ) ;
#61971 = ORIENTED_EDGE ( 'NONE', *, *, #45707, .T. ) ;
#61970 = CARTESIAN_POINT ( 'NONE',  ( 12.00648345035338238, 4.173516549646515195, 455.0000000000000568 ) ) ;
#61972 = ORIENTED_EDGE ( 'NONE', *, *, #13824, .F. ) ;
#61973 = VECTOR ( 'NONE', #27874, 1000.000000000000000 ) ;
#61974 = PLANE ( 'NONE',  #27002 ) ;
#61975 = DIRECTION ( 'NONE',  ( -1.000000000000000000, 0.000000000000000000, 0.000000000000000000 ) ) ;
#61976 = CARTESIAN_POINT ( 'NONE',  ( 49.00000000000000000, 13.66939075806899950, 20.80000000000000426 ) ) ;
#61977 = DIRECTION ( 'NONE',  ( 0.000000000000000000, 0.000000000000000000, -1.000000000000000000 ) ) ;
#61978 = VECTOR ( 'NONE', #14909, 1000.000000000000000 ) ;
#61979 = CARTESIAN_POINT ( 'NONE',  ( 30.00000000000000000, -5.200000000000001066, 11.75000000000000000 ) ) ;
#61980 = ORIENTED_EDGE ( 'NONE', *, *, #52243, .F. ) ;
#61981 = EDGE_LOOP ( 'NONE', ( #44200, #41546, #9400, #52458 ) ) ;
#61982 = ORIENTED_EDGE ( 'NONE', *, *, #31010, .T. ) ;
#61983 = ORIENTED_EDGE ( 'NONE', *, *, #54806, .T. ) ;
#61984 = FACE_OUTER_BOUND ( 'NONE', #39390, .T. ) ;
#61985 = PLANE ( 'NONE',  #60294 ) ;
#61986 = DIRECTION ( 'NONE',  ( 0.000000000000000000, 1.000000000000000000, 0.000000000000000000 ) ) ;
#61987 = EDGE_LOOP ( 'NONE', ( #38339, #41293, #14575, #67404, #44254, #15646, #62692, #17431, #56145, #63114, #13870, #44701, #67661, #60019 ) ) ;
#61988 = ORIENTED_EDGE ( 'NONE', *, *, #3622, .T. ) ;
#61989 = ORIENTED_EDGE ( 'NONE', *, *, #35801, .T. ) ;
#61990 = ADVANCED_FACE ( 'NONE', ( #39735 ), #62356, .F. ) ;
#61991 = EDGE_CURVE ( 'NONE', #39877, #8834, #34786, .T. ) ;
#61992 = EDGE_CURVE ( 'NONE', #31845, #46179, #7911, .T. ) ;
#61993 = DIRECTION ( 'NONE',  ( 1.000000000000000000, 0.000000000000000000, 0.000000000000000000 ) ) ;
#61994 = ORIENTED_EDGE ( 'NONE', *, *, #580, .F. ) ;
#61995 = EDGE_LOOP ( 'NONE', ( #69605, #27952, #26027, #5975 ) ) ;
#61996 = LINE ( 'NONE', #12241, #1743 ) ;
#61997 = EDGE_CURVE ( 'NONE', #40124, #15934, #23492, .T. ) ;
#61998 = VERTEX_POINT ( 'NONE', #24887 ) ;
#61999 = VERTEX_POINT ( 'NONE', #24187 ) ;
#62000 = FACE_OUTER_BOUND ( 'NONE', #60757, .T. ) ;
#62002 = ORIENTED_EDGE ( 'NONE', *, *, #9407, .F. ) ;
#62001 = CARTESIAN_POINT ( 'NONE',  ( -7.342976262117259623, 3.834182069070703580, 54.00000000000000711 ) ) ;
#62003 = ORIENTED_EDGE ( 'NONE', *, *, #39095, .F. ) ;
#62004 = AXIS2_PLACEMENT_3D ( 'NONE', #31569, #5402, #53147 ) ;
#62005 = DIRECTION ( 'NONE',  ( -1.794541526872559352E-16, -1.000000000000000000, 0.000000000000000000 ) ) ;
#62006 = LINE ( 'NONE', #50357, #52156 ) ;
#62007 = DIRECTION ( 'NONE',  ( 0.000000000000000000, 0.000000000000000000, -1.000000000000000000 ) ) ;
#62009 = ORIENTED_EDGE ( 'NONE', *, *, #69564, .F. ) ;
#62008 = CARTESIAN_POINT ( 'NONE',  ( 33.89999999999999858, 13.66939075806899240, -20.79999999999999361 ) ) ;
#62010 = ORIENTED_EDGE ( 'NONE', *, *, #371, .T. ) ;
#62011 = AXIS2_PLACEMENT_3D ( 'NONE', #49265, #33677, #17077 ) ;
#62012 = DIRECTION ( 'NONE',  ( 0.000000000000000000, -0.9921567416492215186, 0.1249999999999996531 ) ) ;
#62013 = DIRECTION ( 'NONE',  ( 0.000000000000000000, 0.000000000000000000, 1.000000000000000000 ) ) ;
#62014 = CONICAL_SURFACE ( 'NONE', #59759, 1.621000000000000885, 0.7853981633974518317 ) ;
#62015 = DIRECTION ( 'NONE',  ( 0.000000000000000000, 0.000000000000000000, -1.000000000000000000 ) ) ;
#62016 = ORIENTED_EDGE ( 'NONE', *, *, #59527, .T. ) ;
#62017 = CARTESIAN_POINT ( 'NONE',  ( -30.00000000000000000, -14.33999999999999986, -14.50000000000000000 ) ) ;
#62018 = VECTOR ( 'NONE', #45778, 1000.000000000000000 ) ;
#62019 = CARTESIAN_POINT ( 'NONE',  ( -15.50000000000000000, -0.1999999999999999556, 23.94999999999999929 ) ) ;
#62020 = DIRECTION ( 'NONE',  ( 0.000000000000000000, 0.000000000000000000, 1.000000000000000000 ) ) ;
#62021 = VERTEX_POINT ( 'NONE', #29487 ) ;
#62022 = CARTESIAN_POINT ( 'NONE',  ( 8.930623737882845248, 8.916576262117187568, 54.00000000000000711 ) ) ;
#62023 = VECTOR ( 'NONE', #24690, 1000.000000000000114 ) ;
#62024 = DIRECTION ( 'NONE',  ( 0.000000000000000000, 0.000000000000000000, 1.000000000000000000 ) ) ;
#62025 = DIRECTION ( 'NONE',  ( -1.000000000000000000, 0.000000000000000000, 0.000000000000000000 ) ) ;
#62026 = ORIENTED_EDGE ( 'NONE', *, *, #17497, .T. ) ;
#62027 = LINE ( 'NONE', #14312, #31349 ) ;
#62028 = CARTESIAN_POINT ( 'NONE',  ( -25.50000000000000355, -5.200000000000001066, 24.50000000000000000 ) ) ;
#62029 = ADVANCED_FACE ( 'NONE', ( #24546 ), #1927, .F. ) ;
#62030 = ADVANCED_FACE ( 'NONE', ( #8260 ), #29835, .F. ) ;
#62031 = ORIENTED_EDGE ( 'NONE', *, *, #60827, .T. ) ;
#62032 = AXIS2_PLACEMENT_3D ( 'NONE', #67214, #18410, #34320 ) ;
#62033 = PLANE ( 'NONE',  #43957 ) ;
#62034 = CARTESIAN_POINT ( 'NONE',  ( 8.606483450353334064, 4.383466043307767457, 195.0000000000000284 ) ) ;
#62035 = ADVANCED_FACE ( 'NONE', ( #46106 ), #30194, .F. ) ;
#62036 = DIRECTION ( 'NONE',  ( 0.000000000000000000, 0.000000000000000000, 1.000000000000000000 ) ) ;
#62037 = CARTESIAN_POINT ( 'NONE',  ( 41.09999999999999432, -21.00000000000000000, -13.86939075806900057 ) ) ;
#62038 = ORIENTED_EDGE ( 'NONE', *, *, #60045, .T. ) ;
#62039 = PLANE ( 'NONE',  #20838 ) ;
#62040 = CARTESIAN_POINT ( 'NONE',  ( 283.0000000000000568, -30.80000000000000071, -8.900000000000000355 ) ) ;
#62041 = EDGE_CURVE ( 'NONE', #66059, #18896, #34697, .T. ) ;
#62042 = DIRECTION ( 'NONE',  ( 1.000000000000000000, -0.000000000000000000, 0.000000000000000000 ) ) ;
#62043 = PRODUCT_RELATED_PRODUCT_CATEGORY ( 'part', '', ( #35679 ) ) ;
#62044 = FACE_OUTER_BOUND ( 'NONE', #29306, .T. ) ;
#62045 = EDGE_CURVE ( 'NONE', #61430, #58411, #63776, .T. ) ;
#62046 = CARTESIAN_POINT ( 'NONE',  ( 32.89999999999999858, -14.06939075806900163, -20.80000000000000426 ) ) ;
#62047 = ORIENTED_EDGE ( 'NONE', *, *, #67992, .T. ) ;
#62048 = VECTOR ( 'NONE', #62398, 1000.000000000000000 ) ;
#62050 = ORIENTED_EDGE ( 'NONE', *, *, #50368, .F. ) ;
#62049 = CYLINDRICAL_SURFACE ( 'NONE', #3489, 0.5999999999999989786 ) ;
#62051 = EDGE_CURVE ( 'NONE', #42130, #69904, #37004, .T. ) ;
#62052 = AXIS2_PLACEMENT_3D ( 'NONE', #14866, #36425, #25829 ) ;
#62053 = CARTESIAN_POINT ( 'NONE',  ( -9.547976262117254365, 8.130476262117182884, 54.00000000000000711 ) ) ;
#62054 = CARTESIAN_POINT ( 'NONE',  ( 46.39999999999999858, 33.00000000000000000, -2.250000000000000444 ) ) ;
#62055 = ORIENTED_EDGE ( 'NONE', *, *, #44666, .T. ) ;
#62056 = CARTESIAN_POINT ( 'NONE',  ( 30.00000000000000000, -11.50000000000000000, -11.00000000000000000 ) ) ;
#62057 = ORIENTED_EDGE ( 'NONE', *, *, #56689, .T. ) ;
#62058 = VECTOR ( 'NONE', #18032, 1000.000000000000000 ) ;
#62059 = DIRECTION ( 'NONE',  ( 0.000000000000000000, -1.000000000000000000, 0.000000000000000000 ) ) ;
#62060 = VERTEX_POINT ( 'NONE', #35844 ) ;
#62061 = VERTEX_POINT ( 'NONE', #48211 ) ;
#62062 = DIRECTION ( 'NONE',  ( 0.000000000000000000, 0.000000000000000000, -1.000000000000000000 ) ) ;
#62063 = DIRECTION ( 'NONE',  ( -1.000000000000000000, 1.794541526872559352E-16, 0.000000000000000000 ) ) ;
#62064 = CIRCLE ( 'NONE', #63247, 0.1999999999999987899 ) ;
#62065 = DIRECTION ( 'NONE',  ( 0.000000000000000000, 0.000000000000000000, 1.000000000000000000 ) ) ;
#62066 = DIRECTION ( 'NONE',  ( 1.000000000000000000, 0.000000000000000000, 0.000000000000000000 ) ) ;
#62067 = EDGE_LOOP ( 'NONE', ( #45158, #50522, #28856, #68203 ) ) ;
#62068 = ORIENTED_EDGE ( 'NONE', *, *, #19273, .T. ) ;
#62069 = LINE ( 'NONE', #22862, #48219 ) ;
#62071 = LINE ( 'NONE', #40859, #60960 ) ;
#62070 = CIRCLE ( 'NONE', #62114, 2.215251240775983899 ) ;
#62072 = ORIENTED_EDGE ( 'NONE', *, *, #24016, .T. ) ;
#62073 = ORIENTED_EDGE ( 'NONE', *, *, #7734, .T. ) ;
#62074 = ORIENTED_EDGE ( 'NONE', *, *, #6885, .F. ) ;
#62075 = CARTESIAN_POINT ( 'NONE',  ( 29.25000000000000000, -5.200000000000001066, 11.75000000000000000 ) ) ;
#62077 = ORIENTED_EDGE ( 'NONE', *, *, #9114, .T. ) ;
#62076 = FACE_OUTER_BOUND ( 'NONE', #29630, .T. ) ;
#62078 = DIRECTION ( 'NONE',  ( -1.000000000000000000, 0.000000000000000000, 0.000000000000000000 ) ) ;
#62079 = DIRECTION ( 'NONE',  ( -1.000000000000000000, 0.000000000000000000, 0.000000000000000000 ) ) ;
#62080 = CIRCLE ( 'NONE', #42922, 2.204799999999997429 ) ;
#62081 = ORIENTED_EDGE ( 'NONE', *, *, #21340, .T. ) ;
#62082 = ORIENTED_EDGE ( 'NONE', *, *, #35118, .F. ) ;
#62083 = EDGE_CURVE ( 'NONE', #8462, #28622, #10377, .T. ) ;
#62084 = CARTESIAN_POINT ( 'NONE',  ( 10.74648345035337904, -1.690483450353490680, 455.0000000000000568 ) ) ;
#62085 = FACE_OUTER_BOUND ( 'NONE', #7338, .T. ) ;
#62086 = EDGE_CURVE ( 'NONE', #44680, #56867, #41142, .T. ) ;
#62087 = CARTESIAN_POINT ( 'NONE',  ( 7.000000000000000000, -37.14999999999894698, -8.200000000002349410 ) ) ;
#62088 = VECTOR ( 'NONE', #42597, 1000.000000000000114 ) ;
#62089 = AXIS2_PLACEMENT_3D ( 'NONE', #11175, #43715, #234 ) ;
#62090 = DIRECTION ( 'NONE',  ( 1.000000000000000000, 0.000000000000000000, 0.000000000000000000 ) ) ;
#62091 = CARTESIAN_POINT ( 'NONE',  ( 7.250000000000005329, 8.250000000000001776, -17.50000000000000000 ) ) ;
#62092 = EDGE_CURVE ( 'NONE', #32705, #4531, #57323, .T. ) ;
#62094 = VERTEX_POINT ( 'NONE', #20623 ) ;
#62093 = CARTESIAN_POINT ( 'NONE',  ( -6.651770455163781293, -7.357023737882790293, 54.00000000000000711 ) ) ;
#62095 = VERTEX_POINT ( 'NONE', #26639 ) ;
#62096 = DIRECTION ( 'NONE',  ( -0.8660254037844482555, 0.000000000000000000, 0.4999999999999831801 ) ) ;
#62098 = CARTESIAN_POINT ( 'NONE',  ( -25.50000000000000355, 0.000000000000000000, 22.50000000000000000 ) ) ;
#62097 = VECTOR ( 'NONE', #22223, 1000.000000000000000 ) ;
#62099 = CARTESIAN_POINT ( 'NONE',  ( 0.000000000000000000, -7.449999999999998401, -25.50000000000000355 ) ) ;
#62100 = DIRECTION ( 'NONE',  ( -1.000000000000000000, -3.016910393003147986E-15, 0.000000000000000000 ) ) ;
#62101 = EDGE_CURVE ( 'NONE', #9455, #20433, #47190, .T. ) ;
#62102 = VECTOR ( 'NONE', #44471, 1000.000000000000000 ) ;
#62103 = CARTESIAN_POINT ( 'NONE',  ( 0.000000000000000000, -7.449999999999998401, -10.00000000000000000 ) ) ;
#62104 = ORIENTED_EDGE ( 'NONE', *, *, #58327, .F. ) ;
#62105 = DIRECTION ( 'NONE',  ( 1.000000000000000000, 0.000000000000000000, 0.000000000000000000 ) ) ;
#62107 = VECTOR ( 'NONE', #57401, 1000.000000000000000 ) ;
#62106 = DIRECTION ( 'NONE',  ( 1.000000000000000000, 0.000000000000000000, 0.000000000000000000 ) ) ;
#62108 = FILL_AREA_STYLE_COLOUR ( '', #42361 ) ;
#62109 = AXIS2_PLACEMENT_3D ( 'NONE', #33280, #6065, #73 ) ;
#62110 = FACE_OUTER_BOUND ( 'NONE', #29571, .T. ) ;
#62111 = EDGE_CURVE ( 'NONE', #20447, #325, #13251, .T. ) ;
#62112 = DIRECTION ( 'NONE',  ( 0.000000000000000000, 0.000000000000000000, 1.000000000000000000 ) ) ;
#62113 = CARTESIAN_POINT ( 'NONE',  ( 9.106483450353380249, -10.92648345035339297, 195.0000000000000284 ) ) ;
#62114 = AXIS2_PLACEMENT_3D ( 'NONE', #51412, #67680, #8269 ) ;
#62115 = CIRCLE ( 'NONE', #24893, 1.000000000000002665 ) ;
#62116 = DIRECTION ( 'NONE',  ( 0.000000000000000000, 1.000000000000000000, 0.000000000000000000 ) ) ;
#62117 = ORIENTED_EDGE ( 'NONE', *, *, #21496, .T. ) ;
#62118 = PLANE ( 'NONE',  #68230 ) ;
#62119 = CARTESIAN_POINT ( 'NONE',  ( -7.250000000000000888, -8.249999999999998224, -16.50000000000000000 ) ) ;
#62120 = EDGE_LOOP ( 'NONE', ( #60404, #9885, #54773, #62339 ) ) ;
#62121 = DIRECTION ( 'NONE',  ( 0.000000000000000000, 0.000000000000000000, 1.000000000000000000 ) ) ;
#62122 = CARTESIAN_POINT ( 'NONE',  ( 49.00000000000000000, -0.1999999999911795112, 8.826273045769999343E-12 ) ) ;
#62123 = CARTESIAN_POINT ( 'NONE',  ( 7.000000000000000000, -25.60000000000000142, 15.10000000000000142 ) ) ;
#62124 = CARTESIAN_POINT ( 'NONE',  ( -8.393516549646712122, 6.331612867284047041, 195.0000000000000284 ) ) ;
#62125 = EDGE_CURVE ( 'NONE', #40441, #58819, #19933, .T. ) ;
#62126 = CARTESIAN_POINT ( 'NONE',  ( -17.51999999999999957, -15.50000000000000000, -26.00000000000000355 ) ) ;
#62127 = VERTEX_POINT ( 'NONE', #30544 ) ;
#62128 = EDGE_CURVE ( 'NONE', #23277, #28299, #40359, .T. ) ;
#62129 = CARTESIAN_POINT ( 'NONE',  ( 30.00000000000000000, -17.14999999999999858, -27.00000000000000000 ) ) ;
#62130 = ORIENTED_EDGE ( 'NONE', *, *, #22821, .T. ) ;
#62131 = CARTESIAN_POINT ( 'NONE',  ( -6.835476262117260227, 10.30047626211718104, 26.00000000000000711 ) ) ;
#62132 = AXIS2_PLACEMENT_3D ( 'NONE', #25226, #19915, #41490 ) ;
#62133 = CARTESIAN_POINT ( 'NONE',  ( -4.383466043307968185, -8.406483450353443132, 455.0000000000000568 ) ) ;
#62134 = VERTEX_POINT ( 'NONE', #36915 ) ;
#62135 = FACE_OUTER_BOUND ( 'NONE', #9132, .T. ) ;
#62136 = EDGE_CURVE ( 'NONE', #6331, #59936, #5071, .T. ) ;
#62137 = VERTEX_POINT ( 'NONE', #36188 ) ;
#62138 = VECTOR ( 'NONE', #63698, 999.9999999999998863 ) ;
#62139 = DIRECTION ( 'NONE',  ( -1.794541526872559352E-16, -1.000000000000000000, 0.000000000000000000 ) ) ;
#62140 = EDGE_LOOP ( 'NONE', ( #53053, #627, #34211, #1607 ) ) ;
#62141 = ORIENTED_EDGE ( 'NONE', *, *, #1543, .T. ) ;
#62142 = LINE ( 'NONE', #3465, #41888 ) ;
#62143 = CIRCLE ( 'NONE', #41823, 24.99999999998794920 ) ;
#62144 = ORIENTED_EDGE ( 'NONE', *, *, #55462, .T. ) ;
#62145 = ORIENTED_EDGE ( 'NONE', *, *, #65693, .F. ) ;
#62146 = PRODUCT_DEFINITION_CONTEXT ( 'detailed design', #61160, 'design' ) ;
#62147 = LINE ( 'NONE', #13371, #22595 ) ;
#62148 = CARTESIAN_POINT ( 'NONE',  ( -10.91351654964680584, -9.106483450353376696, 455.0000000000000568 ) ) ;
#62150 = CARTESIAN_POINT ( 'NONE',  ( 36.90000000000000568, 20.60000000000000142, -13.86939075806900057 ) ) ;
#62149 = VECTOR ( 'NONE', #62619, 1000.000000000000000 ) ;
#62151 = ORIENTED_EDGE ( 'NONE', *, *, #62128, .T. ) ;
#62152 = VECTOR ( 'NONE', #43337, 1000.000000000000000 ) ;
#62153 = DIRECTION ( 'NONE',  ( -1.000000000000000000, 0.000000000000000000, 0.000000000000000000 ) ) ;
#62155 = DIRECTION ( 'NONE',  ( 0.000000000000000000, 0.000000000000000000, 1.000000000000000000 ) ) ;
#62154 = DIRECTION ( 'NONE',  ( 1.836970198721029934E-16, 1.836970198721010706E-16, -1.000000000000000000 ) ) ;
#62156 = VERTEX_POINT ( 'NONE', #9326 ) ;
#62158 = ORIENTED_EDGE ( 'NONE', *, *, #18195, .T. ) ;
#62157 = CARTESIAN_POINT ( 'NONE',  ( 8.900000000000005684, -0.2000000000000000111, 0.000000000000000000 ) ) ;
#62159 = ORIENTED_EDGE ( 'NONE', *, *, #682, .T. ) ;
#62160 = AXIS2_PLACEMENT_3D ( 'NONE', #15801, #63897, #43013 ) ;
#62161 = EDGE_CURVE ( 'NONE', #41930, #52180, #61815, .T. ) ;
#62162 =( LENGTH_UNIT ( ) NAMED_UNIT ( * ) SI_UNIT ( .MILLI., .METRE. ) );
#62163 = CARTESIAN_POINT ( 'NONE',  ( 25.57999999999999829, 0.000000000000000000, 0.000000000000000000 ) ) ;
#62164 = ORIENTED_EDGE ( 'NONE', *, *, #65506, .T. ) ;
#62165 = ADVANCED_FACE ( 'NONE', ( #52467 ), #53181, .F. ) ;
#62166 = FACE_OUTER_BOUND ( 'NONE', #65413, .T. ) ;
#62167 = DIRECTION ( 'NONE',  ( -1.000000000000000000, 0.000000000000000000, 0.000000000000000000 ) ) ;
#62168 = ORIENTED_EDGE ( 'NONE', *, *, #58341, .F. ) ;
#62169 = ORIENTED_EDGE ( 'NONE', *, *, #63697, .T. ) ;
#62170 = EDGE_CURVE ( 'NONE', #47387, #60243, #41843, .T. ) ;
#62171 = VECTOR ( 'NONE', #69707, 1000.000000000000000 ) ;
#62172 = FACE_OUTER_BOUND ( 'NONE', #33943, .T. ) ;
#62173 = EDGE_CURVE ( 'NONE', #59597, #14943, #46015, .T. ) ;
#62174 = LINE ( 'NONE', #30715, #68490 ) ;
#62175 = EDGE_LOOP ( 'NONE', ( #32807, #32578, #37040, #41297 ) ) ;
#62176 = DIRECTION ( 'NONE',  ( 3.491481338843133355E-15, 1.000000000000000000, 0.000000000000000000 ) ) ;
#62177 = CARTESIAN_POINT ( 'NONE',  ( 39.90000000000000568, 0.000000000000000000, 3.447897592003593022E-15 ) ) ;
#62178 = EDGE_CURVE ( 'NONE', #2683, #32021, #58487, .T. ) ;
#62179 = DIRECTION ( 'NONE',  ( 1.000000000000000000, 0.000000000000000000, 0.000000000000000000 ) ) ;
#62180 = ORIENTED_EDGE ( 'NONE', *, *, #61163, .F. ) ;
#62181 = LINE ( 'NONE', #48382, #10942 ) ;
#62182 = VECTOR ( 'NONE', #69928, 1000.000000000000000 ) ;
#62183 = CARTESIAN_POINT ( 'NONE',  ( 48.50000000000000000, -0.7500000000000000000, 3.418698582794335028 ) ) ;
#62184 = ADVANCED_FACE ( 'NONE', ( #26287 ), #20974, .F. ) ;
#62186 = VERTEX_POINT ( 'NONE', #5773 ) ;
#62185 =( LENGTH_UNIT ( ) NAMED_UNIT ( * ) SI_UNIT ( .MILLI., .METRE. ) );
#62188 = ORIENTED_EDGE ( 'NONE', *, *, #30918, .T. ) ;
#62187 = CARTESIAN_POINT ( 'NONE',  ( 105.8309041053263257, 3.657408540445008960, 10.00000000000000000 ) ) ;
#62189 = EDGE_CURVE ( 'NONE', #44075, #16486, #5437, .T. ) ;
#62190 = CARTESIAN_POINT ( 'NONE',  ( 9.690000000000001279, -9.750000000000001776, -7.000000000000000000 ) ) ;
#62191 = CARTESIAN_POINT ( 'NONE',  ( 7.250000000000005329, -7.249999999999998224, -18.50000000000000000 ) ) ;
#62192 = EDGE_CURVE ( 'NONE', #29982, #15138, #59849, .T. ) ;
#62193 = DIRECTION ( 'NONE',  ( 1.000000000000000000, 0.000000000000000000, 0.000000000000000000 ) ) ;
#62194 = EDGE_CURVE ( 'NONE', #51208, #29528, #67478, .T. ) ;
#62195 = EDGE_CURVE ( 'NONE', #3591, #3786, #42894, .T. ) ;
#62196 = LINE ( 'NONE', #51238, #26064 ) ;
#62197 = CARTESIAN_POINT ( 'NONE',  ( -7.250000000000000000, -7.449999999999998401, -14.00000000000000000 ) ) ;
#62198 = EDGE_LOOP ( 'NONE', ( #42674, #31676, #14011, #41834 ) ) ;
#62199 = CARTESIAN_POINT ( 'NONE',  ( 17.51999999999999957, -17.50000000000000000, 26.00000000000000355 ) ) ;
#62200 = CARTESIAN_POINT ( 'NONE',  ( 11.90000000000000036, -0.000000000000000000, 20.80000000000000426 ) ) ;
#62201 = VECTOR ( 'NONE', #8800, 1000.000000000000000 ) ;
#62202 = EDGE_CURVE ( 'NONE', #5389, #39722, #16371, .T. ) ;
#62203 = LINE ( 'NONE', #13766, #38922 ) ;
#62205 = ORIENTED_EDGE ( 'NONE', *, *, #55227, .T. ) ;
#62204 = DIRECTION ( 'NONE',  ( -0.000000000000000000, -0.000000000000000000, 1.000000000000000000 ) ) ;
#62206 = VECTOR ( 'NONE', #39488, 1000.000000000000000 ) ;
#62207 = AXIS2_PLACEMENT_3D ( 'NONE', #49505, #1074, #44182 ) ;
#62208 = CARTESIAN_POINT ( 'NONE',  ( 10.92648345035337343, -2.706483450353490916, 455.0000000000000568 ) ) ;
#62209 = CARTESIAN_POINT ( 'NONE',  ( 275.0000000000000000, -42.50000000000000000, 9.950000000000001066 ) ) ;
#62210 = VECTOR ( 'NONE', #28992, 1000.000000000000000 ) ;
#62211 = VERTEX_POINT ( 'NONE', #26990 ) ;
#62212 = ORIENTED_EDGE ( 'NONE', *, *, #36838, .F. ) ;
#62213 = CARTESIAN_POINT ( 'NONE',  ( -7.342976262117259623, 3.834182069070703580, 54.00000000000000711 ) ) ;
#62214 = CARTESIAN_POINT ( 'NONE',  ( -9.942044687070668019, -9.247904806590694804, 455.0000000000000568 ) ) ;
#62215 = ORIENTED_EDGE ( 'NONE', *, *, #13042, .F. ) ;
#62216 = AXIS2_PLACEMENT_3D ( 'NONE', #43375, #4522, #47995 ) ;
#62217 = DIRECTION ( 'NONE',  ( -8.951101527228104953E-17, 1.000000000000000000, -0.000000000000000000 ) ) ;
#62218 = CARTESIAN_POINT ( 'NONE',  ( -7.250000000000000000, -7.449999999999998401, -21.00000000000000000 ) ) ;
#62219 = ADVANCED_FACE ( 'NONE', ( #54215 ), #21683, .F. ) ;
#62220 = CARTESIAN_POINT ( 'NONE',  ( 17.00000000000000000, -17.50000000000000000, 15.70499999999969809 ) ) ;
#62221 = EDGE_CURVE ( 'NONE', #60780, #14841, #12142, .T. ) ;
#62222 = LINE ( 'NONE', #3191, #56813 ) ;
#62223 = ORIENTED_EDGE ( 'NONE', *, *, #64402, .T. ) ;
#62224 = LINE ( 'NONE', #36405, #53124 ) ;
#62225 = DIRECTION ( 'NONE',  ( 0.000000000000000000, 1.000000000000000000, 0.000000000000000000 ) ) ;
#62226 = ORIENTED_EDGE ( 'NONE', *, *, #68093, .T. ) ;
#62227 = CARTESIAN_POINT ( 'NONE',  ( -7.250000000000000888, 7.250000000000001776, -13.00000000000000178 ) ) ;
#62228 = AXIS2_PLACEMENT_3D ( 'NONE', #61484, #13052, #34622 ) ;
#62229 =( NAMED_UNIT ( * ) PLANE_ANGLE_UNIT ( ) SI_UNIT ( $, .RADIAN. ) );
#62230 = DIRECTION ( 'NONE',  ( 1.000000000000000000, 0.000000000000000000, 0.000000000000000000 ) ) ;
#62231 = ORIENTED_EDGE ( 'NONE', *, *, #33828, .F. ) ;
#62232 = ORIENTED_EDGE ( 'NONE', *, *, #65791, .T. ) ;
#62233 = DIRECTION ( 'NONE',  ( -0.6414496315691698980, -0.7671651518152895477, -2.587583378555116957E-16 ) ) ;
#62234 = ORIENTED_EDGE ( 'NONE', *, *, #7806, .T. ) ;
#62235 = EDGE_LOOP ( 'NONE', ( #36777, #802, #52284, #24590 ) ) ;
#62236 = CARTESIAN_POINT ( 'NONE',  ( 46.39999999999999858, 21.00000000000000000, -2.750000000000000444 ) ) ;
#62237 = DIRECTION ( 'NONE',  ( 0.000000000000000000, 1.000000000000000000, 0.000000000000000000 ) ) ;
#62238 = FACE_OUTER_BOUND ( 'NONE', #41196, .T. ) ;
#62239 = AXIS2_PLACEMENT_3D ( 'NONE', #55330, #22111, #65257 ) ;
#62240 = FACE_OUTER_BOUND ( 'NONE', #37846, .T. ) ;
#62241 = VERTEX_POINT ( 'NONE', #1155 ) ;
#62242 = LINE ( 'NONE', #2844, #51479 ) ;
#62244 = DIRECTION ( 'NONE',  ( 0.000000000000000000, 1.000000000000000000, 0.000000000000000000 ) ) ;
#62243 = DIRECTION ( 'NONE',  ( 1.836970198721029934E-16, -1.836970198721036344E-16, 1.000000000000000000 ) ) ;
#62245 = ORIENTED_EDGE ( 'NONE', *, *, #30348, .F. ) ;
#62247 = ORIENTED_EDGE ( 'NONE', *, *, #65686, .T. ) ;
#62246 = DIRECTION ( 'NONE',  ( 0.000000000000000000, 0.000000000000000000, -1.000000000000000000 ) ) ;
#62248 = VERTEX_POINT ( 'NONE', #43927 ) ;
#62249 = EDGE_LOOP ( 'NONE', ( #69465, #39187, #67739, #48840 ) ) ;
#62250 = CARTESIAN_POINT ( 'NONE',  ( -8.250000000000001776, 7.250000000000000888, -12.50000000000000000 ) ) ;
#62251 = VECTOR ( 'NONE', #34344, 1000.000000000000114 ) ;
#62252 = EDGE_CURVE ( 'NONE', #9398, #45363, #5421, .T. ) ;
#62253 = LINE ( 'NONE', #29376, #51911 ) ;
#62254 = VECTOR ( 'NONE', #19142, 1000.000000000000000 ) ;
#62255 = ORIENTED_EDGE ( 'NONE', *, *, #9058, .T. ) ;
#62256 = ORIENTED_EDGE ( 'NONE', *, *, #28703, .T. ) ;
#62257 = EDGE_CURVE ( 'NONE', #53573, #59150, #6110, .T. ) ;
#62258 = CARTESIAN_POINT ( 'NONE',  ( 7.000000000000000000, -37.15000000000001279, -7.700000000000000178 ) ) ;
#62259 = EDGE_CURVE ( 'NONE', #41212, #55616, #33328, .T. ) ;
#62260 = FACE_OUTER_BOUND ( 'NONE', #43953, .T. ) ;
#62261 = ORIENTED_EDGE ( 'NONE', *, *, #51347, .F. ) ;
#62262 = VECTOR ( 'NONE', #22345, 1000.000000000000000 ) ;
#62263 = ORIENTED_EDGE ( 'NONE', *, *, #42186, .T. ) ;
#62264 = LINE ( 'NONE', #35745, #12707 ) ;
#62265 = EDGE_CURVE ( 'NONE', #59745, #27714, #59512, .T. ) ;
#62266 = DIRECTION ( 'NONE',  ( 1.000000000000000000, -0.000000000000000000, 0.000000000000000000 ) ) ;
#62267 = ORIENTED_EDGE ( 'NONE', *, *, #50059, .T. ) ;
#62268 = AXIS2_PLACEMENT_3D ( 'NONE', #37562, #22678, #7786 ) ;
#62269 = CARTESIAN_POINT ( 'NONE',  ( -11.00000000000000000, -17.50000000000000000, 26.64999999999999858 ) ) ;
#62270 = DIRECTION ( 'NONE',  ( 1.836970198721029934E-16, 1.836970198721010706E-16, -1.000000000000000000 ) ) ;
#62272 = ORIENTED_EDGE ( 'NONE', *, *, #27890, .F. ) ;
#62271 = LINE ( 'NONE', #46710, #32893 ) ;
#62273 = ORIENTED_EDGE ( 'NONE', *, *, #60089, .F. ) ;
#62275 = DIRECTION ( 'NONE',  ( 0.000000000000000000, 1.000000000000000000, -0.000000000000000000 ) ) ;
#62274 = AXIS2_PLACEMENT_3D ( 'NONE', #3690, #52486, #4050 ) ;
#62276 = FACE_OUTER_BOUND ( 'NONE', #34929, .T. ) ;
#62277 = DIRECTION ( 'NONE',  ( 0.000000000000000000, 0.000000000000000000, 1.000000000000000000 ) ) ;
#62278 = LINE ( 'NONE', #67946, #58378 ) ;
#62279 = DIRECTION ( 'NONE',  ( 0.000000000000000000, 0.000000000000000000, 1.000000000000000000 ) ) ;
#62280 = ADVANCED_FACE ( 'NONE', ( #6783 ), #27341, .F. ) ;
#62281 = CARTESIAN_POINT ( 'NONE',  ( -9.722976262117226653, -2.544523737882726344, 54.00000000000000711 ) ) ;
#62282 = CYLINDRICAL_SURFACE ( 'NONE', #34909, 4.500000000000188294 ) ;
#62283 = ORIENTED_EDGE ( 'NONE', *, *, #36142, .T. ) ;
#62284 = CARTESIAN_POINT ( 'NONE',  ( 31.89999999999999858, -0.1999999999911795112, 8.826273045769999343E-12 ) ) ;
#62286 = VERTEX_POINT ( 'NONE', #37603 ) ;
#62285 = LINE ( 'NONE', #13503, #55930 ) ;
#62287 = LINE ( 'NONE', #46725, #43442 ) ;
#62288 = DIRECTION ( 'NONE',  ( -1.000000000000000000, 0.000000000000000000, 0.000000000000000000 ) ) ;
#62289 = VECTOR ( 'NONE', #28779, 1000.000000000000000 ) ;
#62290 = DIRECTION ( 'NONE',  ( 0.000000000000000000, 0.000000000000000000, 1.000000000000000000 ) ) ;
#62291 = DIRECTION ( 'NONE',  ( -1.000000000000000000, 0.000000000000000000, 0.000000000000000000 ) ) ;
#62292 = CYLINDRICAL_SURFACE ( 'NONE', #11152, 0.5999999999999998668 ) ;
#62293 = ORIENTED_EDGE ( 'NONE', *, *, #36677, .T. ) ;
#62294 = DIRECTION ( 'NONE',  ( 1.000000000000000000, 0.000000000000000000, -0.000000000000000000 ) ) ;
#62295 = PLANE ( 'NONE',  #63290 ) ;
#62296 = ORIENTED_EDGE ( 'NONE', *, *, #37793, .F. ) ;
#62297 = DIRECTION ( 'NONE',  ( 0.000000000000000000, 0.000000000000000000, -1.000000000000000000 ) ) ;
#62298 = EDGE_CURVE ( 'NONE', #42454, #52350, #28025, .T. ) ;
#62299 = EDGE_CURVE ( 'NONE', #65403, #3828, #15563, .T. ) ;
#62300 = AXIS2_PLACEMENT_3D ( 'NONE', #40276, #34957, #27938 ) ;
#62301 = DIRECTION ( 'NONE',  ( 0.000000000000000000, 0.000000000000000000, -1.000000000000000000 ) ) ;
#62302 = VERTEX_POINT ( 'NONE', #65510 ) ;
#62303 = CARTESIAN_POINT ( 'NONE',  ( 7.826483450353380000, -11.78648345035349010, 455.0000000000000568 ) ) ;
#62304 = VERTEX_POINT ( 'NONE', #43587 ) ;
#62305 = EDGE_CURVE ( 'NONE', #63139, #38943, #38635, .T. ) ;
#62306 = VERTEX_POINT ( 'NONE', #65175 ) ;
#62307 = PLANE ( 'NONE',  #18860 ) ;
#62308 = PLANE ( 'NONE',  #21828 ) ;
#62309 = DIRECTION ( 'NONE',  ( -1.000000000000000000, 0.000000000000000000, 0.000000000000000000 ) ) ;
#62310 = VECTOR ( 'NONE', #67383, 1000.000000000000000 ) ;
#62311 = AXIS2_PLACEMENT_3D ( 'NONE', #2314, #29529, #23881 ) ;
#62312 = DIRECTION ( 'NONE',  ( 0.000000000000000000, 1.000000000000000000, 0.000000000000000000 ) ) ;
#62313 = CARTESIAN_POINT ( 'NONE',  ( 8.900000000000005684, -21.00000000000000000, 13.86939075806900057 ) ) ;
#62314 = VERTEX_POINT ( 'NONE', #125 ) ;
#62315 = ORIENTED_EDGE ( 'NONE', *, *, #69404, .F. ) ;
#62317 = EDGE_LOOP ( 'NONE', ( #724, #28601, #53375, #31403 ) ) ;
#62316 = DIRECTION ( 'NONE',  ( 0.000000000000000000, 0.000000000000000000, 1.000000000000000000 ) ) ;
#62318 = VECTOR ( 'NONE', #56241, 1000.000000000000000 ) ;
#62319 = EDGE_LOOP ( 'NONE', ( #40815, #49953, #7201, #52508 ) ) ;
#62320 = DIRECTION ( 'NONE',  ( -0.4999999999999832356, 0.000000000000000000, -0.8660254037844483666 ) ) ;
#62321 = CARTESIAN_POINT ( 'NONE',  ( 30.00000000000000000, -12.00000000000000000, 12.20000000000000107 ) ) ;
#62322 = CARTESIAN_POINT ( 'NONE',  ( -11.77351654964670935, 4.173516549646604901, 195.0000000000000284 ) ) ;
#62323 = CARTESIAN_POINT ( 'NONE',  ( 4.456444791733522252E-16, 7.450000000000002842, -9.500000000000001776 ) ) ;
#62324 = VECTOR ( 'NONE', #35064, 1000.000000000000000 ) ;
#62325 = DIRECTION ( 'NONE',  ( -0.000000000000000000, -0.000000000000000000, -1.000000000000000000 ) ) ;
#62326 = DIRECTION ( 'NONE',  ( 1.836970198721029934E-16, 1.836970198721010706E-16, -1.000000000000000000 ) ) ;
#62327 = ORIENTED_EDGE ( 'NONE', *, *, #52934, .F. ) ;
#62328 = ORIENTED_EDGE ( 'NONE', *, *, #9457, .T. ) ;
#62329 = ORIENTED_EDGE ( 'NONE', *, *, #56411, .F. ) ;
#62330 = ORIENTED_EDGE ( 'NONE', *, *, #10802, .T. ) ;
#62331 = DIRECTION ( 'NONE',  ( -0.000000000000000000, 0.000000000000000000, -1.000000000000000000 ) ) ;
#62332 = DIRECTION ( 'NONE',  ( 1.836970198721029934E-16, 1.836970198721010706E-16, -1.000000000000000000 ) ) ;
#62333 = EDGE_CURVE ( 'NONE', #20373, #38076, #16731, .T. ) ;
#62334 = CARTESIAN_POINT ( 'NONE',  ( 8.606483450353380249, -7.616533956692325802, 455.0000000000000568 ) ) ;
#62335 = ORIENTED_EDGE ( 'NONE', *, *, #40222, .F. ) ;
#62336 = ORIENTED_EDGE ( 'NONE', *, *, #44448, .T. ) ;
#62337 = ORIENTED_EDGE ( 'NONE', *, *, #16010, .F. ) ;
#62338 = CARTESIAN_POINT ( 'NONE',  ( -29.50000000000000355, -15.46862696659690073, -14.50000000000000000 ) ) ;
#62339 = ORIENTED_EDGE ( 'NONE', *, *, #67184, .T. ) ;
#62340 = ORIENTED_EDGE ( 'NONE', *, *, #5996, .T. ) ;
#62341 = EDGE_CURVE ( 'NONE', #56310, #61891, #65844, .T. ) ;
#62342 = LINE ( 'NONE', #22189, #10793 ) ;
#62343 = CIRCLE ( 'NONE', #5886, 2.000000000000001776 ) ;
#62344 = EDGE_CURVE ( 'NONE', #11392, #52946, #17802, .T. ) ;
#62345 = ORIENTED_EDGE ( 'NONE', *, *, #61311, .F. ) ;
#62346 = ORIENTED_EDGE ( 'NONE', *, *, #69164, .F. ) ;
#62347 = CARTESIAN_POINT ( 'NONE',  ( 30.90000000000000213, 0.000000000000000000, 0.000000000000000000 ) ) ;
#62348 = EDGE_CURVE ( 'NONE', #49054, #39974, #42638, .T. ) ;
#62349 = ADVANCED_FACE ( 'NONE', ( #40708 ), #29053, .F. ) ;
#62351 = VERTEX_POINT ( 'NONE', #62269 ) ;
#62350 = DIRECTION ( 'NONE',  ( -0.000000000000000000, 1.000000000000000000, -0.000000000000000000 ) ) ;
#62352 = ORIENTED_EDGE ( 'NONE', *, *, #11192, .T. ) ;
#62353 = CARTESIAN_POINT ( 'NONE',  ( 275.0000000000000000, -30.80000000000000071, 12.20000000000000107 ) ) ;
#62354 = LINE ( 'NONE', #45390, #41960 ) ;
#62355 = EDGE_CURVE ( 'NONE', #6680, #62579, #50561, .T. ) ;
#62356 = PLANE ( 'NONE',  #59561 ) ;
#62357 = CIRCLE ( 'NONE', #58993, 0.4000000000000010214 ) ;
#62359 = VERTEX_POINT ( 'NONE', #34699 ) ;
#62358 = CARTESIAN_POINT ( 'NONE',  ( -9.915476262117200790, -0.9555237378827209360, 54.00000000000000711 ) ) ;
#62360 = EDGE_LOOP ( 'NONE', ( #63053, #66448, #9399, #51002 ) ) ;
#62361 = LINE ( 'NONE', #33748, #27201 ) ;
#62362 = VECTOR ( 'NONE', #27388, 1000.000000000000000 ) ;
#62363 = DIRECTION ( 'NONE',  ( 8.339399738404099512E-15, 1.000000000000000000, 1.836970198721025990E-16 ) ) ;
#62364 = CARTESIAN_POINT ( 'NONE',  ( 3.857023737882779635, -10.31452373788281029, 54.00000000000000711 ) ) ;
#62365 = EDGE_LOOP ( 'NONE', ( #664, #48244 ) ) ;
#62366 = DIRECTION ( 'NONE',  ( 0.7071067811865474617, 0.7071067811865474617, 2.597868168706479611E-16 ) ) ;
#62367 = DIRECTION ( 'NONE',  ( -0.000000000000000000, 3.673940397442059868E-16, -1.000000000000000000 ) ) ;
#62368 = AXIS2_PLACEMENT_3D ( 'NONE', #49308, #26337, #11454 ) ;
#62369 = CARTESIAN_POINT ( 'NONE',  ( 46.39999999999999858, 21.00000000000000000, 1.750000000000000222 ) ) ;
#62370 = VERTEX_POINT ( 'NONE', #46017 ) ;
#62371 = DIRECTION ( 'NONE',  ( 0.000000000000000000, 1.000000000000000000, 0.000000000000000000 ) ) ;
#62373 = CARTESIAN_POINT ( 'NONE',  ( -25.50000000000000355, 0.000000000000000000, 22.50000000000000000 ) ) ;
#62372 = VECTOR ( 'NONE', #8017, 1000.000000000000000 ) ;
#62374 = DIRECTION ( 'NONE',  ( 0.000000000000000000, -1.000000000000000000, 0.000000000000000000 ) ) ;
#62375 = VERTEX_POINT ( 'NONE', #66191 ) ;
#62376 = CARTESIAN_POINT ( 'NONE',  ( 3.664523737882819709, 10.30047626211720413, 54.00000000000000711 ) ) ;
#62377 = LINE ( 'NONE', #36214, #52560 ) ;
#62378 = ORIENTED_EDGE ( 'NONE', *, *, #59973, .T. ) ;
#62379 = PLANE ( 'NONE',  #7852 ) ;
#62380 = FACE_OUTER_BOUND ( 'NONE', #49404, .T. ) ;
#62381 = CARTESIAN_POINT ( 'NONE',  ( -11.00000000000000000, -16.64230188589299786, 14.64519951917100116 ) ) ;
#62382 = EDGE_CURVE ( 'NONE', #35045, #46508, #39249, .T. ) ;
#62383 = EDGE_CURVE ( 'NONE', #36022, #47486, #13836, .T. ) ;
#62384 = DIRECTION ( 'NONE',  ( -1.000000000000000000, 0.000000000000000000, 0.000000000000000000 ) ) ;
#62385 = CARTESIAN_POINT ( 'NONE',  ( -7.250000000000000888, 7.250000000000001776, -24.50000000000000000 ) ) ;
#62386 = VERTEX_POINT ( 'NONE', #24091 ) ;
#62387 = CARTESIAN_POINT ( 'NONE',  ( -10.30047626211725031, -3.857023737882713466, 54.00000000000000711 ) ) ;
#62388 = FACE_OUTER_BOUND ( 'NONE', #28051, .T. ) ;
#62389 = VECTOR ( 'NONE', #18922, 1000.000000000000000 ) ;
#62390 = DIRECTION ( 'NONE',  ( -2.891205793294675467E-15, -1.000000000000000000, 0.000000000000000000 ) ) ;
#62391 = EDGE_CURVE ( 'NONE', #28477, #34023, #34336, .T. ) ;
#62392 = PLANE ( 'NONE',  #35360 ) ;
#62393 = DIRECTION ( 'NONE',  ( -0.000000000000000000, -1.000000000000000000, 0.000000000000000000 ) ) ;
#62394 = CIRCLE ( 'NONE', #59038, 0.5000000000009441337 ) ;
#62395 = ORIENTED_EDGE ( 'NONE', *, *, #23994, .T. ) ;
#62397 = ORIENTED_EDGE ( 'NONE', *, *, #19977, .T. ) ;
#62396 = CARTESIAN_POINT ( 'NONE',  ( 15.70366306705350112, -0.2717122460102739390, -23.82579074638668004 ) ) ;
#62398 = DIRECTION ( 'NONE',  ( -1.000000000000000000, 0.000000000000000000, 0.000000000000000000 ) ) ;
#62399 = LINE ( 'NONE', #20672, #41309 ) ;
#62400 = CARTESIAN_POINT ( 'NONE',  ( 17.00000000000000000, -15.50000000000000000, -14.50000000000000000 ) ) ;
#62401 = EDGE_LOOP ( 'NONE', ( #43381, #4633, #32246, #56848, #25629, #45443, #17118, #49147 ) ) ;
#62402 = LINE ( 'NONE', #1974, #6986 ) ;
#62403 = ORIENTED_EDGE ( 'NONE', *, *, #57023, .T. ) ;
#62404 = ORIENTED_EDGE ( 'NONE', *, *, #11062, .F. ) ;
#62405 = VERTEX_POINT ( 'NONE', #50624 ) ;
#62406 = DIRECTION ( 'NONE',  ( 0.000000000000000000, 0.000000000000000000, -1.000000000000000000 ) ) ;
#62407 = DIRECTION ( 'NONE',  ( -1.000000000000000000, 1.671920889371702657E-15, 0.000000000000000000 ) ) ;
#62408 = CARTESIAN_POINT ( 'NONE',  ( 15.50000000000000000, -0.4000000000000000222, 22.50000000000000000 ) ) ;
#62409 = CARTESIAN_POINT ( 'NONE',  ( 7.250000000000005329, 8.250000000000001776, -20.50000000000000000 ) ) ;
#62410 = VECTOR ( 'NONE', #8229, 1000.000000000000000 ) ;
#62411 = ORIENTED_EDGE ( 'NONE', *, *, #36591, .F. ) ;
#62412 = ORIENTED_EDGE ( 'NONE', *, *, #20407, .T. ) ;
#62413 = FACE_OUTER_BOUND ( 'NONE', #9559, .T. ) ;
#62414 = AXIS2_PLACEMENT_3D ( 'NONE', #13606, #35158, #8288 ) ;
#62415 = DIRECTION ( 'NONE',  ( 0.000000000000000000, 0.000000000000000000, 1.000000000000000000 ) ) ;
#62416 = VERTEX_POINT ( 'NONE', #2182 ) ;
#62417 = VECTOR ( 'NONE', #52231, 1000.000000000000114 ) ;
#62418 = ORIENTED_EDGE ( 'NONE', *, *, #57166, .T. ) ;
#62419 = VERTEX_POINT ( 'NONE', #45300 ) ;
#62420 = CARTESIAN_POINT ( 'NONE',  ( 17.00000000000000000, -16.64230188589299786, -14.64519951917100116 ) ) ;
#62421 = CIRCLE ( 'NONE', #38716, 0.1749999999999998224 ) ;
#62422 = EDGE_CURVE ( 'NONE', #24533, #21671, #53960, .T. ) ;
#62424 = ORIENTED_EDGE ( 'NONE', *, *, #38205, .F. ) ;
#62423 = DIRECTION ( 'NONE',  ( -0.5773502691896270633, 0.5773502691896270633, -0.5773502691896230665 ) ) ;
#62425 = LINE ( 'NONE', #61376, #26614 ) ;
#62426 = AXIS2_PLACEMENT_3D ( 'NONE', #39224, #33234, #11646 ) ;
#62427 = LINE ( 'NONE', #13999, #18222 ) ;
#62428 = EDGE_CURVE ( 'NONE', #11348, #61661, #44603, .T. ) ;
#62429 = EDGE_CURVE ( 'NONE', #62021, #58452, #12424, .T. ) ;
#62430 = ORIENTED_EDGE ( 'NONE', *, *, #41942, .F. ) ;
#62431 = ORIENTED_EDGE ( 'NONE', *, *, #1602, .T. ) ;
#62432 = AXIS2_PLACEMENT_3D ( 'NONE', #33363, #16066, #10749 ) ;
#62433 = DIRECTION ( 'NONE',  ( -1.000000000000000000, 0.000000000000000000, 0.000000000000000000 ) ) ;
#62434 = DIRECTION ( 'NONE',  ( 0.000000000000000000, 0.000000000000000000, 1.000000000000000000 ) ) ;
#62435 = VECTOR ( 'NONE', #14082, 1000.000000000000000 ) ;
#62436 = DIRECTION ( 'NONE',  ( -0.7071067811865475727, -0.7071067811865475727, 0.000000000000000000 ) ) ;
#62437 = EDGE_CURVE ( 'NONE', #26720, #23985, #39320, .T. ) ;
#62438 = CARTESIAN_POINT ( 'NONE',  ( 7.249999999999995559, -7.848062532927998269, -1.000000000000000000 ) ) ;
#62439 = DIRECTION ( 'NONE',  ( -0.7071067811865487940, -0.7071067811865463515, -0.000000000000000000 ) ) ;
#62441 = EDGE_LOOP ( 'NONE', ( #66168, #2880, #49379, #19152, #27889, #47882, #13726 ) ) ;
#62440 =( NAMED_UNIT ( * ) PLANE_ANGLE_UNIT ( ) SI_UNIT ( $, .RADIAN. ) );
#62442 = VERTEX_POINT ( 'NONE', #29741 ) ;
#62443 = CARTESIAN_POINT ( 'NONE',  ( 10.05377373788281048, 8.916576262117187568, 26.00000000000000711 ) ) ;
#62444 = DIRECTION ( 'NONE',  ( 0.000000000000000000, -1.000000000000000000, 0.000000000000000000 ) ) ;
#62445 = LINE ( 'NONE', #68116, #5934 ) ;
#62446 = DIRECTION ( 'NONE',  ( 1.000000000000000000, 0.000000000000000000, 0.000000000000000000 ) ) ;
#62447 = DIRECTION ( 'NONE',  ( 3.510749891857827507E-15, 1.000000000000000000, 0.000000000000000000 ) ) ;
#62448 = ORIENTED_EDGE ( 'NONE', *, *, #9509, .T. ) ;
#62449 = CARTESIAN_POINT ( 'NONE',  ( 30.00000000000000000, -5.599999999999999645, 9.400000000000000355 ) ) ;
#62450 = CARTESIAN_POINT ( 'NONE',  ( 11.50000000000000000, -11.50000000000000000, -15.00000000000000000 ) ) ;
#62451 = DIRECTION ( 'NONE',  ( 1.000000000000000000, 0.000000000000000000, 0.000000000000000000 ) ) ;
#62452 = FACE_OUTER_BOUND ( 'NONE', #36854, .T. ) ;
#62453 = CIRCLE ( 'NONE', #68129, 24.99999999998794920 ) ;
#62454 = DIRECTION ( 'NONE',  ( -1.000000000000000000, 0.000000000000000000, 0.000000000000000000 ) ) ;
#62455 = LINE ( 'NONE', #3778, #11544 ) ;
#62456 = AXIS2_PLACEMENT_3D ( 'NONE', #14660, #6737, #45600 ) ;
#62457 = DIRECTION ( 'NONE',  ( -0.000000000000000000, -0.000000000000000000, 1.000000000000000000 ) ) ;
#62458 = VECTOR ( 'NONE', #46487, 1000.000000000000114 ) ;
#62459 = ORIENTED_EDGE ( 'NONE', *, *, #56129, .F. ) ;
#62460 = VECTOR ( 'NONE', #49908, 1000.000000000000000 ) ;
#62461 = DIRECTION ( 'NONE',  ( 1.836970198721029934E-16, 1.836970198721010706E-16, -1.000000000000000000 ) ) ;
#62462 = CARTESIAN_POINT ( 'NONE',  ( -1.077516549646670541, 11.33351654964656596, 455.0000000000000568 ) ) ;
#62463 = ORIENTED_EDGE ( 'NONE', *, *, #27802, .T. ) ;
#62464 = CARTESIAN_POINT ( 'NONE',  ( -9.093516549646771807, -10.09643294401451286, 195.0000000000000284 ) ) ;
#62465 = CARTESIAN_POINT ( 'NONE',  ( 10.50702373788281996, -6.849523737882823760, 54.00000000000000711 ) ) ;
#62466 = EDGE_CURVE ( 'NONE', #6379, #43564, #45649, .T. ) ;
#62467 = DIRECTION ( 'NONE',  ( -0.5773502691896230665, -0.5773502691896271743, 0.5773502691896271743 ) ) ;
#62469 = VECTOR ( 'NONE', #42296, 1000.000000000000114 ) ;
#62468 = LINE ( 'NONE', #8027, #53419 ) ;
#62470 = CARTESIAN_POINT ( 'NONE',  ( -15.50000000000000000, -0.1999999999999999556, 22.50000000000000000 ) ) ;
#62471 = VERTEX_POINT ( 'NONE', #50272 ) ;
#62472 = CARTESIAN_POINT ( 'NONE',  ( 6.364920264886885448, -6.836383711243021466, 54.00000000000000711 ) ) ;
#62473 = ORIENTED_EDGE ( 'NONE', *, *, #37024, .F. ) ;
#62474 = LINE ( 'NONE', #17352, #19154 ) ;
#62475 = CARTESIAN_POINT ( 'NONE',  ( -4.393516549646667713, 11.77351654964658856, 455.0000000000000568 ) ) ;
#62476 = VERTEX_POINT ( 'NONE', #7477 ) ;
#62477 = CARTESIAN_POINT ( 'NONE',  ( -4.727349090213461835, 4.188533722949259186, 455.0000000000000568 ) ) ;
#62478 = EDGE_CURVE ( 'NONE', #67217, #44960, #50401, .T. ) ;
#62479 = CIRCLE ( 'NONE', #39864, 0.3499999999999611200 ) ;
#62480 = ORIENTED_EDGE ( 'NONE', *, *, #6976, .F. ) ;
#62481 = SHAPE_REPRESENTATION ( 'HOLDING PLATE', ( #45918 ), #69670 ) ;
#62482 = EDGE_CURVE ( 'NONE', #67667, #15946, #28698, .T. ) ;
#62483 = CARTESIAN_POINT ( 'NONE',  ( 7.450000000000004619, -1.336933437520057563E-15, -15.50000000000000000 ) ) ;
#62484 = ORIENTED_EDGE ( 'NONE', *, *, #8156, .F. ) ;
#62485 = VERTEX_POINT ( 'NONE', #56273 ) ;
#62486 = CARTESIAN_POINT ( 'NONE',  ( 35.89999999999999858, 0.000000000000000000, 2.458500000000000796 ) ) ;
#62487 = ORIENTED_EDGE ( 'NONE', *, *, #48517, .F. ) ;
#62488 = ORIENTED_EDGE ( 'NONE', *, *, #37894, .T. ) ;
#62489 = DIRECTION ( 'NONE',  ( -1.836970198721029934E-16, 1.836970198721036344E-16, -1.000000000000000000 ) ) ;
#62490 = DIRECTION ( 'NONE',  ( -1.000000000000000000, 0.000000000000000000, 0.000000000000000000 ) ) ;
#62491 = LINE ( 'NONE', #14064, #9605 ) ;
#62492 = VERTEX_POINT ( 'NONE', #7821 ) ;
#62493 = CIRCLE ( 'NONE', #69289, 0.9999999999999991118 ) ;
#62494 = FACE_OUTER_BOUND ( 'NONE', #59087, .T. ) ;
#62496 = CYLINDRICAL_SURFACE ( 'NONE', #23150, 0.1999999999999987899 ) ;
#62495 = DIRECTION ( 'NONE',  ( 0.000000000000000000, 0.000000000000000000, 1.000000000000000000 ) ) ;
#62497 = ORIENTED_EDGE ( 'NONE', *, *, #25579, .T. ) ;
#62499 = ORIENTED_EDGE ( 'NONE', *, *, #56860, .T. ) ;
#62498 = DIRECTION ( 'NONE',  ( 1.000000000000000000, -0.000000000000000000, 0.000000000000000000 ) ) ;
#62500 = EDGE_LOOP ( 'NONE', ( #54972, #33469, #46501, #52094 ) ) ;
#62501 = APPLICATION_PROTOCOL_DEFINITION ( 'draft international standard', 'automotive_design', 1998, #44027 ) ;
#62502 = APPLICATION_CONTEXT ( 'automotive_design' ) ;
#62503 = CARTESIAN_POINT ( 'NONE',  ( 10.31452373788277654, 3.650476262117150483, 26.00000000000000711 ) ) ;
#62505 = ORIENTED_EDGE ( 'NONE', *, *, #48465, .T. ) ;
#62504 = CARTESIAN_POINT ( 'NONE',  ( 5.257023737882795977, 5.242976262117205799, 26.00000000000000711 ) ) ;
#62506 = EDGE_CURVE ( 'NONE', #28450, #19822, #67232, .T. ) ;
#62507 = DIRECTION ( 'NONE',  ( 0.000000000000000000, -5.800915303574361727E-12, -1.000000000000000000 ) ) ;
#62508 = AXIS2_PLACEMENT_3D ( 'NONE', #67537, #14125, #28637 ) ;
#62509 = VECTOR ( 'NONE', #42254, 1000.000000000000000 ) ;
#62510 = DIRECTION ( 'NONE',  ( -1.000000000000000000, 0.000000000000000000, 0.000000000000000000 ) ) ;
#62511 = EDGE_CURVE ( 'NONE', #187, #41721, #61923, .T. ) ;
#62512 = ORIENTED_EDGE ( 'NONE', *, *, #6019, .T. ) ;
#62513 = EDGE_CURVE ( 'NONE', #20566, #49587, #14538, .T. ) ;
#62514 = VERTEX_POINT ( 'NONE', #41405 ) ;
#62515 = VECTOR ( 'NONE', #50660, 1000.000000000000000 ) ;
#62516 = VECTOR ( 'NONE', #61672, 1000.000000000000000 ) ;
#62517 = DIRECTION ( 'NONE',  ( 1.000000000000000000, 0.000000000000000000, 0.000000000000000000 ) ) ;
#62518 = EDGE_CURVE ( 'NONE', #15490, #13113, #30804, .T. ) ;
#62519 = ORIENTED_EDGE ( 'NONE', *, *, #54393, .T. ) ;
#62520 = ADVANCED_FACE ( 'NONE', ( #24799 ), #9241, .F. ) ;
#62521 = DIRECTION ( 'NONE',  ( -1.047444401652940007E-14, -1.000000000000000000, -1.836970198721029934E-16 ) ) ;
#62522 = DIRECTION ( 'NONE',  ( 9.912705577010312730E-15, 1.000000000000000000, 0.000000000000000000 ) ) ;
#62523 = CIRCLE ( 'NONE', #51225, 1.399999999999998579 ) ;
#62524 = AXIS2_PLACEMENT_3D ( 'NONE', #1124, #22682, #17368 ) ;
#62525 = AXIS2_PLACEMENT_3D ( 'NONE', #66526, #33988, #66862 ) ;
#62526 = EDGE_CURVE ( 'NONE', #34832, #45723, #28946, .T. ) ;
#62527 = CARTESIAN_POINT ( 'NONE',  ( -7.447976262117260049, 9.880476262117177555, 25.99999580000000421 ) ) ;
#62528 = EDGE_LOOP ( 'NONE', ( #51918, #50965, #4492, #31949 ) ) ;
#62529 = ADVANCED_FACE ( 'NONE', ( #25512 ), #68286, .T. ) ;
#62530 = DIRECTION ( 'NONE',  ( 0.000000000000000000, 0.000000000000000000, -1.000000000000000000 ) ) ;
#62531 = LINE ( 'NONE', #39910, #40464 ) ;
#62533 = ORIENTED_EDGE ( 'NONE', *, *, #16790, .T. ) ;
#62532 =( NAMED_UNIT ( * ) PLANE_ANGLE_UNIT ( ) SI_UNIT ( $, .RADIAN. ) );
#62535 = ORIENTED_EDGE ( 'NONE', *, *, #39298, .F. ) ;
#62534 = CARTESIAN_POINT ( 'NONE',  ( 4.720772854004780861, 4.141586236041042923, 54.00000000000000711 ) ) ;
#62536 = DIRECTION ( 'NONE',  ( -0.7071067811865475727, -0.7071067811865475727, -2.597868168706480597E-16 ) ) ;
#62537 = DIRECTION ( 'NONE',  ( -1.000000000000000000, 0.000000000000000000, 0.000000000000000000 ) ) ;
#62538 = DIRECTION ( 'NONE',  ( -1.000000000000000000, 0.000000000000000000, 0.000000000000000000 ) ) ;
#62539 = CARTESIAN_POINT ( 'NONE',  ( 283.0000000000000568, -42.50000000000000000, 14.50000000000000000 ) ) ;
#62540 = CARTESIAN_POINT ( 'NONE',  ( 12.00648345035340903, 7.813516549646560172, 455.0000000000000568 ) ) ;
#62541 = ORIENTED_EDGE ( 'NONE', *, *, #34095, .F. ) ;
#62542 = DIRECTION ( 'NONE',  ( 1.000000000000000000, -1.047444401652940007E-14, 1.836970198721010706E-16 ) ) ;
#62543 = FACE_OUTER_BOUND ( 'NONE', #25223, .T. ) ;
#62544 = LINE ( 'NONE', #30031, #48127 ) ;
#62546 = ORIENTED_EDGE ( 'NONE', *, *, #68882, .F. ) ;
#62545 = CARTESIAN_POINT ( 'NONE',  ( -15.50000000000000000, -15.50000000000000000, 22.50000000000000000 ) ) ;
#62547 = LINE ( 'NONE', #31100, #47129 ) ;
#62548 = EDGE_CURVE ( 'NONE', #54687, #23129, #22201, .T. ) ;
#62549 = CARTESIAN_POINT ( 'NONE',  ( 15.50000000000000000, -15.50000000000000000, -22.50000000000000000 ) ) ;
#62550 = ORIENTED_EDGE ( 'NONE', *, *, #50456, .F. ) ;
#62551 = CARTESIAN_POINT ( 'NONE',  ( 4.206483450353374565, 11.31351654964663034, 195.0000000000000284 ) ) ;
#62552 = LINE ( 'NONE', #25095, #6887 ) ;
#62553 = AXIS2_PLACEMENT_3D ( 'NONE', #54756, #59018, #5290 ) ;
#62554 = ORIENTED_EDGE ( 'NONE', *, *, #37452, .T. ) ;
#62555 = ADVANCED_FACE ( 'NONE', ( #46358 ), #9952, .F. ) ;
#62556 = DIRECTION ( 'NONE',  ( -1.000000000000000000, 0.000000000000000000, 0.000000000000000000 ) ) ;
#62557 = PLANE ( 'NONE',  #42279 ) ;
#62558 = CARTESIAN_POINT ( 'NONE',  ( 9.899999999999998579, -21.00000000000000355, -14.57806571531352269 ) ) ;
#62559 = ADVANCED_FACE ( 'NONE', ( #42461 ), #25152, .T. ) ;
#62560 = CARTESIAN_POINT ( 'NONE',  ( 7.000000000000000000, -32.94999999999885176, 8.199999999997979572 ) ) ;
#62561 = AXIS2_PLACEMENT_3D ( 'NONE', #66393, #29948, #33858 ) ;
#62562 = AXIS2_PLACEMENT_3D ( 'NONE', #6530, #16437, #27394 ) ;
#62563 = ORIENTED_EDGE ( 'NONE', *, *, #68978, .F. ) ;
#62564 = DIRECTION ( 'NONE',  ( -1.000000000000000000, 0.000000000000000000, 0.000000000000000000 ) ) ;
#62565 = EDGE_LOOP ( 'NONE', ( #55299, #51376, #57357, #49326 ) ) ;
#62566 = VERTEX_POINT ( 'NONE', #62983 ) ;
#62567 = VERTEX_POINT ( 'NONE', #4305 ) ;
#62568 = FACE_OUTER_BOUND ( 'NONE', #62249, .T. ) ;
#62569 = VECTOR ( 'NONE', #4606, 1000.000000000000000 ) ;
#62570 = CIRCLE ( 'NONE', #20848, 1.000000000000000000 ) ;
#62571 = CARTESIAN_POINT ( 'NONE',  ( 7.250000000000004441, 7.450000000000001954, -19.50000000000000000 ) ) ;
#62572 = AXIS2_PLACEMENT_3D ( 'NONE', #61818, #39536, #28584 ) ;
#62573 = EDGE_CURVE ( 'NONE', #27098, #12341, #45908, .T. ) ;
#62574 = CARTESIAN_POINT ( 'NONE',  ( -7.250000000000000888, 7.250000000000001776, -19.00000000000000000 ) ) ;
#62575 = ORIENTED_EDGE ( 'NONE', *, *, #57053, .T. ) ;
#62576 = ORIENTED_EDGE ( 'NONE', *, *, #55462, .F. ) ;
#62577 = DIRECTION ( 'NONE',  ( 0.000000000000000000, 1.000000000000000000, 0.000000000000000000 ) ) ;
#62578 = ORIENTED_EDGE ( 'NONE', *, *, #67848, .T. ) ;
#62579 = VERTEX_POINT ( 'NONE', #63332 ) ;
#62580 = DIRECTION ( 'NONE',  ( 0.000000000000000000, 1.000000000000000000, 0.000000000000000000 ) ) ;
#62581 = CARTESIAN_POINT ( 'NONE',  ( -7.250000000000001776, -7.249999999999998224, -16.50000000000000000 ) ) ;
#62582 = DIRECTION ( 'NONE',  ( -1.000000000000000000, 0.000000000000000000, 0.000000000000000000 ) ) ;
#62583 = CARTESIAN_POINT ( 'NONE',  ( 49.00000000000000000, -0.2000000000089119934, -8.913009219568841313E-12 ) ) ;
#62584 = ADVANCED_FACE ( 'NONE', ( #20891 ), #14897, .F. ) ;
#62585 = VERTEX_POINT ( 'NONE', #47762 ) ;
#62587 = EDGE_CURVE ( 'NONE', #36987, #28218, #37174, .T. ) ;
#62586 = CIRCLE ( 'NONE', #27576, 1.000000000000000000 ) ;
#62588 = LINE ( 'NONE', #10264, #35666 ) ;
#62590 = DIRECTION ( 'NONE',  ( -1.000000000000000000, 0.000000000000000000, 0.000000000000000000 ) ) ;
#62589 = DIRECTION ( 'NONE',  ( 0.000000000000000000, 1.000000000000000000, 0.000000000000000000 ) ) ;
#62591 = EDGE_LOOP ( 'NONE', ( #60190, #33237, #23413, #46558 ) ) ;
#62594 = ADVANCED_FACE ( 'NONE', ( #36822 ), #62618, .T. ) ;
#62593 = ORIENTED_EDGE ( 'NONE', *, *, #28485, .F. ) ;
#62592 = LINE ( 'NONE', #30433, #39828 ) ;
#62595 = ORIENTED_EDGE ( 'NONE', *, *, #64381, .F. ) ;
#62596 = ORIENTED_EDGE ( 'NONE', *, *, #33220, .F. ) ;
#62597 = EDGE_CURVE ( 'NONE', #24588, #33736, #57324, .T. ) ;
#62598 = EDGE_CURVE ( 'NONE', #36828, #1391, #8663, .T. ) ;
#62599 = DIRECTION ( 'NONE',  ( 1.883404846338789915E-14, 1.000000000000000000, 1.836970198721045465E-16 ) ) ;
#62600 = EDGE_CURVE ( 'NONE', #42804, #30522, #63690, .T. ) ;
#62601 = DIRECTION ( 'NONE',  ( -1.836970198721029934E-16, 1.836970198721036344E-16, -1.000000000000000000 ) ) ;
#62602 = EDGE_CURVE ( 'NONE', #51028, #62370, #3588, .T. ) ;
#62603 = ORIENTED_EDGE ( 'NONE', *, *, #33697, .T. ) ;
#62604 = ORIENTED_EDGE ( 'NONE', *, *, #38282, .T. ) ;
#62605 = ADVANCED_FACE ( 'NONE', ( #64388 ), #16646, .T. ) ;
#62606 = CARTESIAN_POINT ( 'NONE',  ( -7.342976262117293373, -6.665817930929262225, 54.00000000000000711 ) ) ;
#62607 = DIRECTION ( 'NONE',  ( -0.000000000000000000, 3.673940397442059868E-16, -1.000000000000000000 ) ) ;
#62608 = VECTOR ( 'NONE', #26072, 1000.000000000000000 ) ;
#62609 = ORIENTED_EDGE ( 'NONE', *, *, #5202, .T. ) ;
#62610 = ORIENTED_EDGE ( 'NONE', *, *, #37344, .T. ) ;
#62611 = CARTESIAN_POINT ( 'NONE',  ( 24.00000000000000000, -15.50000000000000000, -14.50000000000000000 ) ) ;
#62612 = EDGE_CURVE ( 'NONE', #39955, #55314, #44180, .T. ) ;
#62613 = CARTESIAN_POINT ( 'NONE',  ( -7.250000000000001776, -7.249999999999998224, -20.50000000000000000 ) ) ;
#62614 = ORIENTED_EDGE ( 'NONE', *, *, #55267, .F. ) ;
#62615 = EDGE_CURVE ( 'NONE', #12122, #6097, #48122, .T. ) ;
#62616 = AXIS2_PLACEMENT_3D ( 'NONE', #50394, #7947, #29523 ) ;
#62617 = VECTOR ( 'NONE', #58801, 1000.000000000000000 ) ;
#62618 = CYLINDRICAL_SURFACE ( 'NONE', #31256, 24.99999999998789946 ) ;
#62619 = DIRECTION ( 'NONE',  ( -1.000000000000000000, 0.000000000000000000, 0.000000000000000000 ) ) ;
#62621 = ORIENTED_EDGE ( 'NONE', *, *, #27658, .T. ) ;
#62620 = CARTESIAN_POINT ( 'NONE',  ( 6.832023737882818359, -9.737023737882822161, 54.00000000000000711 ) ) ;
#62622 = ORIENTED_EDGE ( 'NONE', *, *, #9607, .T. ) ;
#62623 = FACE_OUTER_BOUND ( 'NONE', #22173, .T. ) ;
#62624 = AXIS2_PLACEMENT_3D ( 'NONE', #44496, #17635, #49133 ) ;
#62625 = VECTOR ( 'NONE', #41716, 1000.000000000000000 ) ;
#62626 = CARTESIAN_POINT ( 'NONE',  ( -29.50000000000000355, -11.50000000000000000, -11.00000000000000000 ) ) ;
#62627 = ADVANCED_FACE ( 'NONE', ( #376 ), #26551, .T. ) ;
#62628 = DIRECTION ( 'NONE',  ( 0.7071067811865500152, 0.7071067811865451302, -4.683861624749757595E-31 ) ) ;
#62629 = DIRECTION ( 'NONE',  ( 1.836970198721029934E-16, -1.836970198721036344E-16, 1.000000000000000000 ) ) ;
#62630 = FACE_OUTER_BOUND ( 'NONE', #64349, .T. ) ;
#62631 = AXIS2_PLACEMENT_3D ( 'NONE', #60247, #16784, #54973 ) ;
#62632 = CARTESIAN_POINT ( 'NONE',  ( 5.257023737882819070, -5.257023737882825287, 54.00000000000000711 ) ) ;
#62633 = VERTEX_POINT ( 'NONE', #59767 ) ;
#62634 = DIRECTION ( 'NONE',  ( -1.000000000000000000, 0.000000000000000000, 0.000000000000000000 ) ) ;
#62636 = VERTEX_POINT ( 'NONE', #11316 ) ;
#62635 = CARTESIAN_POINT ( 'NONE',  ( -29.50000000000000355, -15.97213595500069871, 14.50000000000000000 ) ) ;
#62637 = DIRECTION ( 'NONE',  ( 1.000000000000000000, -0.000000000000000000, 0.000000000000000000 ) ) ;
#62638 = PRESENTATION_LAYER_ASSIGNMENT (  '', '', ( #11849 ) ) ;
#62639 = CARTESIAN_POINT ( 'NONE',  ( -5.242976262117259978, 5.242976262117182706, 54.00000000000000711 ) ) ;
#62640 = CIRCLE ( 'NONE', #32174, 0.1749999999999998224 ) ;
#62641 = VECTOR ( 'NONE', #44495, 1000.000000000000000 ) ;
#62642 = CARTESIAN_POINT ( 'NONE',  ( -11.00000000000000000, -12.00000000000000000, -10.20500000000000007 ) ) ;
#62643 = DIRECTION ( 'NONE',  ( 0.000000000000000000, 0.000000000000000000, 1.000000000000000000 ) ) ;
#62644 = EDGE_LOOP ( 'NONE', ( #53832, #7280, #31338, #23488 ) ) ;
#62645 = CARTESIAN_POINT ( 'NONE',  ( 146.5599459900709860, 9.000000000000001776, 328.5239988703752942 ) ) ;
#62646 = DIRECTION ( 'NONE',  ( 0.000000000000000000, 1.000000000000000000, 0.000000000000000000 ) ) ;
#62647 = EDGE_LOOP ( 'NONE', ( #12916, #18634, #41476, #51816 ) ) ;
#62648 = EDGE_CURVE ( 'NONE', #61023, #17140, #65424, .T. ) ;
#62649 = EDGE_CURVE ( 'NONE', #58319, #57460, #43654, .T. ) ;
#62650 = DIRECTION ( 'NONE',  ( -7.751221965937476285E-17, 1.000000000000000000, 0.000000000000000000 ) ) ;
#62651 = EDGE_LOOP ( 'NONE', ( #65872, #62010, #35151, #771 ) ) ;
#62652 = DIRECTION ( 'NONE',  ( -1.000000000000000000, 0.000000000000000000, 0.000000000000000000 ) ) ;
#62653 = ORIENTED_EDGE ( 'NONE', *, *, #18201, .F. ) ;
#62654 = EDGE_CURVE ( 'NONE', #33386, #41057, #49504, .T. ) ;
#62655 = VERTEX_POINT ( 'NONE', #15943 ) ;
#62656 = CARTESIAN_POINT ( 'NONE',  ( 10.90000000000000036, -14.06939075806902117, -20.80000000000000426 ) ) ;
#62657 = CARTESIAN_POINT ( 'NONE',  ( 3.682023737882786918, -9.737023737882811503, 54.00000000000000711 ) ) ;
#62658 = DIRECTION ( 'NONE',  ( 1.000000000000000000, 0.000000000000000000, 0.000000000000000000 ) ) ;
#62659 = ADVANCED_FACE ( 'NONE', ( #21254 ), #32202, .F. ) ;
#62660 = VECTOR ( 'NONE', #10752, 1000.000000000000000 ) ;
#62661 = CARTESIAN_POINT ( 'NONE',  ( -4.706725378239251967, -6.358413763958955300, 26.00000000000000711 ) ) ;
#62662 = EDGE_CURVE ( 'NONE', #65337, #64069, #31865, .T. ) ;
#62663 = LINE ( 'NONE', #68327, #58905 ) ;
#62664 = ORIENTED_EDGE ( 'NONE', *, *, #44886, .F. ) ;
#62665 = ORIENTED_EDGE ( 'NONE', *, *, #59683, .F. ) ;
#62667 = ORIENTED_EDGE ( 'NONE', *, *, #13835, .T. ) ;
#62666 = FACE_OUTER_BOUND ( 'NONE', #48424, .T. ) ;
#62668 = VERTEX_POINT ( 'NONE', #38551 ) ;
#62669 = VECTOR ( 'NONE', #60809, 1000.000000000000000 ) ;
#62670 = VECTOR ( 'NONE', #66076, 1000.000000000000000 ) ;
#62671 = LINE ( 'NONE', #40762, #38263 ) ;
#62672 = DIRECTION ( 'NONE',  ( 0.4999999999999827360, 0.000000000000000000, -0.8660254037844485886 ) ) ;
#62673 = CARTESIAN_POINT ( 'NONE',  ( 8.612468434717184707, 1.991476262117167995, 26.00000000000000711 ) ) ;
#62674 = VECTOR ( 'NONE', #31142, 1000.000000000000000 ) ;
#62675 = DIRECTION ( 'NONE',  ( -1.000000000000000000, 0.000000000000000000, -0.000000000000000000 ) ) ;
#62676 = PLANE ( 'NONE',  #8512 ) ;
#62677 = VECTOR ( 'NONE', #37063, 999.9999999999998863 ) ;
#62678 = AXIS2_PLACEMENT_3D ( 'NONE', #8230, #2937, #51735 ) ;
#62679 = CARTESIAN_POINT ( 'NONE',  ( -5.993516549646711766, 5.993516549646603409, 455.0000000000000568 ) ) ;
#62680 = ORIENTED_EDGE ( 'NONE', *, *, #62086, .F. ) ;
#62681 = VERTEX_POINT ( 'NONE', #48466 ) ;
#62682 = ORIENTED_EDGE ( 'NONE', *, *, #50020, .F. ) ;
#62683 = ADVANCED_FACE ( 'NONE', ( #64725 ), #37513, .F. ) ;
#62685 = ORIENTED_EDGE ( 'NONE', *, *, #65606, .T. ) ;
#62684 = VECTOR ( 'NONE', #14960, 1000.000000000000000 ) ;
#62686 = DIRECTION ( 'NONE',  ( -1.000000000000000000, 0.000000000000000000, 0.000000000000000000 ) ) ;
#62687 = DIRECTION ( 'NONE',  ( -1.000000000000000000, 0.000000000000000000, 0.000000000000000000 ) ) ;
#62688 = CONICAL_SURFACE ( 'NONE', #4008, 2.000000000000001776, 0.7853981633974503884 ) ;
#62689 = FACE_OUTER_BOUND ( 'NONE', #24349, .T. ) ;
#62690 = EDGE_LOOP ( 'NONE', ( #11304, #38432, #31096, #54985 ) ) ;
#62691 = ORIENTED_EDGE ( 'NONE', *, *, #43450, .T. ) ;
#62692 = ORIENTED_EDGE ( 'NONE', *, *, #65262, .F. ) ;
#62693 = VECTOR ( 'NONE', #8001, 1000.000000000000000 ) ;
#62694 = DIRECTION ( 'NONE',  ( -1.000000000000000000, 0.000000000000000000, 0.000000000000000000 ) ) ;
#62695 = EDGE_LOOP ( 'NONE', ( #62972, #34083, #7268, #52994 ) ) ;
#62696 = ORIENTED_EDGE ( 'NONE', *, *, #7658, .T. ) ;
#62697 = LINE ( 'NONE', #58474, #35606 ) ;
#62698 = VERTEX_POINT ( 'NONE', #16281 ) ;
#62699 = ORIENTED_EDGE ( 'NONE', *, *, #725, .T. ) ;
#62700 = CARTESIAN_POINT ( 'NONE',  ( 283.0000000000000568, -25.60000000000000142, -15.10000000000000142 ) ) ;
#62701 = EDGE_CURVE ( 'NONE', #38703, #10783, #41364, .T. ) ;
#62703 = ORIENTED_EDGE ( 'NONE', *, *, #62125, .T. ) ;
#62702 = DIRECTION ( 'NONE',  ( -1.000000000000000000, 0.000000000000000000, 0.000000000000000000 ) ) ;
#62704 = VERTEX_POINT ( 'NONE', #1073 ) ;
#62705 = CARTESIAN_POINT ( 'NONE',  ( 11.19368345035340973, 11.99351654964656433, 455.0000000000000568 ) ) ;
#62706 = EDGE_CURVE ( 'NONE', #11032, #19106, #64009, .T. ) ;
#62707 = LINE ( 'NONE', #57407, #16033 ) ;
#62708 = CARTESIAN_POINT ( 'NONE',  ( 1.690483450353344352, -10.74648345035336128, 195.0000000000000284 ) ) ;
#62710 = ORIENTED_EDGE ( 'NONE', *, *, #19821, .F. ) ;
#62709 = DIRECTION ( 'NONE',  ( -0.000000000000000000, -0.000000000000000000, 1.000000000000000000 ) ) ;
#62711 = ORIENTED_EDGE ( 'NONE', *, *, #30879, .F. ) ;
#62712 = PLANE ( 'NONE',  #69391 ) ;
#62713 = AXIS2_PLACEMENT_3D ( 'NONE', #11949, #5977, #54083 ) ;
#62714 = CARTESIAN_POINT ( 'NONE',  ( -15.50000000000000000, 0.000000000000000000, -22.50000000000000000 ) ) ;
#62715 = DIRECTION ( 'NONE',  ( 0.000000000000000000, 0.000000000000000000, 1.000000000000000000 ) ) ;
#62716 = DIRECTION ( 'NONE',  ( -1.000000000000000000, 0.000000000000000000, 0.000000000000000000 ) ) ;
#62717 = VECTOR ( 'NONE', #16144, 1000.000000000000000 ) ;
#62718 = ORIENTED_EDGE ( 'NONE', *, *, #30756, .F. ) ;
#62719 = CARTESIAN_POINT ( 'NONE',  ( -30.00000000000000000, -15.46862696659690073, -14.50000000000000000 ) ) ;
#62720 = AXIS2_PLACEMENT_3D ( 'NONE', #45466, #50085, #44765 ) ;
#62721 = AXIS2_PLACEMENT_3D ( 'NONE', #29673, #19076, #19423 ) ;
#62723 = CARTESIAN_POINT ( 'NONE',  ( -6.331612867284154511, 8.393516549646601987, 455.0000000000000568 ) ) ;
#62722 = VECTOR ( 'NONE', #41833, 1000.000000000000000 ) ;
#62724 = LINE ( 'NONE', #58127, #54909 ) ;
#62725 = ORIENTED_EDGE ( 'NONE', *, *, #22037, .T. ) ;
#62726 = DIRECTION ( 'NONE',  ( -1.836970198721029934E-16, -1.836970198721010706E-16, 1.000000000000000000 ) ) ;
#62727 = CARTESIAN_POINT ( 'NONE',  ( 277.1811023147819810, -25.34729925119250282, 17.15270074880750428 ) ) ;
#62728 = CIRCLE ( 'NONE', #27764, 24.99999999998784972 ) ;
#62729 = AXIS2_PLACEMENT_3D ( 'NONE', #38607, #33298, #33641 ) ;
#62730 = LINE ( 'NONE', #14650, #63050 ) ;
#62731 = ORIENTED_EDGE ( 'NONE', *, *, #16847, .F. ) ;
#62732 = VECTOR ( 'NONE', #58281, 1000.000000000000000 ) ;
#62733 = DIRECTION ( 'NONE',  ( 1.000000000000000000, -3.491481338843133355E-15, 0.000000000000000000 ) ) ;
#62734 = FACE_OUTER_BOUND ( 'NONE', #68954, .T. ) ;
#62735 = EDGE_CURVE ( 'NONE', #64072, #41205, #51571, .T. ) ;
#62736 = VECTOR ( 'NONE', #21534, 1000.000000000000114 ) ;
#62737 = FACE_OUTER_BOUND ( 'NONE', #48270, .T. ) ;
#62738 = ORIENTED_EDGE ( 'NONE', *, *, #55795, .T. ) ;
#62739 = CARTESIAN_POINT ( 'NONE',  ( 8.900000000000005684, -14.06939075806901940, -20.80000000000000426 ) ) ;
#62740 = CARTESIAN_POINT ( 'NONE',  ( -15.50000000000000000, -2.500000000000000000, -23.94337567297399971 ) ) ;
#62741 = CARTESIAN_POINT ( 'NONE',  ( 9.417013320880792904, -1.866219381641466279, 195.0000000000000284 ) ) ;
#62742 = AXIS2_PLACEMENT_3D ( 'NONE', #42477, #68302, #19853 ) ;
#62743 = EDGE_CURVE ( 'NONE', #58530, #54344, #48204, .T. ) ;
#62744 = CARTESIAN_POINT ( 'NONE',  ( -14.25000000000000000, -0.2038245569916330158, 23.22168783648699986 ) ) ;
#62745 = DIRECTION ( 'NONE',  ( 0.6414496315691494699, -0.7671651518153064231, 0.000000000000000000 ) ) ;
#62746 = ORIENTED_EDGE ( 'NONE', *, *, #43622, .T. ) ;
#62747 = DIRECTION ( 'NONE',  ( 0.000000000000000000, -1.000000000000000000, -2.854859206170826497E-12 ) ) ;
#62748 = CYLINDRICAL_SURFACE ( 'NONE', #59895, 0.8128000000000145109 ) ;
#62749 = EDGE_CURVE ( 'NONE', #46404, #34424, #732, .T. ) ;
#62750 = EDGE_CURVE ( 'NONE', #47619, #12122, #4137, .T. ) ;
#62751 = DIRECTION ( 'NONE',  ( 0.000000000000000000, -1.000000000000000000, 0.000000000000000000 ) ) ;
#62752 = CARTESIAN_POINT ( 'NONE',  ( -11.00000000000000000, -9.199999999999999289, -12.69999999999986073 ) ) ;
#62753 = ADVANCED_FACE ( 'NONE', ( #12686 ), #50183, .T. ) ;
#62754 = DIRECTION ( 'NONE',  ( 0.000000000000000000, 0.000000000000000000, 1.000000000000000000 ) ) ;
#62755 = ADVANCED_FACE ( 'NONE', ( #61127 ), #55503, .T. ) ;
#62756 = VERTEX_POINT ( 'NONE', #34613 ) ;
#62758 = ORIENTED_EDGE ( 'NONE', *, *, #15839, .F. ) ;
#62757 = DIRECTION ( 'NONE',  ( 0.000000000000000000, 1.000000000000000000, 0.000000000000000000 ) ) ;
#62759 = EDGE_CURVE ( 'NONE', #5045, #21232, #35762, .T. ) ;
#62760 = CARTESIAN_POINT ( 'NONE',  ( -13.00000000000000178, -15.50000000000000000, -20.05051025721700242 ) ) ;
#62761 = CARTESIAN_POINT ( 'NONE',  ( -3.593516549646712299, 4.609516549646604844, 455.0000000000000568 ) ) ;
#62762 = CARTESIAN_POINT ( 'NONE',  ( 8.900000000000002132, 18.00000000000000355, -21.00000000000000000 ) ) ;
#62763 = ORIENTED_EDGE ( 'NONE', *, *, #28447, .F. ) ;
#62764 = CIRCLE ( 'NONE', #37950, 0.1749999999999998224 ) ;
#62765 = DIRECTION ( 'NONE',  ( 0.000000000000000000, 0.000000000000000000, 1.000000000000000000 ) ) ;
#62766 = VECTOR ( 'NONE', #63471, 1000.000000000000000 ) ;
#62767 = VERTEX_POINT ( 'NONE', #12337 ) ;
#62768 = AXIS2_PLACEMENT_3D ( 'NONE', #59967, #38745, #65295 ) ;
#62769 = ORIENTED_EDGE ( 'NONE', *, *, #68677, .F. ) ;
#62770 = EDGE_LOOP ( 'NONE', ( #39541, #58794, #31185, #18773 ) ) ;
#62771 = CARTESIAN_POINT ( 'NONE',  ( 7.826483450353380000, -11.78648345035349010, 455.0000000000000568 ) ) ;
#62772 = FACE_OUTER_BOUND ( 'NONE', #50146, .T. ) ;
#62773 = DIRECTION ( 'NONE',  ( 1.000000000000000000, -0.000000000000000000, 0.000000000000000000 ) ) ;
#62774 = DIRECTION ( 'NONE',  ( -0.000000000000000000, 0.000000000000000000, -1.000000000000000000 ) ) ;
#62775 = AXIS2_PLACEMENT_3D ( 'NONE', #59846, #54559, #27672 ) ;
#62776 = CIRCLE ( 'NONE', #53766, 1.399999999999999245 ) ;
#62777 = AXIS2_PLACEMENT_3D ( 'NONE', #68634, #41045, #46701 ) ;
#62778 = ORIENTED_EDGE ( 'NONE', *, *, #60550, .F. ) ;
#62779 = VERTEX_POINT ( 'NONE', #66451 ) ;
#62780 = CARTESIAN_POINT ( 'NONE',  ( -23.75054448485400016, -17.50000000000000000, 25.53140320652400064 ) ) ;
#62781 = CARTESIAN_POINT ( 'NONE',  ( 7.000000000000000000, -21.00000000000000000, -12.50000000000000000 ) ) ;
#62782 = AXIS2_PLACEMENT_3D ( 'NONE', #35487, #56366, #2278 ) ;
#62783 = VECTOR ( 'NONE', #28488, 1000.000000000000000 ) ;
#62784 = VERTEX_POINT ( 'NONE', #12000 ) ;
#62785 = ORIENTED_EDGE ( 'NONE', *, *, #7320, .T. ) ;
#62786 = VERTEX_POINT ( 'NONE', #67511 ) ;
#62787 = ORIENTED_EDGE ( 'NONE', *, *, #16000, .F. ) ;
#62788 = AXIS2_PLACEMENT_3D ( 'NONE', #11479, #54290, #21758 ) ;
#62789 = CYLINDRICAL_SURFACE ( 'NONE', #40643, 4.000000000000000000 ) ;
#62790 = UNCERTAINTY_MEASURE_WITH_UNIT (LENGTH_MEASURE( 1.000000000000000082E-05 ), #54529, 'distance_accuracy_value', 'NONE');
#62792 = VERTEX_POINT ( 'NONE', #56193 ) ;
#62791 = DIRECTION ( 'NONE',  ( 1.000000000000000000, 0.000000000000000000, 0.000000000000000000 ) ) ;
#62793 = LINE ( 'NONE', #51489, #25507 ) ;
#62794 = PRODUCT ( 'Stepper Motor', 'Stepper Motor', '', ( #56857 ) ) ;
#62795 = ADVANCED_FACE ( 'NONE', ( #6701 ), #50539, .F. ) ;
#62796 = VECTOR ( 'NONE', #69070, 1000.000000000000000 ) ;
#62797 = DIRECTION ( 'NONE',  ( 1.000000000000000000, 3.016910393003147986E-15, 0.000000000000000000 ) ) ;
#62798 = ORIENTED_EDGE ( 'NONE', *, *, #19737, .T. ) ;
#62799 = EDGE_CURVE ( 'NONE', #11956, #2551, #23351, .T. ) ;
#62800 = STYLED_ITEM ( 'NONE', ( #45148 ), #44073 ) ;
#62801 = ORIENTED_EDGE ( 'NONE', *, *, #29321, .F. ) ;
#62802 = ADVANCED_FACE ( 'NONE', ( #28616 ), #28273, .F. ) ;
#62803 = EDGE_CURVE ( 'NONE', #49333, #27966, #7738, .T. ) ;
#62804 = LINE ( 'NONE', #35568, #12047 ) ;
#62805 = DIRECTION ( 'NONE',  ( -1.000000000000000000, 0.000000000000000000, 0.000000000000000000 ) ) ;
#62806 = CARTESIAN_POINT ( 'NONE',  ( -7.250000000000001776, -7.249999999999998224, -26.00000000000001066 ) ) ;
#62807 = FACE_OUTER_BOUND ( 'NONE', #22159, .T. ) ;
#62808 = AXIS2_PLACEMENT_3D ( 'NONE', #66977, #56374, #7923 ) ;
#62809 = CARTESIAN_POINT ( 'NONE',  ( 11.78648345035340661, 7.593516549646560421, 455.0000000000000568 ) ) ;
#62810 = VERTEX_POINT ( 'NONE', #1744 ) ;
#62811 = DIRECTION ( 'NONE',  ( 1.000000000000000000, 0.000000000000000000, 0.000000000000000000 ) ) ;
#62812 = LINE ( 'NONE', #13322, #22271 ) ;
#62813 = DIRECTION ( 'NONE',  ( 0.000000000000000000, -0.7071067811865474617, -0.7071067811865474617 ) ) ;
#62814 = AXIS2_PLACEMENT_3D ( 'NONE', #2233, #40416, #51023 ) ;
#62815 = DIRECTION ( 'NONE',  ( -1.836970198721029934E-16, 1.836970198721036590E-16, -1.000000000000000000 ) ) ;
#62816 = VECTOR ( 'NONE', #64859, 1000.000000000000000 ) ;
#62817 = AXIS2_PLACEMENT_3D ( 'NONE', #1480, #17755, #23050 ) ;
#62818 = CARTESIAN_POINT ( 'NONE',  ( -6.500000000000002665, 6.500000000000002665, 0.000000000000000000 ) ) ;
#62819 = EDGE_LOOP ( 'NONE', ( #6859, #27460, #10978, #65100 ) ) ;
#62820 = CARTESIAN_POINT ( 'NONE',  ( -3.650476262117221093, 10.49297626211717116, 26.00000000000000711 ) ) ;
#62821 = DIRECTION ( 'NONE',  ( -1.000000000000000000, 0.000000000000000000, 0.000000000000000000 ) ) ;
#62822 = SURFACE_STYLE_FILL_AREA ( #20390 ) ;
#62823 = DIRECTION ( 'NONE',  ( -0.000000000000000000, -0.000000000000000000, -1.000000000000000000 ) ) ;
#62824 = VECTOR ( 'NONE', #56280, 1000.000000000000000 ) ;
#62825 = AXIS2_PLACEMENT_3D ( 'NONE', #38245, #43525, #27617 ) ;
#62826 = ADVANCED_FACE ( 'NONE', ( #1403 ), #50875, .F. ) ;
#62827 = CIRCLE ( 'NONE', #56014, 0.3499999999999996447 ) ;
#62828 = DIRECTION ( 'NONE',  ( 1.000000000000000000, 0.000000000000000000, 0.000000000000000000 ) ) ;
#62829 = DIRECTION ( 'NONE',  ( 0.000000000000000000, 3.673940397442059868E-16, -1.000000000000000000 ) ) ;
#62830 = DIRECTION ( 'NONE',  ( -1.000000000000000000, 0.000000000000000000, 0.000000000000000000 ) ) ;
#62831 = CIRCLE ( 'NONE', #15406, 0.1749999999999993783 ) ;
#62832 = DIRECTION ( 'NONE',  ( -0.000000000000000000, -0.000000000000000000, -1.000000000000000000 ) ) ;
#62833 = ORIENTED_EDGE ( 'NONE', *, *, #6803, .F. ) ;
#62834 = CYLINDRICAL_SURFACE ( 'NONE', #18551, 0.2000000000000005107 ) ;
#62835 = CARTESIAN_POINT ( 'NONE',  ( -11.00000000000000000, -14.33999999999999986, 14.50000000000000000 ) ) ;
#62836 = VERTEX_POINT ( 'NONE', #40274 ) ;
#62837 = CYLINDRICAL_SURFACE ( 'NONE', #54941, 4.500000000000189182 ) ;
#62838 = PLANE ( 'NONE',  #52593 ) ;
#62839 = CIRCLE ( 'NONE', #35734, 4.000000000000000000 ) ;
#62840 = CARTESIAN_POINT ( 'NONE',  ( 8.406483450353404052, 6.331612867284015955, 455.0000000000000568 ) ) ;
#62841 = EDGE_CURVE ( 'NONE', #44065, #34045, #66096, .T. ) ;
#62842 = DIRECTION ( 'NONE',  ( 1.000000000000000000, -0.000000000000000000, 0.000000000000000000 ) ) ;
#62843 = EDGE_CURVE ( 'NONE', #54850, #59438, #2443, .T. ) ;
#62844 = VERTEX_POINT ( 'NONE', #55839 ) ;
#62845 = DIRECTION ( 'NONE',  ( 0.000000000000000000, 0.000000000000000000, 1.000000000000000000 ) ) ;
#62846 = AXIS2_PLACEMENT_3D ( 'NONE', #4993, #42471, #37183 ) ;
#62847 = ORIENTED_EDGE ( 'NONE', *, *, #69164, .T. ) ;
#62848 = EDGE_CURVE ( 'NONE', #4531, #60100, #28967, .T. ) ;
#62849 = DIRECTION ( 'NONE',  ( -1.000000000000000000, 0.000000000000000000, 0.000000000000000000 ) ) ;
#62850 = CARTESIAN_POINT ( 'NONE',  ( -14.66434062215825840, -0.3156604612126666654, 23.46090750622624910 ) ) ;
#62851 = EDGE_LOOP ( 'NONE', ( #27622, #6058, #31401, #61691 ) ) ;
#62852 = DIRECTION ( 'NONE',  ( -1.000000000000000000, 0.000000000000000000, 0.000000000000000000 ) ) ;
#62853 = DIRECTION ( 'NONE',  ( 3.491481338843133355E-15, 1.000000000000000000, 1.836970198721029934E-16 ) ) ;
#62854 = ORIENTED_EDGE ( 'NONE', *, *, #40719, .T. ) ;
#62855 = CYLINDRICAL_SURFACE ( 'NONE', #18710, 1.224999999999999423 ) ;
#62856 = ORIENTED_EDGE ( 'NONE', *, *, #32900, .T. ) ;
#62857 = ORIENTED_EDGE ( 'NONE', *, *, #9457, .F. ) ;
#62858 = CARTESIAN_POINT ( 'NONE',  ( 7.186223737882800222, 5.242976262117193365, 54.00000000000000711 ) ) ;
#62859 = EDGE_LOOP ( 'NONE', ( #62158, #6526, #47163, #39469 ) ) ;
#62860 = VERTEX_POINT ( 'NONE', #66787 ) ;
#62861 = LINE ( 'NONE', #9830, #13554 ) ;
#62862 = CARTESIAN_POINT ( 'NONE',  ( 39.00000000000000000, 0.000000000000000000, 0.000000000000000000 ) ) ;
#62863 = CYLINDRICAL_SURFACE ( 'NONE', #41180, 0.5999999999999998668 ) ;
#62864 = CIRCLE ( 'NONE', #64003, 1.399999999999999245 ) ;
#62865 = VERTEX_POINT ( 'NONE', #18341 ) ;
#62866 = CARTESIAN_POINT ( 'NONE',  ( 18.89999999999999858, -0.2000000000089119934, -8.913009219568841313E-12 ) ) ;
#62868 = PLANE ( 'NONE',  #3996 ) ;
#62867 = DIRECTION ( 'NONE',  ( 0.000000000000000000, -0.7096009616570518874, 0.7046037717862339012 ) ) ;
#62869 = ORIENTED_EDGE ( 'NONE', *, *, #64102, .T. ) ;
#62871 = ORIENTED_EDGE ( 'NONE', *, *, #53675, .T. ) ;
#62870 = LINE ( 'NONE', #29990, #15034 ) ;
#62872 = CIRCLE ( 'NONE', #68536, 24.99999999998784972 ) ;
#62873 = VERTEX_POINT ( 'NONE', #39909 ) ;
#62874 = AXIS2_PLACEMENT_3D ( 'NONE', #45230, #60805, #66803 ) ;
#62875 = VECTOR ( 'NONE', #13748, 1000.000000000000000 ) ;
#62876 = CARTESIAN_POINT ( 'NONE',  ( 8.465062094116026614, 4.242044687070459119, 195.0000000000000284 ) ) ;
#62878 = VERTEX_POINT ( 'NONE', #45567 ) ;
#62877 = DIRECTION ( 'NONE',  ( 0.000000000000000000, -0.7071067811865077157, 0.7071067811865873187 ) ) ;
#62879 = CIRCLE ( 'NONE', #38067, 0.5999999999999998668 ) ;
#62880 = AXIS2_PLACEMENT_3D ( 'NONE', #18691, #56185, #27927 ) ;
#62881 = CARTESIAN_POINT ( 'NONE',  ( -11.50000000000000000, -15.46862696659690073, -14.50000000000000000 ) ) ;
#62882 = CARTESIAN_POINT ( 'NONE',  ( 275.5000000000000000, -42.50000000000000000, -15.10000000000000142 ) ) ;
#62883 = VERTEX_POINT ( 'NONE', #67144 ) ;
#62884 = ORIENTED_EDGE ( 'NONE', *, *, #7886, .F. ) ;
#62885 = ADVANCED_FACE ( 'NONE', ( #18702 ), #61847, .F. ) ;
#62886 = ADVANCED_FACE ( 'NONE', ( #8085 ), #3502, .F. ) ;
#62887 = EDGE_CURVE ( 'NONE', #40074, #40825, #35297, .T. ) ;
#62888 = AXIS2_PLACEMENT_3D ( 'NONE', #24286, #44531, #14382 ) ;
#62889 = AXIS2_PLACEMENT_3D ( 'NONE', #14438, #20084, #3476 ) ;
#62890 = LINE ( 'NONE', #8074, #28951 ) ;
#62891 = ORIENTED_EDGE ( 'NONE', *, *, #31245, .F. ) ;
#62892 = ADVANCED_FACE ( 'NONE', ( #31072 ), #20461, .F. ) ;
#62893 = CARTESIAN_POINT ( 'NONE',  ( -14.66242688423474227, -0.3152598339554795182, -23.45980260912095616 ) ) ;
#62895 = DIRECTION ( 'NONE',  ( -1.836970198721029934E-16, -1.836970198721010706E-16, 1.000000000000000000 ) ) ;
#62894 = VECTOR ( 'NONE', #16196, 1000.000000000000000 ) ;
#62896 = DIRECTION ( 'NONE',  ( 0.7671651518152998728, -0.6414496315691575745, 2.309356642088859447E-17 ) ) ;
#62897 = ORIENTED_EDGE ( 'NONE', *, *, #3274, .T. ) ;
#62898 = AXIS2_PLACEMENT_3D ( 'NONE', #16567, #66017, #33507 ) ;
#62899 = CARTESIAN_POINT ( 'NONE',  ( 29.50000000000000355, -12.00000000000000000, -10.52786404500095863 ) ) ;
#62900 = DIRECTION ( 'NONE',  ( -1.000000000000000000, 0.000000000000000000, 0.000000000000000000 ) ) ;
#62902 = VERTEX_POINT ( 'NONE', #41671 ) ;
#62901 = DIRECTION ( 'NONE',  ( -1.000000000000000000, 0.000000000000000000, 0.000000000000000000 ) ) ;
#62904 = ORIENTED_EDGE ( 'NONE', *, *, #35168, .T. ) ;
#62903 = DIRECTION ( 'NONE',  ( 1.000000000000000000, 0.000000000000000000, 0.000000000000000000 ) ) ;
#62905 = DIRECTION ( 'NONE',  ( 0.000000000000000000, -1.000000000000000000, 0.000000000000000000 ) ) ;
#62906 = FACE_OUTER_BOUND ( 'NONE', #20282, .T. ) ;
#62907 = DIRECTION ( 'NONE',  ( 1.060575238724892987E-16, 0.5000000000000199840, -0.8660254037844271613 ) ) ;
#62908 = DIRECTION ( 'NONE',  ( 0.000000000000000000, -0.000000000000000000, 1.000000000000000000 ) ) ;
#62909 = EDGE_CURVE ( 'NONE', #51206, #4508, #56102, .T. ) ;
#62910 = FACE_OUTER_BOUND ( 'NONE', #48526, .T. ) ;
#62911 = ORIENTED_EDGE ( 'NONE', *, *, #9425, .T. ) ;
#62912 = LINE ( 'NONE', #19757, #10941 ) ;
#62913 = LINE ( 'NONE', #36033, #37259 ) ;
#62914 = DIRECTION ( 'NONE',  ( -1.000000000000000000, 0.000000000000000000, 0.000000000000000000 ) ) ;
#62916 = VERTEX_POINT ( 'NONE', #35658 ) ;
#62915 = CARTESIAN_POINT ( 'NONE',  ( 157.4206970127263787, -35.25383818724483831, 5.000000000000000000 ) ) ;
#62917 = CARTESIAN_POINT ( 'NONE',  ( 8.250000000000005329, -7.249999999999998224, -26.00000000000001066 ) ) ;
#62918 = CIRCLE ( 'NONE', #33582, 0.5249999999999990230 ) ;
#62919 = DIRECTION ( 'NONE',  ( 0.000000000000000000, 0.000000000000000000, 1.000000000000000000 ) ) ;
#62920 = ORIENTED_EDGE ( 'NONE', *, *, #38536, .T. ) ;
#62921 = CYLINDRICAL_SURFACE ( 'NONE', #37705, 1.000000000000000000 ) ;
#62922 = LINE ( 'NONE', #35685, #53214 ) ;
#62923 = ORIENTED_EDGE ( 'NONE', *, *, #7721, .T. ) ;
#62924 = DIRECTION ( 'NONE',  ( -0.000000000000000000, -0.000000000000000000, -1.000000000000000000 ) ) ;
#62925 = AXIS2_PLACEMENT_3D ( 'NONE', #10196, #36012, #32113 ) ;
#62926 = VECTOR ( 'NONE', #63169, 1000.000000000000000 ) ;
#62927 = VECTOR ( 'NONE', #40377, 1000.000000000000000 ) ;
#62928 = DIRECTION ( 'NONE',  ( -0.000000000000000000, 1.000000000000000000, -0.000000000000000000 ) ) ;
#62929 = DIRECTION ( 'NONE',  ( 0.000000000000000000, 0.000000000000000000, 1.000000000000000000 ) ) ;
#62930 = EDGE_CURVE ( 'NONE', #58887, #32678, #8804, .T. ) ;
#62931 = AXIS2_PLACEMENT_3D ( 'NONE', #31638, #32329, #53215 ) ;
#62933 = CARTESIAN_POINT ( 'NONE',  ( -14.25000000000000000, -2.500000000000000000, -21.77831216351300014 ) ) ;
#62932 = CIRCLE ( 'NONE', #41484, 1.000000000000000000 ) ;
#62934 = VERTEX_POINT ( 'NONE', #14463 ) ;
#62935 = EDGE_CURVE ( 'NONE', #62681, #3213, #68560, .T. ) ;
#62936 = DIRECTION ( 'NONE',  ( -0.000000000000000000, 0.000000000000000000, -1.000000000000000000 ) ) ;
#62937 = ORIENTED_EDGE ( 'NONE', *, *, #22335, .F. ) ;
#62938 = ORIENTED_EDGE ( 'NONE', *, *, #13359, .T. ) ;
#62939 = EDGE_CURVE ( 'NONE', #55991, #21614, #57588, .T. ) ;
#62940 = VERTEX_POINT ( 'NONE', #67849 ) ;
#62941 = PLANE ( 'NONE',  #31404 ) ;
#62942 = AXIS2_PLACEMENT_3D ( 'NONE', #44359, #65932, #59943 ) ;
#62943 = CIRCLE ( 'NONE', #25657, 0.1749999999999989342 ) ;
#62944 = EDGE_CURVE ( 'NONE', #44953, #35986, #52653, .T. ) ;
#62945 = DIRECTION ( 'NONE',  ( 0.000000000000000000, 0.000000000000000000, -1.000000000000000000 ) ) ;
#62946 = EDGE_CURVE ( 'NONE', #43516, #31751, #31441, .T. ) ;
#62947 = DIRECTION ( 'NONE',  ( 0.000000000000000000, 0.000000000000000000, -1.000000000000000000 ) ) ;
#62948 = VERTEX_POINT ( 'NONE', #25416 ) ;
#62949 = EDGE_CURVE ( 'NONE', #55252, #48042, #53867, .T. ) ;
#62950 = ORIENTED_EDGE ( 'NONE', *, *, #19846, .F. ) ;
#62951 = DIRECTION ( 'NONE',  ( 0.000000000000000000, 3.673940397442059868E-16, -1.000000000000000000 ) ) ;
#62953 = ORIENTED_EDGE ( 'NONE', *, *, #13399, .T. ) ;
#62952 = EDGE_CURVE ( 'NONE', #26808, #18477, #22253, .T. ) ;
#62954 = ORIENTED_EDGE ( 'NONE', *, *, #3308, .T. ) ;
#62955 = VECTOR ( 'NONE', #42729, 1000.000000000000000 ) ;
#62956 = LINE ( 'NONE', #64020, #60885 ) ;
#62957 = DIRECTION ( 'NONE',  ( 0.000000000000000000, 0.000000000000000000, -1.000000000000000000 ) ) ;
#62958 = CARTESIAN_POINT ( 'NONE',  ( -5.993516549646799696, -8.211283450353425550, 455.0000000000000568 ) ) ;
#62959 = DIRECTION ( 'NONE',  ( 0.000000000000000000, 0.000000000000000000, -1.000000000000000000 ) ) ;
#62960 = ORIENTED_EDGE ( 'NONE', *, *, #32290, .T. ) ;
#62961 = DIRECTION ( 'NONE',  ( 0.000000000000000000, 0.000000000000000000, 1.000000000000000000 ) ) ;
#62963 = CARTESIAN_POINT ( 'NONE',  ( -7.342976262117259623, 5.538810540049946773, 54.00000000000000711 ) ) ;
#62962 = CARTESIAN_POINT ( 'NONE',  ( 176.4833316329832940, 9.000000000000001776, 282.8454385697650082 ) ) ;
#62964 = ORIENTED_EDGE ( 'NONE', *, *, #22874, .T. ) ;
#62966 = ORIENTED_EDGE ( 'NONE', *, *, #36187, .F. ) ;
#62965 = DIRECTION ( 'NONE',  ( 0.000000000000000000, 0.000000000000000000, 1.000000000000000000 ) ) ;
#62967 = ORIENTED_EDGE ( 'NONE', *, *, #26898, .T. ) ;
#62968 = DIRECTION ( 'NONE',  ( -1.000000000000000000, 0.000000000000000000, 0.000000000000000000 ) ) ;
#62969 = CARTESIAN_POINT ( 'NONE',  ( -17.51999999999999957, -15.50000000000000000, -26.00000000000000355 ) ) ;
#62970 = VERTEX_POINT ( 'NONE', #40965 ) ;
#62971 = VECTOR ( 'NONE', #36940, 1000.000000000000000 ) ;
#62972 = ORIENTED_EDGE ( 'NONE', *, *, #59982, .T. ) ;
#62973 = DIRECTION ( 'NONE',  ( -1.000000000000000000, 0.000000000000000000, 0.000000000000000000 ) ) ;
#62974 = FACE_OUTER_BOUND ( 'NONE', #63287, .T. ) ;
#62975 = ORIENTED_EDGE ( 'NONE', *, *, #63997, .F. ) ;
#62976 = ORIENTED_EDGE ( 'NONE', *, *, #35706, .F. ) ;
#62977 = CIRCLE ( 'NONE', #11045, 0.1999999999999987899 ) ;
#62978 = DIRECTION ( 'NONE',  ( 1.000000000000000000, 0.000000000000000000, 0.000000000000000000 ) ) ;
#62979 = CYLINDRICAL_SURFACE ( 'NONE', #14720, 0.1999999999999996503 ) ;
#62980 = EDGE_LOOP ( 'NONE', ( #4048, #28633 ) ) ;
#62981 = VECTOR ( 'NONE', #35000, 1000.000000000000000 ) ;
#62982 = AXIS2_PLACEMENT_3D ( 'NONE', #69424, #68374, #31268 ) ;
#62983 = CARTESIAN_POINT ( 'NONE',  ( -15.50000000000000000, -0.1999999999999999556, -21.05000000000000071 ) ) ;
#62984 = DIRECTION ( 'NONE',  ( 0.000000000000000000, -1.000000000000000000, 0.000000000000000000 ) ) ;
#62985 = AXIS2_PLACEMENT_3D ( 'NONE', #33587, #6380, #66104 ) ;
#62987 = VERTEX_POINT ( 'NONE', #19400 ) ;
#62986 = DIRECTION ( 'NONE',  ( 2.135044278125301343E-15, -1.000000000000000000, -3.673940397442059868E-16 ) ) ;
#62988 = EDGE_LOOP ( 'NONE', ( #69009, #15066, #36042, #57302 ) ) ;
#62989 = DIRECTION ( 'NONE',  ( 0.000000000000000000, 0.000000000000000000, 1.000000000000000000 ) ) ;
#62990 = AXIS2_PLACEMENT_3D ( 'NONE', #17542, #39118, #54698 ) ;
#62991 = ADVANCED_FACE ( 'NONE', ( #36368 ), #4561, .F. ) ;
#62992 = DIRECTION ( 'NONE',  ( 1.836970198721029934E-16, 1.836970198721010706E-16, -1.000000000000000000 ) ) ;
#62993 = CARTESIAN_POINT ( 'NONE',  ( 17.89999999999999858, -0.2000000000089119934, -8.913009219568841313E-12 ) ) ;
#62994 = DIRECTION ( 'NONE',  ( 0.000000000000000000, 0.000000000000000000, -1.000000000000000000 ) ) ;
#62995 = CARTESIAN_POINT ( 'NONE',  ( -4.135079735113215804, -6.836383711243002814, 54.00000000000000711 ) ) ;
#62996 = EDGE_CURVE ( 'NONE', #13374, #5297, #51942, .T. ) ;
#62997 = CARTESIAN_POINT ( 'NONE',  ( -8.750000000000001776, -7.249999999999998224, -30.00000000000001066 ) ) ;
#62998 = ORIENTED_EDGE ( 'NONE', *, *, #22736, .F. ) ;
#62999 = LINE ( 'NONE', #51697, #16853 ) ;
#63000 = ADVANCED_BREP_SHAPE_REPRESENTATION ( '', ( #20823, #45918 ), #34756 ) ;
#63002 = VERTEX_POINT ( 'NONE', #47682 ) ;
#63001 = DIRECTION ( 'NONE',  ( 0.000000000000000000, 0.000000000000000000, 1.000000000000000000 ) ) ;
#63003 = VECTOR ( 'NONE', #68825, 1000.000000000000000 ) ;
#63004 = DIRECTION ( 'NONE',  ( 0.000000000000000000, 0.000000000000000000, -1.000000000000000000 ) ) ;
#63005 = CARTESIAN_POINT ( 'NONE',  ( 7.450000000000006395, 7.250000000000000888, -8.500000000000000000 ) ) ;
#63006 = EDGE_CURVE ( 'NONE', #16172, #33489, #30013, .T. ) ;
#63007 = CARTESIAN_POINT ( 'NONE',  ( 11.00000000000000000, -12.00000000000000000, 10.52786404500095863 ) ) ;
#63008 = ORIENTED_EDGE ( 'NONE', *, *, #26940, .F. ) ;
#63009 = LINE ( 'NONE', #63717, #68128 ) ;
#63010 = FACE_OUTER_BOUND ( 'NONE', #50603, .T. ) ;
#63011 = EDGE_CURVE ( 'NONE', #58411, #16445, #15166, .T. ) ;
#63012 = ORIENTED_EDGE ( 'NONE', *, *, #52574, .F. ) ;
#63013 = CARTESIAN_POINT ( 'NONE',  ( 276.8000000000000682, -53.81370849898476649, 17.60000000000000142 ) ) ;
#63014 = PLANE ( 'NONE',  #2034 ) ;
#63015 = CARTESIAN_POINT ( 'NONE',  ( -4.135079735113167843, 6.822336235477362010, 26.00000000000000711 ) ) ;
#63016 = ORIENTED_EDGE ( 'NONE', *, *, #28183, .T. ) ;
#63017 = EDGE_CURVE ( 'NONE', #9842, #42028, #36729, .T. ) ;
#63018 = DIRECTION ( 'NONE',  ( 1.047444401652940007E-14, 1.000000000000000000, 1.836970198721029934E-16 ) ) ;
#63019 = VERTEX_POINT ( 'NONE', #69249 ) ;
#63020 = AXIS2_PLACEMENT_3D ( 'NONE', #43527, #16318, #27288 ) ;
#63021 = EDGE_LOOP ( 'NONE', ( #59559, #56122, #65244, #35753 ) ) ;
#63022 = LINE ( 'NONE', #9631, #56212 ) ;
#63023 = DIRECTION ( 'NONE',  ( -1.000000000000000000, 0.000000000000000000, 0.000000000000000000 ) ) ;
#63024 = DIRECTION ( 'NONE',  ( -0.8660254037844482555, 0.000000000000000000, -0.4999999999999831801 ) ) ;
#63025 = CARTESIAN_POINT ( 'NONE',  ( 27.90000000000000213, -0.1999999999911795112, 8.826273045769999343E-12 ) ) ;
#63026 = LINE ( 'NONE', #14582, #41934 ) ;
#63027 = VERTEX_POINT ( 'NONE', #40622 ) ;
#63028 = EDGE_CURVE ( 'NONE', #68712, #9129, #62181, .T. ) ;
#63029 = ORIENTED_EDGE ( 'NONE', *, *, #69566, .T. ) ;
#63031 = ORIENTED_EDGE ( 'NONE', *, *, #9447, .T. ) ;
#63030 = FACE_BOUND ( 'NONE', #16347, .T. ) ;
#63033 = ORIENTED_EDGE ( 'NONE', *, *, #23734, .T. ) ;
#63032 = EDGE_CURVE ( 'NONE', #21463, #55205, #32804, .T. ) ;
#63034 = VECTOR ( 'NONE', #5980, 1000.000000000000000 ) ;
#63035 = CARTESIAN_POINT ( 'NONE',  ( -11.00000000000000000, -11.50000000000100009, -15.00000000000084910 ) ) ;
#63036 = CARTESIAN_POINT ( 'NONE',  ( -3.663616288757055806, 6.350872789121238426, 26.00000000000000711 ) ) ;
#63037 = CARTESIAN_POINT ( 'NONE',  ( 7.250000000000005329, 7.250000000000000888, -24.50000000000000000 ) ) ;
#63038 = CARTESIAN_POINT ( 'NONE',  ( 0.000000000000000000, 0.000000000000000000, -7.500000000000000000 ) ) ;
#63039 = VECTOR ( 'NONE', #39217, 1000.000000000000000 ) ;
#63040 = CARTESIAN_POINT ( 'NONE',  ( -11.11351654964670743, 2.893516549646604208, 455.0000000000000568 ) ) ;
#63041 = DIRECTION ( 'NONE',  ( 1.000000000000000000, 0.000000000000000000, 0.000000000000000000 ) ) ;
#63042 = ORIENTED_EDGE ( 'NONE', *, *, #35934, .T. ) ;
#63043 = EDGE_CURVE ( 'NONE', #24327, #52649, #58649, .T. ) ;
#63044 = EDGE_LOOP ( 'NONE', ( #43983, #65878, #19736, #18866, #59137, #25394, #29340, #3291, #64163, #67300, #20242 ) ) ;
#63045 = VERTEX_POINT ( 'NONE', #63957 ) ;
#63046 = EDGE_LOOP ( 'NONE', ( #41727, #30611, #27867, #63849 ) ) ;
#63047 = FACE_OUTER_BOUND ( 'NONE', #56363, .T. ) ;
#63048 = CARTESIAN_POINT ( 'NONE',  ( -2.752095193409373586, 9.942044687070435316, 195.0000000000000284 ) ) ;
#63049 = DIRECTION ( 'NONE',  ( 0.000000000000000000, 0.000000000000000000, 1.000000000000000000 ) ) ;
#63050 = VECTOR ( 'NONE', #20645, 1000.000000000000000 ) ;
#63051 = CARTESIAN_POINT ( 'NONE',  ( -8.689999999999999503, -9.750000000000001776, -5.000000000000000000 ) ) ;
#63052 = ORIENTED_EDGE ( 'NONE', *, *, #27329, .F. ) ;
#63053 = ORIENTED_EDGE ( 'NONE', *, *, #18681, .F. ) ;
#63054 = ORIENTED_EDGE ( 'NONE', *, *, #47589, .T. ) ;
#63055 = CARTESIAN_POINT ( 'NONE',  ( -25.50000000000000355, -15.50000000000000000, -24.50000000000000000 ) ) ;
#63056 = ORIENTED_EDGE ( 'NONE', *, *, #47627, .T. ) ;
#63057 = EDGE_LOOP ( 'NONE', ( #22972, #39544, #50369, #59487 ) ) ;
#63058 = DIRECTION ( 'NONE',  ( 0.000000000000000000, 0.000000000000000000, 1.000000000000000000 ) ) ;
#63059 = VERTEX_POINT ( 'NONE', #37429 ) ;
#63060 = ADVANCED_FACE ( 'NONE', ( #37087 ), #64636, .F. ) ;
#63061 = EDGE_LOOP ( 'NONE', ( #25178, #40221, #32165, #68391 ) ) ;
#63062 = DIRECTION ( 'NONE',  ( 1.000000000000000000, 0.000000000000000000, 0.000000000000000000 ) ) ;
#63064 = ORIENTED_EDGE ( 'NONE', *, *, #62257, .T. ) ;
#63063 = CYLINDRICAL_SURFACE ( 'NONE', #48104, 2.215251240775983899 ) ;
#63065 = ORIENTED_EDGE ( 'NONE', *, *, #25872, .T. ) ;
#63066 = EDGE_CURVE ( 'NONE', #26162, #64793, #42372, .T. ) ;
#63067 = DIRECTION ( 'NONE',  ( -1.000000000000000000, 0.000000000000000000, 0.000000000000000000 ) ) ;
#63068 = DIRECTION ( 'NONE',  ( 1.000000000000000000, 0.000000000000000000, 0.000000000000000000 ) ) ;
#63069 = EDGE_CURVE ( 'NONE', #23322, #48765, #58989, .T. ) ;
#63071 = ORIENTED_EDGE ( 'NONE', *, *, #1543, .F. ) ;
#63070 = CARTESIAN_POINT ( 'NONE',  ( -10.19191654964680893, -10.20488345035333566, 195.0000000000000284 ) ) ;
#63072 = ORIENTED_EDGE ( 'NONE', *, *, #27017, .F. ) ;
#63073 = CARTESIAN_POINT ( 'NONE',  ( 11.08848345035334404, -11.08848345035349148, 455.0000000000000568 ) ) ;
#63074 = EDGE_CURVE ( 'NONE', #55865, #1150, #43772, .T. ) ;
#63075 = CARTESIAN_POINT ( 'NONE',  ( 7.000000000000000000, -20.40000000000000213, 17.60000000000000142 ) ) ;
#63076 = DIRECTION ( 'NONE',  ( 0.000000000000000000, 1.000000000000000000, 0.000000000000000000 ) ) ;
#63077 = FACE_OUTER_BOUND ( 'NONE', #24538, .T. ) ;
#63078 = EDGE_CURVE ( 'NONE', #56741, #18603, #26804, .T. ) ;
#63079 = ORIENTED_EDGE ( 'NONE', *, *, #11672, .T. ) ;
#63080 = DIRECTION ( 'NONE',  ( 0.000000000000000000, 0.000000000000000000, 1.000000000000000000 ) ) ;
#63081 = AXIS2_PLACEMENT_3D ( 'NONE', #29609, #34908, #24320 ) ;
#63082 = CYLINDRICAL_SURFACE ( 'NONE', #8357, 3.499999999999850342 ) ;
#63083 =( NAMED_UNIT ( * ) SI_UNIT ( $, .STERADIAN. ) SOLID_ANGLE_UNIT ( ) );
#63084 = ORIENTED_EDGE ( 'NONE', *, *, #27409, .T. ) ;
#63085 = EDGE_CURVE ( 'NONE', #50838, #9560, #30168, .T. ) ;
#63086 = DIRECTION ( 'NONE',  ( -0.6414496315691539108, 0.7671651518153028704, 0.000000000000000000 ) ) ;
#63087 = ADVANCED_FACE ( 'NONE', ( #54730 ), #49069, .F. ) ;
#63088 = CARTESIAN_POINT ( 'NONE',  ( 39.00000000000000000, 0.000000000000000000, 5.250000000000000000 ) ) ;
#63089 = VECTOR ( 'NONE', #51775, 1000.000000000000000 ) ;
#63090 = PLANE ( 'NONE',  #46082 ) ;
#63091 = EDGE_CURVE ( 'NONE', #27495, #3937, #5260, .T. ) ;
#63092 = ADVANCED_FACE ( 'NONE', ( #60015 ), #21170, .T. ) ;
#63093 = VERTEX_POINT ( 'NONE', #42721 ) ;
#63094 = LINE ( 'NONE', #56383, #24333 ) ;
#63095 = ADVANCED_FACE ( 'NONE', ( #26827 ), #43410, .F. ) ;
#63097 = CIRCLE ( 'NONE', #26973, 0.1999999999999987899 ) ;
#63096 = CIRCLE ( 'NONE', #6615, 0.5000000000009302559 ) ;
#63098 = DIRECTION ( 'NONE',  ( 0.000000000000000000, -1.000000000000000000, -0.000000000000000000 ) ) ;
#63099 = ORIENTED_EDGE ( 'NONE', *, *, #37390, .F. ) ;
#63100 = CARTESIAN_POINT ( 'NONE',  ( 49.00000000000000000, -21.00000000000000000, 13.86939075806900057 ) ) ;
#63101 = LINE ( 'NONE', #35506, #13953 ) ;
#63102 = DIRECTION ( 'NONE',  ( 0.000000000000000000, 0.000000000000000000, 1.000000000000000000 ) ) ;
#63103 = PLANE ( 'NONE',  #23356 ) ;
#63104 = FACE_OUTER_BOUND ( 'NONE', #908, .T. ) ;
#63105 = ORIENTED_EDGE ( 'NONE', *, *, #28229, .T. ) ;
#63106 = CYLINDRICAL_SURFACE ( 'NONE', #6239, 4.000000000000000000 ) ;
#63107 = CARTESIAN_POINT ( 'NONE',  ( -11.11351654964679270, -7.806483450353373321, 455.0000000000000568 ) ) ;
#63108 = FACE_OUTER_BOUND ( 'NONE', #42920, .T. ) ;
#63109 = SURFACE_SIDE_STYLE ('',( #42589 ) ) ;
#63110 = CARTESIAN_POINT ( 'NONE',  ( -13.00000000000000178, -15.50000000000000000, -14.50000000000000000 ) ) ;
#63111 = EDGE_CURVE ( 'NONE', #62094, #69773, #32479, .T. ) ;
#63112 = ORIENTED_EDGE ( 'NONE', *, *, #38624, .F. ) ;
#63114 = ORIENTED_EDGE ( 'NONE', *, *, #45539, .F. ) ;
#63113 = CARTESIAN_POINT ( 'NONE',  ( 283.0000000000000568, -38.10000000000000142, -8.400000000000000355 ) ) ;
#63115 = EDGE_CURVE ( 'NONE', #22607, #58343, #5596, .T. ) ;
#63116 = LINE ( 'NONE', #30943, #25994 ) ;
#63117 = CARTESIAN_POINT ( 'NONE',  ( -17.00000000000000000, -17.50000000000000000, -15.70500000000000007 ) ) ;
#63118 = DIRECTION ( 'NONE',  ( -1.836970198721029934E-16, 1.836970198721036344E-16, -1.000000000000000000 ) ) ;
#63119 = VERTEX_POINT ( 'NONE', #48726 ) ;
#63120 = SURFACE_STYLE_USAGE ( .BOTH. , #7697 ) ;
#63121 = DIRECTION ( 'NONE',  ( 0.000000000000000000, 1.000000000000000000, -0.000000000000000000 ) ) ;
#63122 = ORIENTED_EDGE ( 'NONE', *, *, #1835, .F. ) ;
#63123 = VERTEX_POINT ( 'NONE', #291 ) ;
#63124 = AXIS2_PLACEMENT_3D ( 'NONE', #38014, #11804, #28087 ) ;
#63125 = ORIENTED_EDGE ( 'NONE', *, *, #29026, .T. ) ;
#63126 = CARTESIAN_POINT ( 'NONE',  ( -8.250000000000001776, -7.249999999999998224, -10.00000000000000178 ) ) ;
#63127 = DIRECTION ( 'NONE',  ( 1.000000000000000000, -1.047444401652940007E-14, 1.836970198721010706E-16 ) ) ;
#63128 = VECTOR ( 'NONE', #431, 1000.000000000000000 ) ;
#63129 = CYLINDRICAL_SURFACE ( 'NONE', #61948, 5.200000000000009948 ) ;
#63130 = ORIENTED_EDGE ( 'NONE', *, *, #50396, .F. ) ;
#63131 = ORIENTED_EDGE ( 'NONE', *, *, #16058, .F. ) ;
#63132 = FACE_OUTER_BOUND ( 'NONE', #61244, .T. ) ;
#63133 = VECTOR ( 'NONE', #38983, 1000.000000000000000 ) ;
#63134 = CARTESIAN_POINT ( 'NONE',  ( 7.265214908726139065, 5.380658396643097419, 455.0000000000000568 ) ) ;
#63135 = ORIENTED_EDGE ( 'NONE', *, *, #4432, .F. ) ;
#63136 = ORIENTED_EDGE ( 'NONE', *, *, #33846, .F. ) ;
#63137 = EDGE_LOOP ( 'NONE', ( #8632, #18271, #6857, #11334 ) ) ;
#63138 = VECTOR ( 'NONE', #63519, 1000.000000000000000 ) ;
#63139 = VERTEX_POINT ( 'NONE', #16559 ) ;
#63140 = CARTESIAN_POINT ( 'NONE',  ( 11.08848345035342042, 11.47551654964652812, 455.0000000000000568 ) ) ;
#63142 = ORIENTED_EDGE ( 'NONE', *, *, #63819, .T. ) ;
#63141 = DIRECTION ( 'NONE',  ( -1.000000000000000000, 0.000000000000000000, 0.000000000000000000 ) ) ;
#63144 = VECTOR ( 'NONE', #65674, 1000.000000000000000 ) ;
#63143 = AXIS2_PLACEMENT_3D ( 'NONE', #20392, #31716, #63539 ) ;
#63145 = EDGE_CURVE ( 'NONE', #66744, #57618, #38134, .T. ) ;
#63146 = CARTESIAN_POINT ( 'NONE',  ( -4.141586236041130853, -5.793274621760842180, 54.00000000000000711 ) ) ;
#63147 = CARTESIAN_POINT ( 'NONE',  ( 9.955011587777175208, 2.752095193409277663, 195.0000000000000284 ) ) ;
#63148 = ORIENTED_EDGE ( 'NONE', *, *, #40615, .T. ) ;
#63149 = ADVANCED_FACE ( 'NONE', ( #27505 ), #638, .F. ) ;
#63150 = ORIENTED_EDGE ( 'NONE', *, *, #34059, .T. ) ;
#63151 = VECTOR ( 'NONE', #36468, 1000.000000000000000 ) ;
#63152 = EDGE_CURVE ( 'NONE', #26381, #63611, #67420, .T. ) ;
#63153 = DIRECTION ( 'NONE',  ( 0.000000000000000000, -0.7096009616570518874, 0.7046037717862339012 ) ) ;
#63154 = EDGE_CURVE ( 'NONE', #67917, #32193, #60353, .T. ) ;
#63155 = EDGE_CURVE ( 'NONE', #39495, #57327, #12952, .T. ) ;
#63156 = DIRECTION ( 'NONE',  ( 1.000000000000000000, -0.000000000000000000, 0.000000000000000000 ) ) ;
#63157 = ORIENTED_EDGE ( 'NONE', *, *, #32569, .T. ) ;
#63158 =( NAMED_UNIT ( * ) PLANE_ANGLE_UNIT ( ) SI_UNIT ( $, .RADIAN. ) );
#63159 = LINE ( 'NONE', #30984, #29046 ) ;
#63160 = VECTOR ( 'NONE', #42092, 1000.000000000000000 ) ;
#63161 = ORIENTED_EDGE ( 'NONE', *, *, #15423, .F. ) ;
#63162 = CARTESIAN_POINT ( 'NONE',  ( -30.00000000000000000, -17.14999999999900027, 26.64999999999900027 ) ) ;
#63163 = FACE_OUTER_BOUND ( 'NONE', #45866, .T. ) ;
#63164 = DIRECTION ( 'NONE',  ( 3.491481338843133355E-15, 1.000000000000000000, 1.836970198721029934E-16 ) ) ;
#63165 = CARTESIAN_POINT ( 'NONE',  ( 0.000000000000000000, -7.449999999999998401, -7.500000000000000000 ) ) ;
#63166 = VECTOR ( 'NONE', #6060, 1000.000000000000000 ) ;
#63167 = CARTESIAN_POINT ( 'NONE',  ( 0.9555237378828111972, 9.390476262117219974, 26.00000000000000711 ) ) ;
#63168 = ORIENTED_EDGE ( 'NONE', *, *, #44102, .T. ) ;
#63169 = DIRECTION ( 'NONE',  ( 0.000000000000000000, 1.000000000000000000, 0.000000000000000000 ) ) ;
#63170 = DIRECTION ( 'NONE',  ( 0.000000000000000000, 0.000000000000000000, 1.000000000000000000 ) ) ;
#63171 = CIRCLE ( 'NONE', #17985, 0.4999999999979843901 ) ;
#63172 = CARTESIAN_POINT ( 'NONE',  ( 290.0000000000000000, 0.000000000000000000, -4.000000000000000000 ) ) ;
#63173 = AXIS2_PLACEMENT_3D ( 'NONE', #10594, #20166, #58701 ) ;
#63174 = CARTESIAN_POINT ( 'NONE',  ( 12.00648345035338060, -4.186483450353492231, 455.0000000000000568 ) ) ;
#63175 = CARTESIAN_POINT ( 'NONE',  ( 72.77321854994619343, 47.95351654967443977, 29.00000000000000000 ) ) ;
#63176 = CARTESIAN_POINT ( 'NONE',  ( 5.257023737882819070, -5.257023737882825287, 54.00000000000000711 ) ) ;
#63177 = AXIS2_PLACEMENT_3D ( 'NONE', #61141, #11671, #6715 ) ;
#63178 = DIRECTION ( 'NONE',  ( 1.836970198721029934E-16, 1.836970198721010706E-16, -1.000000000000000000 ) ) ;
#63179 = CARTESIAN_POINT ( 'NONE',  ( 7.250000000000005329, -7.249999999999998224, -26.00000000000001066 ) ) ;
#63180 = VERTEX_POINT ( 'NONE', #29569 ) ;
#63181 = CARTESIAN_POINT ( 'NONE',  ( -6.651770455163778628, -7.532023737882784786, 26.00000000000000000 ) ) ;
#63182 = CARTESIAN_POINT ( 'NONE',  ( 8.750000000000005329, 0.000000000000000000, -30.00000000000001066 ) ) ;
#63183 = ORIENTED_EDGE ( 'NONE', *, *, #43697, .F. ) ;
#63184 = LINE ( 'NONE', #31011, #731 ) ;
#63185 = DIRECTION ( 'NONE',  ( 0.000000000000000000, 1.000000000000000000, 0.000000000000000000 ) ) ;
#63186 = VECTOR ( 'NONE', #13073, 1000.000000000000000 ) ;
#63187 = PLANE ( 'NONE',  #37801 ) ;
#63188 = CARTESIAN_POINT ( 'NONE',  ( -11.00000000000000000, -11.50000000000000000, 15.00000000000000000 ) ) ;
#63189 = DIRECTION ( 'NONE',  ( -1.000000000000000000, 6.308085367188447236E-15, 0.000000000000000000 ) ) ;
#63190 = ORIENTED_EDGE ( 'NONE', *, *, #28368, .T. ) ;
#63191 = AXIS2_PLACEMENT_3D ( 'NONE', #48319, #44037, #43343 ) ;
#63192 = ADVANCED_FACE ( 'NONE', ( #28870 ), #45480, .F. ) ;
#63193 = ORIENTED_EDGE ( 'NONE', *, *, #43642, .T. ) ;
#63194 = DIRECTION ( 'NONE',  ( -0.000000000000000000, -0.000000000000000000, -1.000000000000000000 ) ) ;
#63195 = CARTESIAN_POINT ( 'NONE',  ( 20.90000000000000213, -21.00000000000000000, 13.86939075806900057 ) ) ;
#63196 = VERTEX_POINT ( 'NONE', #22886 ) ;
#63197 = EDGE_CURVE ( 'NONE', #20570, #65126, #995, .T. ) ;
#63198 = DIRECTION ( 'NONE',  ( 8.673617379884013384E-15, 1.000000000000000000, 0.000000000000000000 ) ) ;
#63199 = VECTOR ( 'NONE', #26797, 1000.000000000000000 ) ;
#63200 = CARTESIAN_POINT ( 'NONE',  ( 41.09999999999999432, -14.48845687959340012, 21.00000000000000000 ) ) ;
#63201 = ORIENTED_EDGE ( 'NONE', *, *, #68472, .T. ) ;
#63202 = DIRECTION ( 'NONE',  ( 0.000000000000000000, 0.000000000000000000, 1.000000000000000000 ) ) ;
#63203 = EDGE_LOOP ( 'NONE', ( #2576, #20265, #24952, #49783 ) ) ;
#63204 = ORIENTED_EDGE ( 'NONE', *, *, #7886, .T. ) ;
#63205 = CARTESIAN_POINT ( 'NONE',  ( -28.00000000000000000, -17.50000000000000000, -15.70500000000000007 ) ) ;
#63206 = ORIENTED_EDGE ( 'NONE', *, *, #45489, .T. ) ;
#63207 = ORIENTED_EDGE ( 'NONE', *, *, #51634, .T. ) ;
#63208 = FACE_OUTER_BOUND ( 'NONE', #33721, .T. ) ;
#63209 = DIRECTION ( 'NONE',  ( -1.000000000000000000, 0.000000000000000000, 0.000000000000000000 ) ) ;
#63210 = DIRECTION ( 'NONE',  ( 1.000000000000000000, 0.000000000000000000, 0.000000000000000000 ) ) ;
#63211 = VECTOR ( 'NONE', #64895, 1000.000000000000000 ) ;
#63212 = ADVANCED_FACE ( 'NONE', ( #2015 ), #34169, .T. ) ;
#63213 = VERTEX_POINT ( 'NONE', #23574 ) ;
#63214 = DIRECTION ( 'NONE',  ( -0.000000000000000000, 0.000000000000000000, -1.000000000000000000 ) ) ;
#63216 = CARTESIAN_POINT ( 'NONE',  ( 3.606483450353406006, 7.415254214038213831, 455.0000000000000568 ) ) ;
#63215 = CARTESIAN_POINT ( 'NONE',  ( 49.00000000000000000, -14.06939075806900163, -20.80000000000000426 ) ) ;
#63217 = ORIENTED_EDGE ( 'NONE', *, *, #34684, .F. ) ;
#63219 = ORIENTED_EDGE ( 'NONE', *, *, #47515, .T. ) ;
#63218 = CARTESIAN_POINT ( 'NONE',  ( 7.000000000000000000, -39.80000000000000426, -12.69999999999999929 ) ) ;
#63220 = ORIENTED_EDGE ( 'NONE', *, *, #5594, .T. ) ;
#63221 = APPLICATION_PROTOCOL_DEFINITION ( 'draft international standard', 'automotive_design', 1998, #25050 ) ;
#63222 = DIRECTION ( 'NONE',  ( -1.000000000000000000, 0.000000000000000000, 0.000000000000000000 ) ) ;
#63223 = AXIS2_PLACEMENT_3D ( 'NONE', #67378, #67713, #51456 ) ;
#63224 = VECTOR ( 'NONE', #49727, 1000.000000000000000 ) ;
#63226 = ORIENTED_EDGE ( 'NONE', *, *, #42312, .T. ) ;
#63225 = LINE ( 'NONE', #42705, #40997 ) ;
#63227 = EDGE_CURVE ( 'NONE', #32424, #13109, #45131, .T. ) ;
#63228 = DIRECTION ( 'NONE',  ( 0.000000000000000000, 1.000000000000000000, 0.000000000000000000 ) ) ;
#63229 = CIRCLE ( 'NONE', #4542, 0.1999999999999987899 ) ;
#63230 = CARTESIAN_POINT ( 'NONE',  ( 23.90000000000000213, -0.000000000000000000, -20.80000000000000426 ) ) ;
#63231 = ORIENTED_EDGE ( 'NONE', *, *, #7471, .F. ) ;
#63232 = ORIENTED_EDGE ( 'NONE', *, *, #58569, .T. ) ;
#63233 = AXIS2_PLACEMENT_3D ( 'NONE', #63870, #15775, #57503 ) ;
#63234 = AXIS2_PLACEMENT_3D ( 'NONE', #25794, #6296, #12268 ) ;
#63235 = DIRECTION ( 'NONE',  ( 0.000000000000000000, -3.673940397442059868E-16, 1.000000000000000000 ) ) ;
#63236 = ADVANCED_FACE ( 'NONE', ( #66709 ), #66008, .F. ) ;
#63237 = EDGE_CURVE ( 'NONE', #10783, #26250, #65678, .T. ) ;
#63238 = EDGE_LOOP ( 'NONE', ( #16686, #67062, #34064, #23553, #61515, #22248, #35343, #44708 ) ) ;
#63239 = AXIS2_PLACEMENT_3D ( 'NONE', #2046, #19004, #18292 ) ;
#63240 = FACE_OUTER_BOUND ( 'NONE', #62441, .T. ) ;
#63241 = DIRECTION ( 'NONE',  ( 0.000000000000000000, 0.000000000000000000, 1.000000000000000000 ) ) ;
#63242 = ADVANCED_FACE ( 'NONE', ( #6959 ), #17226, .T. ) ;
#63243 = DIRECTION ( 'NONE',  ( 1.047444401652940007E-14, 1.000000000000000000, 1.836970198721029934E-16 ) ) ;
#63244 = ADVANCED_FACE ( 'NONE', ( #11912 ), #17917, .T. ) ;
#63245 = AXIS2_PLACEMENT_3D ( 'NONE', #14278, #45733, #35471 ) ;
#63246 = VERTEX_POINT ( 'NONE', #39825 ) ;
#63247 = AXIS2_PLACEMENT_3D ( 'NONE', #25896, #36863, #69019 ) ;
#63248 = EDGE_CURVE ( 'NONE', #10391, #68282, #66374, .T. ) ;
#63249 = DIRECTION ( 'NONE',  ( 0.000000000000000000, -0.9938079899998859545, 0.1111111111112941946 ) ) ;
#63250 = CARTESIAN_POINT ( 'NONE',  ( -5.242976262117275077, -5.257023737882800418, 26.00000000000000711 ) ) ;
#63252 = ORIENTED_EDGE ( 'NONE', *, *, #58301, .T. ) ;
#63251 = DIRECTION ( 'NONE',  ( 3.614007241618349165E-15, 1.000000000000000000, 0.000000000000000000 ) ) ;
#63254 = ORIENTED_EDGE ( 'NONE', *, *, #1487, .F. ) ;
#63253 = CYLINDRICAL_SURFACE ( 'NONE', #46730, 0.5249999999999994671 ) ;
#63255 = CARTESIAN_POINT ( 'NONE',  ( 7.357023737882817827, -4.961189459950063885, 54.00000000000000711 ) ) ;
#63256 = AXIS2_PLACEMENT_3D ( 'NONE', #11753, #33338, #27686 ) ;
#63257 = AXIS2_PLACEMENT_3D ( 'NONE', #41208, #14358, #37325 ) ;
#63258 = LINE ( 'NONE', #57597, #16088 ) ;
#63259 = CARTESIAN_POINT ( 'NONE',  ( 46.39999999999999858, 33.00000000000000000, -2.250000000000000444 ) ) ;
#63260 = DIRECTION ( 'NONE',  ( 1.000000000000000000, -0.000000000000000000, 0.000000000000000000 ) ) ;
#63261 = PLANE ( 'NONE',  #42103 ) ;
#63262 = ORIENTED_EDGE ( 'NONE', *, *, #47761, .T. ) ;
#63263 = CARTESIAN_POINT ( 'NONE',  ( 0.000000000000000000, -7.449999999999998401, -16.00000000000000000 ) ) ;
#63264 = CARTESIAN_POINT ( 'NONE',  ( -4.947141984184481700, 7.342976262117180575, 54.00000000000000711 ) ) ;
#63265 = FILL_AREA_STYLE ('',( #9521 ) ) ;
#63267 = ORIENTED_EDGE ( 'NONE', *, *, #69589, .F. ) ;
#63266 = DIRECTION ( 'NONE',  ( 0.000000000000000000, 0.000000000000000000, -1.000000000000000000 ) ) ;
#63268 = DIRECTION ( 'NONE',  ( 3.540573132209561620E-15, 1.000000000000000000, 0.000000000000000000 ) ) ;
#63269 = AXIS2_PLACEMENT_3D ( 'NONE', #19558, #15320, #4015 ) ;
#63270 = FACE_OUTER_BOUND ( 'NONE', #13526, .T. ) ;
#63271 = CARTESIAN_POINT ( 'NONE',  ( 283.0000000000000568, -25.56180396883900130, -14.25872597390799967 ) ) ;
#63272 = ORIENTED_EDGE ( 'NONE', *, *, #38386, .T. ) ;
#63273 = CARTESIAN_POINT ( 'NONE',  ( 14.89999999999999680, 20.60000000000000142, 13.86939075806900057 ) ) ;
#63274 = PLANE ( 'NONE',  #7990 ) ;
#63275 = ORIENTED_EDGE ( 'NONE', *, *, #42176, .T. ) ;
#63276 = FILL_AREA_STYLE_COLOUR ( '', #60520 ) ;
#63277 = LINE ( 'NONE', #46653, #53818 ) ;
#63278 = FACE_OUTER_BOUND ( 'NONE', #14607, .T. ) ;
#63279 = CARTESIAN_POINT ( 'NONE',  ( 4.155633711806658859, -5.793274621760842180, 54.00000000000000711 ) ) ;
#63280 = VECTOR ( 'NONE', #6025, 1000.000000000000000 ) ;
#63281 = DIRECTION ( 'NONE',  ( 1.000000000000000000, -0.000000000000000000, 0.000000000000000000 ) ) ;
#63282 = VECTOR ( 'NONE', #26409, 1000.000000000000114 ) ;
#63283 = ORIENTED_EDGE ( 'NONE', *, *, #58286, .T. ) ;
#63284 = DIRECTION ( 'NONE',  ( 0.000000000000000000, 0.7071067811865474617, -0.7071067811865474617 ) ) ;
#63285 = ORIENTED_EDGE ( 'NONE', *, *, #34592, .T. ) ;
#63286 = EDGE_LOOP ( 'NONE', ( #24835, #65147, #25273, #710 ) ) ;
#63287 = EDGE_LOOP ( 'NONE', ( #45020, #708, #10035, #10830 ) ) ;
#63288 = ORIENTED_EDGE ( 'NONE', *, *, #55636, .F. ) ;
#63289 = ADVANCED_FACE ( 'NONE', ( #7302 ), #61044, .T. ) ;
#63290 = AXIS2_PLACEMENT_3D ( 'NONE', #66304, #17862, #13863 ) ;
#63291 = CARTESIAN_POINT ( 'NONE',  ( 3.664523737882820598, 10.49297626211720491, 54.00000000000000711 ) ) ;
#63292 = EDGE_CURVE ( 'NONE', #3551, #10117, #55085, .T. ) ;
#63293 = EDGE_CURVE ( 'NONE', #29691, #22003, #8760, .T. ) ;
#63294 = VECTOR ( 'NONE', #46489, 1000.000000000000000 ) ;
#63295 = DIRECTION ( 'NONE',  ( -0.000000000000000000, -0.000000000000000000, 1.000000000000000000 ) ) ;
#63296 = CARTESIAN_POINT ( 'NONE',  ( -5.993516549646711766, 5.993516549646603409, 455.0000000000000568 ) ) ;
#63297 = ORIENTED_EDGE ( 'NONE', *, *, #7030, .T. ) ;
#63298 = EDGE_LOOP ( 'NONE', ( #35595, #36982, #38613, #49455, #34782, #40839, #47087, #54789 ) ) ;
#63299 = CIRCLE ( 'NONE', #69, 3.999999999999993339 ) ;
#63300 = CARTESIAN_POINT ( 'NONE',  ( 7.250000000000005329, -7.449999999999998401, -12.00000000000000000 ) ) ;
#63301 = ORIENTED_EDGE ( 'NONE', *, *, #55417, .T. ) ;
#63302 = VERTEX_POINT ( 'NONE', #28194 ) ;
#63303 = FACE_OUTER_BOUND ( 'NONE', #271, .T. ) ;
#63304 = DIRECTION ( 'NONE',  ( 0.000000000000000000, 0.7071067811865475727, 0.7071067811865475727 ) ) ;
#63305 = DIRECTION ( 'NONE',  ( 0.000000000000000000, 0.000000000000000000, 1.000000000000000000 ) ) ;
#63306 = ORIENTED_EDGE ( 'NONE', *, *, #37136, .F. ) ;
#63307 = CARTESIAN_POINT ( 'NONE',  ( 14.75000000000000178, -42.25000000000000000, -26.75000000000000000 ) ) ;
#63308 = AXIS2_PLACEMENT_3D ( 'NONE', #38563, #44194, #22641 ) ;
#63309 = VECTOR ( 'NONE', #59229, 1000.000000000000000 ) ;
#63311 = LINE ( 'NONE', #4278, #23147 ) ;
#63310 = DIRECTION ( 'NONE',  ( 0.4285714285711672566, 0.000000000000000000, 0.9035079029053751931 ) ) ;
#63312 = ORIENTED_EDGE ( 'NONE', *, *, #46080, .T. ) ;
#63314 = ORIENTED_EDGE ( 'NONE', *, *, #8478, .F. ) ;
#63313 = CARTESIAN_POINT ( 'NONE',  ( -25.50000000000000355, -5.200000000000001066, 20.24999999999999645 ) ) ;
#63315 = ORIENTED_EDGE ( 'NONE', *, *, #50611, .F. ) ;
#63316 = PLANE ( 'NONE',  #55860 ) ;
#63317 = DIRECTION ( 'NONE',  ( 1.000000000000000000, 0.000000000000000000, 0.000000000000000000 ) ) ;
#63318 = CIRCLE ( 'NONE', #37380, 24.99999999998789946 ) ;
#63319 = VERTEX_POINT ( 'NONE', #30636 ) ;
#63320 = ORIENTED_EDGE ( 'NONE', *, *, #861, .T. ) ;
#63321 = LINE ( 'NONE', #9579, #28506 ) ;
#63322 = DIRECTION ( 'NONE',  ( 0.000000000000000000, 0.000000000000000000, -1.000000000000000000 ) ) ;
#63323 = EDGE_LOOP ( 'NONE', ( #44136, #5372, #3634, #5009 ) ) ;
#63324 = ORIENTED_EDGE ( 'NONE', *, *, #55487, .F. ) ;
#63325 = DIRECTION ( 'NONE',  ( 1.000000000000000000, -5.981805089575194965E-17, 0.000000000000000000 ) ) ;
#63326 = DIRECTION ( 'NONE',  ( 1.000000000000000000, 0.000000000000000000, 0.000000000000000000 ) ) ;
#63327 = VECTOR ( 'NONE', #62896, 999.9999999999998863 ) ;
#63328 = ORIENTED_EDGE ( 'NONE', *, *, #38792, .F. ) ;
#63329 = EDGE_CURVE ( 'NONE', #35173, #43873, #40532, .T. ) ;
#63330 = CIRCLE ( 'NONE', #32844, 1.399999999999998579 ) ;
#63331 = ADVANCED_FACE ( 'NONE', ( #62807 ), #14008, .T. ) ;
#63332 = CARTESIAN_POINT ( 'NONE',  ( 8.250000000000005329, -7.249999999999998224, -23.50000000000000000 ) ) ;
#63333 = DIRECTION ( 'NONE',  ( 0.000000000000000000, 0.000000000000000000, 1.000000000000000000 ) ) ;
#63334 = EDGE_CURVE ( 'NONE', #31845, #13045, #46186, .T. ) ;
#63336 = VERTEX_POINT ( 'NONE', #67427 ) ;
#63335 = CARTESIAN_POINT ( 'NONE',  ( 7.500000000000000000, -20.49999999999999645, 20.00000000000000000 ) ) ;
#63338 = ORIENTED_EDGE ( 'NONE', *, *, #54622, .T. ) ;
#63337 = LINE ( 'NONE', #31869, #66203 ) ;
#63339 = VECTOR ( 'NONE', #26579, 1000.000000000000000 ) ;
#63340 = DIRECTION ( 'NONE',  ( -1.000000000000000000, 0.000000000000000000, 0.000000000000000000 ) ) ;
#63341 = EDGE_CURVE ( 'NONE', #30940, #47029, #27949, .T. ) ;
#63342 = DIRECTION ( 'NONE',  ( -1.000000000000000000, 0.000000000000000000, 0.000000000000000000 ) ) ;
#63343 = FACE_BOUND ( 'NONE', #69371, .T. ) ;
#63344 = DIRECTION ( 'NONE',  ( -9.912705577010336396E-15, -1.000000000000000000, 0.000000000000000000 ) ) ;
#63345 = PRODUCT_DEFINITION ( 'UNKNOWN', '', #9905, #11961 ) ;
#63346 = VECTOR ( 'NONE', #43360, 1000.000000000000000 ) ;
#63347 = AXIS2_PLACEMENT_3D ( 'NONE', #68158, #30688, #3809 ) ;
#63348 = CARTESIAN_POINT ( 'NONE',  ( 181.4833316329832940, 0.000000000000000000, 276.7801873289890295 ) ) ;
#63349 = EDGE_CURVE ( 'NONE', #50861, #47806, #18975, .T. ) ;
#63350 = DIRECTION ( 'NONE',  ( 1.000000000000000000, -0.000000000000000000, -0.000000000000000000 ) ) ;
#63351 = VERTEX_POINT ( 'NONE', #67759 ) ;
#63352 = DIRECTION ( 'NONE',  ( -0.000000000000000000, -0.000000000000000000, -1.000000000000000000 ) ) ;
#63353 = EDGE_CURVE ( 'NONE', #17119, #46858, #20029, .T. ) ;
#63354 = VECTOR ( 'NONE', #69117, 1000.000000000000000 ) ;
#63356 = ORIENTED_EDGE ( 'NONE', *, *, #67786, .F. ) ;
#63355 = FACE_BOUND ( 'NONE', #18688, .T. ) ;
#63357 = FACE_OUTER_BOUND ( 'NONE', #24655, .T. ) ;
#63358 = CYLINDRICAL_SURFACE ( 'NONE', #32394, 1.224999999999999423 ) ;
#63359 = CARTESIAN_POINT ( 'NONE',  ( 9.190000000000001279, -9.750000000000001776, -5.000000000000000000 ) ) ;
#63360 = DIRECTION ( 'NONE',  ( 1.000000000000000000, -0.000000000000000000, 0.000000000000000000 ) ) ;
#63361 = AXIS2_PLACEMENT_3D ( 'NONE', #31087, #58316, #9877 ) ;
#63362 = ORIENTED_EDGE ( 'NONE', *, *, #2710, .F. ) ;
#63363 = DIRECTION ( 'NONE',  ( 0.000000000000000000, 0.000000000000000000, -1.000000000000000000 ) ) ;
#63364 = FACE_OUTER_BOUND ( 'NONE', #12169, .T. ) ;
#63365 = EDGE_LOOP ( 'NONE', ( #23423, #38274, #53353, #39296 ) ) ;
#63366 = DIRECTION ( 'NONE',  ( 0.000000000000000000, -1.000000000000000000, 0.000000000000000000 ) ) ;
#63367 = PLANE ( 'NONE',  #53997 ) ;
#63368 = DIRECTION ( 'NONE',  ( -1.000000000000000000, 0.000000000000000000, 0.000000000000000000 ) ) ;
#63369 = ORIENTED_EDGE ( 'NONE', *, *, #44226, .T. ) ;
#63370 = VECTOR ( 'NONE', #14367, 1000.000000000000000 ) ;
#63371 = LINE ( 'NONE', #8560, #1122 ) ;
#63372 = ORIENTED_EDGE ( 'NONE', *, *, #15360, .F. ) ;
#63373 = EDGE_LOOP ( 'NONE', ( #29124, #56176, #48904, #22935 ) ) ;
#63374 = FACE_OUTER_BOUND ( 'NONE', #67122, .T. ) ;
#63375 = DIRECTION ( 'NONE',  ( 1.221996412923863792E-14, 1.000000000000000000, 1.836970198721013910E-16 ) ) ;
#63376 = DIRECTION ( 'NONE',  ( -1.000000000000000000, 0.000000000000000000, 0.000000000000000000 ) ) ;
#63377 = EDGE_CURVE ( 'NONE', #47907, #5174, #60696, .T. ) ;
#63378 = CARTESIAN_POINT ( 'NONE',  ( 11.18999999999999950, -11.18999999999999950, 0.000000000000000000 ) ) ;
#63379 = DIRECTION ( 'NONE',  ( 1.000000000000000000, 0.000000000000000000, 0.000000000000000000 ) ) ;
#63380 = ORIENTED_EDGE ( 'NONE', *, *, #38896, .T. ) ;
#63381 = ORIENTED_EDGE ( 'NONE', *, *, #24123, .F. ) ;
#63382 = CIRCLE ( 'NONE', #6925, 4.000000000000000000 ) ;
#63384 = ORIENTED_EDGE ( 'NONE', *, *, #58817, .F. ) ;
#63383 = CARTESIAN_POINT ( 'NONE',  ( 27.90000000000000213, 0.000000000000000000, 2.154935995002245293E-15 ) ) ;
#63385 = VERTEX_POINT ( 'NONE', #62091 ) ;
#63386 = VECTOR ( 'NONE', #53876, 1000.000000000000000 ) ;
#63387 = PLANE ( 'NONE',  #34883 ) ;
#63388 = DIRECTION ( 'NONE',  ( -0.000000000000000000, 1.000000000000000000, -0.000000000000000000 ) ) ;
#63389 = FACE_OUTER_BOUND ( 'NONE', #69755, .T. ) ;
#63390 = VECTOR ( 'NONE', #60379, 1000.000000000000000 ) ;
#63391 = FACE_OUTER_BOUND ( 'NONE', #41593, .T. ) ;
#63392 = EDGE_CURVE ( 'NONE', #19600, #67816, #40880, .T. ) ;
#63394 = DIRECTION ( 'NONE',  ( -0.000000000000000000, -1.000000000000000000, -0.000000000000000000 ) ) ;
#63393 = DIRECTION ( 'NONE',  ( -1.000000000000000000, 0.000000000000000000, 0.000000000000000000 ) ) ;
#63395 = EDGE_LOOP ( 'NONE', ( #19914, #31595, #30853, #47890 ) ) ;
#63396 = ORIENTED_EDGE ( 'NONE', *, *, #8257, .F. ) ;
#63397 = ORIENTED_EDGE ( 'NONE', *, *, #64350, .T. ) ;
#63398 = AXIS2_PLACEMENT_3D ( 'NONE', #31647, #47889, #58527 ) ;
#63399 = CIRCLE ( 'NONE', #2401, 2.000000000000001776 ) ;
#63400 = ORIENTED_EDGE ( 'NONE', *, *, #11148, .F. ) ;
#63401 = EDGE_CURVE ( 'NONE', #28084, #34664, #2699, .T. ) ;
#63402 = DIRECTION ( 'NONE',  ( 0.000000000000000000, 0.000000000000000000, 1.000000000000000000 ) ) ;
#63403 = CARTESIAN_POINT ( 'NONE',  ( -6.835476262117260227, 10.49297626211718359, 54.00000000000000711 ) ) ;
#63404 = VECTOR ( 'NONE', #21986, 1000.000000000000114 ) ;
#63405 = DIRECTION ( 'NONE',  ( 1.836970198721029934E-16, 1.836970198721010706E-16, -1.000000000000000000 ) ) ;
#63406 = ORIENTED_EDGE ( 'NONE', *, *, #66956, .T. ) ;
#63407 = ORIENTED_EDGE ( 'NONE', *, *, #29875, .T. ) ;
#63408 = EDGE_LOOP ( 'NONE', ( #8010, #6066 ) ) ;
#63410 = DIRECTION ( 'NONE',  ( 0.000000000000000000, 1.000000000000000000, 0.000000000000000000 ) ) ;
#63409 = AXIS2_PLACEMENT_3D ( 'NONE', #52400, #46729, #41432 ) ;
#63411 = EDGE_LOOP ( 'NONE', ( #12800, #49343, #59226, #17566 ) ) ;
#63412 = ORIENTED_EDGE ( 'NONE', *, *, #64017, .F. ) ;
#63413 = DIRECTION ( 'NONE',  ( 1.836970198721029934E-16, 1.836970198721010706E-16, -1.000000000000000000 ) ) ;
#63414 = EDGE_CURVE ( 'NONE', #39526, #6741, #4127, .T. ) ;
#63415 = ORIENTED_EDGE ( 'NONE', *, *, #62429, .F. ) ;
#63416 = ORIENTED_EDGE ( 'NONE', *, *, #30936, .F. ) ;
#63417 = CARTESIAN_POINT ( 'NONE',  ( -11.00000000000000000, -12.00000000000000000, -10.52786404500095863 ) ) ;
#63419 = ORIENTED_EDGE ( 'NONE', *, *, #37191, .T. ) ;
#63418 = CARTESIAN_POINT ( 'NONE',  ( -15.50000000000000000, -5.000000000000000000, 26.50000000000000000 ) ) ;
#63420 = ORIENTED_EDGE ( 'NONE', *, *, #21613, .T. ) ;
#63421 = CYLINDRICAL_SURFACE ( 'NONE', #22776, 0.1999999999999996503 ) ;
#63422 = CIRCLE ( 'NONE', #65630, 4.000000000000000000 ) ;
#63423 = ADVANCED_FACE ( 'NONE', ( #35214 ), #24981, .F. ) ;
#63424 = DIRECTION ( 'NONE',  ( -0.6414496315691473605, -0.7671651518153083105, -2.309356642089130002E-17 ) ) ;
#63426 = ORIENTED_EDGE ( 'NONE', *, *, #14236, .T. ) ;
#63425 = DIRECTION ( 'NONE',  ( 1.000000000000000000, -0.000000000000000000, -0.000000000000000000 ) ) ;
#63427 = EDGE_LOOP ( 'NONE', ( #55350, #26290, #7287, #66853 ) ) ;
#63428 = CARTESIAN_POINT ( 'NONE',  ( -29.50000000000000355, -11.50000000000100009, 15.00000000000084910 ) ) ;
#63429 = ADVANCED_FACE ( 'NONE', ( #68469 ), #30291, .F. ) ;
#63430 = FACE_OUTER_BOUND ( 'NONE', #54993, .T. ) ;
#63431 = CARTESIAN_POINT ( 'NONE',  ( -6.642976262117334940, -10.31452373788278898, 54.00000000000000711 ) ) ;
#63432 = CARTESIAN_POINT ( 'NONE',  ( -2.530476262117228092, 9.722976262117159152, 54.00000000000000711 ) ) ;
#63433 = EDGE_CURVE ( 'NONE', #16007, #40969, #46534, .T. ) ;
#63434 = CIRCLE ( 'NONE', #18231, 0.3499999999998875677 ) ;
#63435 = ORIENTED_EDGE ( 'NONE', *, *, #7185, .F. ) ;
#63436 = LINE ( 'NONE', #14641, #63089 ) ;
#63437 = EDGE_CURVE ( 'NONE', #53130, #32607, #63159, .T. ) ;
#63438 = DIRECTION ( 'NONE',  ( 0.000000000000000000, -1.000000000000000000, 0.000000000000000000 ) ) ;
#63439 = CIRCLE ( 'NONE', #50998, 5.000000000000000000 ) ;
#63440 = CARTESIAN_POINT ( 'NONE',  ( -9.942044687070568543, 2.752095193409294982, 455.0000000000000568 ) ) ;
#63441 = DIRECTION ( 'NONE',  ( -0.000000000000000000, -0.000000000000000000, 1.000000000000000000 ) ) ;
#63442 = CARTESIAN_POINT ( 'NONE',  ( -3.834182069070765309, 7.342976262117170805, 26.00000000000000711 ) ) ;
#63443 = EDGE_CURVE ( 'NONE', #17140, #17991, #24568, .T. ) ;
#63444 = AXIS2_PLACEMENT_3D ( 'NONE', #10502, #36324, #47292 ) ;
#63445 = CLOSED_SHELL ( 'NONE', ( #38664, #17620, #41777, #1892, #64362, #16143, #54945, #7609, #66224 ) ) ;
#63446 = ORIENTED_EDGE ( 'NONE', *, *, #55497, .F. ) ;
#63447 = PRESENTATION_STYLE_ASSIGNMENT (( #58134 ) ) ;
#63448 = CARTESIAN_POINT ( 'NONE',  ( -8.513516549646713116, 11.29351654964659701, 195.0000000000000284 ) ) ;
#63449 = DIRECTION ( 'NONE',  ( 0.000000000000000000, 0.000000000000000000, 1.000000000000000000 ) ) ;
#63450 = ORIENTED_EDGE ( 'NONE', *, *, #19333, .F. ) ;
#63451 = CARTESIAN_POINT ( 'NONE',  ( 8.250000000000005329, 0.000000000000000000, -16.50000000000000000 ) ) ;
#63452 = ADVANCED_FACE ( 'NONE', ( #35942 ), #57499, .F. ) ;
#63453 = DIRECTION ( 'NONE',  ( 1.836970198721029934E-16, -1.836970198721036344E-16, 1.000000000000000000 ) ) ;
#63454 = CARTESIAN_POINT ( 'NONE',  ( -8.393516549646792058, -7.616533956692236096, 455.0000000000000568 ) ) ;
#63455 = VECTOR ( 'NONE', #27280, 1000.000000000000114 ) ;
#63456 = DIRECTION ( 'NONE',  ( 0.000000000000000000, -0.9921567416492215186, 0.1249999999999996531 ) ) ;
#63457 = FACE_OUTER_BOUND ( 'NONE', #66592, .T. ) ;
#63458 = ORIENTED_EDGE ( 'NONE', *, *, #45744, .T. ) ;
#63459 = CYLINDRICAL_SURFACE ( 'NONE', #7236, 0.2000000000000005107 ) ;
#63460 = DIRECTION ( 'NONE',  ( 0.000000000000000000, 0.000000000000000000, -1.000000000000000000 ) ) ;
#63461 = CARTESIAN_POINT ( 'NONE',  ( -3.710438382363119736, 7.394232575409525943, 26.00000000000000711 ) ) ;
#63462 = ADVANCED_FACE ( 'NONE', ( #58208 ), #57849, .F. ) ;
#63463 = DIRECTION ( 'NONE',  ( 0.4999999999999755196, -0.8660254037844528074, 0.000000000000000000 ) ) ;
#63464 = DIRECTION ( 'NONE',  ( 8.673617379884087537E-15, 1.000000000000000000, 0.000000000000000000 ) ) ;
#63465 = EDGE_LOOP ( 'NONE', ( #56774, #1117, #30614, #38428 ) ) ;
#63467 = ORIENTED_EDGE ( 'NONE', *, *, #43284, .T. ) ;
#63466 = PLANE ( 'NONE',  #39599 ) ;
#63468 = EDGE_CURVE ( 'NONE', #63045, #58759, #555, .T. ) ;
#63469 = CARTESIAN_POINT ( 'NONE',  ( 9.912023737882815766, -6.657023737882824754, 54.00000000000000711 ) ) ;
#63470 = VECTOR ( 'NONE', #8964, 1000.000000000000000 ) ;
#63471 = DIRECTION ( 'NONE',  ( -1.000000000000000000, 0.000000000000000000, 0.000000000000000000 ) ) ;
#63472 = DIRECTION ( 'NONE',  ( -0.000000000000000000, 0.000000000000000000, 1.000000000000000000 ) ) ;
#63473 = ORIENTED_EDGE ( 'NONE', *, *, #50092, .T. ) ;
#63474 = ADVANCED_FACE ( 'NONE', ( #64911 ), #11154, .F. ) ;
#63475 = DIRECTION ( 'NONE',  ( 0.000000000000000000, 0.000000000000000000, 1.000000000000000000 ) ) ;
#63476 = CARTESIAN_POINT ( 'NONE',  ( 0.000000000000000000, -7.449999999999998401, -25.50000000000000355 ) ) ;
#63477 = EDGE_CURVE ( 'NONE', #28520, #1459, #22124, .T. ) ;
#63478 = VECTOR ( 'NONE', #56814, 1000.000000000000000 ) ;
#63479 = ORIENTED_EDGE ( 'NONE', *, *, #31729, .F. ) ;
#63480 = ORIENTED_EDGE ( 'NONE', *, *, #53453, .F. ) ;
#63481 = ORIENTED_EDGE ( 'NONE', *, *, #11898, .T. ) ;
#63482 = ADVANCED_FACE ( 'NONE', ( #59941 ), #53269, .T. ) ;
#63483 = VECTOR ( 'NONE', #8091, 1000.000000000000000 ) ;
#63484 = DIRECTION ( 'NONE',  ( -0.000000000000000000, -0.000000000000000000, -1.000000000000000000 ) ) ;
#63485 = DIRECTION ( 'NONE',  ( -1.000000000000000000, 0.000000000000000000, 0.000000000000000000 ) ) ;
#63486 = DIRECTION ( 'NONE',  ( 1.000000000000000000, 0.000000000000000000, 0.000000000000000000 ) ) ;
#63487 = ORIENTED_EDGE ( 'NONE', *, *, #28109, .F. ) ;
#63488 = ADVANCED_FACE ( 'NONE', ( #21420 ), #32041, .T. ) ;
#63489 = ORIENTED_EDGE ( 'NONE', *, *, #51013, .F. ) ;
#63490 = VECTOR ( 'NONE', #37926, 1000.000000000000114 ) ;
#63491 = DIRECTION ( 'NONE',  ( 1.836970198721029934E-16, 1.836970198721010706E-16, -1.000000000000000000 ) ) ;
#63492 = EDGE_CURVE ( 'NONE', #61811, #16870, #33594, .T. ) ;
#63493 = CARTESIAN_POINT ( 'NONE',  ( 32.89999999999999858, -14.06939075806902117, -20.80000000000000426 ) ) ;
#63494 = ORIENTED_EDGE ( 'NONE', *, *, #61740, .T. ) ;
#63495 = EDGE_CURVE ( 'NONE', #66935, #3246, #872, .T. ) ;
#63496 = ORIENTED_EDGE ( 'NONE', *, *, #19685, .T. ) ;
#63498 = EDGE_CURVE ( 'NONE', #12180, #7082, #16821, .T. ) ;
#63497 = VECTOR ( 'NONE', #47902, 1000.000000000000000 ) ;
#63499 = EDGE_CURVE ( 'NONE', #37491, #59376, #43748, .T. ) ;
#63500 = ORIENTED_EDGE ( 'NONE', *, *, #5781, .F. ) ;
#63501 = ORIENTED_EDGE ( 'NONE', *, *, #17890, .F. ) ;
#63502 = CYLINDRICAL_SURFACE ( 'NONE', #16933, 1.500000000000000444 ) ;
#63503 = UNCERTAINTY_MEASURE_WITH_UNIT (LENGTH_MEASURE( 1.000000000000000082E-05 ), #4504, 'distance_accuracy_value', 'NONE');
#63505 = EDGE_LOOP ( 'NONE', ( #68371, #54632, #51860, #41216 ) ) ;
#63504 = CARTESIAN_POINT ( 'NONE',  ( 9.417013320880792904, -1.866219381641561315, 455.0000000000000568 ) ) ;
#63506 = AXIS2_PLACEMENT_3D ( 'NONE', #16245, #65044, #37134 ) ;
#63507 = EDGE_CURVE ( 'NONE', #44316, #46512, #31699, .T. ) ;
#63509 = B_SPLINE_CURVE_WITH_KNOTS ( 'NONE', 3,
 ( #4953, #31837, #26519, #48088, #69667, #21229 ),
 .UNSPECIFIED., .F., .F.,
 ( 4, 2, 4 ),
 ( 0.0002380763768130567115, 0.7291065797294590256, 1.457975083082104995 ),
 .UNSPECIFIED. ) ;
#63508 = DIRECTION ( 'NONE',  ( 0.000000000000000000, 0.000000000000000000, 1.000000000000000000 ) ) ;
#63511 = LINE ( 'NONE', #4806, #26127 ) ;
#63510 = AXIS2_PLACEMENT_3D ( 'NONE', #68148, #56482, #3103 ) ;
#63512 = EDGE_CURVE ( 'NONE', #51301, #45555, #42641, .T. ) ;
#63513 = LINE ( 'NONE', #69503, #58413 ) ;
#63514 = ORIENTED_EDGE ( 'NONE', *, *, #28525, .F. ) ;
#63515 = ORIENTED_EDGE ( 'NONE', *, *, #18726, .F. ) ;
#63516 = VECTOR ( 'NONE', #37796, 1000.000000000000000 ) ;
#63517 = CARTESIAN_POINT ( 'NONE',  ( 75.42576880091937142, 10.00000000000000000, 285.9830310981789125 ) ) ;
#63518 = EDGE_CURVE ( 'NONE', #1406, #8462, #26734, .T. ) ;
#63519 = DIRECTION ( 'NONE',  ( 0.000000000000000000, 0.000000000000000000, 1.000000000000000000 ) ) ;
#63520 = VERTEX_POINT ( 'NONE', #47947 ) ;
#63521 = ADVANCED_FACE ( 'NONE', ( #4476 ), #26041, .T. ) ;
#63522 = FACE_OUTER_BOUND ( 'NONE', #34135, .T. ) ;
#63523 = CARTESIAN_POINT ( 'NONE',  ( 10.31452373788281562, -3.857023737882814718, 26.00000000000000711 ) ) ;
#63524 = PLANE ( 'NONE',  #58168 ) ;
#63525 = VERTEX_POINT ( 'NONE', #32723 ) ;
#63526 = CARTESIAN_POINT ( 'NONE',  ( 7.250000000000005329, -8.249999999999998224, -26.00000000000001066 ) ) ;
#63527 = CARTESIAN_POINT ( 'NONE',  ( 7.000000000000000000, -30.45000000000000639, 15.00000000000000000 ) ) ;
#63528 = CARTESIAN_POINT ( 'NONE',  ( -10.08346604330787777, 9.093516549646603053, 455.0000000000000568 ) ) ;
#63529 = CARTESIAN_POINT ( 'NONE',  ( -24.00000000000000000, -16.64230188589299786, -14.64519951917100116 ) ) ;
#63530 = VECTOR ( 'NONE', #27446, 1000.000000000000000 ) ;
#63531 = EDGE_CURVE ( 'NONE', #64467, #55374, #12134, .T. ) ;
#63532 = CARTESIAN_POINT ( 'NONE',  ( -11.75000000000000000, -5.200000000000001066, 26.25000000000000000 ) ) ;
#63533 = ORIENTED_EDGE ( 'NONE', *, *, #37344, .F. ) ;
#63534 = DIRECTION ( 'NONE',  ( 1.000000000000000000, 0.000000000000000000, 0.000000000000000000 ) ) ;
#63535 = FACE_OUTER_BOUND ( 'NONE', #6691, .T. ) ;
#63536 = LINE ( 'NONE', #63172, #10715 ) ;
#63537 = FACE_OUTER_BOUND ( 'NONE', #33452, .T. ) ;
#63538 = ORIENTED_EDGE ( 'NONE', *, *, #10214, .T. ) ;
#63539 = DIRECTION ( 'NONE',  ( 0.000000000000000000, 0.000000000000000000, -1.000000000000000000 ) ) ;
#63540 = LINE ( 'NONE', #53290, #13872 ) ;
#63541 = VECTOR ( 'NONE', #35363, 1000.000000000000000 ) ;
#63542 = FACE_BOUND ( 'NONE', #3084, .T. ) ;
#63543 = DIRECTION ( 'NONE',  ( 1.000000000000000000, 0.000000000000000000, 0.000000000000000000 ) ) ;
#63544 = VERTEX_POINT ( 'NONE', #59255 ) ;
#63545 = LINE ( 'NONE', #25721, #68180 ) ;
#63546 = DIRECTION ( 'NONE',  ( -1.000000000000000000, 0.000000000000000000, 0.000000000000000000 ) ) ;
#63547 = LINE ( 'NONE', #8376, #25564 ) ;
#63548 = CARTESIAN_POINT ( 'NONE',  ( 8.900000000000002132, 21.00000000000000000, 18.00000000000000355 ) ) ;
#63549 = LINE ( 'NONE', #31013, #56953 ) ;
#63550 = CARTESIAN_POINT ( 'NONE',  ( 47.00000000000000000, 0.000000000000000000, 0.000000000000000000 ) ) ;
#63551 = CYLINDRICAL_SURFACE ( 'NONE', #33898, 0.3500000000009988455 ) ;
#63552 = ORIENTED_EDGE ( 'NONE', *, *, #35873, .T. ) ;
#63553 = EDGE_CURVE ( 'NONE', #14970, #21232, #48997, .T. ) ;
#63554 = VECTOR ( 'NONE', #23460, 1000.000000000000000 ) ;
#63555 = VERTEX_POINT ( 'NONE', #42986 ) ;
#63556 = DIRECTION ( 'NONE',  ( 0.000000000000000000, 0.000000000000000000, 1.000000000000000000 ) ) ;
#63557 = CARTESIAN_POINT ( 'NONE',  ( -8.689999999999999503, 9.750000000000000000, -5.000000000000000000 ) ) ;
#63558 = ORIENTED_EDGE ( 'NONE', *, *, #986, .T. ) ;
#63559 = EDGE_CURVE ( 'NONE', #33326, #57065, #14422, .T. ) ;
#63560 = CARTESIAN_POINT ( 'NONE',  ( -15.50000000000000000, -5.000000000000000000, 22.50000000000000000 ) ) ;
#63561 = AXIS2_PLACEMENT_3D ( 'NONE', #21098, #15788, #55360 ) ;
#63562 = DIRECTION ( 'NONE',  ( -1.000000000000000000, 0.000000000000000000, 0.000000000000000000 ) ) ;
#63563 = EDGE_CURVE ( 'NONE', #20828, #64072, #214, .T. ) ;
#63564 = ORIENTED_EDGE ( 'NONE', *, *, #49640, .T. ) ;
#63565 = DIRECTION ( 'NONE',  ( -0.000000000000000000, -0.000000000000000000, -1.000000000000000000 ) ) ;
#63566 = ORIENTED_EDGE ( 'NONE', *, *, #61939, .F. ) ;
#63567 = VECTOR ( 'NONE', #30733, 1000.000000000000000 ) ;
#63568 = EDGE_CURVE ( 'NONE', #86, #25606, #67952, .T. ) ;
#63569 = ORIENTED_EDGE ( 'NONE', *, *, #22526, .F. ) ;
#63570 = DIRECTION ( 'NONE',  ( -0.7071067811865503483, -0.7071067811865446862, 0.000000000000000000 ) ) ;
#63571 = ORIENTED_EDGE ( 'NONE', *, *, #7343, .F. ) ;
#63572 = DIRECTION ( 'NONE',  ( 9.912705577010336396E-15, 1.000000000000000000, 0.000000000000000000 ) ) ;
#63573 = CARTESIAN_POINT ( 'NONE',  ( 9.804883450353379715, -11.08848345035349325, 455.0000000000000568 ) ) ;
#63574 = PLANE ( 'NONE',  #5064 ) ;
#63575 = AXIS2_PLACEMENT_3D ( 'NONE', #38632, #18079, #33323 ) ;
#63576 = ORIENTED_EDGE ( 'NONE', *, *, #30682, .F. ) ;
#63577 = CARTESIAN_POINT ( 'NONE',  ( -7.393516549646710345, 5.993516549646603409, 455.0000000000000568 ) ) ;
#63579 = CARTESIAN_POINT ( 'NONE',  ( -5.655420232009250370, 8.393516549646600211, 195.0000000000000284 ) ) ;
#63578 = DIRECTION ( 'NONE',  ( 0.000000000000000000, 0.000000000000000000, -1.000000000000000000 ) ) ;
#63580 = ORIENTED_EDGE ( 'NONE', *, *, #33711, .T. ) ;
#63581 = ORIENTED_EDGE ( 'NONE', *, *, #21558, .F. ) ;
#63582 = AXIS2_PLACEMENT_3D ( 'NONE', #12128, #1518, #6820 ) ;
#63583 = ORIENTED_EDGE ( 'NONE', *, *, #6570, .F. ) ;
#63584 = EDGE_CURVE ( 'NONE', #47821, #25376, #29407, .T. ) ;
#63586 = ORIENTED_EDGE ( 'NONE', *, *, #6335, .F. ) ;
#63585 = CONTEXT_DEPENDENT_SHAPE_REPRESENTATION ( #5646, #60623 ) ;
#63587 = LINE ( 'NONE', #16534, #42392 ) ;
#63588 = VECTOR ( 'NONE', #62877, 1000.000000000000114 ) ;
#63590 = ORIENTED_EDGE ( 'NONE', *, *, #65234, .T. ) ;
#63589 = CARTESIAN_POINT ( 'NONE',  ( 4.456444791733522252E-16, 7.450000000000002842, -25.00000000000000000 ) ) ;
#63591 = DIRECTION ( 'NONE',  ( -0.7671651518153038696, 0.6414496315691526895, -2.309356642089022458E-17 ) ) ;
#63592 = PLANE ( 'NONE',  #40744 ) ;
#63593 = ORIENTED_EDGE ( 'NONE', *, *, #27414, .T. ) ;
#63594 = ORIENTED_EDGE ( 'NONE', *, *, #40978, .F. ) ;
#63595 = CIRCLE ( 'NONE', #29696, 2.458500000000000796 ) ;
#63596 = CARTESIAN_POINT ( 'NONE',  ( -5.242976262117259978, 5.242976262117182706, 54.00000000000000711 ) ) ;
#63597 = ORIENTED_EDGE ( 'NONE', *, *, #37452, .F. ) ;
#63598 = CYLINDRICAL_SURFACE ( 'NONE', #56205, 0.1999999999999987899 ) ;
#63599 = DIRECTION ( 'NONE',  ( -0.7671651518153105309, 0.6414496315691445849, 2.356647714346206145E-16 ) ) ;
#63600 = LINE ( 'NONE', #55001, #28335 ) ;
#63601 = ADVANCED_FACE ( 'NONE', ( #13145 ), #50634, .F. ) ;
#63602 = ORIENTED_EDGE ( 'NONE', *, *, #33695, .F. ) ;
#63603 = ADVANCED_FACE ( 'NONE', ( #7491 ), #61221, .T. ) ;
#63604 = AXIS2_PLACEMENT_3D ( 'NONE', #6756, #28325, #49895 ) ;
#63605 =( NAMED_UNIT ( * ) SI_UNIT ( $, .STERADIAN. ) SOLID_ANGLE_UNIT ( ) );
#63606 = DIRECTION ( 'NONE',  ( 1.000000000000000000, -0.000000000000000000, -0.000000000000000000 ) ) ;
#63609 = EDGE_LOOP ( 'NONE', ( #61745, #38011, #55521, #20365 ) ) ;
#63608 = EDGE_CURVE ( 'NONE', #21794, #35470, #19499, .T. ) ;
#63607 = DIRECTION ( 'NONE',  ( 0.000000000000000000, -1.000000000000000000, 0.000000000000000000 ) ) ;
#63611 = VERTEX_POINT ( 'NONE', #51695 ) ;
#63610 = CYLINDRICAL_SURFACE ( 'NONE', #25294, 0.1749999999999998224 ) ;
#63613 = DIRECTION ( 'NONE',  ( 3.717264591378875951E-15, 1.000000000000000000, 0.000000000000000000 ) ) ;
#63612 = AXIS2_PLACEMENT_3D ( 'NONE', #50580, #56230, #7774 ) ;
#63614 = AXIS2_PLACEMENT_3D ( 'NONE', #69888, #9450, #21451 ) ;
#63615 = LINE ( 'NONE', #34964, #63483 ) ;
#63616 = DIRECTION ( 'NONE',  ( -1.000000000000000000, 0.000000000000000000, 0.000000000000000000 ) ) ;
#63617 = CARTESIAN_POINT ( 'NONE',  ( 11.90000000000000036, -0.2000000000089119934, -8.913009219568841313E-12 ) ) ;
#63618 = VECTOR ( 'NONE', #43072, 999.9999999999998863 ) ;
#63619 = VECTOR ( 'NONE', #35223, 1000.000000000000000 ) ;
#63620 = CARTESIAN_POINT ( 'NONE',  ( 23.48000000000000043, -17.50000000000000000, 26.00000000000000355 ) ) ;
#63621 = ORIENTED_EDGE ( 'NONE', *, *, #56288, .T. ) ;
#63622 = LINE ( 'NONE', #25430, #41419 ) ;
#63623 = DIRECTION ( 'NONE',  ( 1.000000000000000000, -0.000000000000000000, -0.000000000000000000 ) ) ;
#63624 =( LENGTH_UNIT ( ) NAMED_UNIT ( * ) SI_UNIT ( .MILLI., .METRE. ) );
#63626 = ORIENTED_EDGE ( 'NONE', *, *, #5352, .F. ) ;
#63625 = LINE ( 'NONE', #59004, #38999 ) ;
#63627 = CARTESIAN_POINT ( 'NONE',  ( -4.393516549646784952, -11.32648345035339510, 195.0000000000000284 ) ) ;
#63628 = DIRECTION ( 'NONE',  ( -1.000000000000000000, 0.000000000000000000, 0.000000000000000000 ) ) ;
#63629 = CARTESIAN_POINT ( 'NONE',  ( 9.737023737882777752, 3.667976262117157660, 26.00000000000000711 ) ) ;
#63630 = ORIENTED_EDGE ( 'NONE', *, *, #58427, .T. ) ;
#63631 = FACE_OUTER_BOUND ( 'NONE', #25475, .T. ) ;
#63632 = CARTESIAN_POINT ( 'NONE',  ( 275.0000000000000000, -25.93000000000544958, 9.412893218815410634 ) ) ;
#63633 = AXIS2_PLACEMENT_3D ( 'NONE', #38254, #64094, #21637 ) ;
#63634 = ORIENTED_EDGE ( 'NONE', *, *, #60842, .T. ) ;
#63635 = LINE ( 'NONE', #69280, #33352 ) ;
#63636 = DIRECTION ( 'NONE',  ( 0.000000000000000000, -1.000000000000000000, -0.000000000000000000 ) ) ;
#63637 = VECTOR ( 'NONE', #3092, 1000.000000000000000 ) ;
#63638 = CARTESIAN_POINT ( 'NONE',  ( 8.250000000000005329, -8.249999999999998224, -26.00000000000001066 ) ) ;
#63639 = ADVANCED_FACE ( 'NONE', ( #2194 ), #24103, .F. ) ;
#63640 = FACE_OUTER_BOUND ( 'NONE', #11902, .T. ) ;
#63641 = ORIENTED_EDGE ( 'NONE', *, *, #33208, .F. ) ;
#63642 = ORIENTED_EDGE ( 'NONE', *, *, #65404, .F. ) ;
#63643 = DIRECTION ( 'NONE',  ( 0.000000000000000000, 0.000000000000000000, 1.000000000000000000 ) ) ;
#63644 = ORIENTED_EDGE ( 'NONE', *, *, #67640, .T. ) ;
#63645 = ORIENTED_EDGE ( 'NONE', *, *, #58817, .T. ) ;
#63646 = VECTOR ( 'NONE', #3702, 1000.000000000000000 ) ;
#63647 = ADVANCED_FACE ( 'NONE', ( #54652 ), #23762, .F. ) ;
#63648 = LINE ( 'NONE', #52334, #965 ) ;
#63649 = EDGE_CURVE ( 'NONE', #30178, #34012, #16873, .T. ) ;
#63650 = EDGE_CURVE ( 'NONE', #46397, #51774, #22482, .T. ) ;
#63651 = DIRECTION ( 'NONE',  ( 0.000000000000000000, 1.000000000000000000, 0.000000000000000000 ) ) ;
#63652 = PLANE ( 'NONE',  #57000 ) ;
#63653 = ORIENTED_EDGE ( 'NONE', *, *, #56120, .T. ) ;
#63654 = EDGE_CURVE ( 'NONE', #46800, #14694, #37181, .T. ) ;
#63655 = VERTEX_POINT ( 'NONE', #35056 ) ;
#63656 = EDGE_CURVE ( 'NONE', #13045, #36255, #6662, .T. ) ;
#63657 = FACE_OUTER_BOUND ( 'NONE', #25457, .T. ) ;
#63658 = ORIENTED_EDGE ( 'NONE', *, *, #33948, .F. ) ;
#63659 = EDGE_LOOP ( 'NONE', ( #5842, #27958, #8053, #9045 ) ) ;
#63660 = DIRECTION ( 'NONE',  ( 0.000000000000000000, 0.000000000000000000, 1.000000000000000000 ) ) ;
#63661 = DIRECTION ( 'NONE',  ( 1.000000000000000000, 0.000000000000000000, 0.000000000000000000 ) ) ;
#63662 = AXIS2_PLACEMENT_3D ( 'NONE', #25536, #47438, #14561 ) ;
#63663 = VECTOR ( 'NONE', #964, 1000.000000000000000 ) ;
#63664 = LINE ( 'NONE', #14868, #19667 ) ;
#63665 = ADVANCED_FACE ( 'NONE', ( #1849 ), #2887, .T. ) ;
#63666 = EDGE_LOOP ( 'NONE', ( #17888, #39712, #68182, #10379 ) ) ;
#63667 = AXIS2_PLACEMENT_3D ( 'NONE', #323, #61819, #54078 ) ;
#63668 = DIRECTION ( 'NONE',  ( -1.000000000000000000, 0.000000000000000000, -0.000000000000000000 ) ) ;
#63670 = DIRECTION ( 'NONE',  ( 0.7671651518152985405, 0.6414496315691592399, -2.309356642088639737E-17 ) ) ;
#63669 = CARTESIAN_POINT ( 'NONE',  ( 6.364920264886885448, -6.836383711243021466, 54.00000000000000711 ) ) ;
#63671 = AXIS2_PLACEMENT_3D ( 'NONE', #18927, #41181, #18216 ) ;
#63673 = VERTEX_POINT ( 'NONE', #13848 ) ;
#63672 = VECTOR ( 'NONE', #26975, 1000.000000000000000 ) ;
#63675 = EDGE_LOOP ( 'NONE', ( #51070, #6941, #58477, #47807 ) ) ;
#63674 = CARTESIAN_POINT ( 'NONE',  ( 280.0000000000000000, -25.60000000000000142, 20.00000000000000000 ) ) ;
#63676 = VERTEX_POINT ( 'NONE', #46030 ) ;
#63677 = VECTOR ( 'NONE', #66242, 1000.000000000000000 ) ;
#63678 = AXIS2_PLACEMENT_3D ( 'NONE', #2515, #40348, #61915 ) ;
#63679 = CARTESIAN_POINT ( 'NONE',  ( 11.32648345035340576, 7.793516549646564151, 455.0000000000000568 ) ) ;
#63680 = DIRECTION ( 'NONE',  ( 0.000000000000000000, 0.000000000000000000, 1.000000000000000000 ) ) ;
#63681 = ORIENTED_EDGE ( 'NONE', *, *, #68032, .F. ) ;
#63682 = CARTESIAN_POINT ( 'NONE',  ( 9.795823737882805915, -9.795823737882802362, 26.00000000000000000 ) ) ;
#63683 = LINE ( 'NONE', #19133, #28842 ) ;
#63684 = ORIENTED_EDGE ( 'NONE', *, *, #41234, .F. ) ;
#63685 = VERTEX_POINT ( 'NONE', #23422 ) ;
#63686 = DIRECTION ( 'NONE',  ( 0.000000000000000000, 0.000000000000000000, -1.000000000000000000 ) ) ;
#63687 = DIRECTION ( 'NONE',  ( 1.000000000000000000, -2.309061475090597584E-14, 1.836970198720987533E-16 ) ) ;
#63688 = ORIENTED_EDGE ( 'NONE', *, *, #26377, .F. ) ;
#63689 = EDGE_CURVE ( 'NONE', #14272, #6091, #43965, .T. ) ;
#63690 = LINE ( 'NONE', #31520, #54971 ) ;
#63691 = CARTESIAN_POINT ( 'NONE',  ( 39.00000000000000000, -21.00000000000000000, -16.96999999999999886 ) ) ;
#63694 = EDGE_LOOP ( 'NONE', ( #72, #13461, #42930, #7523, #30803, #27257, #6700, #66666 ) ) ;
#63693 = ADVANCED_FACE ( 'NONE', ( #44975 ), #62282, .F. ) ;
#63692 = SURFACE_SIDE_STYLE ('',( #35392 ) ) ;
#63696 = ORIENTED_EDGE ( 'NONE', *, *, #65796, .F. ) ;
#63695 = DIRECTION ( 'NONE',  ( -0.000000000000000000, -0.000000000000000000, 1.000000000000000000 ) ) ;
#63697 = EDGE_CURVE ( 'NONE', #10069, #65486, #68812, .T. ) ;
#63698 = DIRECTION ( 'NONE',  ( 0.7071067811865560104, 8.659560562354830553E-17, 0.7071067811865391350 ) ) ;
#63699 = CARTESIAN_POINT ( 'NONE',  ( 7.250000000000005329, 8.250000000000001776, -14.50000000000000000 ) ) ;
#63700 = PLANE ( 'NONE',  #33518 ) ;
#63701 = CARTESIAN_POINT ( 'NONE',  ( 25.50000000000000355, -15.12100000000000044, 20.87900000000000134 ) ) ;
#63702 = EDGE_CURVE ( 'NONE', #25592, #40341, #18097, .T. ) ;
#63703 = DIRECTION ( 'NONE',  ( 0.000000000000000000, 0.000000000000000000, 1.000000000000000000 ) ) ;
#63704 = DIRECTION ( 'NONE',  ( 1.000000000000000000, -1.047444401652940007E-14, 1.836970198721010706E-16 ) ) ;
#63705 = VERTEX_POINT ( 'NONE', #52759 ) ;
#63706 = LINE ( 'NONE', #25876, #23644 ) ;
#63708 = ORIENTED_EDGE ( 'NONE', *, *, #27174, .F. ) ;
#63707 = DIRECTION ( 'NONE',  ( -0.000000000000000000, -0.000000000000000000, -1.000000000000000000 ) ) ;
#63709 = FACE_OUTER_BOUND ( 'NONE', #32883, .T. ) ;
#63710 = VECTOR ( 'NONE', #14838, 1000.000000000000000 ) ;
#63711 = VECTOR ( 'NONE', #1544, 1000.000000000000000 ) ;
#63712 = DIRECTION ( 'NONE',  ( -1.000000000000000000, 0.000000000000000000, 0.000000000000000000 ) ) ;
#63713 = LINE ( 'NONE', #50720, #3755 ) ;
#63714 = DIRECTION ( 'NONE',  ( 0.000000000000000000, 0.000000000000000000, 1.000000000000000000 ) ) ;
#63715 = AXIS2_PLACEMENT_3D ( 'NONE', #17495, #45057, #24200 ) ;
#63716 = ORIENTED_EDGE ( 'NONE', *, *, #43010, .F. ) ;
#63717 = CARTESIAN_POINT ( 'NONE',  ( 3.664523737882819709, 10.30047626211720413, 54.00000000000000711 ) ) ;
#63718 = CARTESIAN_POINT ( 'NONE',  ( 41.09999999999999432, -14.06939075806900163, 20.80000000000000426 ) ) ;
#63719 = ORIENTED_EDGE ( 'NONE', *, *, #46226, .T. ) ;
#63720 = CARTESIAN_POINT ( 'NONE',  ( -7.342976262117282715, -5.552858015815545834, 54.00000000000000711 ) ) ;
#63721 = AXIS2_PLACEMENT_3D ( 'NONE', #57643, #35720, #26178 ) ;
#63722 = DIRECTION ( 'NONE',  ( 1.000000000000000000, -0.000000000000000000, 0.000000000000000000 ) ) ;
#63723 = VECTOR ( 'NONE', #56798, 1000.000000000000000 ) ;
#63724 = EDGE_CURVE ( 'NONE', #18134, #61969, #10304, .T. ) ;
#63725 = PLANE ( 'NONE',  #69204 ) ;
#63726 = ORIENTED_EDGE ( 'NONE', *, *, #21484, .F. ) ;
#63727 = FACE_OUTER_BOUND ( 'NONE', #11542, .T. ) ;
#63728 = ORIENTED_EDGE ( 'NONE', *, *, #60978, .T. ) ;
#63729 = VERTEX_POINT ( 'NONE', #15621 ) ;
#63730 = DIRECTION ( 'NONE',  ( 1.000000000000000000, -0.000000000000000000, 0.000000000000000000 ) ) ;
#63731 = PLANE ( 'NONE',  #61321 ) ;
#63732 = LINE ( 'NONE', #59721, #46909 ) ;
#63733 = CARTESIAN_POINT ( 'NONE',  ( -5.779227145995285753, 6.344366288193340253, 54.00000000000000711 ) ) ;
#63734 = CARTESIAN_POINT ( 'NONE',  ( 7.249999999999995559, -7.848062532927998269, -5.000000000000000000 ) ) ;
#63735 = EDGE_LOOP ( 'NONE', ( #58768, #50941, #41439, #19927 ) ) ;
#63736 = ORIENTED_EDGE ( 'NONE', *, *, #16461, .T. ) ;
#63737 = EDGE_CURVE ( 'NONE', #67553, #68804, #47774, .T. ) ;
#63739 = EDGE_LOOP ( 'NONE', ( #60946, #23965, #16242, #31254, #69057, #6076 ) ) ;
#63738 = CYLINDRICAL_SURFACE ( 'NONE', #37415, 3.499999999999999556 ) ;
#63740 = EDGE_LOOP ( 'NONE', ( #10055, #13028, #19890, #18418, #66407, #69479, #7003, #22799 ) ) ;
#63741 = DIRECTION ( 'NONE',  ( -1.000000000000000000, 0.000000000000000000, 0.000000000000000000 ) ) ;
#63742 = CARTESIAN_POINT ( 'NONE',  ( -8.250000000000001776, 0.000000000000000000, -14.50000000000000000 ) ) ;
#63743 = EDGE_CURVE ( 'NONE', #64507, #49054, #25523, .T. ) ;
#63744 = CARTESIAN_POINT ( 'NONE',  ( 10.09643294401454661, -9.106483450353398013, 195.0000000000000284 ) ) ;
#63745 = AXIS2_PLACEMENT_3D ( 'NONE', #28059, #59544, #493 ) ;
#63746 = DIRECTION ( 'NONE',  ( 1.000000000000000000, -5.981805089575194965E-17, 0.000000000000000000 ) ) ;
#63748 = CARTESIAN_POINT ( 'NONE',  ( 7.250000000000005329, 8.250000000000001776, -26.00000000000001066 ) ) ;
#63747 = DIRECTION ( 'NONE',  ( 0.000000000000000000, 0.000000000000000000, 1.000000000000000000 ) ) ;
#63749 = ORIENTED_EDGE ( 'NONE', *, *, #9106, .F. ) ;
#63750 = VECTOR ( 'NONE', #13780, 1000.000000000000000 ) ;
#63751 = ORIENTED_EDGE ( 'NONE', *, *, #61457, .F. ) ;
#63752 = VERTEX_POINT ( 'NONE', #53443 ) ;
#63753 = DIRECTION ( 'NONE',  ( -0.000000000000000000, -0.000000000000000000, -1.000000000000000000 ) ) ;
#63754 = LINE ( 'NONE', #24521, #3891 ) ;
#63755 =( NAMED_UNIT ( * ) SI_UNIT ( $, .STERADIAN. ) SOLID_ANGLE_UNIT ( ) );
#63756 = EDGE_CURVE ( 'NONE', #42484, #35695, #21272, .T. ) ;
#63757 = VECTOR ( 'NONE', #27448, 1000.000000000000000 ) ;
#63759 = PLANE ( 'NONE',  #13929 ) ;
#63758 = VECTOR ( 'NONE', #31927, 1000.000000000000000 ) ;
#63760 = ORIENTED_EDGE ( 'NONE', *, *, #34401, .T. ) ;
#63761 = ORIENTED_EDGE ( 'NONE', *, *, #1288, .T. ) ;
#63762 = ORIENTED_EDGE ( 'NONE', *, *, #31898, .T. ) ;
#63763 = LINE ( 'NONE', #30179, #21525 ) ;
#63764 = ORIENTED_EDGE ( 'NONE', *, *, #35587, .T. ) ;
#63765 = AXIS2_PLACEMENT_3D ( 'NONE', #28316, #6746, #16690 ) ;
#63766 = CIRCLE ( 'NONE', #61448, 4.000000000000000000 ) ;
#63767 = CARTESIAN_POINT ( 'NONE',  ( -11.00000000000000000, -14.04000000000000092, 14.80000000000000071 ) ) ;
#63768 = ORIENTED_EDGE ( 'NONE', *, *, #29347, .F. ) ;
#63769 = ORIENTED_EDGE ( 'NONE', *, *, #32837, .T. ) ;
#63770 = LINE ( 'NONE', #59505, #5722 ) ;
#63771 = VECTOR ( 'NONE', #25040, 1000.000000000000000 ) ;
#63773 = ORIENTED_EDGE ( 'NONE', *, *, #57970, .T. ) ;
#63772 = DIRECTION ( 'NONE',  ( -1.280238727658158235E-15, -1.000000000000000000, 0.000000000000000000 ) ) ;
#63774 = ORIENTED_EDGE ( 'NONE', *, *, #40814, .F. ) ;
#63775 = DIRECTION ( 'NONE',  ( 0.000000000000000000, -0.9938079899998859545, -0.1111111111112941946 ) ) ;
#63776 = LINE ( 'NONE', #52111, #4250 ) ;
#63779 = VERTEX_POINT ( 'NONE', #9608 ) ;
#63778 = EDGE_CURVE ( 'NONE', #1459, #54522, #47352, .T. ) ;
#63777 = CARTESIAN_POINT ( 'NONE',  ( -9.689726262117227762, 8.566576262117216345, 26.00000000000000711 ) ) ;
#63780 = CIRCLE ( 'NONE', #52470, 4.500000000000190958 ) ;
#63781 = EDGE_LOOP ( 'NONE', ( #34952, #39100, #64143, #10018, #22873, #58796, #16441, #38530, #59199, #30875 ) ) ;
#63782 = DIRECTION ( 'NONE',  ( 0.000000000000000000, 1.000000000000000000, 0.000000000000000000 ) ) ;
#63783 = DIRECTION ( 'NONE',  ( 0.000000000000000000, 1.000000000000000000, 0.000000000000000000 ) ) ;
#63784 = CARTESIAN_POINT ( 'NONE',  ( 6.006483450353379716, -8.211283450353491276, 455.0000000000000568 ) ) ;
#63785 = LINE ( 'NONE', #15340, #33459 ) ;
#63786 = EDGE_CURVE ( 'NONE', #37400, #27400, #41421, .T. ) ;
#63787 = DIRECTION ( 'NONE',  ( -0.7071067811865515695, -0.7071067811865435759, 0.000000000000000000 ) ) ;
#63788 = VERTEX_POINT ( 'NONE', #62997 ) ;
#63789 = FACE_OUTER_BOUND ( 'NONE', #32877, .T. ) ;
#63790 = ORIENTED_EDGE ( 'NONE', *, *, #3528, .T. ) ;
#63791 = DIRECTION ( 'NONE',  ( 0.000000000000000000, 1.000000000000000000, 0.000000000000000000 ) ) ;
#63792 = CARTESIAN_POINT ( 'NONE',  ( 9.247904806590689475, -9.955011587777349291, 455.0000000000000568 ) ) ;
#63793 = LINE ( 'NONE', #9703, #56219 ) ;
#63794 = FACE_OUTER_BOUND ( 'NONE', #22661, .T. ) ;
#63795 = FACE_OUTER_BOUND ( 'NONE', #69504, .T. ) ;
#63796 = AXIS2_PLACEMENT_3D ( 'NONE', #12977, #61073, #34555 ) ;
#63797 = EDGE_LOOP ( 'NONE', ( #59788, #47959, #60175, #17078 ) ) ;
#63798 = EDGE_CURVE ( 'NONE', #29489, #29928, #30464, .T. ) ;
#63799 = CYLINDRICAL_SURFACE ( 'NONE', #22354, 0.5000000000009284795 ) ;
#63800 = DIRECTION ( 'NONE',  ( -0.8660254037844322683, 0.5000000000000111022, 0.000000000000000000 ) ) ;
#63801 = VECTOR ( 'NONE', #9972, 1000.000000000000000 ) ;
#63802 = CARTESIAN_POINT ( 'NONE',  ( 7.250000000000005329, 7.250000000000000888, -26.00000000000001066 ) ) ;
#63803 = ORIENTED_EDGE ( 'NONE', *, *, #2175, .T. ) ;
#63804 = DIRECTION ( 'NONE',  ( -1.000000000000000000, 0.000000000000000000, 0.000000000000000000 ) ) ;
#63805 = DIRECTION ( 'NONE',  ( -0.000000000000000000, -0.000000000000000000, -1.000000000000000000 ) ) ;
#63806 = DIRECTION ( 'NONE',  ( 0.000000000000000000, 1.000000000000000000, 0.000000000000000000 ) ) ;
#63807 = DIRECTION ( 'NONE',  ( -1.000000000000000000, 0.000000000000000000, 0.000000000000000000 ) ) ;
#63808 = CYLINDRICAL_SURFACE ( 'NONE', #50025, 3.499999999999055866 ) ;
#63809 = MECHANICAL_DESIGN_GEOMETRIC_PRESENTATION_REPRESENTATION (  '', ( #64915 ), #34391 ) ;
#63810 = ORIENTED_EDGE ( 'NONE', *, *, #60758, .T. ) ;
#63811 = CARTESIAN_POINT ( 'NONE',  ( 10.90000000000000036, -14.06939075806900874, 20.80000000000001137 ) ) ;
#63812 = DIRECTION ( 'NONE',  ( 1.000000000000000000, 0.000000000000000000, 0.000000000000000000 ) ) ;
#63813 = CARTESIAN_POINT ( 'NONE',  ( 16.89194109070750116, -5.000000000000000000, -26.25000000000000000 ) ) ;
#63814 = CARTESIAN_POINT ( 'NONE',  ( 283.0000000000000568, -30.80000000000000071, 12.20000000000000107 ) ) ;
#63815 = CARTESIAN_POINT ( 'NONE',  ( -9.690000000000001279, 9.690000000000001279, -5.000000000000000000 ) ) ;
#63816 = ORIENTED_EDGE ( 'NONE', *, *, #17453, .T. ) ;
#63818 = EDGE_LOOP ( 'NONE', ( #34323, #64613, #35747, #27589 ) ) ;
#63817 = LINE ( 'NONE', #37297, #31766 ) ;
#63819 = EDGE_CURVE ( 'NONE', #997, #28252, #4996, .T. ) ;
#63820 = CARTESIAN_POINT ( 'NONE',  ( -29.50000000000000355, -11.50000000000100009, 10.50000000000065903 ) ) ;
#63821 = EDGE_CURVE ( 'NONE', #24182, #62314, #28122, .T. ) ;
#63822 = CARTESIAN_POINT ( 'NONE',  ( 283.0000000000000568, -25.50000000000000355, 14.74860679774999994 ) ) ;
#63823 = CIRCLE ( 'NONE', #3960, 4.000000000000000000 ) ;
#63824 = CARTESIAN_POINT ( 'NONE',  ( 78.77321854994620765, 47.95351654967443977, 15.00000000000000000 ) ) ;
#63825 = ORIENTED_EDGE ( 'NONE', *, *, #36521, .F. ) ;
#63826 = EDGE_CURVE ( 'NONE', #53491, #40788, #26565, .T. ) ;
#63827 = AXIS2_PLACEMENT_3D ( 'NONE', #18806, #66886, #45668 ) ;
#63828 = CARTESIAN_POINT ( 'NONE',  ( 7.357023737882817827, -3.848229544836346605, 54.00000000000000711 ) ) ;
#63829 = EDGE_CURVE ( 'NONE', #10010, #10380, #20556, .T. ) ;
#63830 = ORIENTED_EDGE ( 'NONE', *, *, #39145, .T. ) ;
#63831 = ORIENTED_EDGE ( 'NONE', *, *, #62701, .T. ) ;
#63832 = ORIENTED_EDGE ( 'NONE', *, *, #5202, .F. ) ;
#63833 = EDGE_CURVE ( 'NONE', #64346, #20240, #8893, .T. ) ;
#63834 = CARTESIAN_POINT ( 'NONE',  ( 275.4999999999998863, -0.5000000000000781597, 27.00000000000004263 ) ) ;
#63835 = ADVANCED_FACE ( 'NONE', ( #52041 ), #68658, .T. ) ;
#63836 = DIRECTION ( 'NONE',  ( 1.000000000000000000, -0.000000000000000000, -0.000000000000000000 ) ) ;
#63837 = DIRECTION ( 'NONE',  ( 0.000000000000000000, 0.000000000000000000, -1.000000000000000000 ) ) ;
#63838 = ORIENTED_EDGE ( 'NONE', *, *, #57352, .F. ) ;
#63839 = ORIENTED_EDGE ( 'NONE', *, *, #53507, .F. ) ;
#63840 = LINE ( 'NONE', #10100, #36140 ) ;
#63841 = VERTEX_POINT ( 'NONE', #68298 ) ;
#63842 = VECTOR ( 'NONE', #53554, 1000.000000000000000 ) ;
#63843 = ORIENTED_EDGE ( 'NONE', *, *, #66446, .F. ) ;
#63844 = ORIENTED_EDGE ( 'NONE', *, *, #55078, .F. ) ;
#63845 = ORIENTED_EDGE ( 'NONE', *, *, #35031, .F. ) ;
#63846 = CIRCLE ( 'NONE', #13151, 24.99999999998789946 ) ;
#63847 = DIRECTION ( 'NONE',  ( 0.000000000000000000, -0.7278708115916125987, 0.6857142857145147596 ) ) ;
#63849 = ORIENTED_EDGE ( 'NONE', *, *, #51494, .T. ) ;
#63848 = CARTESIAN_POINT ( 'NONE',  ( -11.00000000000000000, -17.35230188589299871, 15.35019951917099945 ) ) ;
#63850 = PLANE ( 'NONE',  #728 ) ;
#63851 = AXIS2_PLACEMENT_3D ( 'NONE', #33054, #54640, #6188 ) ;
#63852 = AXIS2_PLACEMENT_3D ( 'NONE', #61864, #56554, #63266 ) ;
#63853 = VECTOR ( 'NONE', #48710, 1000.000000000000000 ) ;
#63854 = LINE ( 'NONE', #58194, #23885 ) ;
#63855 = EDGE_CURVE ( 'NONE', #8645, #13751, #20906, .T. ) ;
#63856 = DIRECTION ( 'NONE',  ( 1.000000000000000000, 0.000000000000000000, 0.000000000000000000 ) ) ;
#63857 = VERTEX_POINT ( 'NONE', #19850 ) ;
#63858 = VERTEX_POINT ( 'NONE', #20204 ) ;
#63859 = AXIS2_PLACEMENT_3D ( 'NONE', #60330, #33123, #39123 ) ;
#63860 = AXIS2_PLACEMENT_3D ( 'NONE', #60928, #66589, #49636 ) ;
#63861 = PLANE ( 'NONE',  #24371 ) ;
#63862 = CIRCLE ( 'NONE', #27768, 0.5249999999999990230 ) ;
#63863 = DIRECTION ( 'NONE',  ( -1.000000000000000000, 0.000000000000000000, 0.000000000000000000 ) ) ;
#63864 = EDGE_LOOP ( 'NONE', ( #6153, #6386 ) ) ;
#63865 = CARTESIAN_POINT ( 'NONE',  ( -5.242976262117259978, 5.242976262117182706, 26.00000000000000711 ) ) ;
#63866 = DIRECTION ( 'NONE',  ( -1.000000000000000000, 0.000000000000000000, 0.000000000000000000 ) ) ;
#63867 = FILL_AREA_STYLE_COLOUR ( '', #36719 ) ;
#63868 = ORIENTED_EDGE ( 'NONE', *, *, #54162, .F. ) ;
#63869 = VECTOR ( 'NONE', #32221, 1000.000000000000000 ) ;
#63870 = CARTESIAN_POINT ( 'NONE',  ( 9.841277389592701041, 2.277516549646538824, 455.0000000000000568 ) ) ;
#63871 = LINE ( 'NONE', #38054, #18870 ) ;
#63872 = DIRECTION ( 'NONE',  ( 0.000000000000000000, 0.000000000000000000, 1.000000000000000000 ) ) ;
#63873 = CYLINDRICAL_SURFACE ( 'NONE', #59575, 0.2000000000000005107 ) ;
#63874 = EDGE_CURVE ( 'NONE', #45978, #13397, #17959, .T. ) ;
#63875 = DIRECTION ( 'NONE',  ( -1.000000000000000000, 0.000000000000000000, 0.000000000000000000 ) ) ;
#63876 = ORIENTED_EDGE ( 'NONE', *, *, #14701, .F. ) ;
#63877 = LINE ( 'NONE', #15441, #64115 ) ;
#63878 = DIRECTION ( 'NONE',  ( 0.000000000000000000, 0.000000000000000000, -1.000000000000000000 ) ) ;
#63879 = CARTESIAN_POINT ( 'NONE',  ( -6.817976262117261044, 9.722976262117182245, 54.00000000000000711 ) ) ;
#63880 = PLANE ( 'NONE',  #49216 ) ;
#63881 = ORIENTED_EDGE ( 'NONE', *, *, #32797, .T. ) ;
#63882 = DIRECTION ( 'NONE',  ( 0.000000000000000000, 0.000000000000000000, 1.000000000000000000 ) ) ;
#63883 = EDGE_CURVE ( 'NONE', #14976, #18063, #49574, .T. ) ;
#63884 = FACE_OUTER_BOUND ( 'NONE', #43903, .T. ) ;
#63885 = PLANE ( 'NONE',  #34649 ) ;
#63886 = DIRECTION ( 'NONE',  ( 0.000000000000000000, 0.000000000000000000, 1.000000000000000000 ) ) ;
#63887 = ORIENTED_EDGE ( 'NONE', *, *, #46175, .T. ) ;
#63888 = DIRECTION ( 'NONE',  ( 0.000000000000000000, 0.000000000000000000, -1.000000000000000000 ) ) ;
#63889 = DIRECTION ( 'NONE',  ( 0.000000000000000000, 0.000000000000000000, -1.000000000000000000 ) ) ;
#63890 = ADVANCED_FACE ( 'NONE', ( #58034 ), #31184, .F. ) ;
#63891 = CIRCLE ( 'NONE', #62713, 0.5999999999999998668 ) ;
#63892 = EDGE_CURVE ( 'NONE', #15537, #29056, #57493, .T. ) ;
#63893 = DIRECTION ( 'NONE',  ( 0.000000000000000000, 0.000000000000000000, 1.000000000000000000 ) ) ;
#63894 = DIRECTION ( 'NONE',  ( 0.000000000000000000, -0.7046037717806115097, 0.7096009616626348659 ) ) ;
#63895 = CIRCLE ( 'NONE', #25486, 24.99999999998789946 ) ;
#63896 = DIRECTION ( 'NONE',  ( 0.8660254037850523279, 0.000000000000000000, 0.4999999999989371835 ) ) ;
#63897 = DIRECTION ( 'NONE',  ( 0.000000000000000000, 1.000000000000000000, 0.000000000000000000 ) ) ;
#63898 = ORIENTED_EDGE ( 'NONE', *, *, #14790, .T. ) ;
#63899 = VECTOR ( 'NONE', #50001, 1000.000000000000000 ) ;
#63900 = VECTOR ( 'NONE', #48664, 1000.000000000000000 ) ;
#63901 = VECTOR ( 'NONE', #32631, 1000.000000000000114 ) ;
#63902 = ORIENTED_EDGE ( 'NONE', *, *, #24112, .T. ) ;
#63903 = DIRECTION ( 'NONE',  ( -1.000000000000000000, 0.000000000000000000, 0.000000000000000000 ) ) ;
#63904 = EDGE_CURVE ( 'NONE', #53029, #27929, #54489, .T. ) ;
#63905 = LINE ( 'NONE', #68510, #2902 ) ;
#63906 = VERTEX_POINT ( 'NONE', #17327 ) ;
#63907 = LINE ( 'NONE', #58249, #28055 ) ;
#63908 = AXIS2_PLACEMENT_3D ( 'NONE', #40805, #45398, #2621 ) ;
#63909 = VECTOR ( 'NONE', #32767, 999.9999999999998863 ) ;
#63910 = CARTESIAN_POINT ( 'NONE',  ( 14.89999999999999680, -0.1999999999911430404, -8.864436962241481021E-12 ) ) ;
#63911 = ORIENTED_EDGE ( 'NONE', *, *, #25616, .F. ) ;
#63912 = VECTOR ( 'NONE', #46870, 1000.000000000000000 ) ;
#63913 = CARTESIAN_POINT ( 'NONE',  ( -7.450000000000001954, 0.000000000000000000, -12.50000000000000000 ) ) ;
#63914 = ORIENTED_EDGE ( 'NONE', *, *, #50547, .T. ) ;
#63915 = ORIENTED_EDGE ( 'NONE', *, *, #57958, .F. ) ;
#63917 = EDGE_CURVE ( 'NONE', #24393, #47170, #21612, .T. ) ;
#63916 = CARTESIAN_POINT ( 'NONE',  ( -11.29351654964668583, 8.513516549646642062, 194.9999952000000292 ) ) ;
#63918 = ORIENTED_EDGE ( 'NONE', *, *, #20801, .F. ) ;
#63919 = ADVANCED_FACE ( 'NONE', ( #64401 ), #49516, .F. ) ;
#63920 = PLANE ( 'NONE',  #5652 ) ;
#63921 = CARTESIAN_POINT ( 'NONE',  ( 41.09999999999999432, -21.00000000000000000, -13.86939075806900057 ) ) ;
#63922 = VECTOR ( 'NONE', #62121, 1000.000000000000000 ) ;
#63923 = CARTESIAN_POINT ( 'NONE',  ( 7.450000000000003730, -7.249999999999997335, -11.50000000000000000 ) ) ;
#63924 = ORIENTED_EDGE ( 'NONE', *, *, #60380, .F. ) ;
#63925 = ORIENTED_EDGE ( 'NONE', *, *, #11160, .T. ) ;
#63926 =( GEOMETRIC_REPRESENTATION_CONTEXT ( 3 ) GLOBAL_UNCERTAINTY_ASSIGNED_CONTEXT ( ( #20357 ) ) GLOBAL_UNIT_ASSIGNED_CONTEXT ( ( #63624, #37444, #16215 ) ) REPRESENTATION_CONTEXT ( 'NONE', 'WORKASPACE' ) );
#63927 = LINE ( 'NONE', #15491, #68450 ) ;
#63929 = CARTESIAN_POINT ( 'NONE',  ( -10.91351654964670637, 2.693516549646604030, 455.0000000000000568 ) ) ;
#63928 = DIRECTION ( 'NONE',  ( 0.000000000000000000, 0.000000000000000000, 1.000000000000000000 ) ) ;
#63930 = VERTEX_POINT ( 'NONE', #42820 ) ;
#63931 = EDGE_CURVE ( 'NONE', #28029, #20859, #6041, .T. ) ;
#63932 = ORIENTED_EDGE ( 'NONE', *, *, #29851, .F. ) ;
#63934 = ORIENTED_EDGE ( 'NONE', *, *, #8142, .T. ) ;
#63933 = CONTEXT_DEPENDENT_SHAPE_REPRESENTATION ( #15142, #48747 ) ;
#63935 = FACE_OUTER_BOUND ( 'NONE', #17751, .T. ) ;
#63937 = VERTEX_POINT ( 'NONE', #26920 ) ;
#63936 = CARTESIAN_POINT ( 'NONE',  ( 46.39999999999999858, 33.00000000000000000, -1.750000000000000222 ) ) ;
#63938 = CARTESIAN_POINT ( 'NONE',  ( 7.250000000000005329, 7.250000000000000888, -19.00000000000000000 ) ) ;
#63939 = DIRECTION ( 'NONE',  ( -1.000000000000000000, 0.000000000000000000, 0.000000000000000000 ) ) ;
#63940 = ORIENTED_EDGE ( 'NONE', *, *, #33156, .F. ) ;
#63941 = VECTOR ( 'NONE', #42567, 1000.000000000000114 ) ;
#63942 = ORIENTED_EDGE ( 'NONE', *, *, #50092, .F. ) ;
#63943 = CARTESIAN_POINT ( 'NONE',  ( 9.404523737882819034, -0.9555237378828154160, 26.00000000000000711 ) ) ;
#63944 = AXIS2_PLACEMENT_3D ( 'NONE', #49031, #592, #22161 ) ;
#63945 = EDGE_LOOP ( 'NONE', ( #13946, #34249, #28107, #54367 ) ) ;
#63946 = EDGE_CURVE ( 'NONE', #4452, #43025, #49856, .T. ) ;
#63947 = CARTESIAN_POINT ( 'NONE',  ( 30.00000000000000000, -12.00000000000000000, -10.20500000000000007 ) ) ;
#63948 = DIRECTION ( 'NONE',  ( -1.000000000000000000, 0.000000000000000000, 0.000000000000000000 ) ) ;
#63949 = AXIS2_PLACEMENT_3D ( 'NONE', #20546, #48470, #21258 ) ;
#63950 = CARTESIAN_POINT ( 'NONE',  ( 4.186483450353337687, -11.78648345035347589, 455.0000000000000568 ) ) ;
#63951 = ORIENTED_EDGE ( 'NONE', *, *, #5917, .T. ) ;
#63952 = ADVANCED_FACE ( 'NONE', ( #10638 ), #389, .F. ) ;
#63953 = CIRCLE ( 'NONE', #34595, 0.5249999999999990230 ) ;
#63954 = VECTOR ( 'NONE', #37541, 1000.000000000000000 ) ;
#63955 = CIRCLE ( 'NONE', #39103, 0.5000000000000000000 ) ;
#63956 = DIRECTION ( 'NONE',  ( -0.000000000000000000, -0.000000000000000000, 1.000000000000000000 ) ) ;
#63957 = CARTESIAN_POINT ( 'NONE',  ( 9.249999999999998224, 8.250000000000001776, 0.000000000000000000 ) ) ;
#63959 = ORIENTED_EDGE ( 'NONE', *, *, #5600, .F. ) ;
#63958 = CARTESIAN_POINT ( 'NONE',  ( -8.250000000000001776, -8.249999999999998224, -26.00000000000001066 ) ) ;
#63961 = VERTEX_POINT ( 'NONE', #16660 ) ;
#63960 = CARTESIAN_POINT ( 'NONE',  ( 7.900000000000000355, -21.00000000000000000, 18.00000000000000355 ) ) ;
#63962 = ADVANCED_FACE ( 'NONE', ( #49 ), #15958, .F. ) ;
#63963 = DIRECTION ( 'NONE',  ( 0.7071067811865441310, -0.7071067811865510144, -2.597868168706485034E-16 ) ) ;
#63964 = AXIS2_PLACEMENT_3D ( 'NONE', #41855, #3681, #16041 ) ;
#63965 = VECTOR ( 'NONE', #4364, 1000.000000000000000 ) ;
#63966 = AXIS2_PLACEMENT_3D ( 'NONE', #58367, #20170, #64025 ) ;
#63967 = DIRECTION ( 'NONE',  ( -1.000000000000000000, 0.000000000000000000, 0.000000000000000000 ) ) ;
#63968 = ADVANCED_FACE ( 'NONE', ( #1085, #59782 ), #27599, .T. ) ;
#63969 = CARTESIAN_POINT ( 'NONE',  ( 7.757955312929523117, -8.465062094116182934, 455.0000000000000568 ) ) ;
#63970 = CARTESIAN_POINT ( 'NONE',  ( -7.250000000000000888, 8.250000000000001776, -26.00000000000001066 ) ) ;
#63971 = AXIS2_PLACEMENT_3D ( 'NONE', #49839, #60438, #39225 ) ;
#63972 = EDGE_CURVE ( 'NONE', #29119, #68211, #745, .T. ) ;
#63973 = FACE_OUTER_BOUND ( 'NONE', #4948, .T. ) ;
#63974 = ORIENTED_EDGE ( 'NONE', *, *, #40364, .T. ) ;
#63975 = DIRECTION ( 'NONE',  ( 1.000000000000000000, -3.491481338843133355E-15, 0.000000000000000000 ) ) ;
#63976 = LINE ( 'NONE', #37788, #55315 ) ;
#63977 = DIRECTION ( 'NONE',  ( -0.5000000000000018874, -0.8660254037844374864, 0.000000000000000000 ) ) ;
#63979 = ORIENTED_EDGE ( 'NONE', *, *, #47846, .F. ) ;
#63978 = DIRECTION ( 'NONE',  ( 1.000000000000000000, 0.000000000000000000, 0.000000000000000000 ) ) ;
#63980 = AXIS2_PLACEMENT_3D ( 'NONE', #2973, #13924, #39737 ) ;
#63981 = FACE_OUTER_BOUND ( 'NONE', #36052, .T. ) ;
#63982 = CARTESIAN_POINT ( 'NONE',  ( 4.155633711806655306, 4.706725378239160484, 54.00000000000000711 ) ) ;
#63983 = ADVANCED_FACE ( 'NONE', ( #48483 ), #32217, .F. ) ;
#63984 = DIRECTION ( 'NONE',  ( 1.000000000000000000, 0.000000000000000000, 0.000000000000000000 ) ) ;
#63985 = ADVANCED_FACE ( 'NONE', ( #43164 ), #5703, .F. ) ;
#63986 = CARTESIAN_POINT ( 'NONE',  ( -11.50000000000000000, -11.50000000000100009, -15.00000000000084910 ) ) ;
#63987 = ORIENTED_EDGE ( 'NONE', *, *, #62706, .T. ) ;
#63988 = LINE ( 'NONE', #26491, #60293 ) ;
#63989 = DIRECTION ( 'NONE',  ( -0.000000000000000000, -0.000000000000000000, -1.000000000000000000 ) ) ;
#63990 = ORIENTED_EDGE ( 'NONE', *, *, #43843, .T. ) ;
#63991 = CARTESIAN_POINT ( 'NONE',  ( -4.141586236041100655, 5.779227145995200488, 54.00000000000000711 ) ) ;
#63992 = EDGE_CURVE ( 'NONE', #50235, #17310, #38564, .T. ) ;
#63993 = EDGE_CURVE ( 'NONE', #26623, #54084, #11668, .T. ) ;
#63994 = DIRECTION ( 'NONE',  ( -4.121462285523434951E-16, -1.000000000000000000, -0.000000000000000000 ) ) ;
#63995 = CARTESIAN_POINT ( 'NONE',  ( 2.005523737882813240, 8.598420958951633608, 54.00000000000000711 ) ) ;
#63996 = DIRECTION ( 'NONE',  ( 0.000000000000000000, 0.000000000000000000, -1.000000000000000000 ) ) ;
#63997 = EDGE_CURVE ( 'NONE', #37776, #29168, #33596, .T. ) ;
#63998 = FACE_OUTER_BOUND ( 'NONE', #18164, .T. ) ;
#63999 = ORIENTED_EDGE ( 'NONE', *, *, #22703, .F. ) ;
#64000 = ORIENTED_EDGE ( 'NONE', *, *, #909, .F. ) ;
#64001 = CARTESIAN_POINT ( 'NONE',  ( -9.547976262117254365, 2.355476262117183417, 26.00000000000000711 ) ) ;
#64002 = ORIENTED_EDGE ( 'NONE', *, *, #61747, .T. ) ;
#64003 = AXIS2_PLACEMENT_3D ( 'NONE', #67958, #4326, #57343 ) ;
#64004 = EDGE_LOOP ( 'NONE', ( #51124, #16901, #36417, #66238 ) ) ;
#64005 = CARTESIAN_POINT ( 'NONE',  ( 7.250000000000004441, 7.450000000000001954, -9.000000000000001776 ) ) ;
#64006 = VECTOR ( 'NONE', #25567, 1000.000000000000000 ) ;
#64007 = DIRECTION ( 'NONE',  ( 0.000000000000000000, 0.7071067811865474617, 0.7071067811865474617 ) ) ;
#64008 = AXIS2_PLACEMENT_3D ( 'NONE', #6378, #27940, #17316 ) ;
#64009 = CIRCLE ( 'NONE', #33494, 24.99999999998784972 ) ;
#64010 = DIRECTION ( 'NONE',  ( 1.000000000000000000, -0.000000000000000000, 0.000000000000000000 ) ) ;
#64011 = EDGE_LOOP ( 'NONE', ( #52015, #52523, #56177, #65345 ) ) ;
#64012 = ORIENTED_EDGE ( 'NONE', *, *, #50062, .T. ) ;
#64014 = EDGE_CURVE ( 'NONE', #38597, #7366, #6713, .T. ) ;
#64013 = DIRECTION ( 'NONE',  ( -0.000000000000000000, -0.000000000000000000, -1.000000000000000000 ) ) ;
#64015 = ORIENTED_EDGE ( 'NONE', *, *, #7151, .F. ) ;
#64016 = ORIENTED_EDGE ( 'NONE', *, *, #44942, .F. ) ;
#64017 = EDGE_CURVE ( 'NONE', #59398, #12520, #52978, .T. ) ;
#64018 = AXIS2_PLACEMENT_3D ( 'NONE', #19606, #13257, #40829 ) ;
#64019 = AXIS2_PLACEMENT_3D ( 'NONE', #19089, #57619, #36046 ) ;
#64020 = CARTESIAN_POINT ( 'NONE',  ( -9.547976262117254365, 2.355476262117183417, 54.00000000000000711 ) ) ;
#64021 = LINE ( 'NONE', #15582, #16623 ) ;
#64022 = DIRECTION ( 'NONE',  ( -0.7071067811865527908, -0.7071067811865422437, 0.000000000000000000 ) ) ;
#64023 =( GEOMETRIC_REPRESENTATION_CONTEXT ( 3 ) GLOBAL_UNCERTAINTY_ASSIGNED_CONTEXT ( ( #43674 ) ) GLOBAL_UNIT_ASSIGNED_CONTEXT ( ( #6175, #48968, #17466 ) ) REPRESENTATION_CONTEXT ( 'NONE', 'WORKASPACE' ) );
#64024 = ORIENTED_EDGE ( 'NONE', *, *, #31834, .T. ) ;
#64025 = DIRECTION ( 'NONE',  ( -1.000000000000000000, 0.000000000000000000, 0.000000000000000000 ) ) ;
#64026 = AXIS2_PLACEMENT_3D ( 'NONE', #20201, #62629, #26562 ) ;
#64027 = AXIS2_PLACEMENT_3D ( 'NONE', #54020, #6607, #11543 ) ;
#64029 = DIRECTION ( 'NONE',  ( 1.000000000000000000, 0.000000000000000000, 0.000000000000000000 ) ) ;
#64028 = FACE_OUTER_BOUND ( 'NONE', #3232, .T. ) ;
#64030 = ORIENTED_EDGE ( 'NONE', *, *, #37438, .T. ) ;
#64032 = VERTEX_POINT ( 'NONE', #56888 ) ;
#64031 = CARTESIAN_POINT ( 'NONE',  ( 15.89999999999999680, -21.00000000000000000, 13.86939075806900057 ) ) ;
#64033 = VERTEX_POINT ( 'NONE', #67523 ) ;
#64034 = VECTOR ( 'NONE', #43766, 1000.000000000000000 ) ;
#64035 = CARTESIAN_POINT ( 'NONE',  ( 0.000000000000000000, 0.000000000000000000, -23.50000000000000000 ) ) ;
#64036 = VECTOR ( 'NONE', #5359, 1000.000000000000000 ) ;
#64037 = CARTESIAN_POINT ( 'NONE',  ( -11.00000000000000000, -17.14999999999999858, 27.00000000000000000 ) ) ;
#64038 = ORIENTED_EDGE ( 'NONE', *, *, #39085, .T. ) ;
#64039 = CARTESIAN_POINT ( 'NONE',  ( -5.655420232009250370, 8.393516549646600211, 455.0000000000000568 ) ) ;
#64040 = EDGE_CURVE ( 'NONE', #37208, #30152, #40525, .T. ) ;
#64041 = DIRECTION ( 'NONE',  ( 1.000000000000000000, 0.000000000000000000, 0.000000000000000000 ) ) ;
#64042 = ORIENTED_EDGE ( 'NONE', *, *, #51773, .T. ) ;
#64043 = ORIENTED_EDGE ( 'NONE', *, *, #39745, .T. ) ;
#64044 = CARTESIAN_POINT ( 'NONE',  ( -9.234937905884020637, 9.942044687070460185, 455.0000000000000568 ) ) ;
#64045 = CYLINDRICAL_SURFACE ( 'NONE', #15463, 0.5000000000001374456 ) ;
#64046 = DIRECTION ( 'NONE',  ( -1.000000000000000000, 0.000000000000000000, 0.000000000000000000 ) ) ;
#64047 = ORIENTED_EDGE ( 'NONE', *, *, #24619, .T. ) ;
#64048 = EDGE_CURVE ( 'NONE', #20196, #41718, #12349, .T. ) ;
#64049 = DIRECTION ( 'NONE',  ( 1.000000000000000000, 0.000000000000000000, 0.000000000000000000 ) ) ;
#64050 = CARTESIAN_POINT ( 'NONE',  ( 7.000000000000000000, -26.28355339059299922, 9.766446609406699508 ) ) ;
#64051 = CIRCLE ( 'NONE', #23391, 2.204799999999997429 ) ;
#64053 = ORIENTED_EDGE ( 'NONE', *, *, #65055, .F. ) ;
#64052 =( NAMED_UNIT ( * ) SI_UNIT ( $, .STERADIAN. ) SOLID_ANGLE_UNIT ( ) );
#64055 = VERTEX_POINT ( 'NONE', #24018 ) ;
#64054 = CARTESIAN_POINT ( 'NONE',  ( -11.33351654964663879, -1.090483450353281425, 195.0000000000000284 ) ) ;
#64056 = EDGE_CURVE ( 'NONE', #63385, #12173, #8446, .T. ) ;
#64057 = CARTESIAN_POINT ( 'NONE',  ( -5.993516549646776603, -6.006483450353426790, 455.0000000000000568 ) ) ;
#64058 = LINE ( 'NONE', #4991, #17138 ) ;
#64059 = EDGE_CURVE ( 'NONE', #44826, #5610, #34266, .T. ) ;
#64060 = DIRECTION ( 'NONE',  ( 1.000000000000000000, 0.000000000000000000, -0.000000000000000000 ) ) ;
#64061 = EDGE_CURVE ( 'NONE', #54337, #64273, #45577, .T. ) ;
#64062 = LINE ( 'NONE', #48134, #32412 ) ;
#64063 = PLANE ( 'NONE',  #46333 ) ;
#64064 = AXIS2_PLACEMENT_3D ( 'NONE', #649, #59696, #37441 ) ;
#64065 = VECTOR ( 'NONE', #49760, 1000.000000000000000 ) ;
#64066 = EDGE_CURVE ( 'NONE', #8058, #29091, #44893, .T. ) ;
#64067 = ADVANCED_FACE ( 'NONE', ( #66114 ), #66461, .T. ) ;
#64068 = DIRECTION ( 'NONE',  ( 0.000000000000000000, -3.673940397442059868E-16, 1.000000000000000000 ) ) ;
#64069 = VERTEX_POINT ( 'NONE', #2798 ) ;
#64070 = CARTESIAN_POINT ( 'NONE',  ( 69.92576880110416937, 10.00000000000000000, 335.4830310981152479 ) ) ;
#64072 = VERTEX_POINT ( 'NONE', #39243 ) ;
#64071 = DIRECTION ( 'NONE',  ( 0.000000000000000000, 0.000000000000000000, 1.000000000000000000 ) ) ;
#64073 = AXIS2_PLACEMENT_3D ( 'NONE', #30489, #67275, #51005 ) ;
#64075 = DIRECTION ( 'NONE',  ( -0.000000000000000000, 1.000000000000000000, -0.000000000000000000 ) ) ;
#64074 = AXIS2_PLACEMENT_3D ( 'NONE', #65920, #33414, #6867 ) ;
#64076 = CARTESIAN_POINT ( 'NONE',  ( -5.242976262117280406, -5.257023737882805747, 54.00000000000000711 ) ) ;
#64077 = AXIS2_PLACEMENT_3D ( 'NONE', #16016, #28594, #61111 ) ;
#64078 = CARTESIAN_POINT ( 'NONE',  ( 7.000000000000000000, -32.95000000000000284, -13.19999999999999929 ) ) ;
#64079 = VECTOR ( 'NONE', #60970, 1000.000000000000114 ) ;
#64080 = VECTOR ( 'NONE', #55473, 1000.000000000000000 ) ;
#64081 = EDGE_LOOP ( 'NONE', ( #20418, #5246, #22986, #48422 ) ) ;
#64082 = CARTESIAN_POINT ( 'NONE',  ( -16.75000000000000000, -0.2714405302574894319, 22.98746066354538087 ) ) ;
#64083 = DIRECTION ( 'NONE',  ( 0.000000000000000000, 0.7071067811865474617, -0.7071067811865474617 ) ) ;
#64084 = ORIENTED_EDGE ( 'NONE', *, *, #47112, .F. ) ;
#64085 = DIRECTION ( 'NONE',  ( 0.000000000000000000, 0.000000000000000000, 1.000000000000000000 ) ) ;
#64086 = SURFACE_STYLE_USAGE ( .BOTH. , #36130 ) ;
#64087 = VECTOR ( 'NONE', #47690, 1000.000000000000000 ) ;
#64088 = CARTESIAN_POINT ( 'NONE',  ( 12.00000000000000000, 11.18999999999999950, -4.250000000000000000 ) ) ;
#64089 = ORIENTED_EDGE ( 'NONE', *, *, #39823, .T. ) ;
#64090 = DIRECTION ( 'NONE',  ( 0.000000000000000000, 0.000000000000000000, 1.000000000000000000 ) ) ;
#64091 = ORIENTED_EDGE ( 'NONE', *, *, #46377, .T. ) ;
#64092 = VERTEX_POINT ( 'NONE', #19069 ) ;
#64093 = CARTESIAN_POINT ( 'NONE',  ( 14.75000000000000178, -42.25000000000000000, 26.75000000000000000 ) ) ;
#64094 = DIRECTION ( 'NONE',  ( 1.000000000000000000, 0.000000000000000000, 0.000000000000000000 ) ) ;
#64095 = FACE_OUTER_BOUND ( 'NONE', #7691, .T. ) ;
#64096 = DIRECTION ( 'NONE',  ( -0.7142857142857395036, 0.000000000000000000, -0.6998542122237394469 ) ) ;
#64097 = ORIENTED_EDGE ( 'NONE', *, *, #29933, .F. ) ;
#64098 = VERTEX_POINT ( 'NONE', #62197 ) ;
#64100 = ORIENTED_EDGE ( 'NONE', *, *, #32385, .T. ) ;
#64099 = CARTESIAN_POINT ( 'NONE',  ( 4.201500623656039934, 7.259684009079806266, 455.0000000000000568 ) ) ;
#64101 = EDGE_LOOP ( 'NONE', ( #20935, #19616, #28431, #10325 ) ) ;
#64102 = EDGE_CURVE ( 'NONE', #64845, #69297, #18013, .T. ) ;
#64103 = DIRECTION ( 'NONE',  ( 0.000000000000000000, 1.000000000000000000, 0.000000000000000000 ) ) ;
#64104 = CARTESIAN_POINT ( 'NONE',  ( -6.835476262117260227, 10.49297626211718359, 54.00000000000000711 ) ) ;
#64105 = DIRECTION ( 'NONE',  ( -1.000000000000000000, 0.000000000000000000, 0.000000000000000000 ) ) ;
#64106 = STYLED_ITEM ( 'NONE', ( #48051 ), #20709 ) ;
#64107 = EDGE_CURVE ( 'NONE', #59237, #8340, #18716, .T. ) ;
#64108 = PLANE ( 'NONE',  #61550 ) ;
#64110 = LINE ( 'NONE', #42163, #44694 ) ;
#64109 = DIRECTION ( 'NONE',  ( -0.000000000000000000, -0.000000000000000000, -1.000000000000000000 ) ) ;
#64111 = ORIENTED_EDGE ( 'NONE', *, *, #49440, .T. ) ;
#64112 = ORIENTED_EDGE ( 'NONE', *, *, #18629, .F. ) ;
#64113 = ORIENTED_EDGE ( 'NONE', *, *, #55188, .T. ) ;
#64114 = ORIENTED_EDGE ( 'NONE', *, *, #36284, .T. ) ;
#64115 = VECTOR ( 'NONE', #37359, 1000.000000000000000 ) ;
#64116 = VECTOR ( 'NONE', #48645, 1000.000000000000114 ) ;
#64117 = DIRECTION ( 'NONE',  ( 0.000000000000000000, 0.000000000000000000, 1.000000000000000000 ) ) ;
#64118 = CARTESIAN_POINT ( 'NONE',  ( -8.697938382363103571, -2.420780051175099423, 54.00000000000000711 ) ) ;
#64119 = DIRECTION ( 'NONE',  ( 0.000000000000000000, 0.000000000000000000, 1.000000000000000000 ) ) ;
#64120 = CIRCLE ( 'NONE', #31357, 0.3500000000009988455 ) ;
#64121 = VECTOR ( 'NONE', #52837, 1000.000000000000000 ) ;
#64122 = FACE_OUTER_BOUND ( 'NONE', #61512, .T. ) ;
#64123 = EDGE_CURVE ( 'NONE', #28168, #68940, #64198, .T. ) ;
#64124 = ORIENTED_EDGE ( 'NONE', *, *, #36659, .F. ) ;
#64125 = ORIENTED_EDGE ( 'NONE', *, *, #8643, .F. ) ;
#64126 = ORIENTED_EDGE ( 'NONE', *, *, #66934, .F. ) ;
#64127 = CARTESIAN_POINT ( 'NONE',  ( -10.03972626211722918, 9.689726262117183353, 54.00000000000000711 ) ) ;
#64128 = CIRCLE ( 'NONE', #44907, 5.200000000000009948 ) ;
#64129 = VECTOR ( 'NONE', #48352, 1000.000000000000000 ) ;
#64130 = EDGE_LOOP ( 'NONE', ( #46060, #59817, #59842, #59584 ) ) ;
#64131 = DIRECTION ( 'NONE',  ( -1.000000000000000000, 0.000000000000000000, 0.000000000000000000 ) ) ;
#64132 = ORIENTED_EDGE ( 'NONE', *, *, #48235, .T. ) ;
#64133 = ORIENTED_EDGE ( 'NONE', *, *, #35368, .F. ) ;
#64134 = CARTESIAN_POINT ( 'NONE',  ( -7.250000000000000888, 7.250000000000001776, -25.00000000000000000 ) ) ;
#64136 = VERTEX_POINT ( 'NONE', #22979 ) ;
#64135 = DIRECTION ( 'NONE',  ( 0.000000000000000000, 0.000000000000000000, -1.000000000000000000 ) ) ;
#64137 = VERTEX_POINT ( 'NONE', #40285 ) ;
#64138 = AXIS2_PLACEMENT_3D ( 'NONE', #40188, #13675, #45848 ) ;
#64139 = EDGE_CURVE ( 'NONE', #48487, #19877, #52250, .T. ) ;
#64140 = CARTESIAN_POINT ( 'NONE',  ( 15.50000000000000000, -1.037157890325000054, 26.50000000000000000 ) ) ;
#64141 = DIRECTION ( 'NONE',  ( 1.000000000000000000, 0.000000000000000000, 0.000000000000000000 ) ) ;
#64143 = ORIENTED_EDGE ( 'NONE', *, *, #4285, .F. ) ;
#64142 = DIRECTION ( 'NONE',  ( 0.000000000000000000, 0.000000000000000000, 1.000000000000000000 ) ) ;
#64144 = ORIENTED_EDGE ( 'NONE', *, *, #68616, .F. ) ;
#64145 = DIRECTION ( 'NONE',  ( 1.836970198721029934E-16, 1.836970198721010706E-16, -1.000000000000000000 ) ) ;
#64146 = DIRECTION ( 'NONE',  ( 0.000000000000000000, 1.000000000000000000, 0.000000000000000000 ) ) ;
#64147 = EDGE_CURVE ( 'NONE', #9849, #1721, #62421, .T. ) ;
#64148 = FACE_OUTER_BOUND ( 'NONE', #32018, .T. ) ;
#64149 = DIRECTION ( 'NONE',  ( 0.6414496315691445849, 0.7671651518153106419, -0.000000000000000000 ) ) ;
#64150 = CARTESIAN_POINT ( 'NONE',  ( 7.000000000000000000, -53.81370849898476649, -16.03137303340311348 ) ) ;
#64151 = EDGE_CURVE ( 'NONE', #22300, #63937, #7403, .T. ) ;
#64152 = EDGE_CURVE ( 'NONE', #48227, #41721, #34970, .T. ) ;
#64153 = ORIENTED_EDGE ( 'NONE', *, *, #66000, .T. ) ;
#64154 = FACE_BOUND ( 'NONE', #19005, .T. ) ;
#64155 = VERTEX_POINT ( 'NONE', #2111 ) ;
#64156 = DIRECTION ( 'NONE',  ( -0.000000000000000000, -1.000000000000000000, -0.000000000000000000 ) ) ;
#64157 = PRESENTATION_STYLE_ASSIGNMENT (( #31622 ) ) ;
#64158 = EDGE_CURVE ( 'NONE', #2063, #21563, #8097, .T. ) ;
#64159 =( GEOMETRIC_REPRESENTATION_CONTEXT ( 3 ) GLOBAL_UNCERTAINTY_ASSIGNED_CONTEXT ( ( #53593 ) ) GLOBAL_UNIT_ASSIGNED_CONTEXT ( ( #26311, #19953, #42217 ) ) REPRESENTATION_CONTEXT ( 'NONE', 'WORKASPACE' ) );
#64160 = CARTESIAN_POINT ( 'NONE',  ( -7.250000000000000888, 7.250000000000001776, -8.500000000000000000 ) ) ;
#64161 = PLANE ( 'NONE',  #28360 ) ;
#64162 = CARTESIAN_POINT ( 'NONE',  ( -7.793516549646712477, 11.11351654964660085, 455.0000000000000568 ) ) ;
#64163 = ORIENTED_EDGE ( 'NONE', *, *, #36837, .F. ) ;
#64164 = LINE ( 'NONE', #52490, #57309 ) ;
#64165 = CIRCLE ( 'NONE', #49461, 0.4999999999945534124 ) ;
#64166 = EDGE_LOOP ( 'NONE', ( #232, #11016, #10097, #44244 ) ) ;
#64167 = DIRECTION ( 'NONE',  ( 1.000000000000000000, 0.000000000000000000, 0.000000000000000000 ) ) ;
#64168 = DIRECTION ( 'NONE',  ( 1.000000000000000000, -0.000000000000000000, -0.000000000000000000 ) ) ;
#64169 = CARTESIAN_POINT ( 'NONE',  ( 6.657023737882821202, 10.30047626211719347, 54.00000000000000711 ) ) ;
#64170 = AXIS2_PLACEMENT_3D ( 'NONE', #50525, #11635, #66436 ) ;
#64171 = PLANE ( 'NONE',  #69715 ) ;
#64172 = VECTOR ( 'NONE', #46857, 1000.000000000000000 ) ;
#64173 = DIRECTION ( 'NONE',  ( -0.000000000000000000, 3.673940397442059868E-16, -1.000000000000000000 ) ) ;
#64174 = ORIENTED_EDGE ( 'NONE', *, *, #62128, .F. ) ;
#64175 = CARTESIAN_POINT ( 'NONE',  ( -7.955476262117259445, 8.821682069070703847, 54.00000000000000711 ) ) ;
#64176 = LINE ( 'NONE', #46833, #36168 ) ;
#64177 = CARTESIAN_POINT ( 'NONE',  ( 41.09999999999999432, -14.48845687959340012, 21.00000000000000000 ) ) ;
#64178 = SURFACE_STYLE_USAGE ( .BOTH. , #63109 ) ;
#64179 = CARTESIAN_POINT ( 'NONE',  ( 275.0000000000000000, -25.00000000000000000, 17.50000000000000000 ) ) ;
#64180 = VERTEX_POINT ( 'NONE', #24378 ) ;
#64182 = EDGE_LOOP ( 'NONE', ( #2939, #68519, #41698, #18585 ) ) ;
#64181 = LINE ( 'NONE', #22076, #9140 ) ;
#64183 = CIRCLE ( 'NONE', #31423, 0.2000000000000005107 ) ;
#64184 = CARTESIAN_POINT ( 'NONE',  ( 14.25000000000000000, -2.500000000000000000, 23.22168783648699986 ) ) ;
#64185 = CARTESIAN_POINT ( 'NONE',  ( 7.450000000000004619, -1.336933437520057563E-15, -17.00000000000000000 ) ) ;
#64186 = FACE_OUTER_BOUND ( 'NONE', #39280, .T. ) ;
#64187 = ORIENTED_EDGE ( 'NONE', *, *, #54716, .F. ) ;
#64188 = EDGE_CURVE ( 'NONE', #7124, #35485, #57898, .T. ) ;
#64189 = EDGE_CURVE ( 'NONE', #63676, #24780, #66801, .T. ) ;
#64190 = ADVANCED_FACE ( 'NONE', ( #47342 ), #15177, .F. ) ;
#64191 = LINE ( 'NONE', #37655, #17191 ) ;
#64192 = ORIENTED_EDGE ( 'NONE', *, *, #36245, .F. ) ;
#64193 = ORIENTED_EDGE ( 'NONE', *, *, #18278, .T. ) ;
#64194 = ADVANCED_FACE ( 'NONE', ( #46285 ), #26312, .F. ) ;
#64195 = ORIENTED_EDGE ( 'NONE', *, *, #58669, .T. ) ;
#64196 = FACE_OUTER_BOUND ( 'NONE', #23549, .T. ) ;
#64197 = CARTESIAN_POINT ( 'NONE',  ( 289.7500000000001137, -0.2499999999999414080, 26.75000000000004263 ) ) ;
#64198 = LINE ( 'NONE', #15745, #33657 ) ;
#64199 = ORIENTED_EDGE ( 'NONE', *, *, #51497, .F. ) ;
#64200 = ORIENTED_EDGE ( 'NONE', *, *, #28877, .F. ) ;
#64201 = CARTESIAN_POINT ( 'NONE',  ( 9.562023737882801910, 8.130476262117189989, 26.00000000000000711 ) ) ;
#64202 = ORIENTED_EDGE ( 'NONE', *, *, #43753, .T. ) ;
#64203 = VERTEX_POINT ( 'NONE', #14822 ) ;
#64204 = ORIENTED_EDGE ( 'NONE', *, *, #35555, .T. ) ;
#64205 = VERTEX_POINT ( 'NONE', #31089 ) ;
#64206 = DIRECTION ( 'NONE',  ( -1.000000000000000000, 0.000000000000000000, 0.000000000000000000 ) ) ;
#64207 = UNCERTAINTY_MEASURE_WITH_UNIT (LENGTH_MEASURE( 1.000000000000000082E-05 ), #29277, 'distance_accuracy_value', 'NONE');
#64209 = ORIENTED_EDGE ( 'NONE', *, *, #16454, .F. ) ;
#64208 = DIRECTION ( 'NONE',  ( 0.000000000000000000, 0.000000000000000000, 1.000000000000000000 ) ) ;
#64210 = VECTOR ( 'NONE', #18140, 1000.000000000000000 ) ;
#64211 = LINE ( 'NONE', #53256, #61669 ) ;
#64212 = LINE ( 'NONE', #16108, #14869 ) ;
#64213 = CARTESIAN_POINT ( 'NONE',  ( 39.00000000000000000, 16.96999999999999886, -21.00000000000000000 ) ) ;
#64214 = VERTEX_POINT ( 'NONE', #68209 ) ;
#64215 = VECTOR ( 'NONE', #5168, 1000.000000000000000 ) ;
#64216 = CARTESIAN_POINT ( 'NONE',  ( 277.1811023147819810, -25.34729925119250282, -17.15270074880750784 ) ) ;
#64217 = CYLINDRICAL_SURFACE ( 'NONE', #1065, 0.5000000000001357803 ) ;
#64218 = VERTEX_POINT ( 'NONE', #46993 ) ;
#64219 = EDGE_CURVE ( 'NONE', #31408, #16734, #36743, .T. ) ;
#64220 = AXIS2_PLACEMENT_3D ( 'NONE', #46041, #48052, #69632 ) ;
#64221 = DIRECTION ( 'NONE',  ( -1.000000000000000000, 0.000000000000000000, 0.000000000000000000 ) ) ;
#64222 = DIRECTION ( 'NONE',  ( -1.000000000000000000, 0.000000000000000000, 0.000000000000000000 ) ) ;
#64223 = ADVANCED_FACE ( 'NONE', ( #63973 ), #4227, .F. ) ;
#64224 = EDGE_CURVE ( 'NONE', #67312, #22480, #68915, .T. ) ;
#64225 = DIRECTION ( 'NONE',  ( 0.000000000000000000, 1.000000000000000000, 0.000000000000000000 ) ) ;
#64226 = VERTEX_POINT ( 'NONE', #14474 ) ;
#64227 = DIRECTION ( 'NONE',  ( 0.000000000000000000, -2.854859206170826497E-12, 1.000000000000000000 ) ) ;
#64228 = DIRECTION ( 'NONE',  ( 0.000000000000000000, 0.000000000000000000, -1.000000000000000000 ) ) ;
#64229 = LINE ( 'NONE', #26738, #4832 ) ;
#64230 = EDGE_CURVE ( 'NONE', #7472, #51947, #67862, .T. ) ;
#64231 = DIRECTION ( 'NONE',  ( 0.000000000000000000, 0.000000000000000000, -1.000000000000000000 ) ) ;
#64232 = DIRECTION ( 'NONE',  ( -1.000000000000000000, 1.047444401652940007E-14, 0.000000000000000000 ) ) ;
#64233 = EDGE_CURVE ( 'NONE', #56183, #66802, #52668, .T. ) ;
#64234 = VERTEX_POINT ( 'NONE', #20471 ) ;
#64235 = CARTESIAN_POINT ( 'NONE',  ( 9.737023737882816832, -6.832023737882813919, 26.00000000000000000 ) ) ;
#64236 = FACE_OUTER_BOUND ( 'NONE', #44845, .T. ) ;
#64238 = ADVANCED_FACE ( 'NONE', ( #62910 ), #19417, .F. ) ;
#64237 = DIRECTION ( 'NONE',  ( 0.000000000000000000, 3.673940397442059868E-16, -1.000000000000000000 ) ) ;
#64239 = LINE ( 'NONE', #32405, #8555 ) ;
#64240 = ORIENTED_EDGE ( 'NONE', *, *, #5321, .T. ) ;
#64241 = DIRECTION ( 'NONE',  ( 1.836970198721029934E-16, -1.836970198721036344E-16, 1.000000000000000000 ) ) ;
#64242 = CARTESIAN_POINT ( 'NONE',  ( 5.393625297349900372, -7.265214908726231435, 455.0000000000000568 ) ) ;
#64243 = DIRECTION ( 'NONE',  ( 1.000000000000000000, -0.000000000000000000, -0.000000000000000000 ) ) ;
#64244 = LINE ( 'NONE', #41613, #53392 ) ;
#64245 = ORIENTED_EDGE ( 'NONE', *, *, #39147, .T. ) ;
#64246 = FACE_OUTER_BOUND ( 'NONE', #13112, .T. ) ;
#64247 = CARTESIAN_POINT ( 'NONE',  ( -8.916576262117258622, 10.03972626211718477, 54.00000000000000711 ) ) ;
#64248 = DIRECTION ( 'NONE',  ( 0.6414496315691446959, -0.7671651518153106419, 0.000000000000000000 ) ) ;
#64249 = FACE_OUTER_BOUND ( 'NONE', #47747, .T. ) ;
#64250 = DIRECTION ( 'NONE',  ( 0.000000000000000000, 0.000000000000000000, 1.000000000000000000 ) ) ;
#64251 = ORIENTED_EDGE ( 'NONE', *, *, #32988, .T. ) ;
#64252 = AXIS2_PLACEMENT_3D ( 'NONE', #50239, #16697, #11709 ) ;
#64253 = SHAPE_REPRESENTATION ( 'LINEAR ACTUATOR', ( #45918 ), #825 ) ;
#64254 = ORIENTED_EDGE ( 'NONE', *, *, #14790, .F. ) ;
#64255 = CARTESIAN_POINT ( 'NONE',  ( 283.0000000000000568, -26.42999999999999972, -9.412893218813501051 ) ) ;
#64256 = LINE ( 'NONE', #51894, #15338 ) ;
#64257 = EDGE_LOOP ( 'NONE', ( #30408, #18312, #38539, #37199 ) ) ;
#64258 = LINE ( 'NONE', #58946, #24665 ) ;
#64259 = VECTOR ( 'NONE', #2197, 1000.000000000000000 ) ;
#64260 = DIRECTION ( 'NONE',  ( 0.000000000000000000, -0.5547756303226734076, 0.8320000000000482565 ) ) ;
#64261 = ORIENTED_EDGE ( 'NONE', *, *, #40569, .F. ) ;
#64262 = AXIS2_PLACEMENT_3D ( 'NONE', #49196, #21287, #11692 ) ;
#64263 = CARTESIAN_POINT ( 'NONE',  ( -11.99351654964671354, 4.173516549646604901, 455.0000000000000568 ) ) ;
#64264 = ORIENTED_EDGE ( 'NONE', *, *, #6355, .T. ) ;
#64265 = ORIENTED_EDGE ( 'NONE', *, *, #7512, .F. ) ;
#64266 = CARTESIAN_POINT ( 'NONE',  ( 25.57999999999999829, 0.000000000000000000, 0.000000000000000000 ) ) ;
#64267 = ORIENTED_EDGE ( 'NONE', *, *, #7555, .F. ) ;
#64268 = LINE ( 'NONE', #8854, #51160 ) ;
#64270 = AXIS2_PLACEMENT_3D ( 'NONE', #33823, #32472, #54041 ) ;
#64269 = AXIS2_PLACEMENT_3D ( 'NONE', #40200, #46203, #30307 ) ;
#64271 = CARTESIAN_POINT ( 'NONE',  ( 277.3542486889354564, -20.49999999999999645, -17.00000000000000000 ) ) ;
#64272 = DIRECTION ( 'NONE',  ( -1.836970198721029934E-16, -1.836970198721010706E-16, 1.000000000000000000 ) ) ;
#64273 = VERTEX_POINT ( 'NONE', #58660 ) ;
#64274 = ORIENTED_EDGE ( 'NONE', *, *, #49603, .F. ) ;
#64275 = DIRECTION ( 'NONE',  ( 0.000000000000000000, 1.000000000000000000, 0.000000000000000000 ) ) ;
#64278 = LINE ( 'NONE', #4185, #10750 ) ;
#64277 = CARTESIAN_POINT ( 'NONE',  ( 289.2330000000000041, 0.000000000000000000, 0.000000000000000000 ) ) ;
#64276 = AXIS2_PLACEMENT_3D ( 'NONE', #53102, #4655, #26215 ) ;
#64279 = EDGE_CURVE ( 'NONE', #63002, #69628, #25083, .T. ) ;
#64280 = VERTEX_POINT ( 'NONE', #63620 ) ;
#64281 = VERTEX_POINT ( 'NONE', #58318 ) ;
#64282 = ORIENTED_EDGE ( 'NONE', *, *, #24519, .T. ) ;
#64283 = EDGE_CURVE ( 'NONE', #8396, #61131, #7054, .T. ) ;
#64284 = LINE ( 'NONE', #10528, #53712 ) ;
#64286 = ORIENTED_EDGE ( 'NONE', *, *, #32903, .F. ) ;
#64285 = CARTESIAN_POINT ( 'NONE',  ( -9.781776262117249487, 10.49297626211718359, 54.00000000000000711 ) ) ;
#64287 = LINE ( 'NONE', #15148, #62732 ) ;
#64288 = DIRECTION ( 'NONE',  ( 0.000000000000000000, 0.000000000000000000, -1.000000000000000000 ) ) ;
#64289 = ORIENTED_EDGE ( 'NONE', *, *, #61832, .F. ) ;
#64290 = ORIENTED_EDGE ( 'NONE', *, *, #69567, .F. ) ;
#64291 = PLANE ( 'NONE',  #43662 ) ;
#64292 = ADVANCED_FACE ( 'NONE', ( #31792 ), #9878, .F. ) ;
#64293 = VERTEX_POINT ( 'NONE', #3865 ) ;
#64294 = AXIS2_PLACEMENT_3D ( 'NONE', #42610, #55646, #65898 ) ;
#64295 = DIRECTION ( 'NONE',  ( 0.5773502691896230665, -0.5773502691896271743, -0.5773502691896271743 ) ) ;
#64296 = CARTESIAN_POINT ( 'NONE',  ( 4.747751991980625696, -6.619341603356940773, 455.0000000000000568 ) ) ;
#64297 = DIRECTION ( 'NONE',  ( -1.000000000000000000, 0.000000000000000000, 0.000000000000000000 ) ) ;
#64298 = ORIENTED_EDGE ( 'NONE', *, *, #65245, .T. ) ;
#64299 = VECTOR ( 'NONE', #69980, 1000.000000000000000 ) ;
#64300 = DIRECTION ( 'NONE',  ( 1.836970198721029934E-16, 1.836970198721010706E-16, -1.000000000000000000 ) ) ;
#64301 = DIRECTION ( 'NONE',  ( 8.802523127157697409E-15, 1.000000000000000000, 0.000000000000000000 ) ) ;
#64302 = ADVANCED_FACE ( 'NONE', ( #68570 ), #63261, .F. ) ;
#64304 = ORIENTED_EDGE ( 'NONE', *, *, #69137, .F. ) ;
#64303 =( NAMED_UNIT ( * ) SI_UNIT ( $, .STERADIAN. ) SOLID_ANGLE_UNIT ( ) );
#64305 = ORIENTED_EDGE ( 'NONE', *, *, #43279, .T. ) ;
#64306 = LINE ( 'NONE', #31447, #8316 ) ;
#64307 = AXIS2_PLACEMENT_3D ( 'NONE', #8817, #30385, #39922 ) ;
#64308 = DIRECTION ( 'NONE',  ( -1.000000000000000000, 0.000000000000000000, 0.000000000000000000 ) ) ;
#64309 = CARTESIAN_POINT ( 'NONE',  ( -28.00000000000000000, -17.50000000000000000, 20.05051025721700242 ) ) ;
#64310 = DIRECTION ( 'NONE',  ( 0.000000000000000000, 0.000000000000000000, -1.000000000000000000 ) ) ;
#64311 = AXIS2_PLACEMENT_3D ( 'NONE', #36630, #62436, #46883 ) ;
#64312 = DIRECTION ( 'NONE',  ( -1.000000000000000000, 0.000000000000000000, 0.000000000000000000 ) ) ;
#64313 = EDGE_CURVE ( 'NONE', #14190, #56758, #4571, .T. ) ;
#64314 = ORIENTED_EDGE ( 'NONE', *, *, #56800, .T. ) ;
#64315 = DIRECTION ( 'NONE',  ( -5.981805089575196197E-17, -1.000000000000000000, 0.000000000000000000 ) ) ;
#64316 = LINE ( 'NONE', #20474, #37305 ) ;
#64318 = EDGE_CURVE ( 'NONE', #54520, #31859, #9351, .T. ) ;
#64317 = CARTESIAN_POINT ( 'NONE',  ( -4.031976262117257903, -3.157023737882818981, 54.00000000000000711 ) ) ;
#64319 = VECTOR ( 'NONE', #4418, 1000.000000000000000 ) ;
#64321 = EDGE_LOOP ( 'NONE', ( #1872, #31742, #58375, #3944 ) ) ;
#64320 = CARTESIAN_POINT ( 'NONE',  ( -8.227189898828699555, -1.634292677759815904, 54.00000000000000711 ) ) ;
#64322 = DIRECTION ( 'NONE',  ( 0.000000000000000000, 0.7071067811865474617, 0.7071067811865474617 ) ) ;
#64323 = PLANE ( 'NONE',  #67588 ) ;
#64324 = DIRECTION ( 'NONE',  ( 1.000000000000000000, -0.000000000000000000, 0.000000000000000000 ) ) ;
#64325 = CYLINDRICAL_SURFACE ( 'NONE', #64976, 4.500000000000188294 ) ;
#64326 = ORIENTED_EDGE ( 'NONE', *, *, #34231, .F. ) ;
#64327 = LINE ( 'NONE', #57615, #49011 ) ;
#64328 = CARTESIAN_POINT ( 'NONE',  ( -7.250000000000000888, 8.250000000000001776, -8.500000000000000000 ) ) ;
#64329 = EDGE_LOOP ( 'NONE', ( #58888, #18124, #58870, #10459 ) ) ;
#64330 = CARTESIAN_POINT ( 'NONE',  ( -30.00000000000000000, 0.000000000000000000, 27.00000000000000000 ) ) ;
#64331 = FACE_OUTER_BOUND ( 'NONE', #19008, .T. ) ;
#64332 = CARTESIAN_POINT ( 'NONE',  ( -25.50000000000000355, 0.000000000000000000, -22.50000000000000000 ) ) ;
#64333 = CARTESIAN_POINT ( 'NONE',  ( -8.598420958951642490, -2.005523737882745738, 54.00000000000000711 ) ) ;
#64334 = CARTESIAN_POINT ( 'NONE',  ( 3.606483450353406006, 7.415254214038213831, 455.0000000000000568 ) ) ;
#64335 = ORIENTED_EDGE ( 'NONE', *, *, #64706, .T. ) ;
#64336 = ORIENTED_EDGE ( 'NONE', *, *, #43763, .F. ) ;
#64337 = FACE_OUTER_BOUND ( 'NONE', #39244, .T. ) ;
#64338 = AXIS2_PLACEMENT_3D ( 'NONE', #62969, #53077, #58010 ) ;
#64339 = ORIENTED_EDGE ( 'NONE', *, *, #31643, .F. ) ;
#64340 = ORIENTED_EDGE ( 'NONE', *, *, #35712, .T. ) ;
#64341 = DIRECTION ( 'NONE',  ( -0.000000000000000000, -0.000000000000000000, -1.000000000000000000 ) ) ;
#64342 = ADVANCED_FACE ( 'NONE', ( #11923 ), #60027, .T. ) ;
#64343 = LINE ( 'NONE', #27544, #11840 ) ;
#64344 = CARTESIAN_POINT ( 'NONE',  ( 15.00000000000000000, -23.65000000000000568, -12.40000000000000213 ) ) ;
#64345 = ORIENTED_EDGE ( 'NONE', *, *, #22526, .T. ) ;
#64346 = VERTEX_POINT ( 'NONE', #48393 ) ;
#64347 = CYLINDRICAL_SURFACE ( 'NONE', #6992, 0.2000000000000005107 ) ;
#64348 = VECTOR ( 'NONE', #23802, 1000.000000000000000 ) ;
#64349 = EDGE_LOOP ( 'NONE', ( #35316, #28149, #49037, #18967 ) ) ;
#64350 = EDGE_CURVE ( 'NONE', #11735, #16770, #48886, .T. ) ;
#64351 = ORIENTED_EDGE ( 'NONE', *, *, #63553, .F. ) ;
#64352 = LINE ( 'NONE', #38521, #39442 ) ;
#64353 = CARTESIAN_POINT ( 'NONE',  ( -9.293516549646710700, 10.08346604330776941, 195.0000000000000284 ) ) ;
#64354 = DIRECTION ( 'NONE',  ( -0.7071067811865422437, 0.7071067811865527908, 2.597868168706499332E-16 ) ) ;
#64355 = VERTEX_POINT ( 'NONE', #53360 ) ;
#64356 = EDGE_CURVE ( 'NONE', #64674, #46952, #21515, .T. ) ;
#64357 = CIRCLE ( 'NONE', #21442, 1.000000000000000000 ) ;
#64358 = CARTESIAN_POINT ( 'NONE',  ( 8.750000000000005329, 0.000000000000000000, -30.00000000000001066 ) ) ;
#64360 = CARTESIAN_POINT ( 'NONE',  ( -8.916576262117352769, -9.703773737882729122, 26.00000000000000000 ) ) ;
#64359 = FACE_OUTER_BOUND ( 'NONE', #28136, .T. ) ;
#64361 = ORIENTED_EDGE ( 'NONE', *, *, #40004, .F. ) ;
#64362 = ADVANCED_FACE ( 'NONE', ( #59694 ), #54396, .T. ) ;
#64364 = ORIENTED_EDGE ( 'NONE', *, *, #65053, .T. ) ;
#64363 = FACE_OUTER_BOUND ( 'NONE', #45629, .T. ) ;
#64365 = ORIENTED_EDGE ( 'NONE', *, *, #21781, .F. ) ;
#64366 = VECTOR ( 'NONE', #44213, 1000.000000000000000 ) ;
#64367 = EDGE_CURVE ( 'NONE', #47595, #54695, #10457, .T. ) ;
#64368 = DIRECTION ( 'NONE',  ( -1.000000000000000000, 0.000000000000000000, 0.000000000000000000 ) ) ;
#64369 = VECTOR ( 'NONE', #51001, 1000.000000000000000 ) ;
#64370 = DIRECTION ( 'NONE',  ( -0.5773502691896230665, 0.5773502691896271743, -0.5773502691896271743 ) ) ;
#64371 = VERTEX_POINT ( 'NONE', #4915 ) ;
#64372 = EDGE_CURVE ( 'NONE', #48826, #43831, #300, .T. ) ;
#64373 = EDGE_CURVE ( 'NONE', #19531, #35354, #60169, .T. ) ;
#64374 = VECTOR ( 'NONE', #13932, 1000.000000000000000 ) ;
#64375 = AXIS2_PLACEMENT_3D ( 'NONE', #3049, #7279, #34147 ) ;
#64376 = LINE ( 'NONE', #31854, #48209 ) ;
#64377 = CARTESIAN_POINT ( 'NONE',  ( -7.249999999999995559, 8.250000000000001776, 0.000000000000000000 ) ) ;
#64378 = EDGE_CURVE ( 'NONE', #29056, #55597, #5947, .T. ) ;
#64379 = ORIENTED_EDGE ( 'NONE', *, *, #43178, .F. ) ;
#64380 = EDGE_CURVE ( 'NONE', #22852, #6870, #35309, .T. ) ;
#64381 = EDGE_CURVE ( 'NONE', #7253, #50419, #22559, .T. ) ;
#64382 = VERTEX_POINT ( 'NONE', #49080 ) ;
#64383 = DIRECTION ( 'NONE',  ( 0.000000000000000000, 0.000000000000000000, -1.000000000000000000 ) ) ;
#64384 = DIRECTION ( 'NONE',  ( -1.836970198721029934E-16, 1.836970198721036344E-16, -1.000000000000000000 ) ) ;
#64385 = CARTESIAN_POINT ( 'NONE',  ( -9.722976262117258628, 3.667976262117184749, 54.00000000000000711 ) ) ;
#64386 = ORIENTED_EDGE ( 'NONE', *, *, #32334, .F. ) ;
#64387 = EDGE_CURVE ( 'NONE', #30360, #43706, #64647, .T. ) ;
#64388 = FACE_OUTER_BOUND ( 'NONE', #32874, .T. ) ;
#64389 = CIRCLE ( 'NONE', #20311, 1.499999999997024602 ) ;
#64390 = EDGE_CURVE ( 'NONE', #32920, #56770, #69209, .T. ) ;
#64391 = DIRECTION ( 'NONE',  ( 0.000000000000000000, 1.000000000000000000, 0.000000000000000000 ) ) ;
#64393 = ORIENTED_EDGE ( 'NONE', *, *, #33230, .T. ) ;
#64392 = FACE_OUTER_BOUND ( 'NONE', #67273, .T. ) ;
#64395 = ORIENTED_EDGE ( 'NONE', *, *, #64040, .T. ) ;
#64394 = LINE ( 'NONE', #36827, #32303 ) ;
#64396 = LINE ( 'NONE', #64732, #40702 ) ;
#64397 = LINE ( 'NONE', #32572, #69080 ) ;
#64398 = LINE ( 'NONE', #47771, #64036 ) ;
#64399 = LINE ( 'NONE', #55168, #36920 ) ;
#64400 = LINE ( 'NONE', #16294, #14745 ) ;
#64401 = FACE_OUTER_BOUND ( 'NONE', #17121, .T. ) ;
#64402 = EDGE_CURVE ( 'NONE', #42019, #28379, #32129, .T. ) ;
#64403 = ORIENTED_EDGE ( 'NONE', *, *, #3846, .F. ) ;
#64404 = CARTESIAN_POINT ( 'NONE',  ( 0.000000000000000000, 8.250000000000001776, -14.50000000000000000 ) ) ;
#64405 = AXIS2_PLACEMENT_3D ( 'NONE', #57020, #2232, #2933 ) ;
#64408 = ORIENTED_EDGE ( 'NONE', *, *, #32816, .F. ) ;
#64407 = EDGE_CURVE ( 'NONE', #57399, #40401, #54739, .T. ) ;
#64406 = CARTESIAN_POINT ( 'NONE',  ( -3.663616288757055806, 6.350872789121238426, 26.00000000000000711 ) ) ;
#64410 = ORIENTED_EDGE ( 'NONE', *, *, #26442, .F. ) ;
#64409 = DIRECTION ( 'NONE',  ( 0.000000000000000000, 1.000000000000000000, 0.000000000000000000 ) ) ;
#64411 = AXIS2_PLACEMENT_3D ( 'NONE', #57875, #9443, #31009 ) ;
#64412 = CARTESIAN_POINT ( 'NONE',  ( -29.50000000000000355, -11.50000000000000000, 15.00000000000000000 ) ) ;
#64413 = CARTESIAN_POINT ( 'NONE',  ( 49.00000000000000000, 20.60000000000000142, -13.86939075806900057 ) ) ;
#64414 = AXIS2_PLACEMENT_3D ( 'NONE', #42652, #3771, #46899 ) ;
#64415 = ORIENTED_EDGE ( 'NONE', *, *, #67903, .T. ) ;
#64416 = CARTESIAN_POINT ( 'NONE',  ( 283.0000000000000568, -28.94999999999999929, -13.50000000000000000 ) ) ;
#64417 = CARTESIAN_POINT ( 'NONE',  ( -4.188533722949335569, 7.259684009079808931, 455.0000000000000568 ) ) ;
#64418 = ORIENTED_EDGE ( 'NONE', *, *, #52783, .F. ) ;
#64419 = CARTESIAN_POINT ( 'NONE',  ( -17.00000000000000000, -17.50000000000000000, -15.70500000000000007 ) ) ;
#64420 = CARTESIAN_POINT ( 'NONE',  ( -10.19191654964671301, 11.07551654964660415, 195.0000000000000284 ) ) ;
#64421 = AXIS2_PLACEMENT_3D ( 'NONE', #52460, #13568, #35123 ) ;
#64422 = VERTEX_POINT ( 'NONE', #5271 ) ;
#64423 = CARTESIAN_POINT ( 'NONE',  ( 11.50000000000000000, -11.50000000000000000, -15.00000000000000000 ) ) ;
#64424 = ORIENTED_EDGE ( 'NONE', *, *, #15839, .T. ) ;
#64425 = EDGE_LOOP ( 'NONE', ( #5924, #1203, #5913, #53679 ) ) ;
#64426 = DIRECTION ( 'NONE',  ( -1.000000000000000000, 0.000000000000000000, 0.000000000000000000 ) ) ;
#64427 = AXIS2_PLACEMENT_3D ( 'NONE', #12697, #7053, #32907 ) ;
#64428 = CARTESIAN_POINT ( 'NONE',  ( 283.0000000000000568, -41.99999999999906208, -14.49999999999903899 ) ) ;
#64429 = DIRECTION ( 'NONE',  ( 7.665540703601096574E-15, 1.000000000000000000, -0.000000000000000000 ) ) ;
#64430 = LINE ( 'NONE', #64776, #26155 ) ;
#64431 = VERTEX_POINT ( 'NONE', #5609 ) ;
#64432 = ORIENTED_EDGE ( 'NONE', *, *, #9044, .T. ) ;
#64434 = ORIENTED_EDGE ( 'NONE', *, *, #32434, .T. ) ;
#64433 = FACE_OUTER_BOUND ( 'NONE', #6810, .T. ) ;
#64435 = ORIENTED_EDGE ( 'NONE', *, *, #69912, .T. ) ;
#64436 = EDGE_CURVE ( 'NONE', #61056, #53553, #22918, .T. ) ;
#64437 = CARTESIAN_POINT ( 'NONE',  ( 49.00000000000000000, -0.1999999999911430404, -8.864436962241481021E-12 ) ) ;
#64438 = FACE_OUTER_BOUND ( 'NONE', #40468, .T. ) ;
#64439 = VECTOR ( 'NONE', #12670, 1000.000000000000000 ) ;
#64440 = DIRECTION ( 'NONE',  ( 1.836970198721029934E-16, 1.836970198721010706E-16, -1.000000000000000000 ) ) ;
#64441 = EDGE_CURVE ( 'NONE', #55425, #64531, #27177, .T. ) ;
#64442 = LINE ( 'NONE', #16001, #15355 ) ;
#64444 = LINE ( 'NONE', #15305, #40202 ) ;
#64443 = FACE_OUTER_BOUND ( 'NONE', #32702, .T. ) ;
#64445 = EDGE_LOOP ( 'NONE', ( #27775, #59642, #24874, #9465, #34131, #46507 ) ) ;
#64446 = ADVANCED_FACE ( 'NONE', ( #6293, #27866 ), #49439, .T. ) ;
#64448 = ORIENTED_EDGE ( 'NONE', *, *, #66858, .F. ) ;
#64447 = DIRECTION ( 'NONE',  ( -0.000000000000000000, -0.000000000000000000, -1.000000000000000000 ) ) ;
#64449 = ORIENTED_EDGE ( 'NONE', *, *, #61950, .F. ) ;
#64450 = ORIENTED_EDGE ( 'NONE', *, *, #16728, .T. ) ;
#64451 = AXIS2_PLACEMENT_3D ( 'NONE', #20549, #32209, #10632 ) ;
#64452 = CYLINDRICAL_SURFACE ( 'NONE', #22072, 3.499999999999999556 ) ;
#64453 = EDGE_CURVE ( 'NONE', #62442, #18780, #10506, .T. ) ;
#64454 = DIRECTION ( 'NONE',  ( 1.062075597536821205E-14, 1.000000000000000000, 0.000000000000000000 ) ) ;
#64455 = CIRCLE ( 'NONE', #37342, 0.4999999999991867061 ) ;
#64456 = SHAPE_REPRESENTATION_RELATIONSHIP ( 'NONE' , 'NONE' ,  #1995, #14912 ) ;
#64457 = CARTESIAN_POINT ( 'NONE',  ( 14.25000000000000000, -2.500000000000000000, -21.77831216351300014 ) ) ;
#64458 = VECTOR ( 'NONE', #22295, 1000.000000000000000 ) ;
#64459 = EDGE_LOOP ( 'NONE', ( #42926, #48368, #62691, #62180 ) ) ;
#64460 = ORIENTED_EDGE ( 'NONE', *, *, #3863, .F. ) ;
#64461 = ORIENTED_EDGE ( 'NONE', *, *, #62526, .F. ) ;
#64462 = AXIS2_PLACEMENT_3D ( 'NONE', #59793, #15631, #58758 ) ;
#64463 = CARTESIAN_POINT ( 'NONE',  ( -28.00000000000000000, -16.28999999999710369, -15.00000000000794920 ) ) ;
#64464 = ORIENTED_EDGE ( 'NONE', *, *, #21973, .T. ) ;
#64465 = DIRECTION ( 'NONE',  ( -0.000000000000000000, -0.000000000000000000, -1.000000000000000000 ) ) ;
#64466 = DIRECTION ( 'NONE',  ( -0.000000000000000000, -0.000000000000000000, -1.000000000000000000 ) ) ;
#64467 = VERTEX_POINT ( 'NONE', #55093 ) ;
#64468 = VECTOR ( 'NONE', #38083, 1000.000000000000000 ) ;
#64469 = ADVANCED_FACE ( 'NONE', ( #24289 ), #29225, .F. ) ;
#64470 = ORIENTED_EDGE ( 'NONE', *, *, #54711, .F. ) ;
#64471 = DIRECTION ( 'NONE',  ( 0.000000000000000000, 0.000000000000000000, 1.000000000000000000 ) ) ;
#64472 = CARTESIAN_POINT ( 'NONE',  ( -1.466476262117318630, -9.404523737882838574, 26.00000000000000711 ) ) ;
#64473 = VERTEX_POINT ( 'NONE', #51153 ) ;
#64474 = AXIS2_PLACEMENT_3D ( 'NONE', #41892, #47553, #46840 ) ;
#64475 = DIRECTION ( 'NONE',  ( 0.7671651518153006499, -0.6414496315691565753, -2.356647714346250026E-16 ) ) ;
#64477 = ORIENTED_EDGE ( 'NONE', *, *, #4982, .T. ) ;
#64476 = DIRECTION ( 'NONE',  ( -1.000000000000000000, 0.000000000000000000, 0.000000000000000000 ) ) ;
#64478 = ORIENTED_EDGE ( 'NONE', *, *, #45185, .T. ) ;
#64480 = DIRECTION ( 'NONE',  ( -0.000000000000000000, 3.673940397442059868E-16, -1.000000000000000000 ) ) ;
#64479 = TOROIDAL_SURFACE ( 'NONE', #57696, 3.299999999999470024, 0.2000000000005275058 ) ;
#64481 = FACE_OUTER_BOUND ( 'NONE', #13132, .T. ) ;
#64482 = CARTESIAN_POINT ( 'NONE',  ( 9.404523737882817258, -1.480523737882815993, 26.00000000000000711 ) ) ;
#64483 = FACE_OUTER_BOUND ( 'NONE', #61514, .T. ) ;
#64484 = CARTESIAN_POINT ( 'NONE',  ( -7.250000000000001776, -7.249999999999998224, -12.00000000000000000 ) ) ;
#64485 = EDGE_CURVE ( 'NONE', #28718, #65641, #3744, .T. ) ;
#64486 = EDGE_LOOP ( 'NONE', ( #53412, #18827, #36346, #16037 ) ) ;
#64487 = CARTESIAN_POINT ( 'NONE',  ( -2.693516549646780334, -10.92648345035340895, 195.0000000000000284 ) ) ;
#64489 = ORIENTED_EDGE ( 'NONE', *, *, #27337, .T. ) ;
#64488 = EDGE_CURVE ( 'NONE', #50504, #27562, #21813, .T. ) ;
#64490 = DIRECTION ( 'NONE',  ( 0.000000000000000000, 0.000000000000000000, -1.000000000000000000 ) ) ;
#64491 = LINE ( 'NONE', #43947, #48144 ) ;
#64492 = CIRCLE ( 'NONE', #26077, 0.1999999999999996503 ) ;
#64493 = EDGE_CURVE ( 'NONE', #42459, #56941, #28558, .T. ) ;
#64494 = CARTESIAN_POINT ( 'NONE',  ( -7.250000000000001776, -7.249999999999998224, -9.500000000000001776 ) ) ;
#64495 = DIRECTION ( 'NONE',  ( 0.5001543609659999667, 1.060466075314215496E-16, 0.8659362650950080953 ) ) ;
#64496 = CARTESIAN_POINT ( 'NONE',  ( -8.916576262117345664, -8.580623737882765667, 54.00000000000000711 ) ) ;
#64497 = ORIENTED_EDGE ( 'NONE', *, *, #30529, .T. ) ;
#64498 = DIRECTION ( 'NONE',  ( -1.000000000000000000, 0.000000000000000000, 0.000000000000000000 ) ) ;
#64499 = VECTOR ( 'NONE', #53346, 1000.000000000000000 ) ;
#64500 = DIRECTION ( 'NONE',  ( -0.000000000000000000, -0.000000000000000000, 1.000000000000000000 ) ) ;
#64501 = AXIS2_PLACEMENT_3D ( 'NONE', #27509, #11235, #44440 ) ;
#64502 = VECTOR ( 'NONE', #29396, 1000.000000000000000 ) ;
#64503 = ORIENTED_EDGE ( 'NONE', *, *, #9036, .T. ) ;
#64504 = CARTESIAN_POINT ( 'NONE',  ( -7.450000000000001954, 7.250000000000000000, -17.00000000000000000 ) ) ;
#64505 = CARTESIAN_POINT ( 'NONE',  ( -6.350872789121313922, -3.677663764522584255, 26.00000000000000711 ) ) ;
#64506 = VECTOR ( 'NONE', #68222, 1000.000000000000000 ) ;
#64507 = VERTEX_POINT ( 'NONE', #2026 ) ;
#64508 = CARTESIAN_POINT ( 'NONE',  ( -7.250000000000000888, 7.250000000000001776, -19.50000000000000000 ) ) ;
#64509 = DIRECTION ( 'NONE',  ( -1.000000000000000000, 0.000000000000000000, 0.000000000000000000 ) ) ;
#64510 = VERTEX_POINT ( 'NONE', #23581 ) ;
#64511 = CARTESIAN_POINT ( 'NONE',  ( 8.093267424590459669, 8.697938382363064491, 54.00000000000000711 ) ) ;
#64512 = DIRECTION ( 'NONE',  ( -0.000000000000000000, -1.000000000000000000, -0.000000000000000000 ) ) ;
#64513 = AXIS2_PLACEMENT_3D ( 'NONE', #21018, #49628, #55288 ) ;
#64514 = CARTESIAN_POINT ( 'NONE',  ( 8.250000000000005329, 7.250000000000000888, -23.50000000000000000 ) ) ;
#64515 = LINE ( 'NONE', #43637, #11401 ) ;
#64516 = ORIENTED_EDGE ( 'NONE', *, *, #63702, .F. ) ;
#64518 = ORIENTED_EDGE ( 'NONE', *, *, #57640, .T. ) ;
#64517 = LINE ( 'NONE', #11111, #57688 ) ;
#64519 = VECTOR ( 'NONE', #11370, 1000.000000000000000 ) ;
#64520 = EDGE_CURVE ( 'NONE', #44220, #44549, #40190, .T. ) ;
#64521 = VECTOR ( 'NONE', #24722, 1000.000000000000000 ) ;
#64522 = CARTESIAN_POINT ( 'NONE',  ( -9.897976262117259338, 3.842976262117183683, 54.00000000000000711 ) ) ;
#64523 = DIRECTION ( 'NONE',  ( -0.8660254037844485886, 0.000000000000000000, -0.4999999999999827360 ) ) ;
#64524 = CARTESIAN_POINT ( 'NONE',  ( 9.404523737882758638, 1.466476262117154983, 54.00000000000000711 ) ) ;
#64525 = EDGE_LOOP ( 'NONE', ( #55411, #6838, #33570, #30185, #52067, #31662, #15551, #2834 ) ) ;
#64526 = EDGE_CURVE ( 'NONE', #51301, #4070, #12612, .T. ) ;
#64527 = VECTOR ( 'NONE', #31968, 1000.000000000000000 ) ;
#64528 = CARTESIAN_POINT ( 'NONE',  ( 30.00000000000000000, -5.599999999999379696, -26.60000000000059828 ) ) ;
#64529 = DIRECTION ( 'NONE',  ( 1.000000000000000000, -0.000000000000000000, 0.000000000000000000 ) ) ;
#64530 = EDGE_CURVE ( 'NONE', #61661, #27061, #28882, .T. ) ;
#64531 = VERTEX_POINT ( 'NONE', #17585 ) ;
#64532 = ORIENTED_EDGE ( 'NONE', *, *, #13414, .T. ) ;
#64533 = EDGE_CURVE ( 'NONE', #36733, #34015, #54587, .T. ) ;
#64534 = VERTEX_POINT ( 'NONE', #67436 ) ;
#64535 = EDGE_CURVE ( 'NONE', #15613, #59398, #13326, .T. ) ;
#64536 = EDGE_CURVE ( 'NONE', #13015, #2551, #1665, .T. ) ;
#64537 = DIRECTION ( 'NONE',  ( 1.034072152899300274E-14, 1.000000000000000000, 0.000000000000000000 ) ) ;
#64538 = FACE_OUTER_BOUND ( 'NONE', #23095, .T. ) ;
#64539 = DIRECTION ( 'NONE',  ( -1.000000000000000000, 0.000000000000000000, 0.000000000000000000 ) ) ;
#64540 = EDGE_CURVE ( 'NONE', #65447, #31143, #7105, .T. ) ;
#64541 = VECTOR ( 'NONE', #15064, 1000.000000000000000 ) ;
#64542 = ORIENTED_EDGE ( 'NONE', *, *, #52129, .T. ) ;
#64543 = ORIENTED_EDGE ( 'NONE', *, *, #33580, .F. ) ;
#64544 = DIRECTION ( 'NONE',  ( 0.000000000000000000, -1.000000000000000000, 0.000000000000000000 ) ) ;
#64545 = ORIENTED_EDGE ( 'NONE', *, *, #17161, .T. ) ;
#64546 = ORIENTED_EDGE ( 'NONE', *, *, #18820, .T. ) ;
#64547 = EDGE_LOOP ( 'NONE', ( #340, #15046, #17733, #20334 ) ) ;
#64548 = ORIENTED_EDGE ( 'NONE', *, *, #18680, .F. ) ;
#64549 = CARTESIAN_POINT ( 'NONE',  ( 289.5000000000000000, -0.5000000000000000000, 27.00000000000000000 ) ) ;
#64550 = CIRCLE ( 'NONE', #4685, 0.5249999999999994671 ) ;
#64552 = ORIENTED_EDGE ( 'NONE', *, *, #45135, .F. ) ;
#64551 = CARTESIAN_POINT ( 'NONE',  ( 6.006483450353379716, -8.211283450353491276, 455.0000000000000568 ) ) ;
#64553 = FACE_OUTER_BOUND ( 'NONE', #25404, .T. ) ;
#64554 = AXIS2_PLACEMENT_3D ( 'NONE', #37516, #21256, #734 ) ;
#64555 = CARTESIAN_POINT ( 'NONE',  ( 30.00000000000000000, -9.199999999999999289, 12.69999999999986073 ) ) ;
#64556 = DIRECTION ( 'NONE',  ( -7.751221965937476285E-17, 1.000000000000000000, -0.000000000000000000 ) ) ;
#64557 = EDGE_LOOP ( 'NONE', ( #2940, #35732, #38471, #19467 ) ) ;
#64558 = CIRCLE ( 'NONE', #13707, 1.000000000000000000 ) ;
#64559 = CLOSED_SHELL ( 'NONE', ( #849, #1036, #64446, #27249, #5443, #18962, #55418, #62594, #44550, #48120, #69823, #67729 ) ) ;
#64560 = LINE ( 'NONE', #31352, #50361 ) ;
#64561 = DIRECTION ( 'NONE',  ( -0.7071067811865300312, 0.000000000000000000, 0.7071067811865650032 ) ) ;
#64562 = ORIENTED_EDGE ( 'NONE', *, *, #68623, .T. ) ;
#64563 = CARTESIAN_POINT ( 'NONE',  ( 10.31452373788278187, 3.842976262117144159, 54.00000000000000711 ) ) ;
#64564 = DIRECTION ( 'NONE',  ( 1.000000000000000000, 0.000000000000000000, 0.000000000000000000 ) ) ;
#64565 = CARTESIAN_POINT ( 'NONE',  ( -7.250000000000001776, -7.249999999999998224, -21.50000000000000000 ) ) ;
#64566 = ORIENTED_EDGE ( 'NONE', *, *, #5830, .T. ) ;
#64567 = EDGE_CURVE ( 'NONE', #44397, #56086, #18408, .T. ) ;
#64568 = FACE_OUTER_BOUND ( 'NONE', #58408, .T. ) ;
#64569 = EDGE_CURVE ( 'NONE', #41347, #57661, #61398, .T. ) ;
#64570 = CARTESIAN_POINT ( 'NONE',  ( -11.99351654964671354, 7.813516549646603693, 195.0000000000000284 ) ) ;
#64571 = PLANE ( 'NONE',  #52835 ) ;
#64572 = EDGE_CURVE ( 'NONE', #44582, #47818, #33842, .T. ) ;
#64573 = LINE ( 'NONE', #26743, #20703 ) ;
#64574 = CARTESIAN_POINT ( 'NONE',  ( 30.00000000000000000, -11.50000000000082068, -10.20500000000000007 ) ) ;
#64575 = PLANE ( 'NONE',  #22655 ) ;
#64576 = DIRECTION ( 'NONE',  ( -1.000000000000000000, 0.000000000000000000, 0.000000000000000000 ) ) ;
#64577 = DIRECTION ( 'NONE',  ( -1.000000000000000000, 3.491481338843133355E-15, 0.000000000000000000 ) ) ;
#64578 = ORIENTED_EDGE ( 'NONE', *, *, #52389, .F. ) ;
#64579 = FACE_OUTER_BOUND ( 'NONE', #45467, .T. ) ;
#64580 = CARTESIAN_POINT ( 'NONE',  ( 7.250000000000005329, 7.250000000000000888, -16.00000000000000000 ) ) ;
#64581 = DIRECTION ( 'NONE',  ( 1.000000000000000000, 0.000000000000000000, 0.000000000000000000 ) ) ;
#64582 = DIRECTION ( 'NONE',  ( 0.000000000000000000, 1.000000000000000000, 0.000000000000000000 ) ) ;
#64583 = ORIENTED_EDGE ( 'NONE', *, *, #4491, .F. ) ;
#64584 = DIRECTION ( 'NONE',  ( 0.000000000000000000, 0.000000000000000000, -1.000000000000000000 ) ) ;
#64585 = LINE ( 'NONE', #47973, #23748 ) ;
#64586 = DIRECTION ( 'NONE',  ( 1.000000000000000000, 0.000000000000000000, 0.000000000000000000 ) ) ;
#64587 = DIRECTION ( 'NONE',  ( 0.000000000000000000, 0.000000000000000000, -1.000000000000000000 ) ) ;
#64588 =( NAMED_UNIT ( * ) SI_UNIT ( $, .STERADIAN. ) SOLID_ANGLE_UNIT ( ) );
#64589 = CARTESIAN_POINT ( 'NONE',  ( -7.250000000000001776, -7.249999999999998224, -23.50000000000000000 ) ) ;
#64590 = VECTOR ( 'NONE', #24462, 1000.000000000000000 ) ;
#64591 = EDGE_LOOP ( 'NONE', ( #60395, #17210, #30383, #30986, #30882, #16100, #19556, #24903 ) ) ;
#64592 = ORIENTED_EDGE ( 'NONE', *, *, #18471, .T. ) ;
#64593 = FACE_OUTER_BOUND ( 'NONE', #54156, .T. ) ;
#64594 = CARTESIAN_POINT ( 'NONE',  ( 30.00000000000000000, -5.200000000000001066, 26.59999999999999787 ) ) ;
#64595 = EDGE_LOOP ( 'NONE', ( #4563, #31809, #68710, #56670 ) ) ;
#64596 = CARTESIAN_POINT ( 'NONE',  ( -29.50000000000000355, -11.50000000000100009, 10.50000000000065903 ) ) ;
#64597 = CARTESIAN_POINT ( 'NONE',  ( -8.250000000000001776, 0.000000000000000000, -12.50000000000000000 ) ) ;
#64598 = EDGE_LOOP ( 'NONE', ( #7889, #6781, #48583, #3116 ) ) ;
#64599 = AXIS2_PLACEMENT_3D ( 'NONE', #51107, #45798, #24939 ) ;
#64600 = AXIS2_PLACEMENT_3D ( 'NONE', #16595, #49108, #4939 ) ;
#64601 = LINE ( 'NONE', #10854, #4104 ) ;
#64602 = ORIENTED_EDGE ( 'NONE', *, *, #25580, .T. ) ;
#64603 = ORIENTED_EDGE ( 'NONE', *, *, #68120, .T. ) ;
#64604 = CARTESIAN_POINT ( 'NONE',  ( 7.250000000000005329, -7.249999999999998224, -21.50000000000000000 ) ) ;
#64605 = EDGE_CURVE ( 'NONE', #69141, #27966, #50112, .T. ) ;
#64606 = ORIENTED_EDGE ( 'NONE', *, *, #3139, .T. ) ;
#64607 = VECTOR ( 'NONE', #44150, 1000.000000000000000 ) ;
#64608 = FACE_OUTER_BOUND ( 'NONE', #38693, .T. ) ;
#64609 = DIRECTION ( 'NONE',  ( -0.000000000000000000, -0.000000000000000000, 1.000000000000000000 ) ) ;
#64610 = CARTESIAN_POINT ( 'NONE',  ( 25.50000000000000355, -15.50000000000000000, -22.50000000000000000 ) ) ;
#64611 = ADVANCED_FACE ( 'NONE', ( #18623 ), #66382, .F. ) ;
#64612 = ORIENTED_EDGE ( 'NONE', *, *, #56578, .T. ) ;
#64613 = ORIENTED_EDGE ( 'NONE', *, *, #909, .T. ) ;
#64614 = FACE_OUTER_BOUND ( 'NONE', #3919, .T. ) ;
#64615 = AXIS2_PLACEMENT_3D ( 'NONE', #49089, #50120, #54747 ) ;
#64617 = LINE ( 'NONE', #20432, #20946 ) ;
#64616 = LINE ( 'NONE', #38105, #66573 ) ;
#64618 = ORIENTED_EDGE ( 'NONE', *, *, #69626, .F. ) ;
#64619 = VERTEX_POINT ( 'NONE', #34878 ) ;
#64620 = ORIENTED_EDGE ( 'NONE', *, *, #23655, .F. ) ;
#64621 = LINE ( 'NONE', #10879, #63853 ) ;
#64622 = EDGE_CURVE ( 'NONE', #59771, #30313, #8009, .T. ) ;
#64624 = ORIENTED_EDGE ( 'NONE', *, *, #24946, .F. ) ;
#64623 = CARTESIAN_POINT ( 'NONE',  ( -9.293516549646827940, -10.92648345035338764, 455.0000000000000568 ) ) ;
#64625 = DIRECTION ( 'NONE',  ( 1.000000000000000000, 0.000000000000000000, 0.000000000000000000 ) ) ;
#64626 = FACE_OUTER_BOUND ( 'NONE', #61553, .T. ) ;
#64627 = ORIENTED_EDGE ( 'NONE', *, *, #11503, .T. ) ;
#64628 = ORIENTED_EDGE ( 'NONE', *, *, #11103, .F. ) ;
#64629 = DIRECTION ( 'NONE',  ( 0.000000000000000000, 3.673940397442059868E-16, -1.000000000000000000 ) ) ;
#64630 = ORIENTED_EDGE ( 'NONE', *, *, #13448, .F. ) ;
#64631 = DIRECTION ( 'NONE',  ( 0.000000000000000000, 0.000000000000000000, 1.000000000000000000 ) ) ;
#64632 = LINE ( 'NONE', #10891, #34499 ) ;
#64633 = VECTOR ( 'NONE', #60022, 1000.000000000000000 ) ;
#64634 = ORIENTED_EDGE ( 'NONE', *, *, #47067, .F. ) ;
#64635 = CARTESIAN_POINT ( 'NONE',  ( 2.420780051175163816, 8.697938382363089360, 26.00000000000000711 ) ) ;
#64636 = CYLINDRICAL_SURFACE ( 'NONE', #4192, 0.3499999999999996447 ) ;
#64638 = VERTEX_POINT ( 'NONE', #47607 ) ;
#64637 = CARTESIAN_POINT ( 'NONE',  ( -9.722976262117256852, 7.955476262117183062, 26.00000000000000711 ) ) ;
#64639 = ORIENTED_EDGE ( 'NONE', *, *, #66010, .T. ) ;
#64640 = AXIS2_PLACEMENT_3D ( 'NONE', #440, #11381, #59134 ) ;
#64641 = FACE_OUTER_BOUND ( 'NONE', #45570, .T. ) ;
#64642 = DIRECTION ( 'NONE',  ( 0.000000000000000000, 1.000000000000000000, 0.000000000000000000 ) ) ;
#64643 = DIRECTION ( 'NONE',  ( 0.000000000000000000, 0.000000000000000000, 1.000000000000000000 ) ) ;
#64644 = AXIS2_PLACEMENT_3D ( 'NONE', #178, #22767, #22433 ) ;
#64645 = DIRECTION ( 'NONE',  ( -1.000000000000000000, 0.000000000000000000, 0.000000000000000000 ) ) ;
#64646 = EDGE_CURVE ( 'NONE', #58210, #1231, #29935, .T. ) ;
#64647 = LINE ( 'NONE', #1004, #47755 ) ;
#64648 = ORIENTED_EDGE ( 'NONE', *, *, #14884, .T. ) ;
#64649 = FACE_OUTER_BOUND ( 'NONE', #104, .T. ) ;
#64650 = PLANE ( 'NONE',  #15790 ) ;
#64651 = LINE ( 'NONE', #37789, #7413 ) ;
#64653 = ORIENTED_EDGE ( 'NONE', *, *, #41193, .T. ) ;
#64652 = PLANE ( 'NONE',  #28841 ) ;
#64654 = VECTOR ( 'NONE', #52884, 999.9999999999998863 ) ;
#64655 = LINE ( 'NONE', #37794, #22476 ) ;
#64656 = DIRECTION ( 'NONE',  ( -0.000000000000000000, -0.000000000000000000, -1.000000000000000000 ) ) ;
#64657 = VECTOR ( 'NONE', #15453, 1000.000000000000114 ) ;
#64658 = EDGE_CURVE ( 'NONE', #69392, #30786, #52207, .T. ) ;
#64659 = DIRECTION ( 'NONE',  ( -1.000000000000000000, 0.000000000000000000, 0.000000000000000000 ) ) ;
#64660 = AXIS2_PLACEMENT_3D ( 'NONE', #60054, #34556, #27884 ) ;
#64661 = ORIENTED_EDGE ( 'NONE', *, *, #58052, .F. ) ;
#64662 = CARTESIAN_POINT ( 'NONE',  ( -15.50000000000000000, -0.2038245569916614930, 21.05662432702600029 ) ) ;
#64663 = DIRECTION ( 'NONE',  ( 1.000000000000000000, 0.000000000000000000, 0.000000000000000000 ) ) ;
#64664 = ORIENTED_EDGE ( 'NONE', *, *, #17731, .F. ) ;
#64665 = DIRECTION ( 'NONE',  ( 0.000000000000000000, 0.000000000000000000, -1.000000000000000000 ) ) ;
#64666 = DIRECTION ( 'NONE',  ( 1.000000000000000000, 0.000000000000000000, 0.000000000000000000 ) ) ;
#64667 = FACE_OUTER_BOUND ( 'NONE', #10030, .T. ) ;
#64668 = EDGE_CURVE ( 'NONE', #10176, #5167, #41952, .T. ) ;
#64669 = AXIS2_PLACEMENT_3D ( 'NONE', #43419, #11240, #65687 ) ;
#64670 = DIRECTION ( 'NONE',  ( -0.000000000000000000, 1.000000000000000000, -0.000000000000000000 ) ) ;
#64671 = CARTESIAN_POINT ( 'NONE',  ( 39.00000000000000000, 0.000000000000000000, 0.000000000000000000 ) ) ;
#64672 = CIRCLE ( 'NONE', #24026, 1.929199999999998028 ) ;
#64673 = ORIENTED_EDGE ( 'NONE', *, *, #20555, .T. ) ;
#64674 = VERTEX_POINT ( 'NONE', #58216 ) ;
#64675 = DIRECTION ( 'NONE',  ( 0.000000000000000000, 0.7071067811865474617, -0.7071067811865474617 ) ) ;
#64676 = VERTEX_POINT ( 'NONE', #8729 ) ;
#64677 = ORIENTED_EDGE ( 'NONE', *, *, #51335, .T. ) ;
#64678 = CARTESIAN_POINT ( 'NONE',  ( 7.450000000000004619, -1.336933437520057563E-15, -13.00000000000000178 ) ) ;
#64679 = AXIS2_PLACEMENT_3D ( 'NONE', #68410, #31639, #19964 ) ;
#64680 = DIRECTION ( 'NONE',  ( -0.000000000000000000, -0.000000000000000000, -1.000000000000000000 ) ) ;
#64681 = DIRECTION ( 'NONE',  ( 0.000000000000000000, 0.000000000000000000, 1.000000000000000000 ) ) ;
#64682 = ORIENTED_EDGE ( 'NONE', *, *, #37480, .T. ) ;
#64683 = EDGE_LOOP ( 'NONE', ( #60345, #26877, #58386, #4810 ) ) ;
#64684 = AXIS2_PLACEMENT_3D ( 'NONE', #6564, #1581, #60972 ) ;
#64685 = CARTESIAN_POINT ( 'NONE',  ( 7.000000000000000000, -28.95000000000155183, -14.49999999999845990 ) ) ;
#64686 = ORIENTED_EDGE ( 'NONE', *, *, #68656, .T. ) ;
#64687 = ORIENTED_EDGE ( 'NONE', *, *, #16397, .F. ) ;
#64688 = EDGE_CURVE ( 'NONE', #10538, #11799, #46896, .T. ) ;
#64689 = DIRECTION ( 'NONE',  ( 0.000000000000000000, 0.000000000000000000, -1.000000000000000000 ) ) ;
#64690 = DIRECTION ( 'NONE',  ( 0.000000000000000000, -1.000000000000000000, 0.000000000000000000 ) ) ;
#64691 = CARTESIAN_POINT ( 'NONE',  ( 8.250000000000005329, -8.249999999999998224, -26.00000000000001066 ) ) ;
#64692 = ADVANCED_FACE ( 'NONE', ( #52573 ), #8360, .F. ) ;
#64693 = EDGE_CURVE ( 'NONE', #15959, #27077, #30299, .T. ) ;
#64694 = VERTEX_POINT ( 'NONE', #56805 ) ;
#64695 = VECTOR ( 'NONE', #53410, 1000.000000000000000 ) ;
#64696 = CARTESIAN_POINT ( 'NONE',  ( 283.0000000000000568, -37.61196062927500350, 8.008708659369300875 ) ) ;
#64698 = CARTESIAN_POINT ( 'NONE',  ( -11.00000000000000000, -17.50000000000000000, 15.70499999999969809 ) ) ;
#64697 = LINE ( 'NONE', #32871, #64889 ) ;
#64699 = VERTEX_POINT ( 'NONE', #36647 ) ;
#64700 = ORIENTED_EDGE ( 'NONE', *, *, #34967, .T. ) ;
#64703 = ORIENTED_EDGE ( 'NONE', *, *, #59780, .T. ) ;
#64702 = EDGE_CURVE ( 'NONE', #31249, #39691, #41036, .T. ) ;
#64701 = DIRECTION ( 'NONE',  ( 1.000000000000000000, 0.000000000000000000, 0.000000000000000000 ) ) ;
#64704 = VERTEX_POINT ( 'NONE', #14734 ) ;
#64705 = EDGE_CURVE ( 'NONE', #48543, #37936, #25709, .T. ) ;
#64706 = EDGE_CURVE ( 'NONE', #35602, #44169, #57162, .T. ) ;
#64707 = DIRECTION ( 'NONE',  ( 0.000000000000000000, 0.000000000000000000, -1.000000000000000000 ) ) ;
#64708 = ADVANCED_FACE ( 'NONE', ( #36296 ), #31370, .F. ) ;
#64709 = LINE ( 'NONE', #66352, #42872 ) ;
#64710 = AXIS2_PLACEMENT_3D ( 'NONE', #58788, #37918, #59479 ) ;
#64711 = VERTEX_POINT ( 'NONE', #19668 ) ;
#64712 = ORIENTED_EDGE ( 'NONE', *, *, #36878, .F. ) ;
#64713 = CIRCLE ( 'NONE', #59111, 24.99999999998784972 ) ;
#64715 = DIRECTION ( 'NONE',  ( -1.000000000000000000, 3.491481338843132961E-15, 1.836970198721036344E-16 ) ) ;
#64714 = AXIS2_PLACEMENT_3D ( 'NONE', #63188, #67454, #2732 ) ;
#64716 = LINE ( 'NONE', #43838, #37966 ) ;
#64717 = ORIENTED_EDGE ( 'NONE', *, *, #68420, .T. ) ;
#64718 = ORIENTED_EDGE ( 'NONE', *, *, #23833, .F. ) ;
#64719 = DIRECTION ( 'NONE',  ( -1.000000000000000000, 0.000000000000000000, 0.000000000000000000 ) ) ;
#64720 = DIRECTION ( 'NONE',  ( -1.000000000000000000, 0.000000000000000000, 0.000000000000000000 ) ) ;
#64721 = VECTOR ( 'NONE', #4828, 1000.000000000000000 ) ;
#64722 = FACE_OUTER_BOUND ( 'NONE', #51346, .T. ) ;
#64723 = ORIENTED_EDGE ( 'NONE', *, *, #29409, .F. ) ;
#64724 = CIRCLE ( 'NONE', #62426, 0.3499999999999996447 ) ;
#64725 = FACE_OUTER_BOUND ( 'NONE', #48394, .T. ) ;
#64726 = EDGE_CURVE ( 'NONE', #7495, #19227, #51175, .T. ) ;
#64727 = DIRECTION ( 'NONE',  ( 0.000000000000000000, 1.000000000000000000, 0.000000000000000000 ) ) ;
#64729 = VERTEX_POINT ( 'NONE', #35581 ) ;
#64728 = DIRECTION ( 'NONE',  ( -1.000000000000000000, 0.000000000000000000, 0.000000000000000000 ) ) ;
#64731 = ORIENTED_EDGE ( 'NONE', *, *, #44270, .T. ) ;
#64730 = LINE ( 'NONE', #9956, #22200 ) ;
#64732 = CARTESIAN_POINT ( 'NONE',  ( -9.293516549646710700, 10.08346604330776941, 455.0000000000000568 ) ) ;
#64733 = DIRECTION ( 'NONE',  ( 0.6414496315691494699, -0.7671651518153064231, 0.000000000000000000 ) ) ;
#64734 = AXIS2_PLACEMENT_3D ( 'NONE', #37211, #33285, #42503 ) ;
#64735 = CARTESIAN_POINT ( 'NONE',  ( 17.51999999999999957, -15.50000000000000000, -26.00000000000000355 ) ) ;
#64736 = CARTESIAN_POINT ( 'NONE',  ( 6.657023737882818537, -9.912023737882819319, 54.00000000000000711 ) ) ;
#64737 = EDGE_CURVE ( 'NONE', #18477, #57396, #19328, .T. ) ;
#64738 = CARTESIAN_POINT ( 'NONE',  ( 283.0000000000000568, -29.94999999999999929, -14.50000000000000000 ) ) ;
#64739 = CARTESIAN_POINT ( 'NONE',  ( 6.006483450353379716, -3.606483450353394904, 195.0000000000000284 ) ) ;
#64740 = CONICAL_SURFACE ( 'NONE', #21832, 1732.050807568789651, 1.047197551196575871 ) ;
#64741 = ORIENTED_EDGE ( 'NONE', *, *, #31630, .F. ) ;
#64742 = LINE ( 'NONE', #64070, #29289 ) ;
#64744 = ORIENTED_EDGE ( 'NONE', *, *, #42128, .T. ) ;
#64743 = LINE ( 'NONE', #48486, #6274 ) ;
#64746 = VERTEX_POINT ( 'NONE', #41243 ) ;
#64745 = DIRECTION ( 'NONE',  ( -1.062171939662868249E-14, -1.000000000000000000, 0.000000000000000000 ) ) ;
#64747 = DIRECTION ( 'NONE',  ( -0.000000000000000000, -0.000000000000000000, -1.000000000000000000 ) ) ;
#64748 = VECTOR ( 'NONE', #2421, 1000.000000000000000 ) ;
#64749 = CARTESIAN_POINT ( 'NONE',  ( -8.333516549646715177, 11.11351654964659730, 455.0000000000000568 ) ) ;
#64750 = VERTEX_POINT ( 'NONE', #62818 ) ;
#64751 = LINE ( 'NONE', #21961, #6063 ) ;
#64752 = DIRECTION ( 'NONE',  ( -0.000000000000000000, -1.000000000000000000, -0.000000000000000000 ) ) ;
#64753 = VERTEX_POINT ( 'NONE', #14023 ) ;
#64754 = LINE ( 'NONE', #21964, #13096 ) ;
#64755 = DIRECTION ( 'NONE',  ( 1.836970198721029934E-16, -1.836970198721036344E-16, 1.000000000000000000 ) ) ;
#64756 = FILL_AREA_STYLE_COLOUR ( '', #35913 ) ;
#64757 = EDGE_CURVE ( 'NONE', #12819, #53577, #35949, .T. ) ;
#64758 = CIRCLE ( 'NONE', #4956, 25.39999999999999858 ) ;
#64759 = ORIENTED_EDGE ( 'NONE', *, *, #16421, .F. ) ;
#64760 = CARTESIAN_POINT ( 'NONE',  ( -3.142976262117262998, -4.046023737882823212, 26.00000000000000711 ) ) ;
#64761 = ORIENTED_EDGE ( 'NONE', *, *, #24197, .F. ) ;
#64762 = EDGE_CURVE ( 'NONE', #48516, #18370, #9077, .T. ) ;
#64763 = ORIENTED_EDGE ( 'NONE', *, *, #28435, .T. ) ;
#64764 = ADVANCED_FACE ( 'NONE', ( #9426 ), #30995, .F. ) ;
#64765 = AXIS2_PLACEMENT_3D ( 'NONE', #48067, #42060, #65030 ) ;
#64766 = DIRECTION ( 'NONE',  ( 1.000000000000000000, -0.000000000000000000, 0.000000000000000000 ) ) ;
#64767 = DIRECTION ( 'NONE',  ( -1.000000000000000000, 0.000000000000000000, 0.000000000000000000 ) ) ;
#64768 = STYLED_ITEM ( 'NONE', ( #26680 ), #66294 ) ;
#64769 = AXIS2_PLACEMENT_3D ( 'NONE', #23388, #66519, #32625 ) ;
#64770 = EDGE_CURVE ( 'NONE', #69700, #64422, #26052, .T. ) ;
#64771 = ADVANCED_FACE ( 'NONE', ( #31708 ), #21086, .F. ) ;
#64772 = ADVANCED_FACE ( 'NONE', ( #42649 ), #26391, .T. ) ;
#64773 = FACE_OUTER_BOUND ( 'NONE', #57502, .T. ) ;
#64774 = AXIS2_PLACEMENT_3D ( 'NONE', #7659, #38798, #60017 ) ;
#64775 = AXIS2_PLACEMENT_3D ( 'NONE', #6214, #39759, #50028 ) ;
#64776 = CARTESIAN_POINT ( 'NONE',  ( 30.00000000000000000, -14.04000000000000092, 14.80000000000000071 ) ) ;
#64777 = ORIENTED_EDGE ( 'NONE', *, *, #64835, .T. ) ;
#64778 = ORIENTED_EDGE ( 'NONE', *, *, #39307, .T. ) ;
#64780 = ORIENTED_EDGE ( 'NONE', *, *, #14601, .T. ) ;
#64779 = CARTESIAN_POINT ( 'NONE',  ( 41.09999999999999432, 14.08845687959340331, 21.00000000000000000 ) ) ;
#64781 = EDGE_CURVE ( 'NONE', #829, #15324, #69867, .T. ) ;
#64782 = ORIENTED_EDGE ( 'NONE', *, *, #20014, .T. ) ;
#64783 = CARTESIAN_POINT ( 'NONE',  ( 7.826483450353380000, -12.00648345035339659, 195.0000000000000284 ) ) ;
#64784 = CARTESIAN_POINT ( 'NONE',  ( 10.92648345035331303, 2.693516549646575609, 195.0000000000000284 ) ) ;
#64785 = EDGE_CURVE ( 'NONE', #6993, #17846, #33113, .T. ) ;
#64786 = DIRECTION ( 'NONE',  ( -1.000000000000000000, 0.000000000000000000, 0.000000000000000000 ) ) ;
#64787 = ADVANCED_FACE ( 'NONE', ( #10130 ), #54312, .F. ) ;
#64788 = CARTESIAN_POINT ( 'NONE',  ( 9.912023737882783792, 3.842976262117149044, 54.00000000000000711 ) ) ;
#64790 = CARTESIAN_POINT ( 'NONE',  ( 7.852485183456931139, -3.430747519065418860, 455.0000000000000568 ) ) ;
#64789 = DIRECTION ( 'NONE',  ( 0.000000000000000000, -1.000000000000000000, 0.000000000000000000 ) ) ;
#64791 = ORIENTED_EDGE ( 'NONE', *, *, #16709, .T. ) ;
#64793 = VERTEX_POINT ( 'NONE', #32047 ) ;
#64792 = CARTESIAN_POINT ( 'NONE',  ( -8.689999999999999503, -8.750000000000000000, -7.000000000000000000 ) ) ;
#64794 = ORIENTED_EDGE ( 'NONE', *, *, #39303, .T. ) ;
#64795 = ORIENTED_EDGE ( 'NONE', *, *, #47321, .F. ) ;
#64796 = SHAPE_REPRESENTATION ( 'Part3', ( #45918 ), #6462 ) ;
#64797 = CARTESIAN_POINT ( 'NONE',  ( 7.826483450353421745, 11.77351654964657257, 455.0000000000000568 ) ) ;
#64798 = ADVANCED_FACE ( 'NONE', ( #16481 ), #69524, .F. ) ;
#64799 = DIRECTION ( 'NONE',  ( 1.000000000000000000, -0.000000000000000000, 0.000000000000000000 ) ) ;
#64801 = EDGE_CURVE ( 'NONE', #6004, #24879, #42994, .T. ) ;
#64800 = DIRECTION ( 'NONE',  ( 0.000000000000000000, 0.000000000000000000, 1.000000000000000000 ) ) ;
#64802 = LINE ( 'NONE', #16017, #27512 ) ;
#64803 = ORIENTED_EDGE ( 'NONE', *, *, #6566, .T. ) ;
#64804 = ORIENTED_EDGE ( 'NONE', *, *, #53905, .T. ) ;
#64805 = ORIENTED_EDGE ( 'NONE', *, *, #54001, .T. ) ;
#64806 = CIRCLE ( 'NONE', #35391, 0.3499999999999611200 ) ;
#64807 = DIRECTION ( 'NONE',  ( 0.000000000000000000, -0.7046037717859411353, -0.7096009616573427659 ) ) ;
#64808 = LINE ( 'NONE', #54548, #1562 ) ;
#64809 = DIRECTION ( 'NONE',  ( 1.000000000000000000, -0.000000000000000000, 0.000000000000000000 ) ) ;
#64810 = EDGE_CURVE ( 'NONE', #66383, #33102, #16164, .T. ) ;
#64811 = ORIENTED_EDGE ( 'NONE', *, *, #60394, .T. ) ;
#64812 = ORIENTED_EDGE ( 'NONE', *, *, #43729, .T. ) ;
#64813 = DIRECTION ( 'NONE',  ( -1.000000000000000000, 0.000000000000000000, 0.000000000000000000 ) ) ;
#64814 = APPLICATION_CONTEXT ( 'automotive_design' ) ;
#64815 = DIRECTION ( 'NONE',  ( 0.000000000000000000, 0.000000000000000000, -1.000000000000000000 ) ) ;
#64816 = EDGE_LOOP ( 'NONE', ( #45886, #31262, #21529, #8318, #13884, #42216, #4061, #2159, #19202, #29704, #33200, #56338, #11556, #50533, #4889, #44811, #48954 ) ) ;
#64817 = AXIS2_PLACEMENT_3D ( 'NONE', #27878, #2039, #24656 ) ;
#64818 = VECTOR ( 'NONE', #50678, 1000.000000000000000 ) ;
#64819 = CARTESIAN_POINT ( 'NONE',  ( 7.272650909786598561, -7.811466277050764795, 195.0000000000000284 ) ) ;
#64821 = EDGE_LOOP ( 'NONE', ( #28456, #19235, #55804, #27314 ) ) ;
#64820 = CARTESIAN_POINT ( 'NONE',  ( 25.50000000000000355, -15.12100000000000044, -22.50000000000000000 ) ) ;
#64822 = VERTEX_POINT ( 'NONE', #43335 ) ;
#64823 = CARTESIAN_POINT ( 'NONE',  ( 8.711985858128644011, 2.406732575409517239, 54.00000000000000711 ) ) ;
#64824 = DIRECTION ( 'NONE',  ( -1.836970198721029934E-16, -1.836970198721010706E-16, 1.000000000000000000 ) ) ;
#64825 = AXIS2_PLACEMENT_3D ( 'NONE', #13877, #51356, #24843 ) ;
#64826 = VECTOR ( 'NONE', #6557, 1000.000000000000000 ) ;
#64827 = CARTESIAN_POINT ( 'NONE',  ( -5.242976262117275077, -5.257023737882800418, 26.00000000000000711 ) ) ;
#64828 = CYLINDRICAL_SURFACE ( 'NONE', #17653, 0.5999999999999998668 ) ;
#64829 = EDGE_CURVE ( 'NONE', #49752, #42154, #64573, .T. ) ;
#64830 = CARTESIAN_POINT ( 'NONE',  ( 8.580623737882818958, -8.930623737882845248, 26.00000000000000000 ) ) ;
#64831 = VECTOR ( 'NONE', #38265, 1000.000000000000114 ) ;
#64832 = VECTOR ( 'NONE', #28909, 1000.000000000000114 ) ;
#64833 = ORIENTED_EDGE ( 'NONE', *, *, #8648, .T. ) ;
#64834 = CARTESIAN_POINT ( 'NONE',  ( -9.722976262117294155, -6.832023737882757963, 54.00000000000000711 ) ) ;
#64835 = EDGE_CURVE ( 'NONE', #57460, #18304, #27081, .T. ) ;
#64836 = ORIENTED_EDGE ( 'NONE', *, *, #43279, .F. ) ;
#64837 = FACE_OUTER_BOUND ( 'NONE', #62360, .T. ) ;
#64838 = CARTESIAN_POINT ( 'NONE',  ( 9.417013320880768035, 1.853252480934615809, 455.0000000000000568 ) ) ;
#64840 = EDGE_CURVE ( 'NONE', #50433, #48836, #37698, .T. ) ;
#64839 = CARTESIAN_POINT ( 'NONE',  ( -3.142976262117261221, 4.031976262117183296, 26.00000000000000711 ) ) ;
#64841 = CIRCLE ( 'NONE', #38871, 0.5000000000009302559 ) ;
#64842 = LINE ( 'NONE', #43610, #41949 ) ;
#64843 = LINE ( 'NONE', #64496, #34766 ) ;
#64844 = EDGE_CURVE ( 'NONE', #28520, #64473, #32401, .T. ) ;
#64845 = VERTEX_POINT ( 'NONE', #563 ) ;
#64846 = CYLINDRICAL_SURFACE ( 'NONE', #3107, 1.000000000000000000 ) ;
#64847 = EDGE_CURVE ( 'NONE', #66802, #13113, #38766, .T. ) ;
#64848 = DIRECTION ( 'NONE',  ( 1.000000000000000000, 0.000000000000000000, -0.000000000000000000 ) ) ;
#64849 = ORIENTED_EDGE ( 'NONE', *, *, #2200, .T. ) ;
#64850 = DIRECTION ( 'NONE',  ( -1.000000000000000000, 0.000000000000000000, 0.000000000000000000 ) ) ;
#64851 = CARTESIAN_POINT ( 'NONE',  ( -11.00000000000000000, -5.599999999999379696, -26.60000000000059828 ) ) ;
#64852 = ORIENTED_EDGE ( 'NONE', *, *, #63518, .F. ) ;
#64853 = ADVANCED_FACE ( 'NONE', ( #32731 ), #27432, .F. ) ;
#64854 = DIRECTION ( 'NONE',  ( 0.000000000000000000, 0.000000000000000000, 1.000000000000000000 ) ) ;
#64855 = DIRECTION ( 'NONE',  ( 0.000000000000000000, 1.000000000000000000, -0.000000000000000000 ) ) ;
#64856 = EDGE_LOOP ( 'NONE', ( #53293, #44883, #26272, #62328 ) ) ;
#64857 = CARTESIAN_POINT ( 'NONE',  ( 15.50000000000000000, -15.50000000000000000, -22.50000000000000000 ) ) ;
#64858 = AXIS2_PLACEMENT_3D ( 'NONE', #34987, #50908, #24395 ) ;
#64859 = DIRECTION ( 'NONE',  ( -1.000000000000000000, -1.671920889371702854E-15, -0.000000000000000000 ) ) ;
#64860 = EDGE_CURVE ( 'NONE', #59223, #43564, #26364, .T. ) ;
#64861 = LINE ( 'NONE', #12135, #18505 ) ;
#64862 = DIRECTION ( 'NONE',  ( 3.717264591378875951E-15, 1.000000000000000000, 0.000000000000000000 ) ) ;
#64863 = ORIENTED_EDGE ( 'NONE', *, *, #18939, .F. ) ;
#64865 = ORIENTED_EDGE ( 'NONE', *, *, #51136, .F. ) ;
#64864 = CARTESIAN_POINT ( 'NONE',  ( -7.259684009079930611, 7.798499376343971612, 195.0000000000000284 ) ) ;
#64866 = ADVANCED_FACE ( 'NONE', ( #11499, #33080 ), #54657, .T. ) ;
#64867 = CIRCLE ( 'NONE', #33263, 0.1999999999999996503 ) ;
#64868 = CARTESIAN_POINT ( 'NONE',  ( 3.157023737882804770, 6.486996718459879574, 54.00000000000000711 ) ) ;
#64869 = CARTESIAN_POINT ( 'NONE',  ( 4.456444791733522252E-16, 7.450000000000002842, -14.50000000000000000 ) ) ;
#64870 = CARTESIAN_POINT ( 'NONE',  ( 0.000000000000000000, 8.250000000000001776, -13.00000000000000178 ) ) ;
#64871 = ORIENTED_EDGE ( 'NONE', *, *, #68969, .F. ) ;
#64872 = CARTESIAN_POINT ( 'NONE',  ( 41.09999999999999432, 20.60000000000000142, -13.86939075806900057 ) ) ;
#64873 = VECTOR ( 'NONE', #61172, 1000.000000000000114 ) ;
#64874 = LINE ( 'NONE', #12151, #65752 ) ;
#64875 = AXIS2_PLACEMENT_3D ( 'NONE', #46807, #51778, #56722 ) ;
#64876 = ORIENTED_EDGE ( 'NONE', *, *, #19970, .F. ) ;
#64877 = ORIENTED_EDGE ( 'NONE', *, *, #29222, .T. ) ;
#64879 = VERTEX_POINT ( 'NONE', #66303 ) ;
#64878 = CIRCLE ( 'NONE', #47906, 2.458500000000000796 ) ;
#64880 = EDGE_CURVE ( 'NONE', #3823, #56702, #1586, .T. ) ;
#64881 = DIRECTION ( 'NONE',  ( 0.000000000000000000, -1.000000000000000000, -0.000000000000000000 ) ) ;
#64882 = DIRECTION ( 'NONE',  ( 1.000000000000000000, -0.000000000000000000, -0.000000000000000000 ) ) ;
#64884 = EDGE_CURVE ( 'NONE', #18304, #3392, #12541, .T. ) ;
#64883 =( NAMED_UNIT ( * ) PLANE_ANGLE_UNIT ( ) SI_UNIT ( $, .RADIAN. ) );
#64885 = VECTOR ( 'NONE', #60191, 1000.000000000000000 ) ;
#64886 = EDGE_LOOP ( 'NONE', ( #4808, #29740, #65902, #36816 ) ) ;
#64887 = ORIENTED_EDGE ( 'NONE', *, *, #34216, .T. ) ;
#64888 = ORIENTED_EDGE ( 'NONE', *, *, #45637, .T. ) ;
#64889 = VECTOR ( 'NONE', #16255, 1000.000000000000000 ) ;
#64890 = CARTESIAN_POINT ( 'NONE',  ( 11.00000000000000000, -11.50000000000100009, 15.00000000000084910 ) ) ;
#64891 = VERTEX_POINT ( 'NONE', #61323 ) ;
#64892 = VERTEX_POINT ( 'NONE', #34105 ) ;
#64893 = ORIENTED_EDGE ( 'NONE', *, *, #67296, .F. ) ;
#64894 = ORIENTED_EDGE ( 'NONE', *, *, #59243, .T. ) ;
#64895 = DIRECTION ( 'NONE',  ( 0.000000000000000000, 0.000000000000000000, 1.000000000000000000 ) ) ;
#64896 = UNCERTAINTY_MEASURE_WITH_UNIT (LENGTH_MEASURE( 1.000000000000000082E-05 ), #18157, 'distance_accuracy_value', 'NONE');
#64898 = ORIENTED_EDGE ( 'NONE', *, *, #45372, .F. ) ;
#64897 = DIRECTION ( 'NONE',  ( 0.000000000000000000, -1.000000000000000000, 0.000000000000000000 ) ) ;
#64899 = DIRECTION ( 'NONE',  ( -1.000000000000000000, 0.000000000000000000, 0.000000000000000000 ) ) ;
#64900 = DIRECTION ( 'NONE',  ( -1.000000000000000000, -1.570596175624152290E-15, 0.000000000000000000 ) ) ;
#64901 = CARTESIAN_POINT ( 'NONE',  ( 6.619341603356875936, 7.252248008019321901, 455.0000000000000568 ) ) ;
#64902 = EDGE_LOOP ( 'NONE', ( #27447, #1999, #6247, #30373 ) ) ;
#64903 = CIRCLE ( 'NONE', #52488, 0.5000000000079362072 ) ;
#64904 = CARTESIAN_POINT ( 'NONE',  ( 22.90000000000000213, -21.00000000000000000, 13.86939075806900057 ) ) ;
#64905 = LINE ( 'NONE', #38979, #66514 ) ;
#64906 = EDGE_LOOP ( 'NONE', ( #9303, #17365, #64053, #49977 ) ) ;
#64907 = CARTESIAN_POINT ( 'NONE',  ( 15.50000000000000000, -0.2038245569916610489, 21.05662432702600029 ) ) ;
#64908 = ADVANCED_FACE ( 'NONE', ( #60648 ), #17162, .T. ) ;
#64909 = AXIS2_PLACEMENT_3D ( 'NONE', #3921, #3219, #2855 ) ;
#64910 = DIRECTION ( 'NONE',  ( -1.000000000000000000, 0.000000000000000000, 0.000000000000000000 ) ) ;
#64911 = FACE_OUTER_BOUND ( 'NONE', #64130, .T. ) ;
#64912 = ORIENTED_EDGE ( 'NONE', *, *, #36058, .T. ) ;
#64914 = ADVANCED_FACE ( 'NONE', ( #39416 ), #45416, .T. ) ;
#64913 = DIRECTION ( 'NONE',  ( -1.000000000000000000, 0.000000000000000000, 0.000000000000000000 ) ) ;
#64915 = STYLED_ITEM ( 'NONE', ( #66412 ), #67216 ) ;
#64916 = DIRECTION ( 'NONE',  ( 0.5773502691896257311, -0.5773502691896298389, -0.5773502691896216232 ) ) ;
#64917 = FACE_OUTER_BOUND ( 'NONE', #35284, .T. ) ;
#64918 = EDGE_CURVE ( 'NONE', #20883, #60595, #33161, .T. ) ;
#64919 = EDGE_CURVE ( 'NONE', #20150, #22770, #10612, .T. ) ;
#64920 = CIRCLE ( 'NONE', #62631, 0.2000000000000005107 ) ;
#64921 = DIRECTION ( 'NONE',  ( -1.214636490590110272E-14, -1.000000000000000000, 0.000000000000000000 ) ) ;
#64922 = EDGE_CURVE ( 'NONE', #57392, #41573, #12195, .T. ) ;
#64923 = CARTESIAN_POINT ( 'NONE',  ( 4.396432944014527777, -8.406483450353382736, 195.0000000000000284 ) ) ;
#64924 = ADVANCED_FACE ( 'NONE', ( #1947 ), #38726, .F. ) ;
#64925 = FACE_OUTER_BOUND ( 'NONE', #64445, .T. ) ;
#64926 = CARTESIAN_POINT ( 'NONE',  ( 30.00000000000000000, -13.79999999999979998, 17.64999999999988844 ) ) ;
#64927 = CARTESIAN_POINT ( 'NONE',  ( -11.18071654964682615, -12.00648345035337350, 455.0000000000000568 ) ) ;
#64928 = EDGE_CURVE ( 'NONE', #36809, #3920, #33768, .T. ) ;
#64929 = ORIENTED_EDGE ( 'NONE', *, *, #1835, .T. ) ;
#64930 = CARTESIAN_POINT ( 'NONE',  ( 169.1780563256071446, -33.83962462487175316, 5.000000000000000000 ) ) ;
#64931 = CARTESIAN_POINT ( 'NONE',  ( 7.250000000000005329, 8.250000000000001776, -20.00000000000000000 ) ) ;
#64932 = CIRCLE ( 'NONE', #63827, 1.929199999999998916 ) ;
#64933 = DIRECTION ( 'NONE',  ( 0.000000000000000000, 3.673940397442059868E-16, -1.000000000000000000 ) ) ;
#64934 = PLANE ( 'NONE',  #40944 ) ;
#64935 = EDGE_LOOP ( 'NONE', ( #39637, #4267, #5659, #38096 ) ) ;
#64936 = CARTESIAN_POINT ( 'NONE',  ( 7.811466277050736373, -4.740315990920255906, 455.0000000000000568 ) ) ;
#64937 = CARTESIAN_POINT ( 'NONE',  ( 176.4833316329832940, 0.000000000000000000, 326.8892501111512843 ) ) ;
#64938 = CARTESIAN_POINT ( 'NONE',  ( -6.651770455163739548, 7.517976262117183062, 54.00000000000000711 ) ) ;
#64939 = CARTESIAN_POINT ( 'NONE',  ( 30.00000000000000000, -9.200000000000120082, 17.30000000000000071 ) ) ;
#64940 = CARTESIAN_POINT ( 'NONE',  ( -8.250000000000001776, 7.250000000000000888, -26.00000000000001066 ) ) ;
#64941 = CARTESIAN_POINT ( 'NONE',  ( -5.242976262117259978, 5.242976262117182706, 54.00000000000000711 ) ) ;
#64942 = VERTEX_POINT ( 'NONE', #55351 ) ;
#64943 = AXIS2_PLACEMENT_3D ( 'NONE', #63162, #15432, #64227 ) ;
#64944 = ORIENTED_EDGE ( 'NONE', *, *, #28916, .F. ) ;
#64945 = CARTESIAN_POINT ( 'NONE',  ( -29.50000000000000355, -11.50000000000100009, 19.50000000000103739 ) ) ;
#64946 = DIRECTION ( 'NONE',  ( -1.000000000000000000, 0.000000000000000000, 0.000000000000000000 ) ) ;
#64947 = ORIENTED_EDGE ( 'NONE', *, *, #47422, .T. ) ;
#64948 = DIRECTION ( 'NONE',  ( 0.000000000000000000, 0.000000000000000000, 1.000000000000000000 ) ) ;
#64949 = DIRECTION ( 'NONE',  ( 0.000000000000000000, 0.000000000000000000, 1.000000000000000000 ) ) ;
#64950 = AXIS2_PLACEMENT_3D ( 'NONE', #29786, #62309, #18834 ) ;
#64951 = ORIENTED_EDGE ( 'NONE', *, *, #23564, .T. ) ;
#64952 = CARTESIAN_POINT ( 'NONE',  ( 9.306483450353379538, -10.92648345035348534, 455.0000000000000568 ) ) ;
#64953 = VERTEX_POINT ( 'NONE', #33434 ) ;
#64954 = VERTEX_POINT ( 'NONE', #6894 ) ;
#64955 = DIRECTION ( 'NONE',  ( 0.7071067811865446862, -0.7071067811865503483, 0.000000000000000000 ) ) ;
#64956 = EDGE_LOOP ( 'NONE', ( #11156, #33385, #56912, #6237 ) ) ;
#64957 = LINE ( 'NONE', #5563, #59105 ) ;
#64958 = FACE_BOUND ( 'NONE', #60166, .T. ) ;
#64960 = EDGE_CURVE ( 'NONE', #34559, #67161, #44714, .T. ) ;
#64959 = DIRECTION ( 'NONE',  ( -1.000000000000000000, 0.000000000000000000, 0.000000000000000000 ) ) ;
#64961 = AXIS2_PLACEMENT_3D ( 'NONE', #40518, #13646, #63141 ) ;
#64962 = CIRCLE ( 'NONE', #34433, 0.1999999999999992339 ) ;
#64963 = VECTOR ( 'NONE', #53677, 1000.000000000000000 ) ;
#64964 = ORIENTED_EDGE ( 'NONE', *, *, #31245, .T. ) ;
#64966 = EDGE_CURVE ( 'NONE', #50438, #29049, #34448, .T. ) ;
#64965 = ORIENTED_EDGE ( 'NONE', *, *, #63069, .T. ) ;
#64967 = LINE ( 'NONE', #48700, #58369 ) ;
#64969 = CARTESIAN_POINT ( 'NONE',  ( 38.90000000000000568, 13.66939075806899950, 20.80000000000000426 ) ) ;
#64968 = CARTESIAN_POINT ( 'NONE',  ( -7.250000000000000888, -8.249999999999998224, -26.00000000000001066 ) ) ;
#64970 = CIRCLE ( 'NONE', #55380, 0.8128000000000145109 ) ;
#64971 = CIRCLE ( 'NONE', #18654, 4.500000000000191847 ) ;
#64972 = ORIENTED_EDGE ( 'NONE', *, *, #37162, .T. ) ;
#64973 = ORIENTED_EDGE ( 'NONE', *, *, #12046, .T. ) ;
#64974 = ADVANCED_FACE ( 'NONE', ( #50724 ), #2295, .F. ) ;
#64975 = ORIENTED_EDGE ( 'NONE', *, *, #31250, .F. ) ;
#64976 = AXIS2_PLACEMENT_3D ( 'NONE', #69274, #20481, #20827 ) ;
#64977 = CARTESIAN_POINT ( 'NONE',  ( -8.593516549646793123, -7.616533956692233431, 455.0000000000000568 ) ) ;
#64979 = ORIENTED_EDGE ( 'NONE', *, *, #43320, .F. ) ;
#64978 = CARTESIAN_POINT ( 'NONE',  ( 50.00000000000000711, 0.7500000000000000000, 4.943429983321300902 ) ) ;
#64980 = CARTESIAN_POINT ( 'NONE',  ( -11.00000000000000000, -5.599999999999999645, -9.400000000000000355 ) ) ;
#64981 = MECHANICAL_DESIGN_GEOMETRIC_PRESENTATION_REPRESENTATION (  '', ( #67230 ), #18667 ) ;
#64982 = DIRECTION ( 'NONE',  ( -0.000000000000000000, 1.000000000000000000, -0.000000000000000000 ) ) ;
#64983 = ORIENTED_EDGE ( 'NONE', *, *, #18356, .F. ) ;
#64984 = ORIENTED_EDGE ( 'NONE', *, *, #19261, .T. ) ;
#64985 = MECHANICAL_DESIGN_GEOMETRIC_PRESENTATION_REPRESENTATION (  '', ( #46891 ), #6326 ) ;
#64986 = DIRECTION ( 'NONE',  ( 0.000000000000000000, 0.000000000000000000, 1.000000000000000000 ) ) ;
#64987 = ORIENTED_EDGE ( 'NONE', *, *, #3301, .T. ) ;
#64988 = DIRECTION ( 'NONE',  ( -1.836970198721029934E-16, -1.836970198721010706E-16, 1.000000000000000000 ) ) ;
#64989 = DIRECTION ( 'NONE',  ( 0.000000000000000000, 0.000000000000000000, -1.000000000000000000 ) ) ;
#64990 = ORIENTED_EDGE ( 'NONE', *, *, #65783, .T. ) ;
#64991 = EDGE_CURVE ( 'NONE', #60595, #38472, #49687, .T. ) ;
#64992 =( LENGTH_UNIT ( ) NAMED_UNIT ( * ) SI_UNIT ( .MILLI., .METRE. ) );
#64993 = DIRECTION ( 'NONE',  ( -1.000000000000000000, 2.309061475090597584E-14, 0.000000000000000000 ) ) ;
#64994 = AXIS2_PLACEMENT_3D ( 'NONE', #48031, #69940, #15165 ) ;
#64996 = ORIENTED_EDGE ( 'NONE', *, *, #28035, .T. ) ;
#64995 = CARTESIAN_POINT ( 'NONE',  ( -2.530476262117318242, -8.835729544836354421, 54.00000000000000711 ) ) ;
#64997 = VERTEX_POINT ( 'NONE', #37940 ) ;
#64998 = CARTESIAN_POINT ( 'NONE',  ( 49.00000000000000000, -0.7500000000000000000, -3.929058411375430104 ) ) ;
#64999 = DIRECTION ( 'NONE',  ( 0.000000000000000000, 0.000000000000000000, 1.000000000000000000 ) ) ;
#65000 = VECTOR ( 'NONE', #12988, 1000.000000000000000 ) ;
#65001 = DIRECTION ( 'NONE',  ( -1.000000000000000000, 0.000000000000000000, 0.000000000000000000 ) ) ;
#65002 = CARTESIAN_POINT ( 'NONE',  ( -15.50000000000000000, -0.2038245569916614930, 21.05662432702600029 ) ) ;
#65003 = AXIS2_PLACEMENT_3D ( 'NONE', #26410, #69192, #20747 ) ;
#65004 = DIRECTION ( 'NONE',  ( 7.665540703601096574E-15, 1.000000000000000000, -0.000000000000000000 ) ) ;
#65006 = EDGE_LOOP ( 'NONE', ( #64290, #49541, #48610, #50266 ) ) ;
#65005 = EDGE_CURVE ( 'NONE', #64098, #27857, #43316, .T. ) ;
#65007 = CARTESIAN_POINT ( 'NONE',  ( 41.09999999999999432, -21.00000000000000000, 14.57806571531351914 ) ) ;
#65008 = EDGE_CURVE ( 'NONE', #10322, #9609, #38288, .T. ) ;
#65009 = FACE_OUTER_BOUND ( 'NONE', #18353, .T. ) ;
#65011 = VERTEX_POINT ( 'NONE', #59498 ) ;
#65010 = LINE ( 'NONE', #36387, #35605 ) ;
#65012 = VECTOR ( 'NONE', #30188, 1000.000000000000000 ) ;
#65013 = AXIS2_PLACEMENT_3D ( 'NONE', #58812, #10369, #53509 ) ;
#65014 = DIRECTION ( 'NONE',  ( 0.000000000000000000, 1.000000000000000000, 0.000000000000000000 ) ) ;
#65015 = ADVANCED_FACE ( 'NONE', ( #43231 ), #27328, .F. ) ;
#65016 = CARTESIAN_POINT ( 'NONE',  ( -7.250000000000000888, -8.249999999999998224, -17.50000000000000000 ) ) ;
#65017 = FACE_OUTER_BOUND ( 'NONE', #3005, .T. ) ;
#65018 = TOROIDAL_SURFACE ( 'NONE', #61768, 0.06000000000000080963, 0.7500000000000000000 ) ;
#65019 = CIRCLE ( 'NONE', #34500, 0.1999999999999987899 ) ;
#65020 = AXIS2_PLACEMENT_3D ( 'NONE', #54875, #55213, #436 ) ;
#65021 = CARTESIAN_POINT ( 'NONE',  ( 11.48848345035334617, -10.20488345035352928, 455.0000000000000568 ) ) ;
#65022 = ORIENTED_EDGE ( 'NONE', *, *, #48558, .F. ) ;
#65023 = DIRECTION ( 'NONE',  ( -1.000000000000000000, 0.000000000000000000, -0.000000000000000000 ) ) ;
#65024 = CARTESIAN_POINT ( 'NONE',  ( 275.0000000000000000, -32.94999999999885176, -8.199999999997979572 ) ) ;
#65025 = ORIENTED_EDGE ( 'NONE', *, *, #17412, .T. ) ;
#65026 = DIRECTION ( 'NONE',  ( 1.836970198721029934E-16, 1.836970198721010706E-16, -1.000000000000000000 ) ) ;
#65027 = DIRECTION ( 'NONE',  ( 1.836970198721029934E-16, 1.836970198721010706E-16, -1.000000000000000000 ) ) ;
#65028 = DIRECTION ( 'NONE',  ( 1.000000000000000000, -1.610765207321970913E-14, 0.000000000000000000 ) ) ;
#65029 = DIRECTION ( 'NONE',  ( -1.836970198721029934E-16, 1.836970198721036344E-16, -1.000000000000000000 ) ) ;
#65030 = DIRECTION ( 'NONE',  ( 0.000000000000000000, 0.000000000000000000, 1.000000000000000000 ) ) ;
#65031 = VECTOR ( 'NONE', #27881, 1000.000000000000114 ) ;
#65032 = VERTEX_POINT ( 'NONE', #1143 ) ;
#65033 = EDGE_LOOP ( 'NONE', ( #68537, #40066, #41003, #394, #20466, #39636, #56311, #68483, #534, #53864, #24956, #27816, #52694, #19978, #31709 ) ) ;
#65034 = LINE ( 'NONE', #42763, #40863 ) ;
#65035 = VERTEX_POINT ( 'NONE', #11397 ) ;
#65036 = FACE_OUTER_BOUND ( 'NONE', #41766, .T. ) ;
#65037 = ORIENTED_EDGE ( 'NONE', *, *, #66103, .F. ) ;
#65038 = COLOUR_RGB ( '', 0.72549020, 0.75294118, 0.79215686) ;
#65039 = CARTESIAN_POINT ( 'NONE',  ( -8.250000000000001776, -7.249999999999998224, -26.00000000000001066 ) ) ;
#65040 = DIRECTION ( 'NONE',  ( 0.000000000000000000, 0.000000000000000000, -1.000000000000000000 ) ) ;
#65041 = DIRECTION ( 'NONE',  ( 0.000000000000000000, 0.7071067811865474617, -0.7071067811865474617 ) ) ;
#65042 = VERTEX_POINT ( 'NONE', #26629 ) ;
#65043 = VERTEX_POINT ( 'NONE', #53508 ) ;
#65044 = DIRECTION ( 'NONE',  ( -0.000000000000000000, 1.000000000000000000, -0.000000000000000000 ) ) ;
#65045 = ORIENTED_EDGE ( 'NONE', *, *, #47924, .F. ) ;
#65046 = VERTEX_POINT ( 'NONE', #49244 ) ;
#65047 = FACE_OUTER_BOUND ( 'NONE', #25841, .T. ) ;
#65048 = FACE_OUTER_BOUND ( 'NONE', #30071, .T. ) ;
#65049 = LINE ( 'NONE', #58703, #51275 ) ;
#65050 = VECTOR ( 'NONE', #67685, 1000.000000000000000 ) ;
#65051 = EDGE_LOOP ( 'NONE', ( #28924, #19893, #9821, #45895 ) ) ;
#65052 = ADVANCED_FACE ( 'NONE', ( #5059 ), #21324, .F. ) ;
#65053 = EDGE_CURVE ( 'NONE', #1557, #50270, #61356, .T. ) ;
#65054 = CARTESIAN_POINT ( 'NONE',  ( 10.20488345035345290, 9.791916549646566992, 455.0000000000000568 ) ) ;
#65055 = EDGE_CURVE ( 'NONE', #54865, #33821, #64808, .T. ) ;
#65057 = LINE ( 'NONE', #65737, #27663 ) ;
#65056 = DIRECTION ( 'NONE',  ( -1.836970198721029934E-16, 1.836970198721036590E-16, -1.000000000000000000 ) ) ;
#65058 = ORIENTED_EDGE ( 'NONE', *, *, #44602, .T. ) ;
#65059 = ORIENTED_EDGE ( 'NONE', *, *, #16558, .T. ) ;
#65061 = EDGE_LOOP ( 'NONE', ( #62960, #50843, #48648, #41891 ) ) ;
#65060 = DIRECTION ( 'NONE',  ( 0.000000000000000000, 0.000000000000000000, 1.000000000000000000 ) ) ;
#65062 = AXIS2_PLACEMENT_3D ( 'NONE', #27115, #54341, #27459 ) ;
#65063 = VERTEX_POINT ( 'NONE', #110 ) ;
#65064 = EDGE_CURVE ( 'NONE', #7367, #51302, #27665, .T. ) ;
#65065 = AXIS2_PLACEMENT_3D ( 'NONE', #7949, #19269, #45431 ) ;
#65066 = CARTESIAN_POINT ( 'NONE',  ( 1.480523737882813773, 8.598420958951637161, 54.00000000000000711 ) ) ;
#65067 = VECTOR ( 'NONE', #27783, 1000.000000000000000 ) ;
#65068 = AXIS2_PLACEMENT_3D ( 'NONE', #1063, #1394, #67135 ) ;
#65069 = PLANE ( 'NONE',  #57378 ) ;
#65070 = ORIENTED_EDGE ( 'NONE', *, *, #58776, .T. ) ;
#65071 = ORIENTED_EDGE ( 'NONE', *, *, #51678, .F. ) ;
#65072 = AXIS2_PLACEMENT_3D ( 'NONE', #31692, #47252, #20022 ) ;
#65073 = AXIS2_PLACEMENT_3D ( 'NONE', #55721, #45802, #7624 ) ;
#65074 = VECTOR ( 'NONE', #25387, 1000.000000000000000 ) ;
#65075 = DIRECTION ( 'NONE',  ( -1.000000000000000000, 0.000000000000000000, 0.000000000000000000 ) ) ;
#65076 = CARTESIAN_POINT ( 'NONE',  ( -8.249999999999996447, 8.250000000000001776, 0.000000000000000000 ) ) ;
#65077 = ORIENTED_EDGE ( 'NONE', *, *, #67633, .T. ) ;
#65078 = CARTESIAN_POINT ( 'NONE',  ( 11.78648345035340839, 7.813516549646560172, 455.0000000000000568 ) ) ;
#65079 = LINE ( 'NONE', #48116, #18822 ) ;
#65080 = CARTESIAN_POINT ( 'NONE',  ( 17.89999999999999858, -0.000000000000000000, -20.80000000000000426 ) ) ;
#65081 = VERTEX_POINT ( 'NONE', #44257 ) ;
#65082 = AXIS2_PLACEMENT_3D ( 'NONE', #29139, #24547, #40079 ) ;
#65083 = CARTESIAN_POINT ( 'NONE',  ( 30.00000000000000000, -5.200000000000001066, -26.59999999999999787 ) ) ;
#65084 = CARTESIAN_POINT ( 'NONE',  ( -13.00000000000000178, -17.00000000000000000, 15.70499999999969809 ) ) ;
#65086 = ORIENTED_EDGE ( 'NONE', *, *, #45587, .F. ) ;
#65085 = CYLINDRICAL_SURFACE ( 'NONE', #4741, 0.2000000000000005107 ) ;
#65088 = ORIENTED_EDGE ( 'NONE', *, *, #53036, .T. ) ;
#65087 = CARTESIAN_POINT ( 'NONE',  ( -11.77351654964674132, -4.186483450353323477, 455.0000000000000568 ) ) ;
#65089 = CARTESIAN_POINT ( 'NONE',  ( 7.250000000000004441, 7.450000000000001954, -7.500000000000000000 ) ) ;
#65090 = CARTESIAN_POINT ( 'NONE',  ( 290.0000000000000000, -42.00000000000000000, -27.00000000000000000 ) ) ;
#65091 = CARTESIAN_POINT ( 'NONE',  ( -30.00000000000000000, -11.70000000000000284, -12.50000000000000000 ) ) ;
#65092 = CARTESIAN_POINT ( 'NONE',  ( -25.50000000000000355, 0.000000000000000000, -24.75000000000000000 ) ) ;
#65093 = DIRECTION ( 'NONE',  ( 0.000000000000000000, 0.000000000000000000, 1.000000000000000000 ) ) ;
#65094 = CARTESIAN_POINT ( 'NONE',  ( 7.272650909786554152, 4.188533722949247640, 195.0000000000000284 ) ) ;
#65095 = ORIENTED_EDGE ( 'NONE', *, *, #19087, .T. ) ;
#65096 = LINE ( 'NONE', #11331, #20283 ) ;
#65097 = EDGE_CURVE ( 'NONE', #12559, #40641, #69315, .T. ) ;
#65098 = ORIENTED_EDGE ( 'NONE', *, *, #27409, .F. ) ;
#65100 = ORIENTED_EDGE ( 'NONE', *, *, #61834, .T. ) ;
#65099 = DIRECTION ( 'NONE',  ( 0.000000000000000000, 1.000000000000000000, 0.000000000000000000 ) ) ;
#65101 = DIRECTION ( 'NONE',  ( -0.000000000000000000, 0.000000000000000000, 1.000000000000000000 ) ) ;
#65102 = EDGE_CURVE ( 'NONE', #58960, #57228, #16210, .T. ) ;
#65103 = EDGE_CURVE ( 'NONE', #3828, #20214, #54205, .T. ) ;
#65104 = CIRCLE ( 'NONE', #53801, 0.4999999999991867061 ) ;
#65105 = CARTESIAN_POINT ( 'NONE',  ( 14.25000000000000000, -0.3156864504677152627, -22.74361999681790536 ) ) ;
#65106 = EDGE_CURVE ( 'NONE', #4795, #49394, #22017, .T. ) ;
#65107 = VECTOR ( 'NONE', #31656, 1000.000000000000000 ) ;
#65108 = ORIENTED_EDGE ( 'NONE', *, *, #60856, .F. ) ;
#65109 = CARTESIAN_POINT ( 'NONE',  ( -2.406732575409671337, -8.711985858128709737, 54.00000000000000711 ) ) ;
#65110 = CARTESIAN_POINT ( 'NONE',  ( 28.90000000000000213, -14.06939075806900163, -20.80000000000000426 ) ) ;
#65111 = ORIENTED_EDGE ( 'NONE', *, *, #15636, .F. ) ;
#65112 = DIRECTION ( 'NONE',  ( 1.000000000000000000, -0.000000000000000000, 0.000000000000000000 ) ) ;
#65113 = DIRECTION ( 'NONE',  ( 1.000000000000000000, 0.000000000000000000, 0.000000000000000000 ) ) ;
#65114 = CIRCLE ( 'NONE', #62874, 4.000000000000001776 ) ;
#65116 = EDGE_CURVE ( 'NONE', #54496, #54832, #16721, .T. ) ;
#65115 = VECTOR ( 'NONE', #11653, 1000.000000000000000 ) ;
#65117 = FACE_OUTER_BOUND ( 'NONE', #69793, .T. ) ;
#65118 = EDGE_CURVE ( 'NONE', #7495, #42297, #22372, .T. ) ;
#65119 = DIRECTION ( 'NONE',  ( 0.000000000000000000, 0.000000000000000000, -1.000000000000000000 ) ) ;
#65120 = EDGE_CURVE ( 'NONE', #58826, #29208, #42879, .T. ) ;
#65121 = VECTOR ( 'NONE', #49928, 1000.000000000000000 ) ;
#65122 = CIRCLE ( 'NONE', #59510, 0.5249999999999994671 ) ;
#65123 = ORIENTED_EDGE ( 'NONE', *, *, #15233, .T. ) ;
#65124 = DIRECTION ( 'NONE',  ( -0.4999999999989371835, 0.000000000000000000, 0.8660254037850523279 ) ) ;
#65125 = ORIENTED_EDGE ( 'NONE', *, *, #16892, .T. ) ;
#65126 = VERTEX_POINT ( 'NONE', #38627 ) ;
#65127 = DIRECTION ( 'NONE',  ( -0.000000000000000000, -0.000000000000000000, -1.000000000000000000 ) ) ;
#65129 = CYLINDRICAL_SURFACE ( 'NONE', #64734, 0.1999999999999996503 ) ;
#65128 = AXIS2_PLACEMENT_3D ( 'NONE', #59860, #33673, #17765 ) ;
#65130 = VECTOR ( 'NONE', #52622, 1000.000000000000000 ) ;
#65131 = VECTOR ( 'NONE', #2966, 1000.000000000000000 ) ;
#65132 = DIRECTION ( 'NONE',  ( 0.000000000000000000, 0.000000000000000000, 1.000000000000000000 ) ) ;
#65133 = CARTESIAN_POINT ( 'NONE',  ( 4.201500623656003519, -7.272650909786698037, 455.0000000000000568 ) ) ;
#65134 = ORIENTED_EDGE ( 'NONE', *, *, #847, .F. ) ;
#65135 = ORIENTED_EDGE ( 'NONE', *, *, #413, .F. ) ;
#65137 = ORIENTED_EDGE ( 'NONE', *, *, #42767, .F. ) ;
#65136 = DIRECTION ( 'NONE',  ( -1.000000000000000000, 0.000000000000000000, 0.000000000000000000 ) ) ;
#65138 = VERTEX_POINT ( 'NONE', #60176 ) ;
#65139 = PRODUCT_DEFINITION_SHAPE ( 'NONE', 'NONE',  #69996 ) ;
#65140 = VECTOR ( 'NONE', #23758, 1000.000000000000000 ) ;
#65141 = CARTESIAN_POINT ( 'NONE',  ( -8.593516549646711411, 7.603567055985436696, 195.0000000000000284 ) ) ;
#65142 = CARTESIAN_POINT ( 'NONE',  ( 290.0000000000000000, 0.000000000000000000, 0.000000000000000000 ) ) ;
#65143 = DIRECTION ( 'NONE',  ( 0.000000000000000000, 0.000000000000000000, 1.000000000000000000 ) ) ;
#65144 = DIRECTION ( 'NONE',  ( 0.7071067811865527908, 0.7071067811865422437, 2.597868168706460875E-16 ) ) ;
#65146 = CARTESIAN_POINT ( 'NONE',  ( 30.00000000000000000, -17.50000000000000000, 26.64999999999999858 ) ) ;
#65145 = CARTESIAN_POINT ( 'NONE',  ( 30.00000000000000000, -17.50000000000000000, -26.64999999999999858 ) ) ;
#65147 = ORIENTED_EDGE ( 'NONE', *, *, #15835, .F. ) ;
#65149 = ORIENTED_EDGE ( 'NONE', *, *, #39131, .F. ) ;
#65148 = DIRECTION ( 'NONE',  ( -1.000000000000000000, 0.000000000000000000, -0.000000000000000000 ) ) ;
#65150 = EDGE_LOOP ( 'NONE', ( #1303, #57471, #40512, #59110 ) ) ;
#65151 = ORIENTED_EDGE ( 'NONE', *, *, #10968, .T. ) ;
#65152 = DIRECTION ( 'NONE',  ( -1.000000000000000000, 0.000000000000000000, 0.000000000000000000 ) ) ;
#65153 = CARTESIAN_POINT ( 'NONE',  ( 41.09999999999999432, -14.06939075806901940, -20.80000000000000426 ) ) ;
#65154 = LINE ( 'NONE', #54542, #419 ) ;
#65155 = ORIENTED_EDGE ( 'NONE', *, *, #13835, .F. ) ;
#65156 = ORIENTED_EDGE ( 'NONE', *, *, #38066, .T. ) ;
#65157 = VECTOR ( 'NONE', #67531, 1000.000000000000000 ) ;
#65158 = ORIENTED_EDGE ( 'NONE', *, *, #30924, .T. ) ;
#65159 = CARTESIAN_POINT ( 'NONE',  ( -8.249999999999996447, -7.848062532927998269, 0.000000000000000000 ) ) ;
#65160 = ADVANCED_FACE ( 'NONE', ( #54898 ), #11729, .F. ) ;
#65161 = DIRECTION ( 'NONE',  ( 0.000000000000000000, 0.000000000000000000, 1.000000000000000000 ) ) ;
#65162 =( GEOMETRIC_REPRESENTATION_CONTEXT ( 3 ) GLOBAL_UNCERTAINTY_ASSIGNED_CONTEXT ( ( #19644 ) ) GLOBAL_UNIT_ASSIGNED_CONTEXT ( ( #53350, #69248, #63605 ) ) REPRESENTATION_CONTEXT ( 'NONE', 'WORKASPACE' ) );
#65163 = DIRECTION ( 'NONE',  ( -1.836970198721029934E-16, -1.836970198721010706E-16, 1.000000000000000000 ) ) ;
#65164 = ORIENTED_EDGE ( 'NONE', *, *, #23480, .F. ) ;
#65165 = EDGE_LOOP ( 'NONE', ( #4976, #7473, #59052, #52175 ) ) ;
#65166 = AXIS2_PLACEMENT_3D ( 'NONE', #38812, #64315, #60368 ) ;
#65168 = CARTESIAN_POINT ( 'NONE',  ( 8.612468434717241550, -1.480523737882825985, 54.00000000000000711 ) ) ;
#65167 = AXIS2_PLACEMENT_3D ( 'NONE', #60446, #60792, #13039 ) ;
#65169 = ADVANCED_FACE ( 'NONE', ( #49576, #55573 ), #23039, .F. ) ;
#65170 = PLANE ( 'NONE',  #5203 ) ;
#65171 = ORIENTED_EDGE ( 'NONE', *, *, #47464, .F. ) ;
#65172 = AXIS2_PLACEMENT_3D ( 'NONE', #27096, #37711, #31719 ) ;
#65173 = CIRCLE ( 'NONE', #34650, 1.000000000000003553 ) ;
#65174 =( GEOMETRIC_REPRESENTATION_CONTEXT ( 3 ) GLOBAL_UNCERTAINTY_ASSIGNED_CONTEXT ( ( #59927 ) ) GLOBAL_UNIT_ASSIGNED_CONTEXT ( ( #45026, #46081, #66600 ) ) REPRESENTATION_CONTEXT ( 'NONE', 'WORKASPACE' ) );
#65175 = CARTESIAN_POINT ( 'NONE',  ( 7.450000000000006395, 7.250000000000000888, -25.50000000000000355 ) ) ;
#65176 = ADVANCED_FACE ( 'NONE', ( #66180 ), #35032, .F. ) ;
#65178 = ORIENTED_EDGE ( 'NONE', *, *, #61800, .T. ) ;
#65177 = LINE ( 'NONE', #5073, #20478 ) ;
#65179 = ORIENTED_EDGE ( 'NONE', *, *, #36331, .F. ) ;
#65180 = CARTESIAN_POINT ( 'NONE',  ( -9.897976262117257562, 6.817976262117182884, 54.00000000000000711 ) ) ;
#65181 = AXIS2_PLACEMENT_3D ( 'NONE', #20552, #30462, #9252 ) ;
#65182 = CARTESIAN_POINT ( 'NONE',  ( 1.866219381641426533, -9.417013320880776917, 195.0000000000000284 ) ) ;
#65183 = VECTOR ( 'NONE', #69300, 1000.000000000000000 ) ;
#65184 = CARTESIAN_POINT ( 'NONE',  ( 7.811466277050736373, -7.272650909786632312, 195.0000000000000284 ) ) ;
#65185 = EDGE_CURVE ( 'NONE', #58876, #17214, #55231, .T. ) ;
#65186 = DIRECTION ( 'NONE',  ( -1.000000000000000000, -2.135044278125301343E-15, -7.844025423732065664E-31 ) ) ;
#65187 = CARTESIAN_POINT ( 'NONE',  ( -7.450000000000001954, 0.000000000000000000, -25.50000000000000355 ) ) ;
#65188 = AXIS2_PLACEMENT_3D ( 'NONE', #35210, #18255, #61749 ) ;
#65189 = ORIENTED_EDGE ( 'NONE', *, *, #56762, .F. ) ;
#65190 = CARTESIAN_POINT ( 'NONE',  ( 7.250000000000004441, 7.450000000000001954, -17.00000000000000000 ) ) ;
#65191 = ORIENTED_EDGE ( 'NONE', *, *, #64372, .F. ) ;
#65192 = AXIS2_PLACEMENT_3D ( 'NONE', #40633, #61134, #50885 ) ;
#65193 = CARTESIAN_POINT ( 'NONE',  ( 0.000000000000000000, -8.249999999999998224, -7.500000000000000000 ) ) ;
#65194 = DIRECTION ( 'NONE',  ( -0.000000000000000000, 3.673940397442059868E-16, -1.000000000000000000 ) ) ;
#65195 = EDGE_CURVE ( 'NONE', #1574, #38911, #24128, .T. ) ;
#65196 = LINE ( 'NONE', #43948, #22370 ) ;
#65197 = CYLINDRICAL_SURFACE ( 'NONE', #37421, 0.4999999999945534124 ) ;
#65198 = CARTESIAN_POINT ( 'NONE',  ( -7.250000000000000888, -8.249999999999998224, -8.000000000000000000 ) ) ;
#65199 = ORIENTED_EDGE ( 'NONE', *, *, #60908, .T. ) ;
#65200 = DIRECTION ( 'NONE',  ( -1.000000000000000000, 0.000000000000000000, 0.000000000000000000 ) ) ;
#65201 = EDGE_CURVE ( 'NONE', #53008, #5450, #29732, .T. ) ;
#65202 = ADVANCED_FACE ( 'NONE', ( #12081 ), #2865, .T. ) ;
#65203 = ORIENTED_EDGE ( 'NONE', *, *, #46229, .T. ) ;
#65204 = CARTESIAN_POINT ( 'NONE',  ( -5.993516549646728642, -6.006483450353378828, 195.0000000000000284 ) ) ;
#65205 = DIRECTION ( 'NONE',  ( -0.000000000000000000, -0.000000000000000000, 1.000000000000000000 ) ) ;
#65206 = CIRCLE ( 'NONE', #26793, 0.4000000000000600298 ) ;
#65207 = EDGE_LOOP ( 'NONE', ( #22542, #54749, #3264, #11248 ) ) ;
#65208 = CARTESIAN_POINT ( 'NONE',  ( 7.250000000000004441, 7.450000000000001954, -15.50000000000000000 ) ) ;
#65209 = CARTESIAN_POINT ( 'NONE',  ( -6.817976262117325881, -9.737023737882786634, 54.00000000000000711 ) ) ;
#65210 = VERTEX_POINT ( 'NONE', #7469 ) ;
#65211 = CARTESIAN_POINT ( 'NONE',  ( 0.2500000000000008882, -0.2499999999999991396, -26.75000000000000000 ) ) ;
#65212 = ADVANCED_FACE ( 'NONE', ( #24442, #29040 ), #50956, .F. ) ;
#65213 = LINE ( 'NONE', #43969, #16498 ) ;
#65214 = CIRCLE ( 'NONE', #62925, 0.1749999999999998224 ) ;
#65215 = AXIS2_PLACEMENT_3D ( 'NONE', #57860, #35225, #56807 ) ;
#65216 = VECTOR ( 'NONE', #57151, 1000.000000000000000 ) ;
#65217 = DIRECTION ( 'NONE',  ( -0.000000000000000000, 1.000000000000000000, -0.000000000000000000 ) ) ;
#65218 = DIRECTION ( 'NONE',  ( 0.000000000000000000, 1.000000000000000000, 0.000000000000000000 ) ) ;
#65219 = ORIENTED_EDGE ( 'NONE', *, *, #65957, .T. ) ;
#65221 = ORIENTED_EDGE ( 'NONE', *, *, #18031, .F. ) ;
#65220 = CYLINDRICAL_SURFACE ( 'NONE', #67835, 1.000000000000000000 ) ;
#65222 = VECTOR ( 'NONE', #4422, 1000.000000000000000 ) ;
#65223 = AXIS2_PLACEMENT_3D ( 'NONE', #46796, #63068, #25241 ) ;
#65224 = LINE ( 'NONE', #59562, #10183 ) ;
#65225 = DIRECTION ( 'NONE',  ( -1.836970198721029934E-16, 1.836970198721036344E-16, -1.000000000000000000 ) ) ;
#65226 = DIRECTION ( 'NONE',  ( -3.491481338843132961E-15, -1.000000000000000000, -1.836970198721029934E-16 ) ) ;
#65227 = ORIENTED_EDGE ( 'NONE', *, *, #63341, .F. ) ;
#65228 = AXIS2_PLACEMENT_3D ( 'NONE', #62022, #68040, #35494 ) ;
#65230 = LINE ( 'NONE', #16778, #39009 ) ;
#65229 = AXIS2_PLACEMENT_3D ( 'NONE', #44752, #6929, #62774 ) ;
#65231 = CARTESIAN_POINT ( 'NONE',  ( -8.697938382363135545, 2.406732575409538111, 26.00000000000000711 ) ) ;
#65232 = VERTEX_POINT ( 'NONE', #38958 ) ;
#65233 = ORIENTED_EDGE ( 'NONE', *, *, #47376, .T. ) ;
#65234 = EDGE_CURVE ( 'NONE', #69196, #45686, #7115, .T. ) ;
#65235 = EDGE_LOOP ( 'NONE', ( #35886, #6946, #63581, #27304 ) ) ;
#65236 = DIRECTION ( 'NONE',  ( -1.836970198721029934E-16, 1.836970198721036344E-16, -1.000000000000000000 ) ) ;
#65237 = CARTESIAN_POINT ( 'NONE',  ( 49.00000000000000000, -0.1999999999911430404, -8.864436962241481021E-12 ) ) ;
#65238 = ADVANCED_FACE ( 'NONE', ( #33658 ), #45638, .F. ) ;
#65239 = CARTESIAN_POINT ( 'NONE',  ( 9.955011587777175208, 2.752095193409277218, 195.0000000000000284 ) ) ;
#65240 =( NAMED_UNIT ( * ) SI_UNIT ( $, .STERADIAN. ) SOLID_ANGLE_UNIT ( ) );
#65241 = AXIS2_PLACEMENT_3D ( 'NONE', #69951, #60024, #53699 ) ;
#65242 = ORIENTED_EDGE ( 'NONE', *, *, #14618, .T. ) ;
#65243 = ORIENTED_EDGE ( 'NONE', *, *, #38103, .F. ) ;
#65244 = ORIENTED_EDGE ( 'NONE', *, *, #10361, .F. ) ;
#65245 = EDGE_CURVE ( 'NONE', #55597, #24719, #50262, .T. ) ;
#65246 = CYLINDRICAL_SURFACE ( 'NONE', #49717, 0.1999999999999987899 ) ;
#65247 = ORIENTED_EDGE ( 'NONE', *, *, #8533, .F. ) ;
#65248 = EDGE_CURVE ( 'NONE', #68268, #27121, #44956, .T. ) ;
#65249 = ORIENTED_EDGE ( 'NONE', *, *, #20020, .F. ) ;
#65250 = ORIENTED_EDGE ( 'NONE', *, *, #11722, .T. ) ;
#65251 = VERTEX_POINT ( 'NONE', #49915 ) ;
#65252 = DIRECTION ( 'NONE',  ( -1.000000000000000000, 0.000000000000000000, 0.000000000000000000 ) ) ;
#65253 = EDGE_CURVE ( 'NONE', #55364, #6741, #45290, .T. ) ;
#65255 = ORIENTED_EDGE ( 'NONE', *, *, #2175, .F. ) ;
#65254 = LINE ( 'NONE', #11477, #11883 ) ;
#65256 = CARTESIAN_POINT ( 'NONE',  ( 72.77321854994619343, 47.95351654967443977, 29.00000000000000000 ) ) ;
#65257 = DIRECTION ( 'NONE',  ( -0.000000000000000000, 0.000000000000000000, -1.000000000000000000 ) ) ;
#65258 = FACE_BOUND ( 'NONE', #53378, .T. ) ;
#65259 = VECTOR ( 'NONE', #65200, 1000.000000000000000 ) ;
#65260 = ADVANCED_FACE ( 'NONE', ( #1471 ), #34685, .T. ) ;
#65261 = EDGE_LOOP ( 'NONE', ( #33723, #56910, #54808, #11127 ) ) ;
#65262 = EDGE_CURVE ( 'NONE', #22100, #22191, #36553, .T. ) ;
#65263 = ADVANCED_FACE ( 'NONE', ( #55917 ), #56264, .F. ) ;
#65264 = EDGE_CURVE ( 'NONE', #16188, #23962, #13473, .T. ) ;
#65265 = DIRECTION ( 'NONE',  ( 0.000000000000000000, 1.000000000000000000, 0.000000000000000000 ) ) ;
#65266 = VERTEX_POINT ( 'NONE', #57663 ) ;
#65267 = PLANE ( 'NONE',  #37110 ) ;
#65268 = EDGE_CURVE ( 'NONE', #57460, #67717, #67581, .T. ) ;
#65269 = VECTOR ( 'NONE', #66828, 1000.000000000000000 ) ;
#65270 = CARTESIAN_POINT ( 'NONE',  ( -7.250000000000000888, 7.250000000000001776, -20.50000000000000000 ) ) ;
#65271 = DIRECTION ( 'NONE',  ( -0.000000000000000000, -0.000000000000000000, -1.000000000000000000 ) ) ;
#65272 = CARTESIAN_POINT ( 'NONE',  ( 2.290483450353350658, -9.841277389592804070, 455.0000000000000568 ) ) ;
#65273 = VECTOR ( 'NONE', #11660, 1000.000000000000000 ) ;
#65274 = ORIENTED_EDGE ( 'NONE', *, *, #62252, .F. ) ;
#65275 = DIRECTION ( 'NONE',  ( 0.000000000000000000, 0.000000000000000000, 1.000000000000000000 ) ) ;
#65276 = CIRCLE ( 'NONE', #20085, 0.5000000000001386669 ) ;
#65277 = DIRECTION ( 'NONE',  ( 0.000000000000000000, 0.7071067811865480168, -0.7071067811865470176 ) ) ;
#65278 = CARTESIAN_POINT ( 'NONE',  ( -29.50000000000000355, -11.50000000000100009, -15.00000000000084910 ) ) ;
#65279 = DIRECTION ( 'NONE',  ( 0.000000000000000000, 0.000000000000000000, -1.000000000000000000 ) ) ;
#65280 = LINE ( 'NONE', #49007, #16658 ) ;
#65281 = DIRECTION ( 'NONE',  ( 8.359604446858499085E-15, 1.000000000000000000, 0.000000000000000000 ) ) ;
#65282 = EDGE_CURVE ( 'NONE', #278, #12416, #68633, .T. ) ;
#65283 = LINE ( 'NONE', #59265, #12950 ) ;
#65284 = DIRECTION ( 'NONE',  ( -1.000000000000000000, 0.000000000000000000, 0.000000000000000000 ) ) ;
#65285 = ADVANCED_FACE ( 'NONE', ( #41745 ), #58382, .F. ) ;
#65286 = VECTOR ( 'NONE', #53540, 1000.000000000000000 ) ;
#65287 = VERTEX_POINT ( 'NONE', #62606 ) ;
#65288 = DIRECTION ( 'NONE',  ( -1.000000000000000000, 0.000000000000000000, 0.000000000000000000 ) ) ;
#65289 = LINE ( 'NONE', #66312, #33062 ) ;
#65290 = DIRECTION ( 'NONE',  ( 0.7071067811865446862, -0.7071067811865503483, 0.000000000000000000 ) ) ;
#65291 = CARTESIAN_POINT ( 'NONE',  ( 49.00000000000000000, 13.66939075806899950, 20.80000000000000426 ) ) ;
#65292 = ORIENTED_EDGE ( 'NONE', *, *, #67397, .F. ) ;
#65293 = CYLINDRICAL_SURFACE ( 'NONE', #53610, 1.000000000000002665 ) ;
#65294 = DIRECTION ( 'NONE',  ( 1.836970198721029934E-16, 1.836970198721010706E-16, -1.000000000000000000 ) ) ;
#65295 = DIRECTION ( 'NONE',  ( -1.000000000000000000, 0.000000000000000000, 0.000000000000000000 ) ) ;
#65296 = DIRECTION ( 'NONE',  ( -1.000000000000000000, 0.000000000000000000, 0.000000000000000000 ) ) ;
#65297 = DIRECTION ( 'NONE',  ( -1.000000000000000000, 0.000000000000000000, 0.000000000000000000 ) ) ;
#65298 = DIRECTION ( 'NONE',  ( 0.000000000000000000, 0.7071067811865475727, 0.7071067811865475727 ) ) ;
#65299 = ORIENTED_EDGE ( 'NONE', *, *, #32046, .F. ) ;
#65300 = EDGE_CURVE ( 'NONE', #45407, #12591, #44447, .T. ) ;
#65301 = ORIENTED_EDGE ( 'NONE', *, *, #2871, .F. ) ;
#65302 = CARTESIAN_POINT ( 'NONE',  ( -11.47551654964682122, -10.20488345035336941, 455.0000000000000568 ) ) ;
#65303 = CARTESIAN_POINT ( 'NONE',  ( -9.942044687070568543, 9.234937905883914055, 455.0000000000000568 ) ) ;
#65304 = STYLED_ITEM ( 'NONE', ( #6061 ), #21410 ) ;
#65305 = ORIENTED_EDGE ( 'NONE', *, *, #44824, .F. ) ;
#65306 = FACE_OUTER_BOUND ( 'NONE', #2742, .T. ) ;
#65307 = ORIENTED_EDGE ( 'NONE', *, *, #27107, .T. ) ;
#65308 = FACE_OUTER_BOUND ( 'NONE', #40743, .T. ) ;
#65309 = ORIENTED_EDGE ( 'NONE', *, *, #2366, .F. ) ;
#65310 = EDGE_LOOP ( 'NONE', ( #37837, #21214, #31444, #22011 ) ) ;
#65311 = DIRECTION ( 'NONE',  ( 0.000000000000000000, 1.000000000000000000, 0.000000000000000000 ) ) ;
#65312 = ORIENTED_EDGE ( 'NONE', *, *, #32892, .F. ) ;
#65313 = CYLINDRICAL_SURFACE ( 'NONE', #61345, 0.1749999999999998224 ) ;
#65314 = AXIS2_PLACEMENT_3D ( 'NONE', #12296, #67096, #39188 ) ;
#65315 = EDGE_CURVE ( 'NONE', #19554, #33973, #60162, .T. ) ;
#65316 = DIRECTION ( 'NONE',  ( -1.000000000000000000, 0.000000000000000000, -0.000000000000000000 ) ) ;
#65317 = DIRECTION ( 'NONE',  ( -1.000000000000000000, 0.000000000000000000, 0.000000000000000000 ) ) ;
#65318 = ORIENTED_EDGE ( 'NONE', *, *, #39318, .T. ) ;
#65319 = EDGE_LOOP ( 'NONE', ( #25071, #13834, #55640, #16018 ) ) ;
#65320 = EDGE_CURVE ( 'NONE', #4176, #45981, #7205, .T. ) ;
#65321 = CARTESIAN_POINT ( 'NONE',  ( 8.900000000000002132, 0.000000000000000000, 0.000000000000000000 ) ) ;
#65322 = AXIS2_PLACEMENT_3D ( 'NONE', #38866, #60781, #44860 ) ;
#65323 = CARTESIAN_POINT ( 'NONE',  ( 1.690483450353418959, 10.73351654964659652, 455.0000000000000568 ) ) ;
#65324 = ORIENTED_EDGE ( 'NONE', *, *, #5143, .T. ) ;
#65325 = EDGE_CURVE ( 'NONE', #24174, #523, #63321, .T. ) ;
#65326 = ORIENTED_EDGE ( 'NONE', *, *, #52374, .F. ) ;
#65328 = ORIENTED_EDGE ( 'NONE', *, *, #32268, .F. ) ;
#65327 = CONTEXT_DEPENDENT_SHAPE_REPRESENTATION ( #32284, #17142 ) ;
#65329 = ADVANCED_FACE ( 'NONE', ( #19132 ), #36444, .T. ) ;
#65330 = PLANE ( 'NONE',  #12986 ) ;
#65332 = VERTEX_POINT ( 'NONE', #53080 ) ;
#65331 = DIRECTION ( 'NONE',  ( 0.000000000000000000, 0.000000000000000000, 1.000000000000000000 ) ) ;
#65333 = CIRCLE ( 'NONE', #10016, 0.1999999999999996503 ) ;
#65334 = DIRECTION ( 'NONE',  ( -1.000000000000000000, 0.000000000000000000, 0.000000000000000000 ) ) ;
#65335 = CARTESIAN_POINT ( 'NONE',  ( -30.00000000000000000, -13.54524521594299991, -17.53999999999999915 ) ) ;
#65336 = VERTEX_POINT ( 'NONE', #41044 ) ;
#65337 = VERTEX_POINT ( 'NONE', #46349 ) ;
#65338 = VERTEX_POINT ( 'NONE', #19476 ) ;
#65339 = DIRECTION ( 'NONE',  ( 1.000000000000000000, 0.000000000000000000, 0.000000000000000000 ) ) ;
#65340 = DIRECTION ( 'NONE',  ( -0.000000000000000000, 3.673940397442059868E-16, -1.000000000000000000 ) ) ;
#65341 = ORIENTED_EDGE ( 'NONE', *, *, #10471, .F. ) ;
#65342 = CARTESIAN_POINT ( 'NONE',  ( 14.25000000000000000, -0.3156864504677177052, 22.25638000318208753 ) ) ;
#65343 = CARTESIAN_POINT ( 'NONE',  ( -10.73351654964669599, -1.690483450353341910, 455.0000000000000568 ) ) ;
#65345 = ORIENTED_EDGE ( 'NONE', *, *, #54113, .F. ) ;
#65344 = FACE_OUTER_BOUND ( 'NONE', #26352, .T. ) ;
#65346 = ORIENTED_EDGE ( 'NONE', *, *, #65120, .T. ) ;
#65347 = CARTESIAN_POINT ( 'NONE',  ( 6.849523737882818430, 10.30047626211719169, 54.00000000000000711 ) ) ;
#65348 = CARTESIAN_POINT ( 'NONE',  ( 7.806483450353372433, 11.11351654964662039, 195.0000000000000284 ) ) ;
#65349 = CARTESIAN_POINT ( 'NONE',  ( 10.31452373788281562, -3.857023737882824932, 54.00000000000000711 ) ) ;
#65350 = LINE ( 'NONE', #27176, #66714 ) ;
#65351 = AXIS2_PLACEMENT_3D ( 'NONE', #12919, #46159, #50426 ) ;
#65352 = DIRECTION ( 'NONE',  ( 0.000000000000000000, -0.000000000000000000, 1.000000000000000000 ) ) ;
#65353 = ORIENTED_EDGE ( 'NONE', *, *, #26942, .T. ) ;
#65354 = PLANE ( 'NONE',  #66301 ) ;
#65355 = CARTESIAN_POINT ( 'NONE',  ( -25.50000000000000355, -5.200000000000001066, -20.49999999999999645 ) ) ;
#65356 = ADVANCED_FACE ( 'NONE', ( #19827 ), #40697, .T. ) ;
#65357 = DIRECTION ( 'NONE',  ( 1.836970198721029934E-16, 1.836970198721010706E-16, -1.000000000000000000 ) ) ;
#65358 = VECTOR ( 'NONE', #49968, 1000.000000000000000 ) ;
#65359 = DIRECTION ( 'NONE',  ( -1.000000000000000000, 0.000000000000000000, 0.000000000000000000 ) ) ;
#65360 = EDGE_CURVE ( 'NONE', #7067, #65973, #35379, .T. ) ;
#65361 = FACE_OUTER_BOUND ( 'NONE', #29785, .T. ) ;
#65362 = LINE ( 'NONE', #43087, #61973 ) ;
#65363 = ADVANCED_FACE ( 'NONE', ( #26194 ), #25852, .F. ) ;
#65364 = FACE_OUTER_BOUND ( 'NONE', #66994, .T. ) ;
#65365 = VECTOR ( 'NONE', #68742, 1000.000000000000000 ) ;
#65366 = CARTESIAN_POINT ( 'NONE',  ( -7.450000000000001954, 7.250000000000000000, -22.50000000000000000 ) ) ;
#65367 = ORIENTED_EDGE ( 'NONE', *, *, #56069, .F. ) ;
#65368 = PLANE ( 'NONE',  #18496 ) ;
#65369 = CARTESIAN_POINT ( 'NONE',  ( 30.00000000000000000, -17.35230188589299871, 15.35019951917099945 ) ) ;
#65370 = EDGE_LOOP ( 'NONE', ( #68260, #62335, #66790, #30103 ) ) ;
#65371 = LINE ( 'NONE', #16924, #61616 ) ;
#65372 = CARTESIAN_POINT ( 'NONE',  ( 25.50000000000000355, -15.50000000000000000, 20.49999999999999645 ) ) ;
#65373 = AXIS2_PLACEMENT_3D ( 'NONE', #20923, #5387, #21633 ) ;
#65374 = CARTESIAN_POINT ( 'NONE',  ( 40.90000000000000568, 21.00000000000000000, -16.96999999999999886 ) ) ;
#65375 = CARTESIAN_POINT ( 'NONE',  ( -11.77351654964674310, -4.406483450353321452, 455.0000000000000568 ) ) ;
#65376 = DIRECTION ( 'NONE',  ( 1.000000000000000000, 0.000000000000000000, 0.000000000000000000 ) ) ;
#65377 = AXIS2_PLACEMENT_3D ( 'NONE', #11250, #39170, #32826 ) ;
#65378 = CARTESIAN_POINT ( 'NONE',  ( -11.50000000000000000, -11.50000000000000000, 19.00000000000000000 ) ) ;
#65379 = EDGE_LOOP ( 'NONE', ( #69218, #25366 ) ) ;
#65380 = CARTESIAN_POINT ( 'NONE',  ( 15.91434062215688350, -0.3156604612129282894, -23.70415600323552852 ) ) ;
#65381 = DIRECTION ( 'NONE',  ( -1.000000000000000000, 0.000000000000000000, 0.000000000000000000 ) ) ;
#65382 = EDGE_CURVE ( 'NONE', #26490, #32938, #30091, .T. ) ;
#65383 = ORIENTED_EDGE ( 'NONE', *, *, #19041, .F. ) ;
#65384 = CARTESIAN_POINT ( 'NONE',  ( 28.00000000000000000, -16.28999999999999915, 14.50000000000000000 ) ) ;
#65385 = FACE_OUTER_BOUND ( 'NONE', #48892, .T. ) ;
#65386 = CARTESIAN_POINT ( 'NONE',  ( 275.0000000000000000, -20.50000000000000000, 17.00000000000000000 ) ) ;
#65387 = ORIENTED_EDGE ( 'NONE', *, *, #24806, .T. ) ;
#65388 = VERTEX_POINT ( 'NONE', #62258 ) ;
#65389 = CARTESIAN_POINT ( 'NONE',  ( 8.465062094116069247, -4.255011587777349114, 455.0000000000000568 ) ) ;
#65390 = ORIENTED_EDGE ( 'NONE', *, *, #44937, .T. ) ;
#65391 = ORIENTED_EDGE ( 'NONE', *, *, #56278, .T. ) ;
#65392 = EDGE_CURVE ( 'NONE', #35877, #6775, #3226, .T. ) ;
#65393 = DIRECTION ( 'NONE',  ( 8.673617379884013384E-15, 1.000000000000000000, 0.000000000000000000 ) ) ;
#65394 = DIRECTION ( 'NONE',  ( 0.000000000000000000, -1.000000000000000000, 0.000000000000000000 ) ) ;
#65395 = CARTESIAN_POINT ( 'NONE',  ( 15.50000000000000000, -5.000000000000000000, -18.50000000000000000 ) ) ;
#65396 = ORIENTED_EDGE ( 'NONE', *, *, #44364, .F. ) ;
#65397 = FACE_OUTER_BOUND ( 'NONE', #26993, .T. ) ;
#65399 = DIRECTION ( 'NONE',  ( -0.7071067811865474617, 0.7071067811865474617, 0.000000000000000000 ) ) ;
#65398 = CARTESIAN_POINT ( 'NONE',  ( 7.616533956692244978, 8.593516549646574632, 455.0000000000000568 ) ) ;
#65400 = EDGE_LOOP ( 'NONE', ( #19501, #13464, #16571, #50815 ) ) ;
#65401 = ORIENTED_EDGE ( 'NONE', *, *, #8550, .F. ) ;
#65403 = VERTEX_POINT ( 'NONE', #42098 ) ;
#65402 = CARTESIAN_POINT ( 'NONE',  ( 7.000000000000000000, -40.30000000000000426, -12.20000000000000107 ) ) ;
#65404 = EDGE_CURVE ( 'NONE', #68798, #6502, #16113, .T. ) ;
#65405 = EDGE_LOOP ( 'NONE', ( #18892, #1360, #38199, #60189 ) ) ;
#65406 = EDGE_CURVE ( 'NONE', #10776, #31223, #8870, .T. ) ;
#65407 = VECTOR ( 'NONE', #24622, 1000.000000000000000 ) ;
#65408 = EDGE_CURVE ( 'NONE', #54829, #29989, #25142, .T. ) ;
#65409 = ADVANCED_FACE ( 'NONE', ( #29086 ), #44636, .T. ) ;
#65410 = CARTESIAN_POINT ( 'NONE',  ( 181.4833316329832940, 0.000000000000000000, 328.5239988703752942 ) ) ;
#65411 = CARTESIAN_POINT ( 'NONE',  ( 25.50000000000000355, -5.200000000000001066, -24.75000000000000000 ) ) ;
#65412 = EDGE_CURVE ( 'NONE', #19489, #57821, #16266, .T. ) ;
#65413 = EDGE_LOOP ( 'NONE', ( #3546, #51549, #11887, #66835 ) ) ;
#65414 = ORIENTED_EDGE ( 'NONE', *, *, #49773, .T. ) ;
#65415 = VECTOR ( 'NONE', #68301, 1000.000000000000000 ) ;
#65416 = DIRECTION ( 'NONE',  ( -0.7671651518153006499, -0.6414496315691565753, -2.356647714346250026E-16 ) ) ;
#65417 = DIRECTION ( 'NONE',  ( 0.000000000000000000, 0.000000000000000000, 1.000000000000000000 ) ) ;
#65418 = ORIENTED_EDGE ( 'NONE', *, *, #1313, .T. ) ;
#65419 = DIRECTION ( 'NONE',  ( 1.836970198721029934E-16, -1.836970198721036344E-16, 1.000000000000000000 ) ) ;
#65420 = CARTESIAN_POINT ( 'NONE',  ( 8.606483450353360709, 7.603567055985452683, 195.0000000000000284 ) ) ;
#65421 = CARTESIAN_POINT ( 'NONE',  ( 106.4257688009193430, 10.00000000000000000, 327.4830310981789694 ) ) ;
#65422 = VERTEX_POINT ( 'NONE', #50999 ) ;
#65423 = VECTOR ( 'NONE', #43627, 1000.000000000000000 ) ;
#65424 = LINE ( 'NONE', #27935, #16552 ) ;
#65425 = LINE ( 'NONE', #60103, #22699 ) ;
#65427 = VERTEX_POINT ( 'NONE', #12805 ) ;
#65426 = CARTESIAN_POINT ( 'NONE',  ( -15.50000000000000000, -0.4000000000005236034, 25.79999999999947136 ) ) ;
#65429 = ORIENTED_EDGE ( 'NONE', *, *, #16546, .F. ) ;
#65428 = CARTESIAN_POINT ( 'NONE',  ( 5.552858015815566262, 7.342976262117203667, 26.00000000000000711 ) ) ;
#65430 = FACE_OUTER_BOUND ( 'NONE', #60138, .T. ) ;
#65431 = AXIS2_PLACEMENT_3D ( 'NONE', #12783, #45313, #45665 ) ;
#65432 = DIRECTION ( 'NONE',  ( -1.000000000000000000, 0.000000000000000000, 0.000000000000000000 ) ) ;
#65433 = CARTESIAN_POINT ( 'NONE',  ( -2.530476262117322239, -9.737023737882823937, 26.00000000000000711 ) ) ;
#65434 = CYLINDRICAL_SURFACE ( 'NONE', #61711, 0.4999999999945534124 ) ;
#65435 = DIRECTION ( 'NONE',  ( 1.334402673828313093E-16, 1.000000000000000000, 0.000000000000000000 ) ) ;
#65436 = DIRECTION ( 'NONE',  ( 0.000000000000000000, -0.000000000000000000, 1.000000000000000000 ) ) ;
#65437 = ORIENTED_EDGE ( 'NONE', *, *, #6491, .F. ) ;
#65438 = FACE_OUTER_BOUND ( 'NONE', #56234, .T. ) ;
#65440 = ORIENTED_EDGE ( 'NONE', *, *, #48662, .T. ) ;
#65439 = DIRECTION ( 'NONE',  ( 0.000000000000000000, -1.000000000000000000, 0.000000000000000000 ) ) ;
#65442 = EDGE_LOOP ( 'NONE', ( #57453, #57932, #60735, #37935 ) ) ;
#65441 = DIRECTION ( 'NONE',  ( 0.000000000000000000, 1.000000000000000000, 0.000000000000000000 ) ) ;
#65443 = FACE_OUTER_BOUND ( 'NONE', #17413, .T. ) ;
#65444 = EDGE_CURVE ( 'NONE', #11546, #54114, #67619, .T. ) ;
#65445 = CARTESIAN_POINT ( 'NONE',  ( 11.00000000000000000, -17.50000000000000000, -15.70500000000000007 ) ) ;
#65446 = ADVANCED_FACE ( 'NONE', ( #66566, #34365 ), #67270, .F. ) ;
#65447 = VERTEX_POINT ( 'NONE', #50649 ) ;
#65448 = LINE ( 'NONE', #17693, #12790 ) ;
#65449 = DIRECTION ( 'NONE',  ( -1.836970198721029934E-16, 1.836970198721036590E-16, -1.000000000000000000 ) ) ;
#65451 = VERTEX_POINT ( 'NONE', #66226 ) ;
#65450 = ADVANCED_FACE ( 'NONE', ( #2213, #34731 ), #23438, .T. ) ;
#65452 = CARTESIAN_POINT ( 'NONE',  ( -1.853252480934834967, -9.417013320880835536, 195.0000000000000284 ) ) ;
#65453 = CARTESIAN_POINT ( 'NONE',  ( 0.5000000000000000000, -42.00000000000000000, 27.00000000000000000 ) ) ;
#65454 = LINE ( 'NONE', #17012, #49493 ) ;
#65455 = PLANE ( 'NONE',  #57581 ) ;
#65456 = VECTOR ( 'NONE', #3452, 1000.000000000000000 ) ;
#65457 = AXIS2_PLACEMENT_3D ( 'NONE', #35009, #61179, #46327 ) ;
#65458 = DIRECTION ( 'NONE',  ( 0.000000000000000000, 0.000000000000000000, -1.000000000000000000 ) ) ;
#65459 = ORIENTED_EDGE ( 'NONE', *, *, #39862, .T. ) ;
#65460 = LINE ( 'NONE', #21971, #46325 ) ;
#65461 = ORIENTED_EDGE ( 'NONE', *, *, #62597, .T. ) ;
#65462 = ORIENTED_EDGE ( 'NONE', *, *, #9945, .F. ) ;
#65463 = VECTOR ( 'NONE', #13764, 1000.000000000000000 ) ;
#65464 = CARTESIAN_POINT ( 'NONE',  ( -7.250000000000001776, -7.249999999999998224, -24.50000000000000000 ) ) ;
#65465 = LINE ( 'NONE', #48163, #26375 ) ;
#65466 = AXIS2_PLACEMENT_3D ( 'NONE', #44555, #12718, #28644 ) ;
#65467 = FACE_OUTER_BOUND ( 'NONE', #63395, .T. ) ;
#65468 = LINE ( 'NONE', #22675, #55512 ) ;
#65469 = ORIENTED_EDGE ( 'NONE', *, *, #57008, .T. ) ;
#65470 = ORIENTED_EDGE ( 'NONE', *, *, #32241, .F. ) ;
#65472 = ORIENTED_EDGE ( 'NONE', *, *, #60640, .F. ) ;
#65471 = CARTESIAN_POINT ( 'NONE',  ( 3.724485858128677940, -7.408280051175156977, 26.00000000000000000 ) ) ;
#65473 = ORIENTED_EDGE ( 'NONE', *, *, #59770, .F. ) ;
#65474 = AXIS2_PLACEMENT_3D ( 'NONE', #65204, #5101, #27706 ) ;
#65475 = DIRECTION ( 'NONE',  ( 1.836970198721029934E-16, 1.836970198721010706E-16, -1.000000000000000000 ) ) ;
#65476 = LINE ( 'NONE', #16698, #25299 ) ;
#65477 = DIRECTION ( 'NONE',  ( -1.000000000000000000, 0.000000000000000000, -0.000000000000000000 ) ) ;
#65478 = CARTESIAN_POINT ( 'NONE',  ( -16.75000000000000000, -2.500000000000000000, -23.22168783648699986 ) ) ;
#65479 = AXIS2_PLACEMENT_3D ( 'NONE', #37748, #69583, #20777 ) ;
#65481 = FACE_OUTER_BOUND ( 'NONE', #439, .T. ) ;
#65480 = DIRECTION ( 'NONE',  ( 0.000000000000000000, 0.000000000000000000, -1.000000000000000000 ) ) ;
#65482 = ORIENTED_EDGE ( 'NONE', *, *, #40272, .T. ) ;
#65484 = ORIENTED_EDGE ( 'NONE', *, *, #26234, .F. ) ;
#65483 = DIRECTION ( 'NONE',  ( 0.000000000000000000, 1.000000000000000000, 0.000000000000000000 ) ) ;
#65485 = ORIENTED_EDGE ( 'NONE', *, *, #43454, .T. ) ;
#65486 = VERTEX_POINT ( 'NONE', #56655 ) ;
#65487 = DIRECTION ( 'NONE',  ( 0.000000000000000000, 1.000000000000000000, 0.000000000000000000 ) ) ;
#65488 = EDGE_CURVE ( 'NONE', #39543, #53282, #13866, .T. ) ;
#65489 = CARTESIAN_POINT ( 'NONE',  ( -9.722976262117249746, -3.682023737882726522, 54.00000000000000711 ) ) ;
#65490 = EDGE_CURVE ( 'NONE', #58160, #26913, #39345, .T. ) ;
#65491 = LINE ( 'NONE', #43913, #42148 ) ;
#65492 = ADVANCED_FACE ( 'NONE', ( #19175 ), #28729, .F. ) ;
#65493 = VECTOR ( 'NONE', #58188, 1000.000000000000000 ) ;
#65494 = DIRECTION ( 'NONE',  ( 0.000000000000000000, -1.000000000000000000, 0.000000000000000000 ) ) ;
#65495 = VERTEX_POINT ( 'NONE', #18462 ) ;
#65496 = ADVANCED_FACE ( 'NONE', ( #17783 ), #56995, .F. ) ;
#65497 = ORIENTED_EDGE ( 'NONE', *, *, #1163, .F. ) ;
#65498 = CARTESIAN_POINT ( 'NONE',  ( 9.900000000000000355, -0.000000000000000000, -20.80000000000000426 ) ) ;
#65499 = DIRECTION ( 'NONE',  ( 0.000000000000000000, 0.000000000000000000, -1.000000000000000000 ) ) ;
#65500 = ORIENTED_EDGE ( 'NONE', *, *, #17982, .F. ) ;
#65501 = VERTEX_POINT ( 'NONE', #56307 ) ;
#65502 = PLANE ( 'NONE',  #54272 ) ;
#65503 = EDGE_CURVE ( 'NONE', #38982, #58107, #60904, .T. ) ;
#65504 = CARTESIAN_POINT ( 'NONE',  ( 22.90000000000000213, -14.06939075806900163, -20.80000000000000426 ) ) ;
#65505 = VECTOR ( 'NONE', #32341, 1000.000000000000000 ) ;
#65507 = ORIENTED_EDGE ( 'NONE', *, *, #38237, .F. ) ;
#65506 = EDGE_CURVE ( 'NONE', #45889, #32328, #55611, .T. ) ;
#65508 = AXIS2_PLACEMENT_3D ( 'NONE', #18583, #40144, #55388 ) ;
#65509 = AXIS2_PLACEMENT_3D ( 'NONE', #57525, #51169, #61784 ) ;
#65510 = CARTESIAN_POINT ( 'NONE',  ( -8.333516549646715177, 11.11351654964659907, 195.0000000000000284 ) ) ;
#65512 = ORIENTED_EDGE ( 'NONE', *, *, #42189, .F. ) ;
#65511 = CARTESIAN_POINT ( 'NONE',  ( 10.92648345035337520, -9.106483450353492159, 455.0000000000000568 ) ) ;
#65513 = EDGE_LOOP ( 'NONE', ( #49296, #1485, #67847, #42785 ) ) ;
#65514 = CIRCLE ( 'NONE', #59854, 8.000000000000000000 ) ;
#65515 = CARTESIAN_POINT ( 'NONE',  ( 9.737023737882804397, 6.817976262117185549, 54.00000000000000711 ) ) ;
#65516 = DIRECTION ( 'NONE',  ( 1.000000000000000000, 0.000000000000000000, 0.000000000000000000 ) ) ;
#65517 = DIRECTION ( 'NONE',  ( -1.000000000000000000, 0.000000000000000000, 0.000000000000000000 ) ) ;
#65518 = DIRECTION ( 'NONE',  ( 0.5000000000000019984, 0.8660254037844375974, 3.181725716174716554E-16 ) ) ;
#65519 = CARTESIAN_POINT ( 'NONE',  ( 21.90000000000000213, -0.000000000000000000, 20.80000000000000426 ) ) ;
#65520 = ORIENTED_EDGE ( 'NONE', *, *, #39704, .F. ) ;
#65521 = CARTESIAN_POINT ( 'NONE',  ( 2.420780051175147829, -8.711985858128667104, 26.00000000000000000 ) ) ;
#65522 = VECTOR ( 'NONE', #57975, 1000.000000000000000 ) ;
#65524 = EDGE_LOOP ( 'NONE', ( #12361, #24190, #24706, #21396, #41386, #7129, #17347, #41987 ) ) ;
#65523 = LINE ( 'NONE', #31362, #37831 ) ;
#65525 = CARTESIAN_POINT ( 'NONE',  ( -6.486996718459931088, 2.617976262117183150, 54.00000000000000711 ) ) ;
#65526 = CARTESIAN_POINT ( 'NONE',  ( -11.50000000000000000, -12.00000000000000000, -10.52786404500095863 ) ) ;
#65527 = LINE ( 'NONE', #6804, #59612 ) ;
#65528 = CARTESIAN_POINT ( 'NONE',  ( -15.50000000000000000, 998.9628421096749662, 22.50000000000000000 ) ) ;
#65529 = CIRCLE ( 'NONE', #2275, 1.399999999999998579 ) ;
#65530 = CARTESIAN_POINT ( 'NONE',  ( 8.250000000000005329, -8.249999999999998224, -26.00000000000001066 ) ) ;
#65531 = ORIENTED_EDGE ( 'NONE', *, *, #16396, .F. ) ;
#65533 = ORIENTED_EDGE ( 'NONE', *, *, #39679, .T. ) ;
#65532 = ADVANCED_FACE ( 'NONE', ( #61241 ), #29426, .F. ) ;
#65534 = DIRECTION ( 'NONE',  ( 1.000000000000000000, 0.000000000000000000, 0.000000000000000000 ) ) ;
#65535 = ORIENTED_EDGE ( 'NONE', *, *, #44132, .T. ) ;
#65536 = VECTOR ( 'NONE', #32969, 1000.000000000000000 ) ;
#65537 = FACE_OUTER_BOUND ( 'NONE', #60436, .T. ) ;
#65538 = DIRECTION ( 'NONE',  ( 1.000000000000000000, -0.000000000000000000, -0.000000000000000000 ) ) ;
#65539 = ORIENTED_EDGE ( 'NONE', *, *, #61802, .F. ) ;
#65540 = DIRECTION ( 'NONE',  ( 1.000000000000000000, 0.000000000000000000, 0.000000000000000000 ) ) ;
#65541 = CARTESIAN_POINT ( 'NONE',  ( 7.250000000000005329, 8.250000000000001776, -24.00000000000000000 ) ) ;
#65543 = VERTEX_POINT ( 'NONE', #46048 ) ;
#65542 = EDGE_CURVE ( 'NONE', #38948, #41197, #29776, .T. ) ;
#65544 = PLANE ( 'NONE',  #53650 ) ;
#65545 = LINE ( 'NONE', #43280, #25540 ) ;
#65546 = DIRECTION ( 'NONE',  ( -1.836970198721029934E-16, 1.836970198721036590E-16, -1.000000000000000000 ) ) ;
#65547 = EDGE_CURVE ( 'NONE', #34324, #30734, #21921, .T. ) ;
#65548 = LINE ( 'NONE', #38338, #54363 ) ;
#65549 = ORIENTED_EDGE ( 'NONE', *, *, #59524, .F. ) ;
#65550 = CIRCLE ( 'NONE', #42981, 1.929199999999998028 ) ;
#65552 = ORIENTED_EDGE ( 'NONE', *, *, #14109, .T. ) ;
#65551 = DIRECTION ( 'NONE',  ( 0.000000000000000000, 0.000000000000000000, -1.000000000000000000 ) ) ;
#65553 = AXIS2_PLACEMENT_3D ( 'NONE', #53637, #63889, #15460 ) ;
#65554 = CARTESIAN_POINT ( 'NONE',  ( 29.50000000000000355, -12.00000000000000000, -10.69999999999999929 ) ) ;
#65555 = CARTESIAN_POINT ( 'NONE',  ( 290.0000000000000000, -42.50000000000000000, 26.50000000000000000 ) ) ;
#65556 = CARTESIAN_POINT ( 'NONE',  ( 7.000000000000000000, -26.28355339059299922, 9.766446609406699508 ) ) ;
#65557 = ORIENTED_EDGE ( 'NONE', *, *, #36821, .F. ) ;
#65558 = AXIS2_PLACEMENT_3D ( 'NONE', #52053, #14562, #25180 ) ;
#65559 = LINE ( 'NONE', #17115, #59310 ) ;
#65560 = DIRECTION ( 'NONE',  ( -0.7071067811865474617, -0.7071067811865474617, -0.000000000000000000 ) ) ;
#65561 = ORIENTED_EDGE ( 'NONE', *, *, #54951, .T. ) ;
#65562 = ORIENTED_EDGE ( 'NONE', *, *, #9387, .F. ) ;
#65563 = EDGE_CURVE ( 'NONE', #18065, #63676, #52056, .T. ) ;
#65564 = VECTOR ( 'NONE', #49385, 1000.000000000000000 ) ;
#65565 = VERTEX_POINT ( 'NONE', #58767 ) ;
#65566 = DIRECTION ( 'NONE',  ( 0.8660254037844510311, 0.4999999999999785727, 1.836970198720951294E-16 ) ) ;
#65567 = CARTESIAN_POINT ( 'NONE',  ( -6.651770455163739548, 7.517976262117183062, 54.00000000000000711 ) ) ;
#65569 = EDGE_CURVE ( 'NONE', #57625, #15217, #46391, .T. ) ;
#65568 = CARTESIAN_POINT ( 'NONE',  ( 11.50000000000000000, -11.50000000000000000, 19.00000000000000000 ) ) ;
#65570 = EDGE_CURVE ( 'NONE', #330, #11541, #10321, .T. ) ;
#65571 = ORIENTED_EDGE ( 'NONE', *, *, #22843, .T. ) ;
#65572 = ORIENTED_EDGE ( 'NONE', *, *, #56284, .F. ) ;
#65573 = ADVANCED_FACE ( 'NONE', ( #4672 ), #31896, .F. ) ;
#65574 = ORIENTED_EDGE ( 'NONE', *, *, #2759, .F. ) ;
#65576 = CARTESIAN_POINT ( 'NONE',  ( 283.0000000000000568, -25.60000000000000142, -17.35424868893542438 ) ) ;
#65575 = VECTOR ( 'NONE', #9254, 1000.000000000000000 ) ;
#65577 = VERTEX_POINT ( 'NONE', #25544 ) ;
#65578 = ADVANCED_FACE ( 'NONE', ( #67969 ), #53466, .T. ) ;
#65579 = ORIENTED_EDGE ( 'NONE', *, *, #46620, .F. ) ;
#65580 = ORIENTED_EDGE ( 'NONE', *, *, #3614, .T. ) ;
#65581 = ORIENTED_EDGE ( 'NONE', *, *, #48647, .T. ) ;
#65582 = DIRECTION ( 'NONE',  ( 0.000000000000000000, -0.7046037717806115097, 0.7096009616626348659 ) ) ;
#65583 = EDGE_CURVE ( 'NONE', #50762, #67938, #15281, .T. ) ;
#65585 = ORIENTED_EDGE ( 'NONE', *, *, #52429, .F. ) ;
#65584 = FACE_OUTER_BOUND ( 'NONE', #67398, .T. ) ;
#65586 = EDGE_CURVE ( 'NONE', #11693, #57047, #42495, .T. ) ;
#65587 = DIRECTION ( 'NONE',  ( 0.000000000000000000, 0.7096009616570518874, 0.7046037717862339012 ) ) ;
#65588 = DIRECTION ( 'NONE',  ( -1.000000000000000000, 0.000000000000000000, 0.000000000000000000 ) ) ;
#65589 = CARTESIAN_POINT ( 'NONE',  ( 41.09999999999999432, -14.06939075806901940, -20.80000000000000426 ) ) ;
#65590 = EDGE_LOOP ( 'NONE', ( #8894, #30950, #35200, #46859, #48009, #63220, #18087, #68535 ) ) ;
#65591 = CYLINDRICAL_SURFACE ( 'NONE', #37391, 0.5000000000004202194 ) ;
#65592 = LINE ( 'NONE', #21765, #45818 ) ;
#65593 = PLANE ( 'NONE',  #22528 ) ;
#65594 = VECTOR ( 'NONE', #30009, 1000.000000000000000 ) ;
#65595 = VERTEX_POINT ( 'NONE', #3971 ) ;
#65596 = LINE ( 'NONE', #28446, #57431 ) ;
#65597 = DIRECTION ( 'NONE',  ( -1.836970198721029934E-16, 1.836970198721036590E-16, -1.000000000000000000 ) ) ;
#65598 = CIRCLE ( 'NONE', #62207, 24.99999999998784972 ) ;
#65599 = DIRECTION ( 'NONE',  ( 1.000000000000000000, 0.000000000000000000, 0.000000000000000000 ) ) ;
#65600 = ADVANCED_FACE ( 'NONE', ( #52412 ), #41085, .F. ) ;
#65601 = ORIENTED_EDGE ( 'NONE', *, *, #54782, .T. ) ;
#65603 = CARTESIAN_POINT ( 'NONE',  ( 8.711985858128693749, -8.093267424590470327, 54.00000000000000711 ) ) ;
#65602 = VECTOR ( 'NONE', #57265, 1000.000000000000000 ) ;
#65604 = CARTESIAN_POINT ( 'NONE',  ( -13.00000000000000178, -17.35230188589299871, 15.35019951917099945 ) ) ;
#65605 = FACE_OUTER_BOUND ( 'NONE', #8190, .T. ) ;
#65606 = EDGE_CURVE ( 'NONE', #2526, #51110, #52782, .T. ) ;
#65607 = DIRECTION ( 'NONE',  ( -1.000000000000000000, 0.000000000000000000, 0.000000000000000000 ) ) ;
#65608 = CARTESIAN_POINT ( 'NONE',  ( 9.900000000000000355, 21.00000000000000000, 18.00000000000000355 ) ) ;
#65609 = CARTESIAN_POINT ( 'NONE',  ( 283.0000000000000568, -20.40000000000000213, -17.60000000000000142 ) ) ;
#65610 = AXIS2_PLACEMENT_3D ( 'NONE', #19979, #42237, #3718 ) ;
#65611 = ADVANCED_FACE ( 'NONE', ( #58430 ), #20574, .F. ) ;
#65612 = DIRECTION ( 'NONE',  ( 1.000000000000000000, -8.540177112501197482E-15, 0.000000000000000000 ) ) ;
#65613 = ORIENTED_EDGE ( 'NONE', *, *, #16243, .T. ) ;
#65614 = LINE ( 'NONE', #21789, #42856 ) ;
#65615 = CARTESIAN_POINT ( 'NONE',  ( -7.450000000000001954, -7.249999999999998224, -23.00000000000000000 ) ) ;
#65616 = ADVANCED_FACE ( 'NONE', ( #14223 ), #35785, .F. ) ;
#65617 = AXIS2_PLACEMENT_3D ( 'NONE', #8278, #30561, #52854 ) ;
#65618 = CARTESIAN_POINT ( 'NONE',  ( -11.19000000000000128, -12.00000000000000000, 0.000000000000000000 ) ) ;
#65619 = DIRECTION ( 'NONE',  ( -1.836970198721029934E-16, -1.836970198721010706E-16, 1.000000000000000000 ) ) ;
#65620 = ORIENTED_EDGE ( 'NONE', *, *, #4812, .F. ) ;
#65621 = DIRECTION ( 'NONE',  ( 0.000000000000000000, -1.000000000000000000, 0.000000000000000000 ) ) ;
#65622 = PLANE ( 'NONE',  #9066 ) ;
#65623 = CARTESIAN_POINT ( 'NONE',  ( 7.250000000000005329, -7.249999999999998224, -26.00000000000001066 ) ) ;
#65624 = CARTESIAN_POINT ( 'NONE',  ( 2.706483450353371900, 10.91351654964663354, 195.0000000000000284 ) ) ;
#65625 = EDGE_CURVE ( 'NONE', #43292, #19689, #4337, .T. ) ;
#65626 = LINE ( 'NONE', #38750, #18149 ) ;
#65627 = EDGE_LOOP ( 'NONE', ( #19440, #34466, #8863, #50134, #40024, #52427, #23606, #39066, #5129 ) ) ;
#65628 = ORIENTED_EDGE ( 'NONE', *, *, #39600, .T. ) ;
#65629 = LINE ( 'NONE', #49713, #24817 ) ;
#65630 = AXIS2_PLACEMENT_3D ( 'NONE', #4466, #47584, #69152 ) ;
#65631 = LINE ( 'NONE', #53645, #67313 ) ;
#65633 = VERTEX_POINT ( 'NONE', #14931 ) ;
#65632 = ADVANCED_FACE ( 'NONE', ( #42137 ), #63725, .F. ) ;
#65634 = EDGE_CURVE ( 'NONE', #9491, #46497, #31551, .T. ) ;
#65635 = CARTESIAN_POINT ( 'NONE',  ( 9.795823737882804139, 9.781776262117173104, 54.00000000000000711 ) ) ;
#65636 = EDGE_CURVE ( 'NONE', #43823, #49722, #69367, .T. ) ;
#65637 = ORIENTED_EDGE ( 'NONE', *, *, #46625, .T. ) ;
#65638 = EDGE_CURVE ( 'NONE', #11892, #13193, #37204, .T. ) ;
#65639 = ADVANCED_FACE ( 'NONE', ( #34199 ), #5970, .F. ) ;
#65640 = DIRECTION ( 'NONE',  ( -0.000000000000000000, -0.000000000000000000, 1.000000000000000000 ) ) ;
#65641 = VERTEX_POINT ( 'NONE', #61418 ) ;
#65642 = ORIENTED_EDGE ( 'NONE', *, *, #4511, .F. ) ;
#65643 = CARTESIAN_POINT ( 'NONE',  ( 15.50000000000000000, -0.1999999999999999556, 22.50000000000000000 ) ) ;
#65644 = AXIS2_PLACEMENT_3D ( 'NONE', #33671, #7132, #60877 ) ;
#65645 = ORIENTED_EDGE ( 'NONE', *, *, #18502, .F. ) ;
#65646 = CARTESIAN_POINT ( 'NONE',  ( 9.703773737882785966, -10.05377373788282469, 54.00000000000000711 ) ) ;
#65647 = ADVANCED_FACE ( 'NONE', ( #22580 ), #54757, .T. ) ;
#65648 = LINE ( 'NONE', #16866, #20328 ) ;
#65649 = CARTESIAN_POINT ( 'NONE',  ( 8.900000000000002132, 21.00000000000000000, 18.00000000000000355 ) ) ;
#65650 = VECTOR ( 'NONE', #42895, 1000.000000000000114 ) ;
#65651 = EDGE_CURVE ( 'NONE', #68084, #24330, #33864, .T. ) ;
#65652 = VERTEX_POINT ( 'NONE', #28557 ) ;
#65653 = ORIENTED_EDGE ( 'NONE', *, *, #43609, .F. ) ;
#65654 = CARTESIAN_POINT ( 'NONE',  ( 10.31452373788281562, -3.664523737882816157, 26.00000000000000711 ) ) ;
#65655 = EDGE_CURVE ( 'NONE', #35824, #51349, #12631, .T. ) ;
#65656 = DIRECTION ( 'NONE',  ( -4.268512490100335178E-15, -1.000000000000000000, 0.000000000000000000 ) ) ;
#65657 = ORIENTED_EDGE ( 'NONE', *, *, #47474, .F. ) ;
#65658 = ORIENTED_EDGE ( 'NONE', *, *, #47944, .T. ) ;
#65659 = AXIS2_PLACEMENT_3D ( 'NONE', #44224, #33961, #39613 ) ;
#65660 = CLOSED_SHELL ( 'NONE', ( #69810, #69069, #23729, #6505, #47164, #59281 ) ) ;
#65661 = ORIENTED_EDGE ( 'NONE', *, *, #34400, .F. ) ;
#65662 = CARTESIAN_POINT ( 'NONE',  ( 8.250000000000005329, 7.250000000000000888, -21.50000000000000000 ) ) ;
#65663 = EDGE_CURVE ( 'NONE', #53017, #6284, #39852, .T. ) ;
#65665 = ORIENTED_EDGE ( 'NONE', *, *, #54165, .F. ) ;
#65664 = LINE ( 'NONE', #622, #28578 ) ;
#65666 = AXIS2_PLACEMENT_3D ( 'NONE', #41461, #20239, #14944 ) ;
#65667 = EDGE_CURVE ( 'NONE', #46124, #1043, #37576, .T. ) ;
#65668 = CARTESIAN_POINT ( 'NONE',  ( 283.0000000000000568, -25.93000000000544958, -9.412893218815410634 ) ) ;
#65669 = DIRECTION ( 'NONE',  ( 0.000000000000000000, -1.000000000000000000, 3.989863994748342081E-13 ) ) ;
#65670 = ORIENTED_EDGE ( 'NONE', *, *, #54144, .T. ) ;
#65671 = ORIENTED_EDGE ( 'NONE', *, *, #13303, .T. ) ;
#65672 = VECTOR ( 'NONE', #23431, 1000.000000000000000 ) ;
#65673 = ADVANCED_FACE ( 'NONE', ( #28222 ), #39180, .F. ) ;
#65674 = DIRECTION ( 'NONE',  ( -1.000000000000000000, 0.000000000000000000, 0.000000000000000000 ) ) ;
#65675 = FACE_OUTER_BOUND ( 'NONE', #16629, .T. ) ;
#65676 = ORIENTED_EDGE ( 'NONE', *, *, #30358, .F. ) ;
#65677 = CARTESIAN_POINT ( 'NONE',  ( 16.89999999999999858, -14.06939075806900874, 20.80000000000001137 ) ) ;
#65678 = LINE ( 'NONE', #33831, #39191 ) ;
#65679 = CIRCLE ( 'NONE', #12605, 1.224999999999998757 ) ;
#65680 = ORIENTED_EDGE ( 'NONE', *, *, #58977, .F. ) ;
#65681 = ORIENTED_EDGE ( 'NONE', *, *, #2236, .T. ) ;
#65682 = CARTESIAN_POINT ( 'NONE',  ( 283.0000000000000568, -39.80000000000000426, 8.400000000000000355 ) ) ;
#65683 = LINE ( 'NONE', #34526, #10432 ) ;
#65684 = CARTESIAN_POINT ( 'NONE',  ( 7.250000000000005329, 7.250000000000000888, -26.00000000000001066 ) ) ;
#65685 = CARTESIAN_POINT ( 'NONE',  ( 7.500000000000000000, -25.60000000000000142, -20.00000000000000000 ) ) ;
#65686 = EDGE_CURVE ( 'NONE', #53195, #52907, #55786, .T. ) ;
#65687 = DIRECTION ( 'NONE',  ( 0.000000000000000000, 0.000000000000000000, -1.000000000000000000 ) ) ;
#65688 = ORIENTED_EDGE ( 'NONE', *, *, #65699, .T. ) ;
#65689 = CARTESIAN_POINT ( 'NONE',  ( -11.33351654964671162, 1.077516549646603483, 455.0000000000000568 ) ) ;
#65690 = DIRECTION ( 'NONE',  ( 1.000000000000000000, -0.000000000000000000, -0.000000000000000000 ) ) ;
#65691 = VECTOR ( 'NONE', #40282, 999.9999999999998863 ) ;
#65692 = FACE_OUTER_BOUND ( 'NONE', #53635, .T. ) ;
#65693 = EDGE_CURVE ( 'NONE', #67098, #63196, #66039, .T. ) ;
#65694 = CARTESIAN_POINT ( 'NONE',  ( 8.930623737882818602, -10.05377373788282469, 54.00000000000000711 ) ) ;
#65695 = CIRCLE ( 'NONE', #20526, 0.1749999999999998224 ) ;
#65696 = DIRECTION ( 'NONE',  ( -0.000000000000000000, -0.000000000000000000, -1.000000000000000000 ) ) ;
#65697 = DIRECTION ( 'NONE',  ( 0.000000000000000000, 3.989863994748342081E-13, 1.000000000000000000 ) ) ;
#65698 = DIRECTION ( 'NONE',  ( 0.000000000000000000, 1.000000000000000000, 0.000000000000000000 ) ) ;
#65699 = EDGE_CURVE ( 'NONE', #35394, #43479, #36150, .T. ) ;
#65700 = CARTESIAN_POINT ( 'NONE',  ( -11.07551654964667520, 9.791916549646639822, 195.0000000000000284 ) ) ;
#65701 = EDGE_LOOP ( 'NONE', ( #61670, #34033, #38443, #36706 ) ) ;
#65702 = CARTESIAN_POINT ( 'NONE',  ( -29.50000000000000355, -11.50000000000000000, 15.00000000000000000 ) ) ;
#65703 = EDGE_CURVE ( 'NONE', #27724, #21330, #39843, .T. ) ;
#65704 = LINE ( 'NONE', #65369, #45129 ) ;
#65705 = ORIENTED_EDGE ( 'NONE', *, *, #62944, .F. ) ;
#65706 = CARTESIAN_POINT ( 'NONE',  ( 283.0000000000000568, -25.60000000000000142, -15.10000000000000142 ) ) ;
#65707 = VECTOR ( 'NONE', #10083, 1000.000000000000000 ) ;
#65708 = CIRCLE ( 'NONE', #64600, 0.5999999999999989786 ) ;
#65709 = LINE ( 'NONE', #60384, #45753 ) ;
#65710 = CARTESIAN_POINT ( 'NONE',  ( -11.77351654964670935, 7.813516549646603693, 455.0000000000000568 ) ) ;
#65711 = CARTESIAN_POINT ( 'NONE',  ( 51.65933123007250316, 62.82898141569881290, 6.488953147413177264E-16 ) ) ;
#65712 = EDGE_CURVE ( 'NONE', #61801, #41571, #37625, .T. ) ;
#65713 = CARTESIAN_POINT ( 'NONE',  ( -11.00000000000000000, -16.28999999999999915, 14.50000000000000000 ) ) ;
#65714 = AXIS2_PLACEMENT_3D ( 'NONE', #50591, #66495, #50926 ) ;
#65715 = CARTESIAN_POINT ( 'NONE',  ( -9.722976262117258628, 7.290476262117218553, 54.00000000000000711 ) ) ;
#65716 = ORIENTED_EDGE ( 'NONE', *, *, #5070, .F. ) ;
#65717 = CARTESIAN_POINT ( 'NONE',  ( 25.57999999999999829, 0.000000000000000000, 0.000000000000000000 ) ) ;
#65718 = ORIENTED_EDGE ( 'NONE', *, *, #3313, .F. ) ;
#65719 = FACE_OUTER_BOUND ( 'NONE', #43272, .T. ) ;
#65720 = VECTOR ( 'NONE', #14834, 1000.000000000000114 ) ;
#65721 = EDGE_CURVE ( 'NONE', #59671, #6649, #17262, .T. ) ;
#65722 = LINE ( 'NONE', #15902, #1644 ) ;
#65723 = DIRECTION ( 'NONE',  ( 0.000000000000000000, 0.000000000000000000, 1.000000000000000000 ) ) ;
#65724 = ORIENTED_EDGE ( 'NONE', *, *, #34275, .T. ) ;
#65725 =( REPRESENTATION_RELATIONSHIP ('NONE','NONE', #4299, #49776 ) REPRESENTATION_RELATIONSHIP_WITH_TRANSFORMATION ( #59998 )SHAPE_REPRESENTATION_RELATIONSHIP( ) );
#65726 = EDGE_LOOP ( 'NONE', ( #62145, #32772, #21186, #44771 ) ) ;
#65727 = CARTESIAN_POINT ( 'NONE',  ( 9.737023737882799068, 6.817976262117189989, 26.00000000000000711 ) ) ;
#65728 = EDGE_LOOP ( 'NONE', ( #53546, #69201, #22089, #15334 ) ) ;
#65729 = ORIENTED_EDGE ( 'NONE', *, *, #47939, .F. ) ;
#65730 = UNCERTAINTY_MEASURE_WITH_UNIT (LENGTH_MEASURE( 1.000000000000000082E-05 ), #62162, 'distance_accuracy_value', 'NONE');
#65731 = CARTESIAN_POINT ( 'NONE',  ( 17.24945551514599984, -15.50000000000000000, 25.53140320652400064 ) ) ;
#65732 = CARTESIAN_POINT ( 'NONE',  ( 8.144523737882815695, 9.547976262117185087, 54.00000000000000711 ) ) ;
#65733 = LINE ( 'NONE', #38850, #68242 ) ;
#65734 = VERTEX_POINT ( 'NONE', #44470 ) ;
#65735 = CARTESIAN_POINT ( 'NONE',  ( 280.0000000000000000, -53.81370849898476649, -20.00000000000000000 ) ) ;
#65737 = CARTESIAN_POINT ( 'NONE',  ( -6.835476262117260227, 10.30047626211718104, 54.00000000000000711 ) ) ;
#65736 = DIRECTION ( 'NONE',  ( 0.000000000000000000, 1.000000000000000000, 0.000000000000000000 ) ) ;
#65738 = ORIENTED_EDGE ( 'NONE', *, *, #65721, .F. ) ;
#65740 = ORIENTED_EDGE ( 'NONE', *, *, #63392, .F. ) ;
#65739 = LINE ( 'NONE', #39542, #21840 ) ;
#65741 = AXIS2_PLACEMENT_3D ( 'NONE', #56471, #8018, #29592 ) ;
#65742 = ORIENTED_EDGE ( 'NONE', *, *, #53014, .F. ) ;
#65743 = DIRECTION ( 'NONE',  ( 0.000000000000000000, 0.000000000000000000, 1.000000000000000000 ) ) ;
#65744 = EDGE_CURVE ( 'NONE', #67142, #26429, #25193, .T. ) ;
#65745 = EDGE_CURVE ( 'NONE', #60571, #52360, #39513, .T. ) ;
#65746 = CARTESIAN_POINT ( 'NONE',  ( -5.655420232009311654, -8.406483450353382736, 195.0000000000000284 ) ) ;
#65747 = ORIENTED_EDGE ( 'NONE', *, *, #66858, .T. ) ;
#65748 = ORIENTED_EDGE ( 'NONE', *, *, #53036, .F. ) ;
#65749 = VECTOR ( 'NONE', #64447, 1000.000000000000000 ) ;
#65750 = CYLINDRICAL_SURFACE ( 'NONE', #62880, 0.1749999999999998224 ) ;
#65751 = FACE_OUTER_BOUND ( 'NONE', #68350, .T. ) ;
#65752 = VECTOR ( 'NONE', #55301, 1000.000000000000000 ) ;
#65753 = VERTEX_POINT ( 'NONE', #16927 ) ;
#65754 = DIRECTION ( 'NONE',  ( -1.000000000000000000, 0.000000000000000000, 0.000000000000000000 ) ) ;
#65755 = LINE ( 'NONE', #49500, #24436 ) ;
#65756 = DIRECTION ( 'NONE',  ( 0.000000000000000000, 1.000000000000000000, 0.000000000000000000 ) ) ;
#65757 = EDGE_LOOP ( 'NONE', ( #13437, #31822, #4864, #26267 ) ) ;
#65758 = VECTOR ( 'NONE', #20145, 1000.000000000000000 ) ;
#65759 = DIRECTION ( 'NONE',  ( 1.000000000000000000, 0.000000000000000000, 0.000000000000000000 ) ) ;
#65760 = DIRECTION ( 'NONE',  ( -0.000000000000000000, -0.000000000000000000, -1.000000000000000000 ) ) ;
#65761 = ORIENTED_EDGE ( 'NONE', *, *, #41744, .T. ) ;
#65763 = ORIENTED_EDGE ( 'NONE', *, *, #66481, .T. ) ;
#65762 = CARTESIAN_POINT ( 'NONE',  ( 5.257023737882819070, -5.257023737882825287, 54.00000000000000711 ) ) ;
#65765 = DIRECTION ( 'NONE',  ( -0.000000000000000000, 1.000000000000000000, -0.000000000000000000 ) ) ;
#65764 = AXIS2_PLACEMENT_3D ( 'NONE', #62113, #62829, #25352 ) ;
#65766 = CARTESIAN_POINT ( 'NONE',  ( -16.75000000000000000, -0.2038245569916330158, -21.77831216351300014 ) ) ;
#65767 = CARTESIAN_POINT ( 'NONE',  ( -28.00000000000000000, -15.50000000000000000, -14.50000000000000000 ) ) ;
#65768 = LINE ( 'NONE', #21268, #30125 ) ;
#65769 = DIRECTION ( 'NONE',  ( 0.000000000000000000, -1.000000000000000000, 0.000000000000000000 ) ) ;
#65770 = DIRECTION ( 'NONE',  ( -1.000000000000000000, 0.000000000000000000, 0.000000000000000000 ) ) ;
#65771 = ORIENTED_EDGE ( 'NONE', *, *, #2768, .T. ) ;
#65772 = FACE_OUTER_BOUND ( 'NONE', #61010, .T. ) ;
#65774 = VERTEX_POINT ( 'NONE', #672 ) ;
#65773 = DIRECTION ( 'NONE',  ( 0.7071067811865474617, 0.7071067811865474617, 0.000000000000000000 ) ) ;
#65775 = EDGE_CURVE ( 'NONE', #11613, #144, #22241, .T. ) ;
#65777 = VERTEX_POINT ( 'NONE', #33182 ) ;
#65776 = CARTESIAN_POINT ( 'NONE',  ( 8.250000000000005329, 0.000000000000000000, -21.50000000000000000 ) ) ;
#65778 = SURFACE_SIDE_STYLE ('',( #59093 ) ) ;
#65779 = CARTESIAN_POINT ( 'NONE',  ( -7.450000000000001954, -7.249999999999998224, -24.50000000000000000 ) ) ;
#65780 = EDGE_CURVE ( 'NONE', #19808, #51221, #48927, .T. ) ;
#65781 = ORIENTED_EDGE ( 'NONE', *, *, #49140, .F. ) ;
#65782 = CARTESIAN_POINT ( 'NONE',  ( -7.250000000000001776, -7.249999999999998224, -26.00000000000001066 ) ) ;
#65783 = EDGE_CURVE ( 'NONE', #42614, #61558, #29601, .T. ) ;
#65784 = CARTESIAN_POINT ( 'NONE',  ( 16.75000000000000000, -2.500000000000000000, -21.77831216351300014 ) ) ;
#65785 = AXIS2_PLACEMENT_3D ( 'NONE', #7945, #29521, #44725 ) ;
#65786 = EDGE_CURVE ( 'NONE', #47516, #53330, #2389, .T. ) ;
#65787 = ORIENTED_EDGE ( 'NONE', *, *, #9033, .T. ) ;
#65788 = CARTESIAN_POINT ( 'NONE',  ( -7.450000000000001954, -7.249999999999998224, -11.00000000000000000 ) ) ;
#65789 = CARTESIAN_POINT ( 'NONE',  ( 8.930623737882845248, 8.916576262117187568, 54.00000000000000711 ) ) ;
#65790 = DIRECTION ( 'NONE',  ( -1.836970198721029934E-16, 1.836970198721036344E-16, -1.000000000000000000 ) ) ;
#65791 = EDGE_CURVE ( 'NONE', #54299, #51332, #62468, .T. ) ;
#65792 = EDGE_CURVE ( 'NONE', #53157, #66031, #7684, .T. ) ;
#65793 = VECTOR ( 'NONE', #40539, 1000.000000000000000 ) ;
#65794 = LINE ( 'NONE', #7077, #45143 ) ;
#65795 = DIRECTION ( 'NONE',  ( 0.000000000000000000, 0.000000000000000000, 1.000000000000000000 ) ) ;
#65796 = EDGE_CURVE ( 'NONE', #18995, #26808, #41621, .T. ) ;
#65797 = ORIENTED_EDGE ( 'NONE', *, *, #60432, .F. ) ;
#65798 = CARTESIAN_POINT ( 'NONE',  ( -11.75000000000000000, -5.000000000000000000, 23.89194109070750116 ) ) ;
#65799 = ORIENTED_EDGE ( 'NONE', *, *, #45821, .F. ) ;
#65800 = ORIENTED_EDGE ( 'NONE', *, *, #8381, .F. ) ;
#65801 = PLANE ( 'NONE',  #34749 ) ;
#65802 = CARTESIAN_POINT ( 'NONE',  ( -4.609516549646713202, 3.593516549646603941, 455.0000000000000568 ) ) ;
#65803 = CYLINDRICAL_SURFACE ( 'NONE', #15208, 1.000000000000000000 ) ;
#65804 = DIRECTION ( 'NONE',  ( 0.000000000000000000, 1.000000000000000000, 0.000000000000000000 ) ) ;
#65805 = ORIENTED_EDGE ( 'NONE', *, *, #9969, .F. ) ;
#65806 = VERTEX_POINT ( 'NONE', #19687 ) ;
#65808 = VERTEX_POINT ( 'NONE', #51174 ) ;
#65807 = DIRECTION ( 'NONE',  ( 1.000000000000000000, 0.000000000000000000, 0.000000000000000000 ) ) ;
#65809 = ORIENTED_EDGE ( 'NONE', *, *, #24236, .T. ) ;
#65810 = CARTESIAN_POINT ( 'NONE',  ( 283.0000000000000568, -38.64999999999999858, -15.00000000000000000 ) ) ;
#65811 = CIRCLE ( 'NONE', #13820, 0.1749999999999998224 ) ;
#65812 = DIRECTION ( 'NONE',  ( 0.000000000000000000, 0.000000000000000000, 1.000000000000000000 ) ) ;
#65813 = CARTESIAN_POINT ( 'NONE',  ( 46.39999999999999858, 21.00000000000000000, 1.250000000000000000 ) ) ;
#65814 = VECTOR ( 'NONE', #28810, 1000.000000000000000 ) ;
#65815 = DIRECTION ( 'NONE',  ( -1.000000000000000000, 0.000000000000000000, 0.000000000000000000 ) ) ;
#65817 = DIRECTION ( 'NONE',  ( 0.000000000000000000, 0.000000000000000000, -1.000000000000000000 ) ) ;
#65816 = CARTESIAN_POINT ( 'NONE',  ( -7.450000000000001954, 7.250000000000000000, -22.00000000000000000 ) ) ;
#65818 = ORIENTED_EDGE ( 'NONE', *, *, #40759, .T. ) ;
#65820 = VERTEX_POINT ( 'NONE', #3791 ) ;
#65819 = DIRECTION ( 'NONE',  ( 0.000000000000000000, -1.000000000000000000, 0.000000000000000000 ) ) ;
#65821 = VERTEX_POINT ( 'NONE', #67793 ) ;
#65822 = ORIENTED_EDGE ( 'NONE', *, *, #25254, .F. ) ;
#65823 = LINE ( 'NONE', #98, #58202 ) ;
#65824 = VECTOR ( 'NONE', #53702, 1000.000000000000000 ) ;
#65825 = CARTESIAN_POINT ( 'NONE',  ( 9.404523737882758638, 1.466476262117154983, 54.00000000000000711 ) ) ;
#65826 = EDGE_CURVE ( 'NONE', #58012, #4367, #55669, .T. ) ;
#65827 = DIRECTION ( 'NONE',  ( -1.836970198721029934E-16, 1.836970198721036344E-16, -1.000000000000000000 ) ) ;
#65828 = MANIFOLD_SOLID_BREP ( 'LPattern1[6]', #10356 ) ;
#65829 = LINE ( 'NONE', #44590, #53444 ) ;
#65830 = ORIENTED_EDGE ( 'NONE', *, *, #55938, .T. ) ;
#65831 = EDGE_LOOP ( 'NONE', ( #8326, #9480, #15662, #18932 ) ) ;
#65832 = EDGE_CURVE ( 'NONE', #12339, #59528, #34898, .T. ) ;
#65833 = ADVANCED_FACE ( 'NONE', ( #35966 ), #61789, .T. ) ;
#65834 = CARTESIAN_POINT ( 'NONE',  ( 30.90000000000000213, -0.1999999999911795112, 8.826273045769999343E-12 ) ) ;
#65835 = CARTESIAN_POINT ( 'NONE',  ( -7.250000000000000888, 7.450000000000003730, -11.00000000000000000 ) ) ;
#65836 = AXIS2_PLACEMENT_3D ( 'NONE', #28736, #1877, #44999 ) ;
#65837 = EDGE_CURVE ( 'NONE', #33774, #8876, #57531, .T. ) ;
#65838 = VERTEX_POINT ( 'NONE', #62124 ) ;
#65839 = EDGE_LOOP ( 'NONE', ( #13899, #67674, #49120, #22995 ) ) ;
#65840 = DIRECTION ( 'NONE',  ( -1.000000000000000000, 0.000000000000000000, 0.000000000000000000 ) ) ;
#65841 = VECTOR ( 'NONE', #34322, 1000.000000000000000 ) ;
#65842 = CARTESIAN_POINT ( 'NONE',  ( 8.250000000000005329, 7.250000000000000888, -20.50000000000000000 ) ) ;
#65843 = VERTEX_POINT ( 'NONE', #13694 ) ;
#65844 = LINE ( 'NONE', #8173, #51677 ) ;
#65846 = EDGE_LOOP ( 'NONE', ( #45737, #7089, #3749, #35099, #62966, #67131, #58842, #67749 ) ) ;
#65845 = LINE ( 'NONE', #27678, #41927 ) ;
#65847 = VERTEX_POINT ( 'NONE', #46916 ) ;
#65848 = FACE_OUTER_BOUND ( 'NONE', #3554, .T. ) ;
#65849 = CARTESIAN_POINT ( 'NONE',  ( -11.99351654964674729, -7.826483450353316051, 195.0000000000000284 ) ) ;
#65850 = CARTESIAN_POINT ( 'NONE',  ( 11.50000000000000000, -11.50000000000100009, -19.50000000000103739 ) ) ;
#65851 = CYLINDRICAL_SURFACE ( 'NONE', #35724, 0.1999999999999996503 ) ;
#65852 = PLANE ( 'NONE',  #36138 ) ;
#65853 = ORIENTED_EDGE ( 'NONE', *, *, #12175, .F. ) ;
#65854 = LINE ( 'NONE', #65521, #29236 ) ;
#65855 = ORIENTED_EDGE ( 'NONE', *, *, #41455, .F. ) ;
#65856 = EDGE_CURVE ( 'NONE', #67811, #64214, #56825, .T. ) ;
#65857 = FACE_OUTER_BOUND ( 'NONE', #10900, .T. ) ;
#65858 = VECTOR ( 'NONE', #48520, 1000.000000000000000 ) ;
#65859 = DIRECTION ( 'NONE',  ( -0.000000000000000000, -0.000000000000000000, -1.000000000000000000 ) ) ;
#65860 = FACE_BOUND ( 'NONE', #9115, .T. ) ;
#65862 = CARTESIAN_POINT ( 'NONE',  ( 40.90000000000000568, -21.00000000000001421, -13.86939075806900945 ) ) ;
#65861 = AXIS2_PLACEMENT_3D ( 'NONE', #44919, #55874, #7428 ) ;
#65863 = CARTESIAN_POINT ( 'NONE',  ( 11.75000000000000000, -5.200000000000001066, 26.25000000000000000 ) ) ;
#65864 = CIRCLE ( 'NONE', #4910, 0.5249999999999990230 ) ;
#65865 = ORIENTED_EDGE ( 'NONE', *, *, #23293, .T. ) ;
#65866 = EDGE_LOOP ( 'NONE', ( #56415, #24767, #38665, #60786 ) ) ;
#65867 = CARTESIAN_POINT ( 'NONE',  ( 30.00000000000000000, -17.14999999999999858, -27.00000000000000000 ) ) ;
#65868 = AXIS2_PLACEMENT_3D ( 'NONE', #49006, #22132, #65279 ) ;
#65869 = EDGE_CURVE ( 'NONE', #29168, #47564, #31969, .T. ) ;
#65870 = FACE_OUTER_BOUND ( 'NONE', #3568, .T. ) ;
#65871 = EDGE_CURVE ( 'NONE', #8868, #2504, #40912, .T. ) ;
#65872 = ORIENTED_EDGE ( 'NONE', *, *, #57550, .T. ) ;
#65873 = CARTESIAN_POINT ( 'NONE',  ( 27.90000000000000213, -0.000000000000000000, -20.80000000000000071 ) ) ;
#65874 = ORIENTED_EDGE ( 'NONE', *, *, #32693, .F. ) ;
#65875 = ORIENTED_EDGE ( 'NONE', *, *, #40865, .F. ) ;
#65876 = DIRECTION ( 'NONE',  ( 0.000000000000000000, 1.000000000000000000, -0.000000000000000000 ) ) ;
#65877 = CARTESIAN_POINT ( 'NONE',  ( 41.09999999999999432, -14.06939075806900163, 20.80000000000000426 ) ) ;
#65878 = ORIENTED_EDGE ( 'NONE', *, *, #45588, .F. ) ;
#65879 = CARTESIAN_POINT ( 'NONE',  ( 9.804883450353408136, 10.19191654964661531, 195.0000000000000284 ) ) ;
#65880 = AXIS2_PLACEMENT_3D ( 'NONE', #35609, #62849, #46571 ) ;
#65881 = CARTESIAN_POINT ( 'NONE',  ( 29.50000000000000355, -11.50000000000100009, -19.50000000000103739 ) ) ;
#65882 = DIRECTION ( 'NONE',  ( -1.000000000000000000, 0.000000000000000000, 0.000000000000000000 ) ) ;
#65883 = ORIENTED_EDGE ( 'NONE', *, *, #65775, .F. ) ;
#65885 = ORIENTED_EDGE ( 'NONE', *, *, #63584, .F. ) ;
#65884 = CARTESIAN_POINT ( 'NONE',  ( 0.000000000000000000, -8.249999999999998224, -17.00000000000000000 ) ) ;
#65886 = EDGE_CURVE ( 'NONE', #4021, #24174, #53298, .T. ) ;
#65887 = CARTESIAN_POINT ( 'NONE',  ( 283.0000000000000568, -23.65000000000000568, -12.40000000000000213 ) ) ;
#65888 = CARTESIAN_POINT ( 'NONE',  ( -7.250000000000000000, -7.449999999999998401, -22.50000000000000000 ) ) ;
#65889 = FACE_OUTER_BOUND ( 'NONE', #4966, .T. ) ;
#65890 = ORIENTED_EDGE ( 'NONE', *, *, #68349, .T. ) ;
#65891 = DIRECTION ( 'NONE',  ( -0.6414496315691619044, 0.7671651518152962090, 0.000000000000000000 ) ) ;
#65892 = DIRECTION ( 'NONE',  ( 0.000000000000000000, 1.000000000000000000, 0.000000000000000000 ) ) ;
#65893 = ORIENTED_EDGE ( 'NONE', *, *, #55021, .F. ) ;
#65894 = ORIENTED_EDGE ( 'NONE', *, *, #13623, .F. ) ;
#65895 = ORIENTED_EDGE ( 'NONE', *, *, #46515, .T. ) ;
#65896 = DIRECTION ( 'NONE',  ( 0.000000000000000000, 0.000000000000000000, 1.000000000000000000 ) ) ;
#65897 = CARTESIAN_POINT ( 'NONE',  ( -2.893516549646681035, 10.08346604330774632, 195.0000000000000284 ) ) ;
#65898 = DIRECTION ( 'NONE',  ( 0.000000000000000000, 0.6801302850037830305, 0.7330912599538155217 ) ) ;
#65899 = CIRCLE ( 'NONE', #28598, 24.99999999998789946 ) ;
#65900 = VECTOR ( 'NONE', #6926, 1000.000000000000000 ) ;
#65901 = ORIENTED_EDGE ( 'NONE', *, *, #54207, .T. ) ;
#65902 = ORIENTED_EDGE ( 'NONE', *, *, #23833, .T. ) ;
#65903 = EDGE_LOOP ( 'NONE', ( #37735, #36704, #28767, #25156 ) ) ;
#65904 = EDGE_CURVE ( 'NONE', #68595, #8070, #15800, .T. ) ;
#65905 = DIRECTION ( 'NONE',  ( -1.000000000000000000, 0.000000000000000000, 0.000000000000000000 ) ) ;
#65906 = ORIENTED_EDGE ( 'NONE', *, *, #6019, .F. ) ;
#65907 = VECTOR ( 'NONE', #45348, 1000.000000000000000 ) ;
#65908 = AXIS2_PLACEMENT_3D ( 'NONE', #22808, #45404, #33757 ) ;
#65909 = ORIENTED_EDGE ( 'NONE', *, *, #48091, .T. ) ;
#65910 = EDGE_CURVE ( 'NONE', #14663, #29539, #66966, .T. ) ;
#65911 = ORIENTED_EDGE ( 'NONE', *, *, #60978, .F. ) ;
#65912 = ORIENTED_EDGE ( 'NONE', *, *, #49100, .T. ) ;
#65913 = DIRECTION ( 'NONE',  ( 0.000000000000000000, 0.000000000000000000, 1.000000000000000000 ) ) ;
#65914 = AXIS2_PLACEMENT_3D ( 'NONE', #60155, #42858, #43553 ) ;
#65915 = AXIS2_PLACEMENT_3D ( 'NONE', #3928, #14887, #30796 ) ;
#65917 = ORIENTED_EDGE ( 'NONE', *, *, #42629, .F. ) ;
#65916 = LINE ( 'NONE', #62001, #63899 ) ;
#65918 = DIRECTION ( 'NONE',  ( 0.000000000000000000, -1.000000000000000000, 0.000000000000000000 ) ) ;
#65919 = DIRECTION ( 'NONE',  ( 0.000000000000000000, 0.000000000000000000, -1.000000000000000000 ) ) ;
#65920 = CARTESIAN_POINT ( 'NONE',  ( 8.249999999999996447, -7.848062532927998269, -5.000000000000000000 ) ) ;
#65921 = ORIENTED_EDGE ( 'NONE', *, *, #11983, .F. ) ;
#65922 = DIRECTION ( 'NONE',  ( 1.261617073437657735E-14, 1.000000000000000000, 0.000000000000000000 ) ) ;
#65923 = DIRECTION ( 'NONE',  ( 1.000000000000000000, -5.981805089575196197E-17, 0.000000000000000000 ) ) ;
#65924 = DIRECTION ( 'NONE',  ( -1.000000000000000000, -2.135044278125301343E-15, -7.844025423732065664E-31 ) ) ;
#65925 = EDGE_CURVE ( 'NONE', #65138, #65565, #26308, .T. ) ;
#65926 = ORIENTED_EDGE ( 'NONE', *, *, #42396, .T. ) ;
#65927 = PLANE ( 'NONE',  #5511 ) ;
#65928 = FACE_OUTER_BOUND ( 'NONE', #68674, .T. ) ;
#65929 = LINE ( 'NONE', #33425, #69533 ) ;
#65930 = MANIFOLD_SOLID_BREP ( 'Cut-Extrude5', #35150 ) ;
#65931 = ORIENTED_EDGE ( 'NONE', *, *, #36789, .T. ) ;
#65932 = DIRECTION ( 'NONE',  ( -1.000000000000000000, 0.000000000000000000, 0.000000000000000000 ) ) ;
#65933 = LINE ( 'NONE', #17857, #42072 ) ;
#65934 = LINE ( 'NONE', #50721, #20098 ) ;
#65935 = AXIS2_PLACEMENT_3D ( 'NONE', #59712, #54419, #27533 ) ;
#65936 = CARTESIAN_POINT ( 'NONE',  ( 39.00000000000000000, -21.00000000000000000, -16.96999999999999886 ) ) ;
#65937 = CYLINDRICAL_SURFACE ( 'NONE', #9898, 3.999999999999993339 ) ;
#65938 = DIRECTION ( 'NONE',  ( 0.000000000000000000, 0.000000000000000000, -1.000000000000000000 ) ) ;
#65939 = CARTESIAN_POINT ( 'NONE',  ( 2.369523737882817116, 9.547976262117204627, 54.00000000000000711 ) ) ;
#65940 = ADVANCED_FACE ( 'NONE', ( #48330 ), #15108, .T. ) ;
#65941 = CIRCLE ( 'NONE', #44490, 0.1749999999999998224 ) ;
#65942 = CIRCLE ( 'NONE', #59156, 0.1749999999999998224 ) ;
#65943 = EDGE_CURVE ( 'NONE', #46756, #96, #53640, .T. ) ;
#65944 = ORIENTED_EDGE ( 'NONE', *, *, #44100, .T. ) ;
#65945 = DIRECTION ( 'NONE',  ( -1.000000000000000000, 0.000000000000000000, 0.000000000000000000 ) ) ;
#65946 = EDGE_CURVE ( 'NONE', #20828, #42371, #4159, .T. ) ;
#65947 = DIRECTION ( 'NONE',  ( -0.000000000000000000, -0.000000000000000000, -1.000000000000000000 ) ) ;
#65948 = CARTESIAN_POINT ( 'NONE',  ( 7.250000000000005329, 7.250000000000000888, -16.00000000000000000 ) ) ;
#65949 = DIRECTION ( 'NONE',  ( 0.000000000000000000, 0.000000000000000000, 1.000000000000000000 ) ) ;
#65950 = VECTOR ( 'NONE', #873, 1000.000000000000000 ) ;
#65951 = ORIENTED_EDGE ( 'NONE', *, *, #17534, .T. ) ;
#65952 = VECTOR ( 'NONE', #44283, 1000.000000000000000 ) ;
#65953 = LINE ( 'NONE', #18213, #60341 ) ;
#65954 = LINE ( 'NONE', #17523, #14723 ) ;
#65955 = ADVANCED_FACE ( 'NONE', ( #48675, #9814 ), #57879, .F. ) ;
#65956 = CARTESIAN_POINT ( 'NONE',  ( 5.793274621760810206, 4.141586236041043811, 26.00000000000000711 ) ) ;
#65957 = EDGE_CURVE ( 'NONE', #12566, #68940, #54581, .T. ) ;
#65958 = EDGE_CURVE ( 'NONE', #45256, #54885, #68851, .T. ) ;
#65959 = AXIS2_PLACEMENT_3D ( 'NONE', #36792, #3911, #14151 ) ;
#65960 = LINE ( 'NONE', #11179, #20694 ) ;
#65961 = ADVANCED_FACE ( 'NONE', ( #32422 ), #69194, .T. ) ;
#65962 = DIRECTION ( 'NONE',  ( -1.836970198721029934E-16, 1.836970198721036344E-16, -1.000000000000000000 ) ) ;
#65963 = VERTEX_POINT ( 'NONE', #31014 ) ;
#65964 = EDGE_CURVE ( 'NONE', #39751, #58695, #52594, .T. ) ;
#65965 = AXIS2_PLACEMENT_3D ( 'NONE', #8354, #55761, #51149 ) ;
#65966 = DIRECTION ( 'NONE',  ( -8.903847840905249551E-15, -1.000000000000000000, -1.836970198721027222E-16 ) ) ;
#65967 = DIRECTION ( 'NONE',  ( 1.836970198721029934E-16, 1.836970198721010706E-16, -1.000000000000000000 ) ) ;
#65968 = VERTEX_POINT ( 'NONE', #16499 ) ;
#65969 = VECTOR ( 'NONE', #8144, 1000.000000000000000 ) ;
#65970 = DIRECTION ( 'NONE',  ( 0.000000000000000000, 1.000000000000000000, 0.000000000000000000 ) ) ;
#65971 = VERTEX_POINT ( 'NONE', #39435 ) ;
#65972 = CARTESIAN_POINT ( 'NONE',  ( 39.00000000000000000, -5.250000000000000000, 0.000000000000000000 ) ) ;
#65973 = VERTEX_POINT ( 'NONE', #22502 ) ;
#65974 = EDGE_LOOP ( 'NONE', ( #21387, #56827, #52586, #32052, #33479, #43464 ) ) ;
#65975 = DIRECTION ( 'NONE',  ( 9.912705577010336396E-15, 1.000000000000000000, 0.000000000000000000 ) ) ;
#65976 = CARTESIAN_POINT ( 'NONE',  ( 3.677663764522614454, -6.364920264886879231, 54.00000000000000711 ) ) ;
#65977 = LINE ( 'NONE', #55729, #6736 ) ;
#65978 = DIRECTION ( 'NONE',  ( -1.000000000000000000, 0.000000000000000000, 0.000000000000000000 ) ) ;
#65979 = VERTEX_POINT ( 'NONE', #34122 ) ;
#65980 = VECTOR ( 'NONE', #10250, 1000.000000000000000 ) ;
#65981 = EDGE_LOOP ( 'NONE', ( #49479, #18868, #44333, #11785, #49738, #55571 ) ) ;
#65982 = DIRECTION ( 'NONE',  ( 0.000000000000000000, 0.000000000000000000, -1.000000000000000000 ) ) ;
#65983 = CARTESIAN_POINT ( 'NONE',  ( -11.77351654964670935, 4.393516549646602876, 195.0000000000000284 ) ) ;
#65984 = ORIENTED_EDGE ( 'NONE', *, *, #16818, .T. ) ;
#65985 = VECTOR ( 'NONE', #51536, 1000.000000000000000 ) ;
#65986 = ORIENTED_EDGE ( 'NONE', *, *, #68110, .F. ) ;
#65988 = ORIENTED_EDGE ( 'NONE', *, *, #38116, .F. ) ;
#65987 = CONTEXT_DEPENDENT_SHAPE_REPRESENTATION ( #58526, #22227 ) ;
#65989 = DIRECTION ( 'NONE',  ( -0.000000000000000000, 1.000000000000000000, -0.000000000000000000 ) ) ;
#65990 = LINE ( 'NONE', #60698, #68335 ) ;
#65992 = ORIENTED_EDGE ( 'NONE', *, *, #29900, .F. ) ;
#65991 = CARTESIAN_POINT ( 'NONE',  ( 28.90000000000000213, 0.000000000000000000, 0.000000000000000000 ) ) ;
#65993 = CARTESIAN_POINT ( 'NONE',  ( 6.500000000000002665, 6.500000000000000888, 0.000000000000000000 ) ) ;
#65994 = CIRCLE ( 'NONE', #35502, 0.1999999999999996503 ) ;
#65995 = LINE ( 'NONE', #6617, #18173 ) ;
#65996 = ORIENTED_EDGE ( 'NONE', *, *, #31973, .F. ) ;
#65997 = ORIENTED_EDGE ( 'NONE', *, *, #43462, .F. ) ;
#65998 = ORIENTED_EDGE ( 'NONE', *, *, #26974, .T. ) ;
#65999 = VECTOR ( 'NONE', #52335, 1000.000000000000114 ) ;
#66000 = EDGE_CURVE ( 'NONE', #56941, #41772, #1274, .T. ) ;
#66001 = AXIS2_PLACEMENT_3D ( 'NONE', #69169, #20724, #46892 ) ;
#66002 = FACE_OUTER_BOUND ( 'NONE', #18677, .T. ) ;
#66003 = CARTESIAN_POINT ( 'NONE',  ( 7.250000000000005329, 7.250000000000000888, -19.00000000000000000 ) ) ;
#66004 = EDGE_CURVE ( 'NONE', #44820, #46180, #65960, .T. ) ;
#66005 = DIRECTION ( 'NONE',  ( 1.000000000000000000, 0.000000000000000000, 0.000000000000000000 ) ) ;
#66006 =( GEOMETRIC_REPRESENTATION_CONTEXT ( 3 ) GLOBAL_UNCERTAINTY_ASSIGNED_CONTEXT ( ( #38032 ) ) GLOBAL_UNIT_ASSIGNED_CONTEXT ( ( #51157, #68835, #2718 ) ) REPRESENTATION_CONTEXT ( 'NONE', 'WORKASPACE' ) );
#66007 = SURFACE_STYLE_USAGE ( .BOTH. , #12255 ) ;
#66008 = CYLINDRICAL_SURFACE ( 'NONE', #56156, 5.000000000000000000 ) ;
#66009 = CIRCLE ( 'NONE', #35530, 1.000000000000000000 ) ;
#66010 = EDGE_CURVE ( 'NONE', #14045, #44953, #60209, .T. ) ;
#66012 = EDGE_LOOP ( 'NONE', ( #45878, #26829, #199, #12756 ) ) ;
#66011 = DIRECTION ( 'NONE',  ( -1.000000000000000000, 0.000000000000000000, 0.000000000000000000 ) ) ;
#66013 = ORIENTED_EDGE ( 'NONE', *, *, #49645, .F. ) ;
#66014 = AXIS2_PLACEMENT_3D ( 'NONE', #1456, #23024, #66163 ) ;
#66015 = CARTESIAN_POINT ( 'NONE',  ( -7.250000000000001776, -7.249999999999998224, -26.00000000000001066 ) ) ;
#66016 = DIRECTION ( 'NONE',  ( -0.000000000000000000, 3.673940397442059868E-16, -1.000000000000000000 ) ) ;
#66017 = DIRECTION ( 'NONE',  ( 1.000000000000000000, -1.356437060717832013E-15, -1.836970198721032646E-16 ) ) ;
#66018 = ADVANCED_FACE ( 'NONE', ( #16843 ), #22153, .T. ) ;
#66019 = DIRECTION ( 'NONE',  ( 1.000000000000000000, 0.000000000000000000, 0.000000000000000000 ) ) ;
#66020 = DIRECTION ( 'NONE',  ( -1.000000000000000000, 0.000000000000000000, 0.000000000000000000 ) ) ;
#66021 = ORIENTED_EDGE ( 'NONE', *, *, #62422, .T. ) ;
#66022 = DIRECTION ( 'NONE',  ( 0.000000000000000000, 0.000000000000000000, -1.000000000000000000 ) ) ;
#66023 = CARTESIAN_POINT ( 'NONE',  ( 10.92648345035335922, 2.693516549646528091, 455.0000000000000568 ) ) ;
#66024 =( NAMED_UNIT ( * ) PLANE_ANGLE_UNIT ( ) SI_UNIT ( $, .RADIAN. ) );
#66025 = LINE ( 'NONE', #49445, #53711 ) ;
#66026 = EDGE_CURVE ( 'NONE', #59384, #1121, #38748, .T. ) ;
#66027 = LINE ( 'NONE', #12272, #29161 ) ;
#66028 = AXIS2_PLACEMENT_3D ( 'NONE', #47259, #58574, #36638 ) ;
#66029 = CARTESIAN_POINT ( 'NONE',  ( 33.89999999999999858, -0.2000000000089119934, 8.909539772616881237E-12 ) ) ;
#66030 = CARTESIAN_POINT ( 'NONE',  ( 105.8309041053263257, 61.65740854044500452, 2.000000000000000000 ) ) ;
#66031 = VERTEX_POINT ( 'NONE', #54680 ) ;
#66032 = CYLINDRICAL_SURFACE ( 'NONE', #2697, 0.1999999999999987899 ) ;
#66033 = FACE_OUTER_BOUND ( 'NONE', #51318, .T. ) ;
#66034 = AXIS2_PLACEMENT_3D ( 'NONE', #8658, #51798, #30929 ) ;
#66035 = ORIENTED_EDGE ( 'NONE', *, *, #31068, .T. ) ;
#66036 = PLANE ( 'NONE',  #47000 ) ;
#66037 = DIRECTION ( 'NONE',  ( -1.000000000000000000, 0.000000000000000000, -0.000000000000000000 ) ) ;
#66038 = PLANE ( 'NONE',  #3931 ) ;
#66039 = LINE ( 'NONE', #17609, #38759 ) ;
#66040 = EDGE_CURVE ( 'NONE', #31960, #17879, #52355, .T. ) ;
#66041 = CARTESIAN_POINT ( 'NONE',  ( 11.50000000000000000, -11.50000000000100009, 15.00000000000084910 ) ) ;
#66042 = EDGE_CURVE ( 'NONE', #66404, #12559, #59968, .T. ) ;
#66043 = CARTESIAN_POINT ( 'NONE',  ( 29.89999999999999858, -14.06939075806902117, -20.80000000000000426 ) ) ;
#66044 = CIRCLE ( 'NONE', #26549, 2.250000000000001776 ) ;
#66045 = ORIENTED_EDGE ( 'NONE', *, *, #3354, .F. ) ;
#66046 = AXIS2_PLACEMENT_3D ( 'NONE', #47046, #13108, #8858 ) ;
#66047 = DIRECTION ( 'NONE',  ( -1.000000000000000000, 0.000000000000000000, 0.000000000000000000 ) ) ;
#66048 = EDGE_LOOP ( 'NONE', ( #68018, #37378, #36316, #6800 ) ) ;
#66049 = CARTESIAN_POINT ( 'NONE',  ( 2.420780051175148273, -8.711985858128667104, 26.00000000000000000 ) ) ;
#66050 = CIRCLE ( 'NONE', #35564, 0.5000000000001362244 ) ;
#66051 = MECHANICAL_DESIGN_GEOMETRIC_PRESENTATION_REPRESENTATION (  '', ( #57026 ), #615 ) ;
#66052 =( LENGTH_UNIT ( ) NAMED_UNIT ( * ) SI_UNIT ( .MILLI., .METRE. ) );
#66053 = VECTOR ( 'NONE', #57613, 1000.000000000000000 ) ;
#66054 = DIRECTION ( 'NONE',  ( 0.4998444328988824181, 0.000000000000000000, -0.8661152018640445593 ) ) ;
#66055 = ORIENTED_EDGE ( 'NONE', *, *, #33769, .T. ) ;
#66056 = VERTEX_POINT ( 'NONE', #17179 ) ;
#66057 = CARTESIAN_POINT ( 'NONE',  ( -7.252248008019455128, 5.380658396643134722, 455.0000000000000568 ) ) ;
#66058 = VERTEX_POINT ( 'NONE', #59634 ) ;
#66059 = VERTEX_POINT ( 'NONE', #49026 ) ;
#66060 = LINE ( 'NONE', #22262, #64299 ) ;
#66061 = DIRECTION ( 'NONE',  ( 1.000000000000000000, -1.952517519553884087E-14, 1.836970198720994435E-16 ) ) ;
#66062 = VECTOR ( 'NONE', #52858, 1000.000000000000000 ) ;
#66063 = B_SPLINE_CURVE_WITH_KNOTS ( 'NONE', 3,
 ( #9621, #30828, #10315, #42485, #64082, #52404 ),
 .UNSPECIFIED., .F., .F.,
 ( 4, 2, 4 ),
 ( 1.820537833122031213, 2.555393473688635453, 3.290249114255239693 ),
 .UNSPECIFIED. ) ;
#66064 = DIRECTION ( 'NONE',  ( -0.000000000000000000, 1.000000000000000000, 3.673940397442059868E-16 ) ) ;
#66065 = VERTEX_POINT ( 'NONE', #45083 ) ;
#66066 = VECTOR ( 'NONE', #67253, 1000.000000000000000 ) ;
#66067 = DIRECTION ( 'NONE',  ( 1.000000000000000000, -0.000000000000000000, 0.000000000000000000 ) ) ;
#66069 = CARTESIAN_POINT ( 'NONE',  ( -6.486996718459903555, -2.632023737882784431, 54.00000000000000711 ) ) ;
#66068 = DIRECTION ( 'NONE',  ( 0.000000000000000000, 0.7046037717862339012, -0.7096009616570518874 ) ) ;
#66070 = ORIENTED_EDGE ( 'NONE', *, *, #51138, .T. ) ;
#66072 = ORIENTED_EDGE ( 'NONE', *, *, #56999, .F. ) ;
#66071 = CARTESIAN_POINT ( 'NONE',  ( 69.92576880110416937, 10.00000000000000000, 335.4830310981152479 ) ) ;
#66073 = VERTEX_POINT ( 'NONE', #6911 ) ;
#66074 = EDGE_CURVE ( 'NONE', #26429, #27857, #50403, .T. ) ;
#66075 = CARTESIAN_POINT ( 'NONE',  ( 220.0878357351774355, 38.49351654964638669, 318.8237994620729410 ) ) ;
#66076 = DIRECTION ( 'NONE',  ( 0.000000000000000000, 0.000000000000000000, 1.000000000000000000 ) ) ;
#66077 = ADVANCED_FACE ( 'NONE', ( #60308 ), #49708, .F. ) ;
#66078 = CARTESIAN_POINT ( 'NONE',  ( -9.390476262117259054, 1.466476262117183182, 54.00000000000000711 ) ) ;
#66079 = VERTEX_POINT ( 'NONE', #39097 ) ;
#66080 = ORIENTED_EDGE ( 'NONE', *, *, #9253, .T. ) ;
#66081 = EDGE_CURVE ( 'NONE', #59339, #45669, #11865, .T. ) ;
#66082 = DIRECTION ( 'NONE',  ( 0.000000000000000000, 1.000000000000000000, 0.000000000000000000 ) ) ;
#66083 = EDGE_CURVE ( 'NONE', #14185, #48034, #24117, .T. ) ;
#66084 = DIRECTION ( 'NONE',  ( -1.000000000000000000, 0.000000000000000000, 0.000000000000000000 ) ) ;
#66085 = AXIS2_PLACEMENT_3D ( 'NONE', #33534, #60746, #42146 ) ;
#66086 = ORIENTED_EDGE ( 'NONE', *, *, #44047, .F. ) ;
#66087 = LINE ( 'NONE', #17662, #43266 ) ;
#66088 = DIRECTION ( 'NONE',  ( 0.000000000000000000, 0.7840980155806945850, 0.6206370130458033207 ) ) ;
#66089 = VECTOR ( 'NONE', #42754, 1000.000000000000000 ) ;
#66090 = EDGE_CURVE ( 'NONE', #47619, #59376, #27453, .T. ) ;
#66091 = FACE_BOUND ( 'NONE', #32542, .T. ) ;
#66092 = ORIENTED_EDGE ( 'NONE', *, *, #2579, .T. ) ;
#66093 = VECTOR ( 'NONE', #41924, 1000.000000000000000 ) ;
#66094 = VECTOR ( 'NONE', #32492, 1000.000000000000000 ) ;
#66095 = VECTOR ( 'NONE', #1309, 1000.000000000000000 ) ;
#66096 = LINE ( 'NONE', #45217, #58406 ) ;
#66097 = DIRECTION ( 'NONE',  ( -0.7071067811865398012, 0.7071067811865552333, 2.597868168706484541E-16 ) ) ;
#66098 = EDGE_CURVE ( 'NONE', #64032, #64371, #41027, .T. ) ;
#66100 = ORIENTED_EDGE ( 'NONE', *, *, #34107, .T. ) ;
#66099 = DIRECTION ( 'NONE',  ( -1.000000000000000000, 0.000000000000000000, 0.000000000000000000 ) ) ;
#66102 = EDGE_LOOP ( 'NONE', ( #59338, #35060, #30277, #14983 ) ) ;
#66101 = CARTESIAN_POINT ( 'NONE',  ( 49.00000000000000000, -0.7500000000000000000, 3.929058411375430104 ) ) ;
#66103 = EDGE_CURVE ( 'NONE', #35248, #35896, #28141, .T. ) ;
#66104 = DIRECTION ( 'NONE',  ( 1.000000000000000000, 0.000000000000000000, 0.000000000000000000 ) ) ;
#66105 = VECTOR ( 'NONE', #36686, 1000.000000000000000 ) ;
#66106 = CIRCLE ( 'NONE', #62678, 5.000000000000000000 ) ;
#66107 = CARTESIAN_POINT ( 'NONE',  ( 8.930623737882818602, -9.703773737882825046, 54.00000000000000711 ) ) ;
#66108 = DIRECTION ( 'NONE',  ( -0.000000000000000000, 0.000000000000000000, 1.000000000000000000 ) ) ;
#66109 = DIRECTION ( 'NONE',  ( 0.000000000000000000, 0.000000000000000000, 1.000000000000000000 ) ) ;
#66110 = EDGE_CURVE ( 'NONE', #13089, #16097, #17353, .T. ) ;
#66111 = EDGE_CURVE ( 'NONE', #57822, #50308, #45556, .T. ) ;
#66112 = CARTESIAN_POINT ( 'NONE',  ( -3.650476262117335668, -10.50702373788282173, 54.00000000000000711 ) ) ;
#66113 = AXIS2_PLACEMENT_3D ( 'NONE', #26113, #68890, #52991 ) ;
#66114 = FACE_OUTER_BOUND ( 'NONE', #19442, .T. ) ;
#66115 = EDGE_LOOP ( 'NONE', ( #44909, #14224, #60609, #56522 ) ) ;
#66116 = CYLINDRICAL_SURFACE ( 'NONE', #41363, 0.5000000000023475666 ) ;
#66117 = CARTESIAN_POINT ( 'NONE',  ( 7.250000000000005329, -7.249999999999998224, -26.00000000000001066 ) ) ;
#66118 = ADVANCED_FACE ( 'NONE', ( #38082 ), #61339, .F. ) ;
#66119 = FACE_OUTER_BOUND ( 'NONE', #11012, .T. ) ;
#66121 = VERTEX_POINT ( 'NONE', #46139 ) ;
#66120 = LINE ( 'NONE', #27604, #34384 ) ;
#66122 = VECTOR ( 'NONE', #47872, 1000.000000000000000 ) ;
#66123 = CARTESIAN_POINT ( 'NONE',  ( 283.0000000000000568, -31.30000000000000071, -12.69999999999999929 ) ) ;
#66124 = CIRCLE ( 'NONE', #9670, 1.000000000000001776 ) ;
#66125 = DIRECTION ( 'NONE',  ( 0.000000000000000000, 0.000000000000000000, 1.000000000000000000 ) ) ;
#66126 = ORIENTED_EDGE ( 'NONE', *, *, #7950, .T. ) ;
#66127 = DIRECTION ( 'NONE',  ( -0.8660254037844528074, -0.4999999999999755751, 6.723777587269133212E-17 ) ) ;
#66128 = DIRECTION ( 'NONE',  ( -1.000000000000000000, 0.000000000000000000, 0.000000000000000000 ) ) ;
#66129 = VERTEX_POINT ( 'NONE', #56397 ) ;
#66130 = CARTESIAN_POINT ( 'NONE',  ( -7.250000000000000888, 7.250000000000001776, -8.500000000000000000 ) ) ;
#66131 = CARTESIAN_POINT ( 'NONE',  ( -7.250000000000000888, 7.450000000000003730, -23.00000000000000000 ) ) ;
#66132 = FACE_BOUND ( 'NONE', #35847, .T. ) ;
#66133 = APPLICATION_CONTEXT ( 'automotive_design' ) ;
#66134 = ADVANCED_FACE ( 'NONE', ( #35890 ), #62392, .F. ) ;
#66135 = LINE ( 'NONE', #6733, #64366 ) ;
#66136 = EDGE_CURVE ( 'NONE', #6447, #13636, #46685, .T. ) ;
#66137 = CARTESIAN_POINT ( 'NONE',  ( 283.0000000000000568, -42.50000000000000000, -15.10000000000000142 ) ) ;
#66138 = ORIENTED_EDGE ( 'NONE', *, *, #53762, .T. ) ;
#66139 = DIRECTION ( 'NONE',  ( 1.000000000000000000, 0.000000000000000000, 0.000000000000000000 ) ) ;
#66140 = ORIENTED_EDGE ( 'NONE', *, *, #59125, .T. ) ;
#66141 = VECTOR ( 'NONE', #65271, 1000.000000000000000 ) ;
#66142 = ORIENTED_EDGE ( 'NONE', *, *, #67296, .T. ) ;
#66143 = FACE_OUTER_BOUND ( 'NONE', #14985, .T. ) ;
#66144 = DIRECTION ( 'NONE',  ( 1.836970198721029934E-16, 1.836970198721010706E-16, -1.000000000000000000 ) ) ;
#66145 = VECTOR ( 'NONE', #43366, 1000.000000000000000 ) ;
#66146 = DIRECTION ( 'NONE',  ( 1.000000000000000000, -1.115702204244422993E-14, -1.836970198721050395E-16 ) ) ;
#66147 = VECTOR ( 'NONE', #11863, 1000.000000000000000 ) ;
#66148 = FACE_OUTER_BOUND ( 'NONE', #18515, .T. ) ;
#66149 = VERTEX_POINT ( 'NONE', #34823 ) ;
#66150 = ORIENTED_EDGE ( 'NONE', *, *, #17196, .T. ) ;
#66151 = DIRECTION ( 'NONE',  ( 0.000000000000000000, 0.000000000000000000, 1.000000000000000000 ) ) ;
#66152 = VERTEX_POINT ( 'NONE', #24586 ) ;
#66153 = AXIS2_PLACEMENT_3D ( 'NONE', #57756, #3669, #68370 ) ;
#66154 = AXIS2_PLACEMENT_3D ( 'NONE', #28806, #50382, #20220 ) ;
#66155 = AXIS2_PLACEMENT_3D ( 'NONE', #52018, #36814, #30092 ) ;
#66156 = CARTESIAN_POINT ( 'NONE',  ( 7.250000000000005329, 8.250000000000001776, -19.50000000000000000 ) ) ;
#66157 = CARTESIAN_POINT ( 'NONE',  ( -9.689726262117309474, -8.580623737882753232, 26.00000000000000000 ) ) ;
#66158 = CARTESIAN_POINT ( 'NONE',  ( 9.737023737882763541, 2.530476262117156594, 26.00000000000000711 ) ) ;
#66159 = LINE ( 'NONE', #64788, #16465 ) ;
#66160 = VECTOR ( 'NONE', #60272, 1000.000000000000000 ) ;
#66161 = CIRCLE ( 'NONE', #27813, 0.1749999999999998224 ) ;
#66162 = VECTOR ( 'NONE', #19460, 1000.000000000000000 ) ;
#66164 = PLANE ( 'NONE',  #33460 ) ;
#66163 = DIRECTION ( 'NONE',  ( -1.000000000000000000, 0.000000000000000000, 0.000000000000000000 ) ) ;
#66165 = ORIENTED_EDGE ( 'NONE', *, *, #33770, .F. ) ;
#66167 = ORIENTED_EDGE ( 'NONE', *, *, #30133, .F. ) ;
#66166 = PLANE ( 'NONE',  #33002 ) ;
#66168 = ORIENTED_EDGE ( 'NONE', *, *, #19385, .T. ) ;
#66169 = ORIENTED_EDGE ( 'NONE', *, *, #38186, .T. ) ;
#66170 = VECTOR ( 'NONE', #14710, 1000.000000000000000 ) ;
#66171 = DIRECTION ( 'NONE',  ( 0.000000000000000000, 1.000000000000000000, -1.500535806722257514E-12 ) ) ;
#66172 = EDGE_CURVE ( 'NONE', #58217, #7028, #34463, .T. ) ;
#66173 = DIRECTION ( 'NONE',  ( 1.000000000000000000, 0.000000000000000000, 0.000000000000000000 ) ) ;
#66174 = MANIFOLD_SOLID_BREP ( 'Cut-Extrude1[5]', #40820 ) ;
#66175 = CARTESIAN_POINT ( 'NONE',  ( 3.006483450353359732, 7.415254214038262681, 195.0000000000000284 ) ) ;
#66176 = ORIENTED_EDGE ( 'NONE', *, *, #45456, .T. ) ;
#66177 = ORIENTED_EDGE ( 'NONE', *, *, #45773, .F. ) ;
#66178 = AXIS2_PLACEMENT_3D ( 'NONE', #10913, #48397, #63977 ) ;
#66179 = EDGE_CURVE ( 'NONE', #35695, #45355, #3019, .T. ) ;
#66180 = FACE_OUTER_BOUND ( 'NONE', #58747, .T. ) ;
#66181 = EDGE_CURVE ( 'NONE', #17331, #34291, #44391, .T. ) ;
#66182 = LINE ( 'NONE', #1472, #40147 ) ;
#66183 = EDGE_CURVE ( 'NONE', #37466, #41057, #56746, .T. ) ;
#66184 = EDGE_LOOP ( 'NONE', ( #11553, #46042, #20498, #15774 ) ) ;
#66185 = ORIENTED_EDGE ( 'NONE', *, *, #48728, .T. ) ;
#66186 = PLANE ( 'NONE',  #36182 ) ;
#66187 = ADVANCED_FACE ( 'NONE', ( #51094 ), #68062, .F. ) ;
#66188 = ADVANCED_FACE ( 'NONE', ( #45789 ), #13615, .F. ) ;
#66189 = LINE ( 'NONE', #39982, #7444 ) ;
#66190 = ORIENTED_EDGE ( 'NONE', *, *, #38701, .F. ) ;
#66191 = CARTESIAN_POINT ( 'NONE',  ( 12.90000000000000213, 13.66939075806899240, -20.79999999999999361 ) ) ;
#66192 = CIRCLE ( 'NONE', #17631, 1.000000000000000000 ) ;
#66194 = EDGE_LOOP ( 'NONE', ( #12002, #66165, #4401, #50429 ) ) ;
#66193 = CARTESIAN_POINT ( 'NONE',  ( 7.500000000000000000, -53.81370849898476649, 20.00000000000000000 ) ) ;
#66195 = ORIENTED_EDGE ( 'NONE', *, *, #64884, .F. ) ;
#66196 = DIRECTION ( 'NONE',  ( -1.836970198721029934E-16, 1.836970198721036344E-16, -1.000000000000000000 ) ) ;
#66197 = CARTESIAN_POINT ( 'NONE',  ( -3.650476262117221093, 10.49297626211717116, 54.00000000000000711 ) ) ;
#66198 = CIRCLE ( 'NONE', #36900, 3.500000000000003109 ) ;
#66199 = PLANE ( 'NONE',  #61076 ) ;
#66200 = PLANE ( 'NONE',  #37212 ) ;
#66201 = CARTESIAN_POINT ( 'NONE',  ( 41.09999999999999432, 13.66939075806899950, 20.80000000000000426 ) ) ;
#66202 = LINE ( 'NONE', #17766, #57595 ) ;
#66203 = VECTOR ( 'NONE', #37518, 1000.000000000000000 ) ;
#66204 = AXIS2_PLACEMENT_3D ( 'NONE', #35481, #2614, #2271 ) ;
#66205 = ORIENTED_EDGE ( 'NONE', *, *, #17258, .T. ) ;
#66206 = FACE_OUTER_BOUND ( 'NONE', #59471, .T. ) ;
#66208 = ORIENTED_EDGE ( 'NONE', *, *, #46543, .T. ) ;
#66207 = CARTESIAN_POINT ( 'NONE',  ( 11.00000000000000000, -16.28999999999710369, -14.50000000000000000 ) ) ;
#66209 = VECTOR ( 'NONE', #50277, 1000.000000000000000 ) ;
#66210 = AXIS2_PLACEMENT_3D ( 'NONE', #55184, #22663, #44210 ) ;
#66212 = LINE ( 'NONE', #61577, #54721 ) ;
#66211 = VECTOR ( 'NONE', #54117, 1000.000000000000000 ) ;
#66213 = DIRECTION ( 'NONE',  ( -1.000000000000000000, 0.000000000000000000, 0.000000000000000000 ) ) ;
#66214 = DIRECTION ( 'NONE',  ( 0.000000000000000000, 0.000000000000000000, -1.000000000000000000 ) ) ;
#66215 = DIRECTION ( 'NONE',  ( 0.000000000000000000, 0.7046037717862339012, -0.7096009616570518874 ) ) ;
#66216 = AXIS2_PLACEMENT_3D ( 'NONE', #47856, #26648, #52843 ) ;
#66217 = CIRCLE ( 'NONE', #609, 24.99999999998794920 ) ;
#66218 = AXIS2_PLACEMENT_3D ( 'NONE', #34582, #56171, #51200 ) ;
#66219 = DIRECTION ( 'NONE',  ( 1.000000000000000000, -0.000000000000000000, 0.000000000000000000 ) ) ;
#66220 = ORIENTED_EDGE ( 'NONE', *, *, #35912, .F. ) ;
#66221 = ORIENTED_EDGE ( 'NONE', *, *, #44184, .T. ) ;
#66222 = VECTOR ( 'NONE', #8963, 1000.000000000000114 ) ;
#66223 = DIRECTION ( 'NONE',  ( -1.000000000000000000, 0.000000000000000000, 0.000000000000000000 ) ) ;
#66224 = ADVANCED_FACE ( 'NONE', ( #62044 ), #35169, .T. ) ;
#66225 = VECTOR ( 'NONE', #36311, 1000.000000000000000 ) ;
#66226 = CARTESIAN_POINT ( 'NONE',  ( 23.48000000000000043, -15.50000000000000000, 26.00000000000000355 ) ) ;
#66227 = ORIENTED_EDGE ( 'NONE', *, *, #24610, .F. ) ;
#66228 = LINE ( 'NONE', #65873, #11301 ) ;
#66229 = ORIENTED_EDGE ( 'NONE', *, *, #22610, .F. ) ;
#66230 = EDGE_CURVE ( 'NONE', #67811, #22061, #11698, .T. ) ;
#66231 = ORIENTED_EDGE ( 'NONE', *, *, #27795, .T. ) ;
#66232 = DIRECTION ( 'NONE',  ( 0.000000000000000000, 0.000000000000000000, -1.000000000000000000 ) ) ;
#66233 = CARTESIAN_POINT ( 'NONE',  ( 4.456444791733522252E-16, 7.450000000000002842, -24.50000000000000000 ) ) ;
#66234 = ORIENTED_EDGE ( 'NONE', *, *, #9425, .F. ) ;
#66235 = PLANE ( 'NONE',  #59291 ) ;
#66236 = DIRECTION ( 'NONE',  ( 1.836970198721029934E-16, 1.836970198721010706E-16, -1.000000000000000000 ) ) ;
#66237 = DIRECTION ( 'NONE',  ( -1.000000000000000000, 0.000000000000000000, 0.000000000000000000 ) ) ;
#66238 = ORIENTED_EDGE ( 'NONE', *, *, #32508, .T. ) ;
#66240 = ORIENTED_EDGE ( 'NONE', *, *, #42387, .T. ) ;
#66239 = DIRECTION ( 'NONE',  ( 0.000000000000000000, 0.000000000000000000, 1.000000000000000000 ) ) ;
#66241 = DIRECTION ( 'NONE',  ( -0.000000000000000000, -0.000000000000000000, -1.000000000000000000 ) ) ;
#66242 = DIRECTION ( 'NONE',  ( 1.836970198721029934E-16, 1.836970198721010706E-16, -1.000000000000000000 ) ) ;
#66243 = FACE_OUTER_BOUND ( 'NONE', #57179, .T. ) ;
#66244 = CARTESIAN_POINT ( 'NONE',  ( 8.930623737882818602, -9.703773737882814387, 26.00000000000000000 ) ) ;
#66245 = EDGE_LOOP ( 'NONE', ( #48756, #37123, #68625, #61850 ) ) ;
#66246 = VECTOR ( 'NONE', #7062, 1000.000000000000000 ) ;
#66247 = CARTESIAN_POINT ( 'NONE',  ( -7.342976262117293373, -6.665817930929262225, 54.00000000000000711 ) ) ;
#66248 = CARTESIAN_POINT ( 'NONE',  ( 7.969523737882811432, 9.547976262117192192, 26.00000000000000711 ) ) ;
#66249 = VECTOR ( 'NONE', #11911, 1000.000000000000000 ) ;
#66250 = EDGE_LOOP ( 'NONE', ( #8030, #37218, #24398, #43156 ) ) ;
#66251 = VERTEX_POINT ( 'NONE', #30934 ) ;
#66252 = AXIS2_PLACEMENT_3D ( 'NONE', #12003, #28278, #49847 ) ;
#66253 = AXIS2_PLACEMENT_3D ( 'NONE', #33579, #39230, #29655 ) ;
#66254 = ORIENTED_EDGE ( 'NONE', *, *, #46000, .F. ) ;
#66255 = DIRECTION ( 'NONE',  ( -1.000000000000000000, 0.000000000000000000, 0.000000000000000000 ) ) ;
#66256 = DIRECTION ( 'NONE',  ( 1.000000000000000000, 0.000000000000000000, 0.000000000000000000 ) ) ;
#66257 = CARTESIAN_POINT ( 'NONE',  ( -7.813516549646839948, -12.00648345035340903, 455.0000000000000568 ) ) ;
#66258 = AXIS2_PLACEMENT_3D ( 'NONE', #65948, #39088, #23522 ) ;
#66259 = EDGE_CURVE ( 'NONE', #13174, #68211, #9439, .T. ) ;
#66260 = CIRCLE ( 'NONE', #17704, 0.1749999999999989342 ) ;
#66261 =( GEOMETRIC_REPRESENTATION_CONTEXT ( 3 ) GLOBAL_UNCERTAINTY_ASSIGNED_CONTEXT ( ( #64896 ) ) GLOBAL_UNIT_ASSIGNED_CONTEXT ( ( #18157, #40058, #35108 ) ) REPRESENTATION_CONTEXT ( 'NONE', 'WORKASPACE' ) );
#66262 = ORIENTED_EDGE ( 'NONE', *, *, #41913, .T. ) ;
#66263 = EDGE_LOOP ( 'NONE', ( #6138, #37052, #3456, #9827 ) ) ;
#66264 = EDGE_LOOP ( 'NONE', ( #44871, #31552, #51060, #49421 ) ) ;
#66265 = CYLINDRICAL_SURFACE ( 'NONE', #68962, 0.5249999999999994671 ) ;
#66266 = AXIS2_PLACEMENT_3D ( 'NONE', #26918, #48479, #41237 ) ;
#66267 = VECTOR ( 'NONE', #14511, 1000.000000000000000 ) ;
#66268 = ORIENTED_EDGE ( 'NONE', *, *, #20370, .T. ) ;
#66269 = ORIENTED_EDGE ( 'NONE', *, *, #49359, .F. ) ;
#66270 = EDGE_CURVE ( 'NONE', #64180, #9560, #68134, .T. ) ;
#66271 = EDGE_CURVE ( 'NONE', #6262, #45635, #58155, .T. ) ;
#66272 = EDGE_LOOP ( 'NONE', ( #1961, #63328 ) ) ;
#66273 = ORIENTED_EDGE ( 'NONE', *, *, #21388, .F. ) ;
#66274 = CARTESIAN_POINT ( 'NONE',  ( 78.77321854994620765, 47.95351654967443977, 29.00000000000000000 ) ) ;
#66275 = ADVANCED_FACE ( 'NONE', ( #20321 ), #36578, .T. ) ;
#66276 = ADVANCED_FACE ( 'NONE', ( #19974 ), #21017, .T. ) ;
#66278 = VERTEX_POINT ( 'NONE', #47888 ) ;
#66277 = PLANE ( 'NONE',  #50301 ) ;
#66279 = CARTESIAN_POINT ( 'NONE',  ( 5.257023737882819070, -5.257023737882815517, 26.00000000000000711 ) ) ;
#66280 = PRODUCT_DEFINITION_SHAPE ( 'NONE', 'NONE',  #28759 ) ;
#66281 = AXIS2_PLACEMENT_3D ( 'NONE', #20625, #46450, #35846 ) ;
#66282 = LINE ( 'NONE', #6191, #1327 ) ;
#66283 = ADVANCED_FACE ( 'NONE', ( #41889 ), #15727, .F. ) ;
#66284 = CARTESIAN_POINT ( 'NONE',  ( 176.4833316329832940, 0.000000000000000000, 322.4587476295993156 ) ) ;
#66286 = ORIENTED_EDGE ( 'NONE', *, *, #47764, .T. ) ;
#66285 = CARTESIAN_POINT ( 'NONE',  ( 11.00000000000000000, -11.10796162543699950, -9.102987789146602893 ) ) ;
#66287 = LINE ( 'NONE', #28784, #32841 ) ;
#66288 = DIRECTION ( 'NONE',  ( 1.000000000000000000, 5.013651664672856055E-16, 0.000000000000000000 ) ) ;
#66289 = CARTESIAN_POINT ( 'NONE',  ( -4.393516549646667713, 11.77351654964658856, 455.0000000000000568 ) ) ;
#66290 = VERTEX_POINT ( 'NONE', #63814 ) ;
#66291 = CARTESIAN_POINT ( 'NONE',  ( -8.689999999999999503, 8.750000000000000000, -7.000000000000000000 ) ) ;
#66292 = CARTESIAN_POINT ( 'NONE',  ( -6.350872789121377870, -6.836383711242978833, 54.00000000000000711 ) ) ;
#66293 = LINE ( 'NONE', #23146, #66141 ) ;
#66294 = MANIFOLD_SOLID_BREP ( 'LPattern1[25]', #26156 ) ;
#66295 = VECTOR ( 'NONE', #8822, 1000.000000000000000 ) ;
#66296 = VERTEX_POINT ( 'NONE', #53223 ) ;
#66297 = DIRECTION ( 'NONE',  ( 0.000000000000000000, -0.7071067811865470176, -0.7071067811865480168 ) ) ;
#66298 = CARTESIAN_POINT ( 'NONE',  ( 290.0000000000000000, 0.000000000000000000, -26.50000000000000000 ) ) ;
#66299 = DIRECTION ( 'NONE',  ( -1.000000000000000000, 0.000000000000000000, 0.000000000000000000 ) ) ;
#66300 = ORIENTED_EDGE ( 'NONE', *, *, #5524, .T. ) ;
#66301 = AXIS2_PLACEMENT_3D ( 'NONE', #11579, #6295, #38481 ) ;
#66302 = AXIS2_PLACEMENT_3D ( 'NONE', #27162, #31782, #21848 ) ;
#66303 = CARTESIAN_POINT ( 'NONE',  ( 3.682023737882814007, 9.722976262117208890, 26.00000000000000711 ) ) ;
#66304 = CARTESIAN_POINT ( 'NONE',  ( -11.11351654964671098, 7.793516549646603231, 455.0000000000000568 ) ) ;
#66305 = DIRECTION ( 'NONE',  ( 0.000000000000000000, -1.000000000000000000, 0.000000000000000000 ) ) ;
#66306 = LINE ( 'NONE', #17513, #65067 ) ;
#66307 = CIRCLE ( 'NONE', #34696, 4.000000000000000888 ) ;
#66308 = VECTOR ( 'NONE', #64556, 1000.000000000000000 ) ;
#66309 = ORIENTED_EDGE ( 'NONE', *, *, #23998, .F. ) ;
#66310 = CARTESIAN_POINT ( 'NONE',  ( 30.00000000000000000, -11.50000000000000000, -15.00000000000000000 ) ) ;
#66311 = DIRECTION ( 'NONE',  ( 0.000000000000000000, 0.000000000000000000, -1.000000000000000000 ) ) ;
#66312 = CARTESIAN_POINT ( 'NONE',  ( -11.11351654964670921, 8.333516549646663663, 455.0000000000000568 ) ) ;
#66313 = EDGE_CURVE ( 'NONE', #56866, #44739, #37293, .T. ) ;
#66314 = EDGE_CURVE ( 'NONE', #66510, #38207, #47207, .T. ) ;
#66315 = EDGE_CURVE ( 'NONE', #63045, #17547, #39947, .T. ) ;
#66316 = VECTOR ( 'NONE', #50022, 1000.000000000000000 ) ;
#66317 = FACE_OUTER_BOUND ( 'NONE', #41719, .T. ) ;
#66318 = AXIS2_PLACEMENT_3D ( 'NONE', #16952, #65394, #33203 ) ;
#66319 = CARTESIAN_POINT ( 'NONE',  ( 280.0000000000000000, -25.50000000000000355, -20.00000000000000000 ) ) ;
#66320 = ORIENTED_EDGE ( 'NONE', *, *, #68542, .T. ) ;
#66321 = DIRECTION ( 'NONE',  ( -9.050731179009442381E-15, -1.000000000000000000, 0.000000000000000000 ) ) ;
#66322 = LINE ( 'NONE', #39430, #32791 ) ;
#66323 = CARTESIAN_POINT ( 'NONE',  ( -5.993516549646728642, -6.006483450353378828, 195.0000000000000284 ) ) ;
#66324 = EDGE_CURVE ( 'NONE', #3393, #28592, #25292, .T. ) ;
#66325 = DIRECTION ( 'NONE',  ( -1.000000000000000000, 0.000000000000000000, 0.000000000000000000 ) ) ;
#66326 = DIRECTION ( 'NONE',  ( 1.000000000000000000, 0.000000000000000000, 0.000000000000000000 ) ) ;
#66327 = ORIENTED_EDGE ( 'NONE', *, *, #54330, .T. ) ;
#66328 = VERTEX_POINT ( 'NONE', #42934 ) ;
#66329 = AXIS2_PLACEMENT_3D ( 'NONE', #55091, #39159, #16208 ) ;
#66330 = FACE_OUTER_BOUND ( 'NONE', #59230, .T. ) ;
#66331 = FACE_OUTER_BOUND ( 'NONE', #69765, .T. ) ;
#66332 = EDGE_LOOP ( 'NONE', ( #56, #22325, #30419, #27184 ) ) ;
#66333 = LINE ( 'NONE', #48684, #53310 ) ;
#66334 = ORIENTED_EDGE ( 'NONE', *, *, #65943, .T. ) ;
#66335 = DIRECTION ( 'NONE',  ( -0.5773502691896175154, 0.5773502691896339467, -0.5773502691896257311 ) ) ;
#66336 = ORIENTED_EDGE ( 'NONE', *, *, #32695, .T. ) ;
#66337 = ORIENTED_EDGE ( 'NONE', *, *, #52517, .T. ) ;
#66338 = DIRECTION ( 'NONE',  ( -1.301042606982605321E-16, 1.000000000000000000, 0.000000000000000000 ) ) ;
#66339 = FACE_OUTER_BOUND ( 'NONE', #59090, .T. ) ;
#66340 = DIRECTION ( 'NONE',  ( -1.000000000000000000, 0.000000000000000000, 0.000000000000000000 ) ) ;
#66341 = CARTESIAN_POINT ( 'NONE',  ( -13.00000000000000178, -17.50000000000000000, 20.05051025721700242 ) ) ;
#66342 = ORIENTED_EDGE ( 'NONE', *, *, #56800, .F. ) ;
#66343 = ORIENTED_EDGE ( 'NONE', *, *, #16798, .T. ) ;
#66344 = PLANE ( 'NONE',  #52718 ) ;
#66345 = CARTESIAN_POINT ( 'NONE',  ( 8.144523737882817471, -9.562023737882817898, 54.00000000000000711 ) ) ;
#66346 = VERTEX_POINT ( 'NONE', #64514 ) ;
#66347 = VERTEX_POINT ( 'NONE', #16072 ) ;
#66348 = ORIENTED_EDGE ( 'NONE', *, *, #4647, .F. ) ;
#66349 = CIRCLE ( 'NONE', #44891, 0.5000000000009302559 ) ;
#66350 = AXIS2_PLACEMENT_3D ( 'NONE', #22486, #21432, #38061 ) ;
#66351 = VECTOR ( 'NONE', #59608, 1000.000000000000000 ) ;
#66352 = CARTESIAN_POINT ( 'NONE',  ( 8.241237374594303944, -1.634292677759888068, 54.00000000000000711 ) ) ;
#66354 = ORIENTED_EDGE ( 'NONE', *, *, #51271, .F. ) ;
#66353 = CARTESIAN_POINT ( 'NONE',  ( 7.606483450353424658, 11.77351654964657435, 455.0000000000000568 ) ) ;
#66355 = EDGE_CURVE ( 'NONE', #33050, #48502, #37643, .T. ) ;
#66356 = VECTOR ( 'NONE', #53473, 1000.000000000000000 ) ;
#66357 = AXIS2_PLACEMENT_3D ( 'NONE', #13127, #2875, #49923 ) ;
#66358 = CARTESIAN_POINT ( 'NONE',  ( -8.393516549646768965, -5.668387132715940524, 455.0000000000000568 ) ) ;
#66359 = CARTESIAN_POINT ( 'NONE',  ( 2.706483450353350584, -10.09643294401463365, 455.0000000000000568 ) ) ;
#66360 = ADVANCED_FACE ( 'NONE', ( #39014 ), #6149, .T. ) ;
#66361 = EDGE_CURVE ( 'NONE', #68364, #21659, #165, .T. ) ;
#66362 = ORIENTED_EDGE ( 'NONE', *, *, #17512, .F. ) ;
#66363 = ORIENTED_EDGE ( 'NONE', *, *, #32220, .F. ) ;
#66364 = AXIS2_PLACEMENT_3D ( 'NONE', #28722, #59535, #29417 ) ;
#66365 = VECTOR ( 'NONE', #37740, 1000.000000000000000 ) ;
#66366 = ADVANCED_FACE ( 'NONE', ( #17439 ), #6509, .T. ) ;
#66367 = LINE ( 'NONE', #3064, #51844 ) ;
#66368 = FACE_OUTER_BOUND ( 'NONE', #46885, .T. ) ;
#66369 = EDGE_CURVE ( 'NONE', #66152, #28918, #1522, .T. ) ;
#66370 = DIRECTION ( 'NONE',  ( 8.659560562354963673E-17, 0.7071067811865450192, -0.7071067811865500152 ) ) ;
#66371 = EDGE_CURVE ( 'NONE', #32538, #2059, #64861, .T. ) ;
#66372 = VECTOR ( 'NONE', #25341, 1000.000000000000000 ) ;
#66373 = CARTESIAN_POINT ( 'NONE',  ( 14.25000000000000000, -0.2038245569916330158, 23.22168783648699986 ) ) ;
#66374 = LINE ( 'NONE', #33500, #16659 ) ;
#66376 = VERTEX_POINT ( 'NONE', #59555 ) ;
#66375 = CARTESIAN_POINT ( 'NONE',  ( 11.00000000000000000, -17.50000000000000000, 15.70499999999969809 ) ) ;
#66377 = ORIENTED_EDGE ( 'NONE', *, *, #22130, .T. ) ;
#66378 = LINE ( 'NONE', #33152, #56931 ) ;
#66379 = DIRECTION ( 'NONE',  ( -0.7671651518153105309, -0.6414496315691445849, 0.000000000000000000 ) ) ;
#66380 = CARTESIAN_POINT ( 'NONE',  ( 41.09999999999999432, -0.2000000000000000111, 0.000000000000000000 ) ) ;
#66381 = DIRECTION ( 'NONE',  ( 1.000000000000000000, 0.000000000000000000, 0.000000000000000000 ) ) ;
#66382 = PLANE ( 'NONE',  #13934 ) ;
#66383 = VERTEX_POINT ( 'NONE', #16419 ) ;
#66384 = FACE_OUTER_BOUND ( 'NONE', #61335, .T. ) ;
#66385 = PLANE ( 'NONE',  #41779 ) ;
#66386 = DIRECTION ( 'NONE',  ( 1.836970198721029934E-16, 1.836970198721010706E-16, -1.000000000000000000 ) ) ;
#66387 = DIRECTION ( 'NONE',  ( 0.000000000000000000, 0.000000000000000000, -1.000000000000000000 ) ) ;
#66388 = PRESENTATION_LAYER_ASSIGNMENT (  '', '', ( #48337 ) ) ;
#66389 = DIRECTION ( 'NONE',  ( -0.000000000000000000, -0.000000000000000000, -1.000000000000000000 ) ) ;
#66390 = CARTESIAN_POINT ( 'NONE',  ( -7.250000000000000888, 8.250000000000001776, -26.00000000000001066 ) ) ;
#66391 = CARTESIAN_POINT ( 'NONE',  ( 11.00000000000000000, -12.00000000000000000, 12.19999999999999929 ) ) ;
#66392 = EDGE_LOOP ( 'NONE', ( #65070, #64849, #20687, #69359 ) ) ;
#66393 = CARTESIAN_POINT ( 'NONE',  ( -9.547976262117256141, 7.955476262117183062, 54.00000000000000711 ) ) ;
#66394 = CARTESIAN_POINT ( 'NONE',  ( -5.242976262117259978, 3.142976262117183062, 54.00000000000000711 ) ) ;
#66395 = EDGE_LOOP ( 'NONE', ( #47008, #30104, #26967, #31120 ) ) ;
#66396 = PLANE ( 'NONE',  #15363 ) ;
#66397 = CARTESIAN_POINT ( 'NONE',  ( 7.969523737882816761, 9.547976262117186863, 54.00000000000000711 ) ) ;
#66398 = EDGE_CURVE ( 'NONE', #50592, #14101, #38856, .T. ) ;
#66399 = DIRECTION ( 'NONE',  ( 0.8660254037844482555, 0.000000000000000000, -0.4999999999999831801 ) ) ;
#66400 = CARTESIAN_POINT ( 'NONE',  ( -9.915476262117259409, 0.9414762621171833823, 54.00000000000000711 ) ) ;
#66401 = ORIENTED_EDGE ( 'NONE', *, *, #3614, .F. ) ;
#66402 = VECTOR ( 'NONE', #45170, 1000.000000000000000 ) ;
#66403 = LINE ( 'NONE', #7690, #57995 ) ;
#66404 = VERTEX_POINT ( 'NONE', #11783 ) ;
#66405 = MANIFOLD_SOLID_BREP ( 'Fillet1', #21663 ) ;
#66406 = DIRECTION ( 'NONE',  ( -1.836970198721029934E-16, -1.836970198721010706E-16, 1.000000000000000000 ) ) ;
#66407 = ORIENTED_EDGE ( 'NONE', *, *, #11903, .F. ) ;
#66408 = CARTESIAN_POINT ( 'NONE',  ( -14.25000000000000000, -0.2038245569916330158, -23.22168783648699986 ) ) ;
#66409 = AXIS2_PLACEMENT_3D ( 'NONE', #38537, #44167, #60088 ) ;
#66410 = AXIS2_PLACEMENT_3D ( 'NONE', #8687, #67029, #24950 ) ;
#66411 = ADVANCED_FACE ( 'NONE', ( #17795 ), #5813, .F. ) ;
#66412 = PRESENTATION_STYLE_ASSIGNMENT (( #63120 ) ) ;
#66413 = EDGE_CURVE ( 'NONE', #35470, #24440, #34041, .T. ) ;
#66414 = DIRECTION ( 'NONE',  ( 0.000000000000000000, 1.000000000000000000, 0.000000000000000000 ) ) ;
#66415 = ORIENTED_EDGE ( 'NONE', *, *, #53349, .F. ) ;
#66416 = ORIENTED_EDGE ( 'NONE', *, *, #55984, .T. ) ;
#66417 = LINE ( 'NONE', #7352, #27215 ) ;
#66418 = ORIENTED_EDGE ( 'NONE', *, *, #50774, .T. ) ;
#66419 = ORIENTED_EDGE ( 'NONE', *, *, #32695, .F. ) ;
#66420 = VECTOR ( 'NONE', #32659, 1000.000000000000114 ) ;
#66421 = CARTESIAN_POINT ( 'NONE',  ( 283.0000000000000568, -40.30000000000000426, 12.20000000000000107 ) ) ;
#66422 = DIRECTION ( 'NONE',  ( 0.000000000000000000, 0.5017180897718492849, 0.8650311892618014475 ) ) ;
#66423 = CARTESIAN_POINT ( 'NONE',  ( 7.357023737882797398, 4.947141984184415087, 54.00000000000000711 ) ) ;
#66424 = VERTEX_POINT ( 'NONE', #504 ) ;
#66425 = PLANE ( 'NONE',  #26710 ) ;
#66427 = DIRECTION ( 'NONE',  ( -0.000000000000000000, -0.000000000000000000, 1.000000000000000000 ) ) ;
#66426 = CARTESIAN_POINT ( 'NONE',  ( -7.250000000000000888, 7.450000000000003730, -11.50000000000000000 ) ) ;
#66428 = ORIENTED_EDGE ( 'NONE', *, *, #66993, .T. ) ;
#66430 = ORIENTED_EDGE ( 'NONE', *, *, #18936, .F. ) ;
#66429 = CARTESIAN_POINT ( 'NONE',  ( 176.4833316329832940, -10.00000000000000178, 280.6301873289890523 ) ) ;
#66431 = EDGE_LOOP ( 'NONE', ( #14892, #54707, #48170, #252 ) ) ;
#66432 = EDGE_CURVE ( 'NONE', #24441, #8384, #38675, .T. ) ;
#66433 = CARTESIAN_POINT ( 'NONE',  ( 0.000000000000000000, 0.000000000000000000, 0.000000000000000000 ) ) ;
#66434 = CARTESIAN_POINT ( 'NONE',  ( 0.000000000000000000, -42.50000000000000000, 26.50000000000000000 ) ) ;
#66435 = VERTEX_POINT ( 'NONE', #43636 ) ;
#66436 = DIRECTION ( 'NONE',  ( 0.000000000000000000, 0.000000000000000000, 1.000000000000000000 ) ) ;
#66437 = FACE_OUTER_BOUND ( 'NONE', #13593, .T. ) ;
#66438 = EDGE_CURVE ( 'NONE', #30263, #6680, #38336, .T. ) ;
#66439 = ORIENTED_EDGE ( 'NONE', *, *, #67554, .T. ) ;
#66440 = VERTEX_POINT ( 'NONE', #33022 ) ;
#66441 = DIRECTION ( 'NONE',  ( -1.000000000000000000, 0.000000000000000000, 0.000000000000000000 ) ) ;
#66442 = DIRECTION ( 'NONE',  ( -1.214636490590110115E-14, -1.000000000000000000, 0.000000000000000000 ) ) ;
#66443 = ORIENTED_EDGE ( 'NONE', *, *, #6684, .T. ) ;
#66444 = LINE ( 'NONE', #55151, #40987 ) ;
#66445 = FACE_OUTER_BOUND ( 'NONE', #60867, .T. ) ;
#66446 = EDGE_CURVE ( 'NONE', #48776, #57629, #54603, .T. ) ;
#66447 = PLANE ( 'NONE',  #49743 ) ;
#66448 = ORIENTED_EDGE ( 'NONE', *, *, #58766, .T. ) ;
#66449 = ADVANCED_FACE ( 'NONE', ( #22422 ), #56665, .T. ) ;
#66450 = AXIS2_PLACEMENT_3D ( 'NONE', #46757, #13536, #14249 ) ;
#66451 = CARTESIAN_POINT ( 'NONE',  ( 17.89999999999999858, -14.06939075806902117, -20.80000000000000426 ) ) ;
#66452 = CARTESIAN_POINT ( 'NONE',  ( 7.606483450353424658, 11.77351654964657435, 455.0000000000000568 ) ) ;
#66454 = ORIENTED_EDGE ( 'NONE', *, *, #44796, .T. ) ;
#66453 = LINE ( 'NONE', #18004, #53302 ) ;
#66456 = ORIENTED_EDGE ( 'NONE', *, *, #48970, .F. ) ;
#66455 = LINE ( 'NONE', #18006, #3017 ) ;
#66457 = DIRECTION ( 'NONE',  ( 0.000000000000000000, -0.7071067811865474617, 0.7071067811865474617 ) ) ;
#66458 = CARTESIAN_POINT ( 'NONE',  ( -11.18999999999999950, 12.00000000000000178, -5.000000000000000000 ) ) ;
#66459 = FACE_BOUND ( 'NONE', #52600, .T. ) ;
#66460 = LINE ( 'NONE', #66112, #11363 ) ;
#66461 = CYLINDRICAL_SURFACE ( 'NONE', #5971, 0.2000000000000005107 ) ;
#66462 = ORIENTED_EDGE ( 'NONE', *, *, #47380, .F. ) ;
#66463 = DIRECTION ( 'NONE',  ( 1.000000000000000000, 0.000000000000000000, 0.000000000000000000 ) ) ;
#66464 = CARTESIAN_POINT ( 'NONE',  ( -10.19191654964685156, -9.804883450353383267, 455.0000000000000568 ) ) ;
#66465 = LINE ( 'NONE', #33599, #7360 ) ;
#66467 = CIRCLE ( 'NONE', #17468, 0.1999999999999987899 ) ;
#66466 = CIRCLE ( 'NONE', #58568, 0.7499999999999997780 ) ;
#66469 = ORIENTED_EDGE ( 'NONE', *, *, #66920, .F. ) ;
#66468 = CARTESIAN_POINT ( 'NONE',  ( 11.78648345035340661, 7.593516549646560421, 455.0000000000000568 ) ) ;
#66470 = CARTESIAN_POINT ( 'NONE',  ( 11.19368345035336532, -11.19368345035347723, 455.0000000000000568 ) ) ;
#66471 = CARTESIAN_POINT ( 'NONE',  ( 10.20488345035340494, 10.19191654964661531, 195.0000000000000284 ) ) ;
#66472 = EDGE_LOOP ( 'NONE', ( #1234, #3565, #20802, #16078 ) ) ;
#66473 = LINE ( 'NONE', #62213, #50096 ) ;
#66474 = DIRECTION ( 'NONE',  ( 1.000000000000000000, 0.000000000000000000, 0.000000000000000000 ) ) ;
#66475 = ORIENTED_EDGE ( 'NONE', *, *, #62382, .T. ) ;
#66476 = EDGE_CURVE ( 'NONE', #36864, #57348, #40751, .T. ) ;
#66477 = DIRECTION ( 'NONE',  ( -1.836970198721029934E-16, 1.836970198721036590E-16, -1.000000000000000000 ) ) ;
#66478 = CARTESIAN_POINT ( 'NONE',  ( 8.250000000000005329, 0.000000000000000000, -14.50000000000000000 ) ) ;
#66479 = LINE ( 'NONE', #2471, #63750 ) ;
#66480 = CARTESIAN_POINT ( 'NONE',  ( 28.00000000000000000, -17.50000000000000000, -15.70500000000000362 ) ) ;
#66481 = EDGE_CURVE ( 'NONE', #15934, #60538, #43347, .T. ) ;
#66482 = FACE_OUTER_BOUND ( 'NONE', #35014, .T. ) ;
#66483 = ORIENTED_EDGE ( 'NONE', *, *, #7168, .F. ) ;
#66484 = DIRECTION ( 'NONE',  ( -0.7671651518152963201, 0.6414496315691619044, 0.000000000000000000 ) ) ;
#66485 = ORIENTED_EDGE ( 'NONE', *, *, #64436, .T. ) ;
#66486 = EDGE_CURVE ( 'NONE', #34907, #67031, #8217, .T. ) ;
#66487 = ORIENTED_EDGE ( 'NONE', *, *, #61270, .T. ) ;
#66488 = LINE ( 'NONE', #50585, #27955 ) ;
#66489 = EDGE_CURVE ( 'NONE', #64510, #32481, #23450, .T. ) ;
#66490 = DIRECTION ( 'NONE',  ( -1.000000000000000000, 0.000000000000000000, 0.000000000000000000 ) ) ;
#66491 = EDGE_CURVE ( 'NONE', #31468, #30799, #2925, .T. ) ;
#66492 = DIRECTION ( 'NONE',  ( 1.000000000000000000, -0.000000000000000000, 0.000000000000000000 ) ) ;
#66493 = ORIENTED_EDGE ( 'NONE', *, *, #26846, .F. ) ;
#66494 = ORIENTED_EDGE ( 'NONE', *, *, #41204, .F. ) ;
#66495 = DIRECTION ( 'NONE',  ( -1.836970198721029934E-16, 1.836970198721036344E-16, -1.000000000000000000 ) ) ;
#66496 = EDGE_LOOP ( 'NONE', ( #59923, #61980, #22851, #67483 ) ) ;
#66497 = CARTESIAN_POINT ( 'NONE',  ( 12.00648345035337883, -11.19368345035347900, 455.0000000000000568 ) ) ;
#66498 = PLANE ( 'NONE',  #56921 ) ;
#66499 = DIRECTION ( 'NONE',  ( 0.000000000000000000, 0.000000000000000000, -1.000000000000000000 ) ) ;
#66500 = EDGE_CURVE ( 'NONE', #25548, #33741, #7525, .T. ) ;
#66501 = EDGE_CURVE ( 'NONE', #54584, #29722, #51012, .T. ) ;
#66502 = AXIS2_PLACEMENT_3D ( 'NONE', #30466, #8895, #50983 ) ;
#66503 = CARTESIAN_POINT ( 'NONE',  ( 15.89999999999999680, -0.2000000000089119934, -8.913009219568841313E-12 ) ) ;
#66505 = CARTESIAN_POINT ( 'NONE',  ( -7.259684009079983902, -7.811466277050722162, 195.0000000000000284 ) ) ;
#66504 = DIRECTION ( 'NONE',  ( 1.819560449471430698E-15, 1.000000000000000000, 1.836970198721032892E-16 ) ) ;
#66506 = ORIENTED_EDGE ( 'NONE', *, *, #19605, .T. ) ;
#66509 = EDGE_CURVE ( 'NONE', #1941, #15054, #19623, .T. ) ;
#66508 = ORIENTED_EDGE ( 'NONE', *, *, #23920, .T. ) ;
#66507 = DIRECTION ( 'NONE',  ( 1.000000000000000000, 0.000000000000000000, 0.000000000000000000 ) ) ;
#66510 = VERTEX_POINT ( 'NONE', #29790 ) ;
#66511 = ORIENTED_EDGE ( 'NONE', *, *, #19327, .F. ) ;
#66512 = EDGE_CURVE ( 'NONE', #3798, #48826, #30147, .T. ) ;
#66513 = EDGE_CURVE ( 'NONE', #52692, #22594, #46401, .T. ) ;
#66514 = VECTOR ( 'NONE', #12104, 1000.000000000000000 ) ;
#66515 = CARTESIAN_POINT ( 'NONE',  ( 27.90000000000000213, -0.000000000000000000, 20.80000000000000426 ) ) ;
#66516 = ADVANCED_FACE ( 'NONE', ( #7865 ), #56317, .F. ) ;
#66518 = AXIS2_PLACEMENT_3D ( 'NONE', #62084, #13658, #35209 ) ;
#66517 = VECTOR ( 'NONE', #57518, 1000.000000000000000 ) ;
#66519 = DIRECTION ( 'NONE',  ( 1.836970198721029934E-16, 1.836970198721010706E-16, -1.000000000000000000 ) ) ;
#66520 = EDGE_CURVE ( 'NONE', #56741, #20459, #46057, .T. ) ;
#66521 = DIRECTION ( 'NONE',  ( -1.000000000000000000, 0.000000000000000000, 0.000000000000000000 ) ) ;
#66522 = ORIENTED_EDGE ( 'NONE', *, *, #19836, .F. ) ;
#66523 = EDGE_LOOP ( 'NONE', ( #37829, #40544, #67761, #67613 ) ) ;
#66524 = EDGE_CURVE ( 'NONE', #66935, #18339, #2223, .T. ) ;
#66525 = VECTOR ( 'NONE', #22308, 1000.000000000000000 ) ;
#66526 = CARTESIAN_POINT ( 'NONE',  ( -7.250000000000001776, -7.249999999999998224, -15.50000000000000000 ) ) ;
#66527 = DIRECTION ( 'NONE',  ( -1.000000000000000000, 0.000000000000000000, 0.000000000000000000 ) ) ;
#66528 = ORIENTED_EDGE ( 'NONE', *, *, #69921, .T. ) ;
#66529 = ORIENTED_EDGE ( 'NONE', *, *, #20714, .F. ) ;
#66530 = DIRECTION ( 'NONE',  ( -1.000000000000000000, 4.745709458399858621E-16, 1.836970198721030674E-16 ) ) ;
#66531 = EDGE_CURVE ( 'NONE', #63520, #17564, #13176, .T. ) ;
#66532 = DIRECTION ( 'NONE',  ( 0.000000000000000000, 0.000000000000000000, 1.000000000000000000 ) ) ;
#66533 = EDGE_LOOP ( 'NONE', ( #51668, #44407, #41902, #11967 ) ) ;
#66534 = ADVANCED_FACE ( 'NONE', ( #34742 ), #39698, .F. ) ;
#66535 = DIRECTION ( 'NONE',  ( -1.000000000000000000, 1.260948829465470062E-14, -1.836970198721007008E-16 ) ) ;
#66537 = VERTEX_POINT ( 'NONE', #8569 ) ;
#66536 = DIRECTION ( 'NONE',  ( -0.7671651518153087546, -0.6414496315691469164, 2.309356642089053889E-17 ) ) ;
#66538 = ORIENTED_EDGE ( 'NONE', *, *, #45281, .F. ) ;
#66539 = DIRECTION ( 'NONE',  ( -0.000000000000000000, -0.000000000000000000, 1.000000000000000000 ) ) ;
#66540 = CARTESIAN_POINT ( 'NONE',  ( 275.0000000000000000, -31.30000000000045191, 8.900000000000430234 ) ) ;
#66541 = DIRECTION ( 'NONE',  ( -0.000000000000000000, -0.000000000000000000, -1.000000000000000000 ) ) ;
#66542 = CARTESIAN_POINT ( 'NONE',  ( 280.0000000000000000, -20.49999999999999645, 20.00000000000000000 ) ) ;
#66543 = DIRECTION ( 'NONE',  ( -1.000000000000000000, 0.000000000000000000, 0.000000000000000000 ) ) ;
#66544 = VECTOR ( 'NONE', #12585, 1000.000000000000000 ) ;
#66545 = CYLINDRICAL_SURFACE ( 'NONE', #63256, 0.1999999999999987899 ) ;
#66546 = DIRECTION ( 'NONE',  ( -0.000000000000000000, -0.000000000000000000, 1.000000000000000000 ) ) ;
#66547 = ORIENTED_EDGE ( 'NONE', *, *, #2696, .T. ) ;
#66548 = DIRECTION ( 'NONE',  ( 0.000000000000000000, 0.000000000000000000, 1.000000000000000000 ) ) ;
#66549 = VECTOR ( 'NONE', #65966, 1000.000000000000000 ) ;
#66550 = VECTOR ( 'NONE', #56928, 1000.000000000000000 ) ;
#66552 = ORIENTED_EDGE ( 'NONE', *, *, #40628, .F. ) ;
#66551 = DIRECTION ( 'NONE',  ( 1.000000000000000000, 0.000000000000000000, -0.000000000000000000 ) ) ;
#66553 = CARTESIAN_POINT ( 'NONE',  ( 9.900000000000000355, -21.00000000000000000, 18.00000000000000355 ) ) ;
#66554 = DIRECTION ( 'NONE',  ( -0.000000000000000000, -0.000000000000000000, -1.000000000000000000 ) ) ;
#66555 = CYLINDRICAL_SURFACE ( 'NONE', #6521, 1.000000000000000000 ) ;
#66556 = LINE ( 'NONE', #1179, #17114 ) ;
#66557 = AXIS2_PLACEMENT_3D ( 'NONE', #69712, #15263, #37189 ) ;
#66558 = CARTESIAN_POINT ( 'NONE',  ( 283.0000000000000568, -25.60000000000000142, 15.10000000000000142 ) ) ;
#66559 = ORIENTED_EDGE ( 'NONE', *, *, #69404, .T. ) ;
#66560 = VERTEX_POINT ( 'NONE', #18835 ) ;
#66561 = VECTOR ( 'NONE', #52137, 1000.000000000000000 ) ;
#66562 = CARTESIAN_POINT ( 'NONE',  ( -7.250000000000000888, 7.250000000000001776, -11.50000000000000000 ) ) ;
#66563 = DIRECTION ( 'NONE',  ( 0.000000000000000000, 1.000000000000000000, 0.000000000000000000 ) ) ;
#66564 = CIRCLE ( 'NONE', #50759, 2.250000000000001776 ) ;
#66565 = ADVANCED_FACE ( 'NONE', ( #3273 ), #61253, .T. ) ;
#66566 = FACE_BOUND ( 'NONE', #48097, .T. ) ;
#66567 = ORIENTED_EDGE ( 'NONE', *, *, #26858, .F. ) ;
#66568 = DIRECTION ( 'NONE',  ( 0.000000000000000000, 0.000000000000000000, 1.000000000000000000 ) ) ;
#66569 = VERTEX_POINT ( 'NONE', #62661 ) ;
#66570 = EDGE_CURVE ( 'NONE', #51618, #31475, #34376, .T. ) ;
#66571 = ORIENTED_EDGE ( 'NONE', *, *, #26637, .T. ) ;
#66572 = DIRECTION ( 'NONE',  ( 0.000000000000000000, -0.8650311892618017806, -0.5017180897718488408 ) ) ;
#66573 = VECTOR ( 'NONE', #16175, 1000.000000000000000 ) ;
#66574 = FACE_BOUND ( 'NONE', #65379, .T. ) ;
#66575 = EDGE_LOOP ( 'NONE', ( #36613, #7868, #34172, #2665 ) ) ;
#66576 = PLANE ( 'NONE',  #2850 ) ;
#66577 = ADVANCED_FACE ( 'NONE', ( #5026, #37213 ), #25556, .T. ) ;
#66578 = CARTESIAN_POINT ( 'NONE',  ( -17.00000000000000000, -16.28999999999999915, 14.50000000000000000 ) ) ;
#66579 = EDGE_CURVE ( 'NONE', #66440, #64822, #52422, .T. ) ;
#66580 = LINE ( 'NONE', #62313, #26105 ) ;
#66581 = ORIENTED_EDGE ( 'NONE', *, *, #32529, .T. ) ;
#66583 = VERTEX_POINT ( 'NONE', #68326 ) ;
#66582 = CARTESIAN_POINT ( 'NONE',  ( -11.00000000000000000, -8.959999999999999076, 17.04524521594300523 ) ) ;
#66584 = DIRECTION ( 'NONE',  ( -0.000000000000000000, -0.000000000000000000, -1.000000000000000000 ) ) ;
#66585 = LINE ( 'NONE', #23099, #9007 ) ;
#66586 = FACE_OUTER_BOUND ( 'NONE', #41021, .T. ) ;
#66587 = AXIS2_PLACEMENT_3D ( 'NONE', #43673, #26363, #5148 ) ;
#66588 = CARTESIAN_POINT ( 'NONE',  ( 11.00000000000000000, -17.50000000000000000, 26.64999999999999858 ) ) ;
#66589 = DIRECTION ( 'NONE',  ( 0.000000000000000000, 0.000000000000000000, 1.000000000000000000 ) ) ;
#66590 = DIRECTION ( 'NONE',  ( -1.000000000000000000, 0.000000000000000000, 0.000000000000000000 ) ) ;
#66591 = VERTEX_POINT ( 'NONE', #69739 ) ;
#66592 = EDGE_LOOP ( 'NONE', ( #36067, #51580, #30952, #68404 ) ) ;
#66593 = ADVANCED_FACE ( 'NONE', ( #9635 ), #21292, .T. ) ;
#66594 = ORIENTED_EDGE ( 'NONE', *, *, #25767, .F. ) ;
#66595 = CARTESIAN_POINT ( 'NONE',  ( 8.250000000000005329, -7.249999999999998224, -13.50000000000000178 ) ) ;
#66596 = DIRECTION ( 'NONE',  ( 2.135044278125299371E-15, 1.000000000000000000, 0.000000000000000000 ) ) ;
#66597 = VECTOR ( 'NONE', #50747, 1000.000000000000000 ) ;
#66598 = VECTOR ( 'NONE', #31035, 1000.000000000000000 ) ;
#66599 = DIRECTION ( 'NONE',  ( -0.000000000000000000, -0.000000000000000000, 1.000000000000000000 ) ) ;
#66600 =( NAMED_UNIT ( * ) SI_UNIT ( $, .STERADIAN. ) SOLID_ANGLE_UNIT ( ) );
#66601 = VECTOR ( 'NONE', #41255, 1000.000000000000000 ) ;
#66602 = ORIENTED_EDGE ( 'NONE', *, *, #37098, .F. ) ;
#66603 = ORIENTED_EDGE ( 'NONE', *, *, #43207, .F. ) ;
#66604 = ORIENTED_EDGE ( 'NONE', *, *, #55335, .F. ) ;
#66605 = AXIS2_PLACEMENT_3D ( 'NONE', #9071, #4131, #25701 ) ;
#66606 = AXIS2_PLACEMENT_3D ( 'NONE', #54742, #59697, #54399 ) ;
#66607 = EDGE_LOOP ( 'NONE', ( #10388, #50238, #41818, #3038 ) ) ;
#66608 = ORIENTED_EDGE ( 'NONE', *, *, #29253, .F. ) ;
#66609 = VERTEX_POINT ( 'NONE', #14940 ) ;
#66610 = AXIS2_PLACEMENT_3D ( 'NONE', #3189, #40998, #62929 ) ;
#66611 = ORIENTED_EDGE ( 'NONE', *, *, #50701, .F. ) ;
#66612 = CARTESIAN_POINT ( 'NONE',  ( 11.75000000000000000, -5.000000000000000000, 23.89194109070750116 ) ) ;
#66613 = CIRCLE ( 'NONE', #4557, 0.5000000000079362072 ) ;
#66614 = EDGE_CURVE ( 'NONE', #38962, #36500, #52401, .T. ) ;
#66616 = VERTEX_POINT ( 'NONE', #10334 ) ;
#66615 = DIRECTION ( 'NONE',  ( -0.8660254037844435926, -0.4999999999999913958, 0.000000000000000000 ) ) ;
#66617 = DIRECTION ( 'NONE',  ( 1.836970198721029934E-16, 1.836970198721010706E-16, -1.000000000000000000 ) ) ;
#66618 = EDGE_CURVE ( 'NONE', #27416, #11776, #33213, .T. ) ;
#66619 = FACE_OUTER_BOUND ( 'NONE', #59794, .T. ) ;
#66620 = CARTESIAN_POINT ( 'NONE',  ( -7.450000000000001954, 0.000000000000000000, -7.500000000000000000 ) ) ;
#66621 = EDGE_CURVE ( 'NONE', #9302, #3011, #15985, .T. ) ;
#66623 = ORIENTED_EDGE ( 'NONE', *, *, #61790, .T. ) ;
#66622 = DIRECTION ( 'NONE',  ( -3.016910393003147986E-15, -1.000000000000000000, -3.673940397442059868E-16 ) ) ;
#66624 = ORIENTED_EDGE ( 'NONE', *, *, #332, .F. ) ;
#66625 = VECTOR ( 'NONE', #24552, 1000.000000000000000 ) ;
#66626 = CARTESIAN_POINT ( 'NONE',  ( 10.00000000000000000, 14.08845687959340331, 21.00000000000000000 ) ) ;
#66627 = CARTESIAN_POINT ( 'NONE',  ( 30.00000000000000000, -12.00000000000000000, 11.00000000000000000 ) ) ;
#66628 = DIRECTION ( 'NONE',  ( 0.000000000000000000, 0.000000000000000000, 1.000000000000000000 ) ) ;
#66629 = ORIENTED_EDGE ( 'NONE', *, *, #69683, .F. ) ;
#66630 = DIRECTION ( 'NONE',  ( -1.000000000000000000, 0.000000000000000000, 0.000000000000000000 ) ) ;
#66631 = DIRECTION ( 'NONE',  ( 0.000000000000000000, -0.000000000000000000, 1.000000000000000000 ) ) ;
#66632 = DIRECTION ( 'NONE',  ( -1.000000000000000000, 0.000000000000000000, 0.000000000000000000 ) ) ;
#66633 = AXIS2_PLACEMENT_3D ( 'NONE', #38368, #37331, #32373 ) ;
#66634 = ORIENTED_EDGE ( 'NONE', *, *, #32359, .T. ) ;
#66635 = CYLINDRICAL_SURFACE ( 'NONE', #3079, 5.250000000000000000 ) ;
#66636 = CARTESIAN_POINT ( 'NONE',  ( 11.78648345035333378, 4.393516549646564684, 195.0000000000000284 ) ) ;
#66637 = CARTESIAN_POINT ( 'NONE',  ( 49.00000000000000000, -0.7500000000000000000, 4.943429983321300014 ) ) ;
#66638 = ORIENTED_EDGE ( 'NONE', *, *, #14781, .F. ) ;
#66639 = CARTESIAN_POINT ( 'NONE',  ( 1.480523737882816437, 9.390476262117212869, 54.00000000000000711 ) ) ;
#66640 = VECTOR ( 'NONE', #41051, 1000.000000000000000 ) ;
#66641 = DIRECTION ( 'NONE',  ( -1.000000000000000000, 1.047444401652939849E-14, -1.836970198721010706E-16 ) ) ;
#66642 = DIRECTION ( 'NONE',  ( 3.491481338843133355E-15, 1.000000000000000000, 1.836970198721029934E-16 ) ) ;
#66643 = ADVANCED_FACE ( 'NONE', ( #26591 ), #46750, .T. ) ;
#66644 = VECTOR ( 'NONE', #3013, 1000.000000000000000 ) ;
#66645 = VERTEX_POINT ( 'NONE', #3631 ) ;
#66646 = DIRECTION ( 'NONE',  ( 1.000000000000000000, -0.000000000000000000, 0.000000000000000000 ) ) ;
#66647 = DIRECTION ( 'NONE',  ( 0.000000000000000000, 0.000000000000000000, 1.000000000000000000 ) ) ;
#66648 = PLANE ( 'NONE',  #48925 ) ;
#66650 = EDGE_CURVE ( 'NONE', #63937, #30915, #47901, .T. ) ;
#66649 = VECTOR ( 'NONE', #20040, 1000.000000000000000 ) ;
#66651 = DIRECTION ( 'NONE',  ( 0.000000000000000000, -0.7071067811865474617, 0.7071067811865474617 ) ) ;
#66652 = CARTESIAN_POINT ( 'NONE',  ( 37.90000000000000568, 0.000000000000000000, 2.458500000000000796 ) ) ;
#66653 = ORIENTED_EDGE ( 'NONE', *, *, #51278, .T. ) ;
#66654 = DIRECTION ( 'NONE',  ( -1.828336019306068379E-14, -1.000000000000000000, -1.836970198721044232E-16 ) ) ;
#66655 = CARTESIAN_POINT ( 'NONE',  ( -11.18071654964669648, 11.18071654964658812, 455.0000000000000568 ) ) ;
#66656 = EDGE_CURVE ( 'NONE', #68234, #2701, #58438, .T. ) ;
#66657 = EDGE_CURVE ( 'NONE', #14316, #17827, #58101, .T. ) ;
#66658 = DIRECTION ( 'NONE',  ( -1.836970198721029934E-16, -1.836970198721010706E-16, 1.000000000000000000 ) ) ;
#66659 = CIRCLE ( 'NONE', #17009, 0.1999999999999996503 ) ;
#66660 = EDGE_CURVE ( 'NONE', #23509, #49868, #35465, .T. ) ;
#66661 = LINE ( 'NONE', #29172, #6840 ) ;
#66662 = EDGE_CURVE ( 'NONE', #12591, #43731, #36143, .T. ) ;
#66663 = VECTOR ( 'NONE', #58478, 1000.000000000000000 ) ;
#66664 = ORIENTED_EDGE ( 'NONE', *, *, #7903, .F. ) ;
#66666 = ORIENTED_EDGE ( 'NONE', *, *, #21024, .F. ) ;
#66665 = DIRECTION ( 'NONE',  ( -1.000000000000000000, 0.000000000000000000, 0.000000000000000000 ) ) ;
#66667 = EDGE_CURVE ( 'NONE', #2145, #47295, #36496, .T. ) ;
#66668 = DIRECTION ( 'NONE',  ( 0.000000000000000000, 0.000000000000000000, 1.000000000000000000 ) ) ;
#66669 = CARTESIAN_POINT ( 'NONE',  ( -9.722976262117258628, 6.817976262117182884, 26.00000000000000711 ) ) ;
#66670 = ORIENTED_EDGE ( 'NONE', *, *, #36265, .F. ) ;
#66671 = VECTOR ( 'NONE', #43163, 1000.000000000000000 ) ;
#66672 = VECTOR ( 'NONE', #12842, 1000.000000000000000 ) ;
#66673 = FACE_OUTER_BOUND ( 'NONE', #4669, .T. ) ;
#66674 = ORIENTED_EDGE ( 'NONE', *, *, #8631, .T. ) ;
#66675 = CARTESIAN_POINT ( 'NONE',  ( 289.7500000000001705, -42.24999999999996447, -26.75000000000008527 ) ) ;
#66676 = ORIENTED_EDGE ( 'NONE', *, *, #46240, .T. ) ;
#66677 = ORIENTED_EDGE ( 'NONE', *, *, #23665, .F. ) ;
#66678 = LINE ( 'NONE', #49396, #11444 ) ;
#66679 = DIRECTION ( 'NONE',  ( 0.000000000000000000, 0.000000000000000000, -1.000000000000000000 ) ) ;
#66680 = CARTESIAN_POINT ( 'NONE',  ( 8.249999999999996447, 8.250000000000001776, -5.000000000000000000 ) ) ;
#66681 = CARTESIAN_POINT ( 'NONE',  ( 7.250000000000005329, -7.249999999999998224, -13.50000000000000178 ) ) ;
#66682 = AXIS2_PLACEMENT_3D ( 'NONE', #29644, #46960, #56182 ) ;
#66683 = ORIENTED_EDGE ( 'NONE', *, *, #2016, .F. ) ;
#66684 = ORIENTED_EDGE ( 'NONE', *, *, #41424, .F. ) ;
#66685 = CARTESIAN_POINT ( 'NONE',  ( 49.00000000000000000, -21.00000000000000000, 13.86939075806900057 ) ) ;
#66686 = FACE_OUTER_BOUND ( 'NONE', #22954, .T. ) ;
#66687 = ORIENTED_EDGE ( 'NONE', *, *, #20536, .T. ) ;
#66688 = EDGE_LOOP ( 'NONE', ( #19570, #21049, #55675, #52196 ) ) ;
#66689 = ORIENTED_EDGE ( 'NONE', *, *, #64356, .F. ) ;
#66690 = DIRECTION ( 'NONE',  ( 0.000000000000000000, -0.7066873191085842887, -0.7075259945833242137 ) ) ;
#66692 = ORIENTED_EDGE ( 'NONE', *, *, #60739, .F. ) ;
#66691 = DIRECTION ( 'NONE',  ( -0.000000000000000000, -0.000000000000000000, -1.000000000000000000 ) ) ;
#66693 = LINE ( 'NONE', #40870, #34505 ) ;
#66694 = EDGE_CURVE ( 'NONE', #63027, #8802, #2762, .T. ) ;
#66695 = DIRECTION ( 'NONE',  ( 0.000000000000000000, 0.000000000000000000, 1.000000000000000000 ) ) ;
#66696 = ORIENTED_EDGE ( 'NONE', *, *, #31426, .T. ) ;
#66697 = EDGE_CURVE ( 'NONE', #36899, #13975, #52454, .T. ) ;
#66698 = CIRCLE ( 'NONE', #47540, 1.399999999999999245 ) ;
#66699 = ORIENTED_EDGE ( 'NONE', *, *, #2768, .F. ) ;
#66700 = ADVANCED_FACE ( 'NONE', ( #64095 ), #52791, .F. ) ;
#66701 = EDGE_CURVE ( 'NONE', #34737, #4189, #15644, .T. ) ;
#66702 = VECTOR ( 'NONE', #46141, 1000.000000000000000 ) ;
#66703 = VECTOR ( 'NONE', #13365, 1000.000000000000000 ) ;
#66704 = DIRECTION ( 'NONE',  ( -0.000000000000000000, -1.000000000000000000, -0.000000000000000000 ) ) ;
#66705 = DIRECTION ( 'NONE',  ( -1.000000000000000000, 0.000000000000000000, 0.000000000000000000 ) ) ;
#66706 = CARTESIAN_POINT ( 'NONE',  ( 11.78648345035337996, 4.173516549646518747, 455.0000000000000568 ) ) ;
#66707 = VECTOR ( 'NONE', #33709, 1000.000000000000000 ) ;
#66708 = CARTESIAN_POINT ( 'NONE',  ( -30.00000000000000000, -17.50000000000000000, 26.64999999999999858 ) ) ;
#66709 = FACE_OUTER_BOUND ( 'NONE', #28564, .T. ) ;
#66711 = VERTEX_POINT ( 'NONE', #27297 ) ;
#66710 = FACE_OUTER_BOUND ( 'NONE', #55062, .T. ) ;
#66712 = VERTEX_POINT ( 'NONE', #5393 ) ;
#66713 = DIRECTION ( 'NONE',  ( -0.000000000000000000, 0.000000000000000000, 1.000000000000000000 ) ) ;
#66714 = VECTOR ( 'NONE', #33508, 1000.000000000000000 ) ;
#66715 = DIRECTION ( 'NONE',  ( -1.836970198721029934E-16, 1.836970198721036344E-16, -1.000000000000000000 ) ) ;
#66716 = DIRECTION ( 'NONE',  ( 0.000000000000000000, 0.000000000000000000, 1.000000000000000000 ) ) ;
#66717 = CARTESIAN_POINT ( 'NONE',  ( 7.250000000000005329, 7.250000000000000888, -10.00000000000000000 ) ) ;
#66718 = ORIENTED_EDGE ( 'NONE', *, *, #5303, .F. ) ;
#66719 = CARTESIAN_POINT ( 'NONE',  ( 30.00000000000000000, -17.00000000000000000, 15.70499999999969809 ) ) ;
#66720 = CARTESIAN_POINT ( 'NONE',  ( -9.690000000000001279, 10.50000000000000000, -4.250000000000000000 ) ) ;
#66721 = SURFACE_SIDE_STYLE ('',( #1340 ) ) ;
#66722 = DIRECTION ( 'NONE',  ( 1.836970198721029934E-16, 1.836970198721010706E-16, -1.000000000000000000 ) ) ;
#66723 = CIRCLE ( 'NONE', #30605, 1.000000000000000000 ) ;
#66724 = FACE_BOUND ( 'NONE', #53788, .T. ) ;
#66725 = DIRECTION ( 'NONE',  ( 0.000000000000000000, 0.000000000000000000, -1.000000000000000000 ) ) ;
#66726 = CARTESIAN_POINT ( 'NONE',  ( 29.50000000000000355, -15.97213595500069871, 14.50000000000000000 ) ) ;
#66727 = EDGE_LOOP ( 'NONE', ( #30547, #44920, #53093, #16436 ) ) ;
#66728 = DIRECTION ( 'NONE',  ( -1.836970198721029934E-16, 1.836970198721036344E-16, -1.000000000000000000 ) ) ;
#66729 = DIRECTION ( 'NONE',  ( -0.000000000000000000, -0.000000000000000000, -1.000000000000000000 ) ) ;
#66730 = ORIENTED_EDGE ( 'NONE', *, *, #53027, .T. ) ;
#66731 = FACE_BOUND ( 'NONE', #18391, .T. ) ;
#66732 = DIRECTION ( 'NONE',  ( -1.836970198721029934E-16, 1.836970198721036590E-16, -1.000000000000000000 ) ) ;
#66733 = DIRECTION ( 'NONE',  ( -0.000000000000000000, 1.000000000000000000, 0.000000000000000000 ) ) ;
#66734 = CARTESIAN_POINT ( 'NONE',  ( 5.257023737882819070, -5.257023737882825287, 54.00000000000000711 ) ) ;
#66735 = DIRECTION ( 'NONE',  ( 0.6414496315691526895, 0.7671651518153038696, 2.587583378555111534E-16 ) ) ;
#66736 = EDGE_CURVE ( 'NONE', #14932, #22707, #36641, .T. ) ;
#66737 = AXIS2_PLACEMENT_3D ( 'NONE', #20631, #36923, #47855 ) ;
#66738 = EDGE_LOOP ( 'NONE', ( #66208, #37179, #53734, #23265 ) ) ;
#66739 = DIRECTION ( 'NONE',  ( 0.000000000000000000, 1.000000000000000000, 0.000000000000000000 ) ) ;
#66740 = VECTOR ( 'NONE', #26205, 1000.000000000000000 ) ;
#66741 = ORIENTED_EDGE ( 'NONE', *, *, #65904, .T. ) ;
#66742 = ADVANCED_FACE ( 'NONE', ( #48861 ), #421, .F. ) ;
#66743 = LINE ( 'NONE', #2738, #57060 ) ;
#66744 = VERTEX_POINT ( 'NONE', #12048 ) ;
#66745 = AXIS2_PLACEMENT_3D ( 'NONE', #2040, #1349, #44124 ) ;
#66746 = DIRECTION ( 'NONE',  ( -0.000000000000000000, -0.000000000000000000, 1.000000000000000000 ) ) ;
#66747 = AXIS2_PLACEMENT_3D ( 'NONE', #8921, #51722, #20585 ) ;
#66748 = CIRCLE ( 'NONE', #50960, 24.99999999998794920 ) ;
#66749 = DIRECTION ( 'NONE',  ( 8.951101527228104953E-17, -1.000000000000000000, 0.000000000000000000 ) ) ;
#66750 = DIRECTION ( 'NONE',  ( 1.000000000000000000, 0.000000000000000000, 0.000000000000000000 ) ) ;
#66751 = VERTEX_POINT ( 'NONE', #49546 ) ;
#66752 = ORIENTED_EDGE ( 'NONE', *, *, #44828, .T. ) ;
#66753 = CARTESIAN_POINT ( 'NONE',  ( -11.50000000000000000, -11.70000000000000284, 11.00000000000000000 ) ) ;
#66755 = ORIENTED_EDGE ( 'NONE', *, *, #68038, .F. ) ;
#66754 = EDGE_CURVE ( 'NONE', #28918, #67361, #30989, .T. ) ;
#66756 = CONICAL_SURFACE ( 'NONE', #48713, 2.000000000000001776, 0.7853981633974503884 ) ;
#66757 = ORIENTED_EDGE ( 'NONE', *, *, #21906, .T. ) ;
#66758 = EDGE_CURVE ( 'NONE', #8276, #46298, #60144, .T. ) ;
#66759 = CARTESIAN_POINT ( 'NONE',  ( -6.350872789121373430, -6.836383711242974393, 26.00000000000000711 ) ) ;
#66760 = FACE_OUTER_BOUND ( 'NONE', #68135, .T. ) ;
#66761 = CARTESIAN_POINT ( 'NONE',  ( 25.57999999999999829, 0.000000000000000000, 0.000000000000000000 ) ) ;
#66762 = ORIENTED_EDGE ( 'NONE', *, *, #46700, .T. ) ;
#66763 = DIRECTION ( 'NONE',  ( -1.000000000000000000, 1.261617073437657735E-14, 4.635105932205236432E-30 ) ) ;
#66765 = LINE ( 'NONE', #61445, #29968 ) ;
#66764 = DIRECTION ( 'NONE',  ( 0.000000000000000000, 0.000000000000000000, 1.000000000000000000 ) ) ;
#66766 = ORIENTED_EDGE ( 'NONE', *, *, #18664, .T. ) ;
#66768 = VERTEX_POINT ( 'NONE', #54858 ) ;
#66767 = DIRECTION ( 'NONE',  ( 0.000000000000000000, 0.000000000000000000, -1.000000000000000000 ) ) ;
#66769 = ORIENTED_EDGE ( 'NONE', *, *, #56117, .T. ) ;
#66770 = CYLINDRICAL_SURFACE ( 'NONE', #9589, 4.000000000000000000 ) ;
#66771 = ORIENTED_EDGE ( 'NONE', *, *, #30666, .F. ) ;
#66772 = DIRECTION ( 'NONE',  ( 0.000000000000000000, 0.000000000000000000, 1.000000000000000000 ) ) ;
#66773 = DIRECTION ( 'NONE',  ( 1.000000000000000000, 0.000000000000000000, 0.000000000000000000 ) ) ;
#66774 = VECTOR ( 'NONE', #37336, 1000.000000000000000 ) ;
#66775 = ORIENTED_EDGE ( 'NONE', *, *, #55803, .F. ) ;
#66776 = ORIENTED_EDGE ( 'NONE', *, *, #66890, .T. ) ;
#66777 = CARTESIAN_POINT ( 'NONE',  ( 275.0000000000000000, -23.50007830495750127, -12.28007262201345995 ) ) ;
#66778 = CARTESIAN_POINT ( 'NONE',  ( -9.547976262117300550, -8.144523737882753522, 26.00000000000000000 ) ) ;
#66779 = ORIENTED_EDGE ( 'NONE', *, *, #4347, .T. ) ;
#66780 = ADVANCED_FACE ( 'NONE', ( #55199 ), #6421, .T. ) ;
#66781 = PLANE ( 'NONE',  #25691 ) ;
#66782 = CARTESIAN_POINT ( 'NONE',  ( 7.250000000000005329, 7.250000000000000888, -13.00000000000000178 ) ) ;
#66783 = FACE_BOUND ( 'NONE', #49315, .T. ) ;
#66784 = AXIS2_PLACEMENT_3D ( 'NONE', #22302, #4648, #26211 ) ;
#66785 = ORIENTED_EDGE ( 'NONE', *, *, #20499, .F. ) ;
#66786 = AXIS2_PLACEMENT_3D ( 'NONE', #65426, #16284, #37861 ) ;
#66787 = CARTESIAN_POINT ( 'NONE',  ( 84.77321854994620765, 47.95351654967443977, 29.00000000000000000 ) ) ;
#66788 = CARTESIAN_POINT ( 'NONE',  ( -8.130476262117324993, -9.562023737882769936, 54.00000000000000711 ) ) ;
#66790 = ORIENTED_EDGE ( 'NONE', *, *, #39087, .T. ) ;
#66789 = CYLINDRICAL_SURFACE ( 'NONE', #44234, 2.204799999999999649 ) ;
#66792 = VERTEX_POINT ( 'NONE', #27631 ) ;
#66791 = LINE ( 'NONE', #40626, #45558 ) ;
#66793 = CARTESIAN_POINT ( 'NONE',  ( 4.622483450353394474, 3.593516549646586622, 455.0000000000000568 ) ) ;
#66794 = ADVANCED_FACE ( 'NONE', ( #38256 ), #80, .F. ) ;
#66795 = CARTESIAN_POINT ( 'NONE',  ( 3.664523737882819709, 10.30047626211720413, 54.00000000000000711 ) ) ;
#66796 = LINE ( 'NONE', #2796, #41443 ) ;
#66797 = CIRCLE ( 'NONE', #12581, 0.1749999999999998224 ) ;
#66798 = CIRCLE ( 'NONE', #207, 0.1749999999999998224 ) ;
#66799 = DIRECTION ( 'NONE',  ( 1.000000000000000000, -6.308085367188447236E-15, -2.317552966102676720E-30 ) ) ;
#66800 = ADVANCED_FACE ( 'NONE', ( #65467 ), #16328, .F. ) ;
#66801 = LINE ( 'NONE', #18352, #15006 ) ;
#66802 = VERTEX_POINT ( 'NONE', #37558 ) ;
#66803 = DIRECTION ( 'NONE',  ( -0.3479852726768751237, 0.000000000000000000, -0.9375000000000004441 ) ) ;
#66804 = DIRECTION ( 'NONE',  ( 1.000000000000000000, -0.000000000000000000, 0.000000000000000000 ) ) ;
#66805 = DIRECTION ( 'NONE',  ( 1.000000000000000000, -2.990116172375847553E-15, -1.836970198721035357E-16 ) ) ;
#66807 = EDGE_LOOP ( 'NONE', ( #26061, #54980, #9696, #2950 ) ) ;
#66806 = DIRECTION ( 'NONE',  ( 0.000000000000000000, -1.000000000000000000, 0.000000000000000000 ) ) ;
#66808 = FACE_OUTER_BOUND ( 'NONE', #34272, .T. ) ;
#66809 = CARTESIAN_POINT ( 'NONE',  ( 83.77321854994620765, 47.95351654967443977, 26.00000000000000355 ) ) ;
#66810 = VECTOR ( 'NONE', #49527, 1000.000000000000000 ) ;
#66811 = ORIENTED_EDGE ( 'NONE', *, *, #32366, .F. ) ;
#66812 = DIRECTION ( 'NONE',  ( -0.000000000000000000, -1.000000000000000000, -0.000000000000000000 ) ) ;
#66813 = DIRECTION ( 'NONE',  ( -1.000000000000000000, 0.000000000000000000, 0.000000000000000000 ) ) ;
#66814 = VERTEX_POINT ( 'NONE', #54517 ) ;
#66815 = LINE ( 'NONE', #28301, #35716 ) ;
#66816 = PLANE ( 'NONE',  #54924 ) ;
#66817 = CARTESIAN_POINT ( 'NONE',  ( -7.450000000000001954, 7.250000000000000000, -13.50000000000000178 ) ) ;
#66818 = CARTESIAN_POINT ( 'NONE',  ( 8.250000000000005329, 7.250000000000000888, -13.50000000000000178 ) ) ;
#66819 = EDGE_CURVE ( 'NONE', #31121, #2764, #37905, .T. ) ;
#66820 = CARTESIAN_POINT ( 'NONE',  ( -9.404046420174113408, -1.866219381641437636, 455.0000000000000568 ) ) ;
#66821 = ORIENTED_EDGE ( 'NONE', *, *, #59173, .T. ) ;
#66822 = AXIS2_PLACEMENT_3D ( 'NONE', #55663, #51402, #66959 ) ;
#66823 = EDGE_CURVE ( 'NONE', #57134, #18694, #27983, .T. ) ;
#66824 = CARTESIAN_POINT ( 'NONE',  ( 30.00000000000000000, -11.85423089348099879, 9.852125413066602277 ) ) ;
#66825 = ORIENTED_EDGE ( 'NONE', *, *, #57355, .T. ) ;
#66826 = ADVANCED_FACE ( 'NONE', ( #783 ), #59469, .T. ) ;
#66827 = VERTEX_POINT ( 'NONE', #22674 ) ;
#66828 = DIRECTION ( 'NONE',  ( 0.000000000000000000, 1.000000000000000000, 0.000000000000000000 ) ) ;
#66829 = ADVANCED_FACE ( 'NONE', ( #44223 ), #65803, .T. ) ;
#66830 = AXIS2_PLACEMENT_3D ( 'NONE', #55101, #6645, #44810 ) ;
#66831 = EDGE_CURVE ( 'NONE', #56086, #58466, #17356, .T. ) ;
#66832 = DIRECTION ( 'NONE',  ( 1.000000000000000000, -0.000000000000000000, 0.000000000000000000 ) ) ;
#66834 = DIRECTION ( 'NONE',  ( 0.000000000000000000, 0.000000000000000000, 1.000000000000000000 ) ) ;
#66833 = CARTESIAN_POINT ( 'NONE',  ( 49.00000000000000000, -0.7500000000000000000, 3.929058411375430104 ) ) ;
#66835 = ORIENTED_EDGE ( 'NONE', *, *, #66509, .F. ) ;
#66836 = ADVANCED_FACE ( 'NONE', ( #64773 ), #60491, .T. ) ;
#66837 = ORIENTED_EDGE ( 'NONE', *, *, #24363, .F. ) ;
#66838 = CIRCLE ( 'NONE', #54454, 0.2000000000000005107 ) ;
#66839 = CARTESIAN_POINT ( 'NONE',  ( -6.642976262117329611, -10.31452373788278365, 26.00000000000000000 ) ) ;
#66841 = ORIENTED_EDGE ( 'NONE', *, *, #1057, .F. ) ;
#66840 = EDGE_CURVE ( 'NONE', #40034, #5797, #67188, .T. ) ;
#66842 = DIRECTION ( 'NONE',  ( 0.000000000000000000, -3.673940397442059868E-16, 1.000000000000000000 ) ) ;
#66843 = CARTESIAN_POINT ( 'NONE',  ( -11.07551654964676935, -9.804883450353326424, 195.0000000000000284 ) ) ;
#66844 = LINE ( 'NONE', #50932, #24060 ) ;
#66845 = VECTOR ( 'NONE', #65483, 1000.000000000000000 ) ;
#66846 = LINE ( 'NONE', #2498, #10800 ) ;
#66848 = DIRECTION ( 'NONE',  ( 0.000000000000000000, 0.7071067811865474617, 0.7071067811865474617 ) ) ;
#66847 = PLANE ( 'NONE',  #69372 ) ;
#66849 = EDGE_LOOP ( 'NONE', ( #8255, #16085, #25185, #59791 ) ) ;
#66851 = ORIENTED_EDGE ( 'NONE', *, *, #59944, .T. ) ;
#66850 = DIRECTION ( 'NONE',  ( 1.836970198721029934E-16, 1.836970198721010706E-16, -1.000000000000000000 ) ) ;
#66852 = ORIENTED_EDGE ( 'NONE', *, *, #37612, .T. ) ;
#66853 = ORIENTED_EDGE ( 'NONE', *, *, #46232, .T. ) ;
#66854 = AXIS2_PLACEMENT_3D ( 'NONE', #31025, #53649, #53308 ) ;
#66855 = CARTESIAN_POINT ( 'NONE',  ( -5.380658396643234198, 4.734785091273867152, 455.0000000000000568 ) ) ;
#66856 = LINE ( 'NONE', #45634, #28178 ) ;
#66857 = MANIFOLD_SOLID_BREP ( 'LPattern1[3]', #6939 ) ;
#66858 = EDGE_CURVE ( 'NONE', #46196, #19320, #24759, .T. ) ;
#66859 = ORIENTED_EDGE ( 'NONE', *, *, #47102, .F. ) ;
#66860 = ORIENTED_EDGE ( 'NONE', *, *, #12770, .F. ) ;
#66861 = VECTOR ( 'NONE', #15548, 1000.000000000000000 ) ;
#66862 = DIRECTION ( 'NONE',  ( 1.000000000000000000, 0.000000000000000000, 0.000000000000000000 ) ) ;
#66863 = DIRECTION ( 'NONE',  ( -1.794541526872559352E-16, -1.000000000000000000, 0.000000000000000000 ) ) ;
#66864 = ORIENTED_EDGE ( 'NONE', *, *, #47627, .F. ) ;
#66865 = ADVANCED_FACE ( 'NONE', ( #13791 ), #50586, .F. ) ;
#66866 = EDGE_LOOP ( 'NONE', ( #12748, #58897, #55975, #27851 ) ) ;
#66867 = FACE_BOUND ( 'NONE', #33932, .T. ) ;
#66868 = CARTESIAN_POINT ( 'NONE',  ( 39.90000000000000568, 16.96999999999999886, -21.00000000000000000 ) ) ;
#66869 = ORIENTED_EDGE ( 'NONE', *, *, #13263, .F. ) ;
#66870 = CARTESIAN_POINT ( 'NONE',  ( -7.250000000000000888, 7.250000000000001776, -24.00000000000000000 ) ) ;
#66871 = CARTESIAN_POINT ( 'NONE',  ( 6.006483450353409914, 8.198316549646580853, 455.0000000000000568 ) ) ;
#66872 = ORIENTED_EDGE ( 'NONE', *, *, #28672, .T. ) ;
#66873 = ORIENTED_EDGE ( 'NONE', *, *, #55887, .F. ) ;
#66874 = CARTESIAN_POINT ( 'NONE',  ( -6.817976262117261044, 9.722976262117182245, 54.00000000000000711 ) ) ;
#66875 = FACE_OUTER_BOUND ( 'NONE', #58096, .T. ) ;
#66876 = DIRECTION ( 'NONE',  ( -1.000000000000000000, 0.000000000000000000, 0.000000000000000000 ) ) ;
#66877 = CIRCLE ( 'NONE', #60129, 4.500000000000190958 ) ;
#66878 = LINE ( 'NONE', #25162, #65140 ) ;
#66879 = LINE ( 'NONE', #61570, #28956 ) ;
#66880 = CARTESIAN_POINT ( 'NONE',  ( -4.135079735113208699, -3.677663764522613121, 54.00000000000000711 ) ) ;
#66881 = ADVANCED_FACE ( 'NONE', ( #7086 ), #23702, .F. ) ;
#66882 = CARTESIAN_POINT ( 'NONE',  ( 14.50000000000000000, -42.50000000000000000, -15.10000000000000142 ) ) ;
#66883 = CONICAL_SURFACE ( 'NONE', #57862, 1.621000000000000885, 0.7853981633974518317 ) ;
#66884 = ORIENTED_EDGE ( 'NONE', *, *, #42332, .F. ) ;
#66885 = CARTESIAN_POINT ( 'NONE',  ( 7.450000000000006395, 7.250000000000000888, -16.50000000000000000 ) ) ;
#66887 = VERTEX_POINT ( 'NONE', #60833 ) ;
#66886 = DIRECTION ( 'NONE',  ( 0.000000000000000000, 0.000000000000000000, 1.000000000000000000 ) ) ;
#66888 = DIRECTION ( 'NONE',  ( -1.000000000000000000, 0.000000000000000000, 0.000000000000000000 ) ) ;
#66889 = DIRECTION ( 'NONE',  ( -0.000000000000000000, -0.000000000000000000, 1.000000000000000000 ) ) ;
#66890 = EDGE_CURVE ( 'NONE', #48961, #13793, #39951, .T. ) ;
#66891 = LINE ( 'NONE', #55947, #7649 ) ;
#66892 = ADVANCED_FACE ( 'NONE', ( #34298 ), #19101, .F. ) ;
#66893 = CARTESIAN_POINT ( 'NONE',  ( 15.50000000000000000, -5.000000000000000000, 22.50000000000000000 ) ) ;
#66894 = DIRECTION ( 'NONE',  ( 0.000000000000000000, 0.000000000000000000, -1.000000000000000000 ) ) ;
#66895 = EDGE_CURVE ( 'NONE', #31751, #19212, #2483, .T. ) ;
#66896 = ORIENTED_EDGE ( 'NONE', *, *, #15181, .T. ) ;
#66897 = EDGE_CURVE ( 'NONE', #2475, #67892, #30058, .T. ) ;
#66898 = EDGE_CURVE ( 'NONE', #46985, #14663, #35002, .T. ) ;
#66899 = ORIENTED_EDGE ( 'NONE', *, *, #68299, .T. ) ;
#66900 = FACE_OUTER_BOUND ( 'NONE', #53210, .T. ) ;
#66901 = CARTESIAN_POINT ( 'NONE',  ( 7.450000000000003730, -7.249999999999997335, -18.00000000000000000 ) ) ;
#66902 = EDGE_CURVE ( 'NONE', #50419, #28489, #14017, .T. ) ;
#66903 = CARTESIAN_POINT ( 'NONE',  ( 7.450000000000003730, -7.249999999999997335, -20.50000000000000000 ) ) ;
#66904 = VECTOR ( 'NONE', #2235, 1000.000000000000000 ) ;
#66905 = EDGE_LOOP ( 'NONE', ( #28768, #68083, #9642, #39687 ) ) ;
#66906 = ADVANCED_FACE ( 'NONE', ( #51273 ), #18046, .F. ) ;
#66907 = CYLINDRICAL_SURFACE ( 'NONE', #21454, 1.000000000000000000 ) ;
#66908 = EDGE_LOOP ( 'NONE', ( #2264, #29825, #27227, #14380 ) ) ;
#66909 = ORIENTED_EDGE ( 'NONE', *, *, #345, .F. ) ;
#66910 = EDGE_CURVE ( 'NONE', #62095, #3656, #44926, .T. ) ;
#66911 = AXIS2_PLACEMENT_3D ( 'NONE', #1265, #48667, #49374 ) ;
#66912 = DIRECTION ( 'NONE',  ( 0.000000000000000000, 0.000000000000000000, -1.000000000000000000 ) ) ;
#66913 = CARTESIAN_POINT ( 'NONE',  ( -4.173516549646792306, -12.00648345035339837, 195.0000000000000284 ) ) ;
#66914 = ORIENTED_EDGE ( 'NONE', *, *, #18813, .F. ) ;
#66915 = LINE ( 'NONE', #13175, #26542 ) ;
#66916 = AXIS2_PLACEMENT_3D ( 'NONE', #58014, #31161, #13826 ) ;
#66917 = DIRECTION ( 'NONE',  ( -0.000000000000000000, 1.000000000000000000, -0.000000000000000000 ) ) ;
#66918 = DIRECTION ( 'NONE',  ( 0.000000000000000000, 0.000000000000000000, -1.000000000000000000 ) ) ;
#66919 = VERTEX_POINT ( 'NONE', #13086 ) ;
#66920 = EDGE_CURVE ( 'NONE', #29528, #51208, #17455, .T. ) ;
#66921 = ORIENTED_EDGE ( 'NONE', *, *, #8042, .T. ) ;
#66923 = ORIENTED_EDGE ( 'NONE', *, *, #18153, .T. ) ;
#66922 = CARTESIAN_POINT ( 'NONE',  ( -1.077516549646670541, 11.33351654964656596, 455.0000000000000568 ) ) ;
#66925 = EDGE_LOOP ( 'NONE', ( #2739, #53684, #40049, #59718 ) ) ;
#66924 = EDGE_CURVE ( 'NONE', #42177, #135, #23056, .T. ) ;
#66926 = LINE ( 'NONE', #3639, #13398 ) ;
#66927 = AXIS2_PLACEMENT_3D ( 'NONE', #54555, #1476, #65840 ) ;
#66928 = CARTESIAN_POINT ( 'NONE',  ( -6.835476262117333057, -10.31452373788278543, 54.00000000000000711 ) ) ;
#66929 = CARTESIAN_POINT ( 'NONE',  ( -10.49297626211732748, -9.795823737882738413, 54.00000000000000711 ) ) ;
#66930 = DIRECTION ( 'NONE',  ( 1.000000000000000000, 0.000000000000000000, 0.000000000000000000 ) ) ;
#66931 = CARTESIAN_POINT ( 'NONE',  ( 4.456444791733522252E-16, 7.450000000000002842, -16.50000000000000000 ) ) ;
#66932 = VECTOR ( 'NONE', #54596, 1000.000000000000000 ) ;
#66933 = ORIENTED_EDGE ( 'NONE', *, *, #33987, .F. ) ;
#66934 = EDGE_CURVE ( 'NONE', #3912, #65820, #58691, .T. ) ;
#66935 = VERTEX_POINT ( 'NONE', #9913 ) ;
#66936 = ORIENTED_EDGE ( 'NONE', *, *, #50688, .T. ) ;
#66937 = ORIENTED_EDGE ( 'NONE', *, *, #53948, .T. ) ;
#66938 = CARTESIAN_POINT ( 'NONE',  ( -7.955476262117326947, -9.737023737882770646, 54.00000000000000711 ) ) ;
#66939 = AXIS2_PLACEMENT_3D ( 'NONE', #33314, #28009, #17382 ) ;
#66940 = FACE_OUTER_BOUND ( 'NONE', #34379, .T. ) ;
#66941 = CARTESIAN_POINT ( 'NONE',  ( 28.00000000000000000, -17.50000000000000000, 20.05051025721700242 ) ) ;
#66942 = SHAPE_REPRESENTATION_RELATIONSHIP ( 'NONE' , 'NONE' ,  #14183, #43586 ) ;
#66943 = CARTESIAN_POINT ( 'NONE',  ( -15.70366306705060033, -0.2717122460100995229, 23.82579074638835692 ) ) ;
#66944 = VERTEX_POINT ( 'NONE', #68241 ) ;
#66945 = ORIENTED_EDGE ( 'NONE', *, *, #47526, .T. ) ;
#66946 = VERTEX_POINT ( 'NONE', #20504 ) ;
#66947 = LINE ( 'NONE', #19217, #66672 ) ;
#66948 = VERTEX_POINT ( 'NONE', #41008 ) ;
#66949 = ORIENTED_EDGE ( 'NONE', *, *, #41959, .T. ) ;
#66950 = EDGE_LOOP ( 'NONE', ( #48538, #57812, #45134, #9970 ) ) ;
#66951 = EDGE_CURVE ( 'NONE', #31022, #48227, #14142, .T. ) ;
#66952 = ORIENTED_EDGE ( 'NONE', *, *, #21777, .T. ) ;
#66953 = DIRECTION ( 'NONE',  ( -1.000000000000000000, 0.000000000000000000, 0.000000000000000000 ) ) ;
#66955 = ORIENTED_EDGE ( 'NONE', *, *, #42269, .T. ) ;
#66954 = FACE_OUTER_BOUND ( 'NONE', #69434, .T. ) ;
#66956 = EDGE_CURVE ( 'NONE', #69324, #23983, #4261, .T. ) ;
#66957 = LINE ( 'NONE', #39392, #7461 ) ;
#66959 = DIRECTION ( 'NONE',  ( 1.000000000000000000, 0.000000000000000000, 0.000000000000000000 ) ) ;
#66958 = VECTOR ( 'NONE', #64786, 1000.000000000000000 ) ;
#66960 = DIRECTION ( 'NONE',  ( -0.000000000000000000, 3.673940397442059868E-16, -1.000000000000000000 ) ) ;
#66961 = ADVANCED_FACE ( 'NONE', ( #31480 ), #15211, .F. ) ;
#66963 = VERTEX_POINT ( 'NONE', #14503 ) ;
#66962 = LINE ( 'NONE', #34082, #2990 ) ;
#66965 = VERTEX_POINT ( 'NONE', #53047 ) ;
#66964 = CIRCLE ( 'NONE', #15049, 2.458500000000000796 ) ;
#66966 = CIRCLE ( 'NONE', #16159, 3.500000000000000444 ) ;
#66967 = EDGE_CURVE ( 'NONE', #54114, #42963, #26169, .T. ) ;
#66968 = CARTESIAN_POINT ( 'NONE',  ( -11.77351654964670935, 4.393516549646602876, 455.0000000000000568 ) ) ;
#66969 = CARTESIAN_POINT ( 'NONE',  ( 11.00000000000000000, -9.199999999999999289, -12.69999999999986073 ) ) ;
#66970 = CYLINDRICAL_SURFACE ( 'NONE', #58672, 0.1749999999999989342 ) ;
#66971 =( GEOMETRIC_REPRESENTATION_CONTEXT ( 3 ) GLOBAL_UNCERTAINTY_ASSIGNED_CONTEXT ( ( #68457 ) ) GLOBAL_UNIT_ASSIGNED_CONTEXT ( ( #62185, #62532, #29657 ) ) REPRESENTATION_CONTEXT ( 'NONE', 'WORKASPACE' ) );
#66972 = VECTOR ( 'NONE', #28204, 1000.000000000000000 ) ;
#66973 = ADVANCED_FACE ( 'NONE', ( #10249 ), #69291, .F. ) ;
#66974 = ORIENTED_EDGE ( 'NONE', *, *, #42728, .F. ) ;
#66975 = DIRECTION ( 'NONE',  ( 1.261617073437657577E-14, 1.000000000000000000, 0.000000000000000000 ) ) ;
#66976 = DIRECTION ( 'NONE',  ( 1.836970198721029934E-16, 1.836970198721010706E-16, -1.000000000000000000 ) ) ;
#66977 = CARTESIAN_POINT ( 'NONE',  ( 15.50000000000000000, -0.4000000000005274892, 25.79999999999946780 ) ) ;
#66978 = VERTEX_POINT ( 'NONE', #36061 ) ;
#66979 = EDGE_CURVE ( 'NONE', #15537, #9996, #20851, .T. ) ;
#66980 = CARTESIAN_POINT ( 'NONE',  ( 8.711985858128686644, 8.079219948824833963, 54.00000000000000711 ) ) ;
#66981 = EDGE_CURVE ( 'NONE', #32501, #25255, #8844, .T. ) ;
#66982 = DIRECTION ( 'NONE',  ( 0.000000000000000000, 1.000000000000000000, 0.000000000000000000 ) ) ;
#66983 = PLANE ( 'NONE',  #37073 ) ;
#66984 = VECTOR ( 'NONE', #38594, 1000.000000000000000 ) ;
#66985 = EDGE_CURVE ( 'NONE', #12173, #37776, #53617, .T. ) ;
#66986 = ADVANCED_FACE ( 'NONE', ( #53393 ), #42421, .F. ) ;
#66987 = ORIENTED_EDGE ( 'NONE', *, *, #46392, .F. ) ;
#66988 = DIRECTION ( 'NONE',  ( -1.836970198721029934E-16, 1.836970198721036590E-16, -1.000000000000000000 ) ) ;
#66989 = DIRECTION ( 'NONE',  ( 0.000000000000000000, 0.7071067811865474617, -0.7071067811865474617 ) ) ;
#66990 = VECTOR ( 'NONE', #60376, 1000.000000000000000 ) ;
#66991 = CARTESIAN_POINT ( 'NONE',  ( -1.853252480934882707, -9.417013320880883498, 455.0000000000000568 ) ) ;
#66992 = CARTESIAN_POINT ( 'NONE',  ( 6.849523737882818430, 10.49297626211719603, 54.00000000000000711 ) ) ;
#66993 = EDGE_CURVE ( 'NONE', #22404, #61284, #26510, .T. ) ;
#66994 = EDGE_LOOP ( 'NONE', ( #7160, #36318, #62998, #69914 ) ) ;
#66995 = CARTESIAN_POINT ( 'NONE',  ( -5.242976262117259978, 5.242976262117182706, 26.00000000000000711 ) ) ;
#66996 = DIRECTION ( 'NONE',  ( -1.000000000000000000, 0.000000000000000000, -0.000000000000000000 ) ) ;
#66997 = CARTESIAN_POINT ( 'NONE',  ( 3.857023737882817827, 9.897976262117204271, 54.00000000000000711 ) ) ;
#66998 = DIRECTION ( 'NONE',  ( -1.000000000000000000, 0.000000000000000000, 0.000000000000000000 ) ) ;
#66999 = DIRECTION ( 'NONE',  ( -1.000000000000000000, -1.084202172485504434E-16, 0.000000000000000000 ) ) ;
#67000 = ORIENTED_EDGE ( 'NONE', *, *, #49831, .T. ) ;
#67001 = CARTESIAN_POINT ( 'NONE',  ( -17.24945551514599984, -15.50000000000000000, -25.53140320652400064 ) ) ;
#67002 = PLANE ( 'NONE',  #38458 ) ;
#67003 = CARTESIAN_POINT ( 'NONE',  ( 10.20488345035338007, -11.08848345035349325, 455.0000000000000568 ) ) ;
#67004 = DIRECTION ( 'NONE',  ( 1.000000000000000000, -0.000000000000000000, -0.000000000000000000 ) ) ;
#67005 = DIRECTION ( 'NONE',  ( 0.000000000000000000, 0.7071067811865474617, 0.7071067811865474617 ) ) ;
#67006 = EDGE_CURVE ( 'NONE', #19038, #1462, #33317, .T. ) ;
#67007 = VERTEX_POINT ( 'NONE', #25109 ) ;
#67009 = ORIENTED_EDGE ( 'NONE', *, *, #37981, .F. ) ;
#67008 = CARTESIAN_POINT ( 'NONE',  ( 0.000000000000000000, -0.7500000000000000000, 0.000000000000000000 ) ) ;
#67010 = EDGE_CURVE ( 'NONE', #41893, #68810, #46667, .T. ) ;
#67011 = VECTOR ( 'NONE', #11013, 1000.000000000000000 ) ;
#67012 = VECTOR ( 'NONE', #8493, 1000.000000000000000 ) ;
#67013 = DIRECTION ( 'NONE',  ( -1.000000000000000000, 0.000000000000000000, 0.000000000000000000 ) ) ;
#67014 = FACE_OUTER_BOUND ( 'NONE', #52100, .T. ) ;
#67015 = VERTEX_POINT ( 'NONE', #15573 ) ;
#67016 = VECTOR ( 'NONE', #23267, 1000.000000000000000 ) ;
#67017 = VECTOR ( 'NONE', #44732, 1000.000000000000000 ) ;
#67018 = DIRECTION ( 'NONE',  ( 0.000000000000000000, 0.000000000000000000, -1.000000000000000000 ) ) ;
#67019 = VECTOR ( 'NONE', #69050, 1000.000000000000000 ) ;
#67020 = ORIENTED_EDGE ( 'NONE', *, *, #28026, .F. ) ;
#67021 = CARTESIAN_POINT ( 'NONE',  ( -14.24999999999999822, -0.3152037684892585179, -22.74589050208021135 ) ) ;
#67023 = ORIENTED_EDGE ( 'NONE', *, *, #33674, .T. ) ;
#67022 = VECTOR ( 'NONE', #2582, 1000.000000000000000 ) ;
#67024 = AXIS2_PLACEMENT_3D ( 'NONE', #23858, #39076, #55687 ) ;
#67025 = VERTEX_POINT ( 'NONE', #37130 ) ;
#67026 = DIRECTION ( 'NONE',  ( -0.000000000000000000, 1.000000000000000000, -0.000000000000000000 ) ) ;
#67027 = CARTESIAN_POINT ( 'NONE',  ( 7.450000000000004619, -1.336933437520057563E-15, -16.50000000000000000 ) ) ;
#67028 = DIRECTION ( 'NONE',  ( -0.7671651518153128624, -0.6414496315691420314, 2.309356642089219057E-17 ) ) ;
#67029 = DIRECTION ( 'NONE',  ( -1.836970198721029934E-16, -1.836970198721010706E-16, 1.000000000000000000 ) ) ;
#67030 = ORIENTED_EDGE ( 'NONE', *, *, #54846, .F. ) ;
#67031 = VERTEX_POINT ( 'NONE', #9202 ) ;
#67032 = FACE_OUTER_BOUND ( 'NONE', #5067, .T. ) ;
#67033 = CARTESIAN_POINT ( 'NONE',  ( 181.4833316329832940, 5.000000000000000000, 316.5239988703752942 ) ) ;
#67034 = EDGE_LOOP ( 'NONE', ( #9983, #66624, #44993, #55977 ) ) ;
#67035 = ORIENTED_EDGE ( 'NONE', *, *, #57874, .F. ) ;
#67036 = EDGE_LOOP ( 'NONE', ( #49809, #39452, #37423, #21569 ) ) ;
#67037 = PLANE ( 'NONE',  #30505 ) ;
#67039 = VERTEX_POINT ( 'NONE', #30767 ) ;
#67038 = CARTESIAN_POINT ( 'NONE',  ( -9.547976262117217061, -2.369523737882723857, 26.00000000000000711 ) ) ;
#67040 = B_SPLINE_CURVE_WITH_KNOTS ( 'NONE', 3,
 ( #56692, #13555, #36167, #8594, #66943, #3297 ),
 .UNSPECIFIED., .F., .F.,
 ( 4, 2, 4 ),
 ( 0.0002380763768113913770, 0.7291065797294570272, 1.457975083082102774 ),
 .UNSPECIFIED. ) ;
#67041 = EDGE_CURVE ( 'NONE', #17336, #29997, #43453, .T. ) ;
#67042 = DIRECTION ( 'NONE',  ( -0.000000000000000000, -0.000000000000000000, -1.000000000000000000 ) ) ;
#67043 = DIRECTION ( 'NONE',  ( -1.000000000000000000, 0.000000000000000000, 0.000000000000000000 ) ) ;
#67044 = VERTEX_POINT ( 'NONE', #53738 ) ;
#67045 = VECTOR ( 'NONE', #66647, 1000.000000000000000 ) ;
#67046 = EDGE_CURVE ( 'NONE', #24537, #67547, #64343, .T. ) ;
#67047 = VERTEX_POINT ( 'NONE', #69656 ) ;
#67048 = EDGE_CURVE ( 'NONE', #10751, #10538, #38513, .T. ) ;
#67049 = EDGE_CURVE ( 'NONE', #23968, #16718, #31045, .T. ) ;
#67050 = DIRECTION ( 'NONE',  ( 0.000000000000000000, -3.673940397442059868E-16, 1.000000000000000000 ) ) ;
#67051 = CARTESIAN_POINT ( 'NONE',  ( 8.250000000000005329, 8.250000000000001776, -26.00000000000001066 ) ) ;
#67052 = EDGE_CURVE ( 'NONE', #55172, #68234, #12943, .T. ) ;
#67053 = EDGE_CURVE ( 'NONE', #9740, #58374, #54431, .T. ) ;
#67054 = CARTESIAN_POINT ( 'NONE',  ( 9.703773737882809058, 8.566576262117189700, 26.00000000000000711 ) ) ;
#67055 = VECTOR ( 'NONE', #65023, 1000.000000000000000 ) ;
#67056 = AXIS2_PLACEMENT_3D ( 'NONE', #6173, #64881, #59573 ) ;
#67057 = EDGE_CURVE ( 'NONE', #33142, #41637, #32160, .T. ) ;
#67058 = DIRECTION ( 'NONE',  ( -0.000000000000000000, 1.000000000000000000, -0.000000000000000000 ) ) ;
#67059 = CARTESIAN_POINT ( 'NONE',  ( 30.00000000000000000, -11.10796162543699950, 9.102987789146602893 ) ) ;
#67061 = ORIENTED_EDGE ( 'NONE', *, *, #6291, .T. ) ;
#67060 = DIRECTION ( 'NONE',  ( -0.6414496315691484707, 0.7671651518153074223, 2.309356642088893343E-17 ) ) ;
#67062 = ORIENTED_EDGE ( 'NONE', *, *, #56206, .F. ) ;
#67063 = LINE ( 'NONE', #35577, #8367 ) ;
#67064 = VECTOR ( 'NONE', #61966, 1000.000000000000000 ) ;
#67066 = VECTOR ( 'NONE', #4564, 1000.000000000000000 ) ;
#67065 = DIRECTION ( 'NONE',  ( 0.000000000000000000, 0.000000000000000000, 1.000000000000000000 ) ) ;
#67067 = DIRECTION ( 'NONE',  ( -0.7671651518153073113, -0.6414496315691485817, -2.587583378555112027E-16 ) ) ;
#67068 = VECTOR ( 'NONE', #62582, 1000.000000000000000 ) ;
#67069 = DIRECTION ( 'NONE',  ( 0.5773502691896270633, -0.5773502691896270633, -0.5773502691896230665 ) ) ;
#67070 = EDGE_LOOP ( 'NONE', ( #49346, #3046, #49967, #46188 ) ) ;
#67071 = DIRECTION ( 'NONE',  ( 0.000000000000000000, 1.000000000000000000, 0.000000000000000000 ) ) ;
#67072 = DIRECTION ( 'NONE',  ( -1.794541526872559352E-16, -1.000000000000000000, 0.000000000000000000 ) ) ;
#67073 = CARTESIAN_POINT ( 'NONE',  ( 13.90000000000000213, -0.2000000000089119934, -8.913009219568841313E-12 ) ) ;
#67074 = DIRECTION ( 'NONE',  ( 1.000000000000000000, 0.000000000000000000, 0.000000000000000000 ) ) ;
#67075 = DIRECTION ( 'NONE',  ( -0.000000000000000000, -0.000000000000000000, -1.000000000000000000 ) ) ;
#67076 = DIRECTION ( 'NONE',  ( 0.000000000000000000, 1.000000000000000000, 0.000000000000000000 ) ) ;
#67077 = AXIS2_PLACEMENT_3D ( 'NONE', #5039, #41473, #14954 ) ;
#67078 = CARTESIAN_POINT ( 'NONE',  ( 283.0000000000000568, -42.50000000000000000, 9.700000000000002842 ) ) ;
#67079 = ORIENTED_EDGE ( 'NONE', *, *, #2195, .F. ) ;
#67080 = CARTESIAN_POINT ( 'NONE',  ( 30.00000000000000000, -12.00000000000000000, -10.20500000000000007 ) ) ;
#67081 = CARTESIAN_POINT ( 'NONE',  ( -8.000000000000000000, -8.000000000000000000, 0.000000000000000000 ) ) ;
#67082 = ORIENTED_EDGE ( 'NONE', *, *, #28472, .F. ) ;
#67083 = LINE ( 'NONE', #56476, #53781 ) ;
#67084 = DIRECTION ( 'NONE',  ( 0.000000000000000000, 1.000000000000000000, 0.000000000000000000 ) ) ;
#67085 = FACE_OUTER_BOUND ( 'NONE', #59400, .T. ) ;
#67086 =( NAMED_UNIT ( * ) SI_UNIT ( $, .STERADIAN. ) SOLID_ANGLE_UNIT ( ) );
#67087 = CARTESIAN_POINT ( 'NONE',  ( -5.993516549646711766, 5.993516549646603409, 455.0000000000000568 ) ) ;
#67088 = VERTEX_POINT ( 'NONE', #687 ) ;
#67089 = CARTESIAN_POINT ( 'NONE',  ( -4.173516549646669738, 11.77351654964658678, 195.0000000000000284 ) ) ;
#67090 = EDGE_CURVE ( 'NONE', #54514, #38741, #65722, .T. ) ;
#67091 = ORIENTED_EDGE ( 'NONE', *, *, #13294, .T. ) ;
#67092 = DIRECTION ( 'NONE',  ( -1.000000000000000000, 0.000000000000000000, 0.000000000000000000 ) ) ;
#67093 = ORIENTED_EDGE ( 'NONE', *, *, #5489, .T. ) ;
#67094 = AXIS2_PLACEMENT_3D ( 'NONE', #32326, #6140, #33360 ) ;
#67095 = EDGE_CURVE ( 'NONE', #29034, #68798, #5643, .T. ) ;
#67096 = DIRECTION ( 'NONE',  ( 0.000000000000000000, 0.000000000000000000, 1.000000000000000000 ) ) ;
#67097 = PRESENTATION_LAYER_ASSIGNMENT (  '', '', ( #4992 ) ) ;
#67099 = EDGE_CURVE ( 'NONE', #47170, #26707, #49113, .T. ) ;
#67098 = VERTEX_POINT ( 'NONE', #11611 ) ;
#67100 = EDGE_CURVE ( 'NONE', #63611, #28340, #25390, .T. ) ;
#67101 = CARTESIAN_POINT ( 'NONE',  ( -8.393516549646733438, -6.344579767990798480, 195.0000000000000284 ) ) ;
#67102 = FACE_OUTER_BOUND ( 'NONE', #67509, .T. ) ;
#67103 = ORIENTED_EDGE ( 'NONE', *, *, #65360, .T. ) ;
#67104 = ORIENTED_EDGE ( 'NONE', *, *, #19261, .F. ) ;
#67105 = DIRECTION ( 'NONE',  ( 0.000000000000000000, -3.673940397442059868E-16, 1.000000000000000000 ) ) ;
#67106 = ORIENTED_EDGE ( 'NONE', *, *, #69320, .T. ) ;
#67107 = ORIENTED_EDGE ( 'NONE', *, *, #58609, .F. ) ;
#67108 = CARTESIAN_POINT ( 'NONE',  ( -5.242976262117275077, -5.257023737882800418, 26.00000000000000711 ) ) ;
#67109 = LINE ( 'NONE', #13006, #58420 ) ;
#67110 = AXIS2_PLACEMENT_3D ( 'NONE', #33095, #5884, #577 ) ;
#67111 = CIRCLE ( 'NONE', #36633, 5.000000000000004441 ) ;
#67112 = CARTESIAN_POINT ( 'NONE',  ( -8.250000000000001776, 7.250000000000000888, -8.500000000000000000 ) ) ;
#67113 = ORIENTED_EDGE ( 'NONE', *, *, #68670, .F. ) ;
#67114 = CARTESIAN_POINT ( 'NONE',  ( 10.50702373788281996, -6.849523737882823760, 54.00000000000000711 ) ) ;
#67116 = CARTESIAN_POINT ( 'NONE',  ( -29.50000000000000355, -11.70000000000012008, -10.70000000000011831 ) ) ;
#67115 = PLANE ( 'NONE',  #20867 ) ;
#67117 = AXIS2_PLACEMENT_3D ( 'NONE', #9928, #20870, #5663 ) ;
#67118 = VECTOR ( 'NONE', #43888, 1000.000000000000000 ) ;
#67120 = ORIENTED_EDGE ( 'NONE', *, *, #7498, .F. ) ;
#67119 = VECTOR ( 'NONE', #69796, 1000.000000000000000 ) ;
#67122 = EDGE_LOOP ( 'NONE', ( #57654, #19843, #46687, #46277, #43999, #9323, #45096, #47060 ) ) ;
#67121 = DIRECTION ( 'NONE',  ( 0.000000000000000000, -0.7071067811865077157, 0.7071067811865873187 ) ) ;
#67123 = ORIENTED_EDGE ( 'NONE', *, *, #62735, .F. ) ;
#67124 = DIRECTION ( 'NONE',  ( 0.000000000000000000, 0.000000000000000000, 1.000000000000000000 ) ) ;
#67125 = CIRCLE ( 'NONE', #36645, 1.929199999999998028 ) ;
#67126 = CARTESIAN_POINT ( 'NONE',  ( 6.789561617636929114, 7.394232575409553476, 26.00000000000000711 ) ) ;
#67127 = EDGE_LOOP ( 'NONE', ( #42867, #54071, #3655, #30458, #14323, #25996 ) ) ;
#67128 = EDGE_CURVE ( 'NONE', #67348, #42310, #55121, .T. ) ;
#67129 = DIRECTION ( 'NONE',  ( 0.000000000000000000, -1.000000000000000000, 0.000000000000000000 ) ) ;
#67130 = LINE ( 'NONE', #41305, #31687 ) ;
#67131 = ORIENTED_EDGE ( 'NONE', *, *, #17407, .F. ) ;
#67132 = ORIENTED_EDGE ( 'NONE', *, *, #16501, .F. ) ;
#67133 = AXIS2_PLACEMENT_3D ( 'NONE', #29715, #7795, #28676 ) ;
#67134 = DIRECTION ( 'NONE',  ( -1.836970198721029934E-16, 1.836970198721036590E-16, -1.000000000000000000 ) ) ;
#67135 = DIRECTION ( 'NONE',  ( 0.000000000000000000, 0.000000000000000000, 1.000000000000000000 ) ) ;
#67136 = ORIENTED_EDGE ( 'NONE', *, *, #27261, .F. ) ;
#67137 = CARTESIAN_POINT ( 'NONE',  ( 1.480523737882816437, 9.390476262117212869, 54.00000000000000711 ) ) ;
#67138 = DIRECTION ( 'NONE',  ( -3.596772705736694889E-15, -1.000000000000000000, 0.000000000000000000 ) ) ;
#67139 = ADVANCED_FACE ( 'NONE', ( #65385 ), #27216, .F. ) ;
#67140 = DIRECTION ( 'NONE',  ( 0.000000000000000000, 3.673940397442059868E-16, -1.000000000000000000 ) ) ;
#67141 = EDGE_CURVE ( 'NONE', #68930, #355, #21219, .T. ) ;
#67142 = VERTEX_POINT ( 'NONE', #33192 ) ;
#67143 = ADVANCED_FACE ( 'NONE', ( #59033 ), #21892, .T. ) ;
#67144 = CARTESIAN_POINT ( 'NONE',  ( -8.452095193409402185, 4.242044687070461784, 195.0000000000000284 ) ) ;
#67145 = LINE ( 'NONE', #23658, #7695 ) ;
#67147 = ORIENTED_EDGE ( 'NONE', *, *, #48549, .F. ) ;
#67146 = FACE_OUTER_BOUND ( 'NONE', #40945, .T. ) ;
#67149 = EDGE_LOOP ( 'NONE', ( #55615, #36347, #60953, #13896 ) ) ;
#67148 = DIRECTION ( 'NONE',  ( -1.000000000000000000, 0.000000000000000000, 0.000000000000000000 ) ) ;
#67150 = DIRECTION ( 'NONE',  ( 0.000000000000000000, 0.000000000000000000, 1.000000000000000000 ) ) ;
#67151 = DIRECTION ( 'NONE',  ( -0.9375000000000006661, 0.000000000000000000, -0.3479852726768744020 ) ) ;
#67152 = CIRCLE ( 'NONE', #6195, 24.99999999998784972 ) ;
#67153 = CYLINDRICAL_SURFACE ( 'NONE', #22283, 0.3499999999999996447 ) ;
#67154 = DIRECTION ( 'NONE',  ( -0.000000000000000000, -0.000000000000000000, -1.000000000000000000 ) ) ;
#67155 = CARTESIAN_POINT ( 'NONE',  ( 7.250000000000005329, 7.250000000000000888, -20.50000000000000000 ) ) ;
#67156 = ORIENTED_EDGE ( 'NONE', *, *, #52864, .F. ) ;
#67157 = CARTESIAN_POINT ( 'NONE',  ( 27.90000000000000213, -14.06939075806902117, -20.80000000000000426 ) ) ;
#67158 = CARTESIAN_POINT ( 'NONE',  ( 7.000000000000000000, -32.95000000000000284, 14.50000000000000000 ) ) ;
#67159 = CARTESIAN_POINT ( 'NONE',  ( 11.50000000000000000, -11.50000000000100009, 15.00000000000084910 ) ) ;
#67161 = VERTEX_POINT ( 'NONE', #6328 ) ;
#67160 = CARTESIAN_POINT ( 'NONE',  ( -6.606374702650211539, -4.747751991980665665, 455.0000000000000568 ) ) ;
#67162 = AXIS2_PLACEMENT_3D ( 'NONE', #55857, #17001, #61490 ) ;
#67163 = VECTOR ( 'NONE', #37153, 1000.000000000000000 ) ;
#67164 = CARTESIAN_POINT ( 'NONE',  ( 4.720772854004774643, -6.358413763958971288, 54.00000000000000711 ) ) ;
#67165 = FACE_OUTER_BOUND ( 'NONE', #44042, .T. ) ;
#67166 = ORIENTED_EDGE ( 'NONE', *, *, #49141, .T. ) ;
#67167 = AXIS2_PLACEMENT_3D ( 'NONE', #61087, #12645, #49802 ) ;
#67168 = EDGE_LOOP ( 'NONE', ( #14076, #4378, #24009, #39050 ) ) ;
#67169 = CARTESIAN_POINT ( 'NONE',  ( 46.39999999999999858, 21.00000000000000000, -2.750000000000000444 ) ) ;
#67170 = FACE_OUTER_BOUND ( 'NONE', #876, .T. ) ;
#67171 = EDGE_LOOP ( 'NONE', ( #57651, #57446, #18423, #67539 ) ) ;
#67172 = DIRECTION ( 'NONE',  ( -0.7071067811865401342, 0.7071067811865550112, 1.355854680848613865E-30 ) ) ;
#67173 =( LENGTH_UNIT ( ) NAMED_UNIT ( * ) SI_UNIT ( .MILLI., .METRE. ) );
#67174 = CARTESIAN_POINT ( 'NONE',  ( 6.849523737882817542, -10.31452373788282095, 54.00000000000000711 ) ) ;
#67175 = DIRECTION ( 'NONE',  ( 1.000000000000000000, 0.000000000000000000, 0.000000000000000000 ) ) ;
#67176 = AXIS2_PLACEMENT_3D ( 'NONE', #24293, #30999, #4142 ) ;
#67177 = ORIENTED_EDGE ( 'NONE', *, *, #32068, .T. ) ;
#67178 = FACE_OUTER_BOUND ( 'NONE', #64321, .T. ) ;
#67179 = ORIENTED_EDGE ( 'NONE', *, *, #65315, .T. ) ;
#67180 = VECTOR ( 'NONE', #17070, 1000.000000000000000 ) ;
#67181 = ORIENTED_EDGE ( 'NONE', *, *, #12211, .F. ) ;
#67182 = EDGE_CURVE ( 'NONE', #18617, #63002, #16240, .T. ) ;
#67183 = AXIS2_PLACEMENT_3D ( 'NONE', #58572, #47599, #59866 ) ;
#67184 = EDGE_CURVE ( 'NONE', #37047, #26866, #49468, .T. ) ;
#67185 = DIRECTION ( 'NONE',  ( 1.000000000000000000, -0.000000000000000000, -0.000000000000000000 ) ) ;
#67186 = ADVANCED_FACE ( 'NONE', ( #38177 ), #54769, .T. ) ;
#67187 = EDGE_CURVE ( 'NONE', #56487, #21960, #9598, .T. ) ;
#67188 = LINE ( 'NONE', #8126, #11795 ) ;
#67190 = DIRECTION ( 'NONE',  ( 0.000000000000000000, 0.000000000000000000, 1.000000000000000000 ) ) ;
#67189 = CARTESIAN_POINT ( 'NONE',  ( 3.682023737882785586, -9.912023737882808661, 54.00000000000000711 ) ) ;
#67191 = ORIENTED_EDGE ( 'NONE', *, *, #7408, .F. ) ;
#67192 = ORIENTED_EDGE ( 'NONE', *, *, #19743, .T. ) ;
#67193 = FACE_OUTER_BOUND ( 'NONE', #56074, .T. ) ;
#67194 = ORIENTED_EDGE ( 'NONE', *, *, #28797, .F. ) ;
#67195 = DIRECTION ( 'NONE',  ( 0.000000000000000000, 0.000000000000000000, 1.000000000000000000 ) ) ;
#67196 = DIRECTION ( 'NONE',  ( -1.000000000000000000, 0.000000000000000000, 0.000000000000000000 ) ) ;
#67197 = LINE ( 'NONE', #29709, #59171 ) ;
#67198 = CARTESIAN_POINT ( 'NONE',  ( -15.50000000000000000, -0.4000000000005236034, 22.50000000000000000 ) ) ;
#67199 = VERTEX_POINT ( 'NONE', #61804 ) ;
#67200 = CARTESIAN_POINT ( 'NONE',  ( -8.821682069070751808, -2.544523737882741887, 54.00000000000000711 ) ) ;
#67202 = DIRECTION ( 'NONE',  ( 0.000000000000000000, -0.7084617869623469621, -0.7057491738671168857 ) ) ;
#67201 = DIRECTION ( 'NONE',  ( 8.359604446858500663E-15, 1.000000000000000000, 3.673940397442059868E-16 ) ) ;
#67203 = VERTEX_POINT ( 'NONE', #1703 ) ;
#67205 = ORIENTED_EDGE ( 'NONE', *, *, #16501, .T. ) ;
#67204 = CARTESIAN_POINT ( 'NONE',  ( -11.07551654964678178, -11.08848345035329075, 195.0000000000000284 ) ) ;
#67206 = AXIS2_PLACEMENT_3D ( 'NONE', #30146, #61964, #46056 ) ;
#67207 = ORIENTED_EDGE ( 'NONE', *, *, #43600, .F. ) ;
#67208 = ORIENTED_EDGE ( 'NONE', *, *, #45719, .F. ) ;
#67209 = AXIS2_PLACEMENT_3D ( 'NONE', #69642, #21201, #54073 ) ;
#67210 = CARTESIAN_POINT ( 'NONE',  ( -11.00000000000000000, -5.599999999999379696, 26.60000000000059828 ) ) ;
#67211 = VECTOR ( 'NONE', #62791, 1000.000000000000000 ) ;
#67212 = AXIS2_PLACEMENT_3D ( 'NONE', #21521, #48745, #43083 ) ;
#67214 = CARTESIAN_POINT ( 'NONE',  ( 7.250000000000005329, -7.249999999999998224, -26.00000000000001066 ) ) ;
#67213 = VECTOR ( 'NONE', #10023, 1000.000000000000000 ) ;
#67215 = B_SPLINE_CURVE_WITH_KNOTS ( 'NONE', 3,
 ( #6705, #2104, #1077, #66101 ),
 .UNSPECIFIED., .F., .F.,
 ( 4, 4 ),
 ( 9.477163989440372305, 10.17593572399551860 ),
 .UNSPECIFIED. ) ;
#67216 = MANIFOLD_SOLID_BREP ( 'LPattern1[19]', #37460 ) ;
#67217 = VERTEX_POINT ( 'NONE', #23966 ) ;
#67218 = ORIENTED_EDGE ( 'NONE', *, *, #15929, .F. ) ;
#67219 = VECTOR ( 'NONE', #52263, 1000.000000000000114 ) ;
#67220 = VECTOR ( 'NONE', #41108, 1000.000000000000000 ) ;
#67221 = DIRECTION ( 'NONE',  ( 0.000000000000000000, -0.6875000000000001110, -0.7261843774138906360 ) ) ;
#67222 = FACE_OUTER_BOUND ( 'NONE', #35710, .T. ) ;
#67223 = ORIENTED_EDGE ( 'NONE', *, *, #12644, .T. ) ;
#67224 = VERTEX_POINT ( 'NONE', #34912 ) ;
#67225 = CARTESIAN_POINT ( 'NONE',  ( 289.7500000000000000, -42.25000000000000711, -26.75000000000000711 ) ) ;
#67226 = VECTOR ( 'NONE', #67650, 1000.000000000000000 ) ;
#67227 = DIRECTION ( 'NONE',  ( -0.000000000000000000, -0.000000000000000000, -1.000000000000000000 ) ) ;
#67228 = ORIENTED_EDGE ( 'NONE', *, *, #5792, .F. ) ;
#67229 = EDGE_CURVE ( 'NONE', #21914, #1362, #45524, .T. ) ;
#67230 = STYLED_ITEM ( 'NONE', ( #31629 ), #44638 ) ;
#67231 = EDGE_CURVE ( 'NONE', #31922, #43306, #60751, .T. ) ;
#67232 = LINE ( 'NONE', #18789, #6403 ) ;
#67233 = DIRECTION ( 'NONE',  ( -1.000000000000000000, 3.491481338843133355E-15, 1.836970198721036344E-16 ) ) ;
#67234 = ADVANCED_FACE ( 'NONE', ( #39866 ), #39524, .T. ) ;
#67236 = VERTEX_POINT ( 'NONE', #56491 ) ;
#67235 = DIRECTION ( 'NONE',  ( 0.000000000000000000, 1.000000000000000000, 0.000000000000000000 ) ) ;
#67237 = VECTOR ( 'NONE', #31882, 1000.000000000000000 ) ;
#67238 = ORIENTED_EDGE ( 'NONE', *, *, #58715, .F. ) ;
#67239 = CARTESIAN_POINT ( 'NONE',  ( 11.00000000000000000, -11.50000000000000000, 19.00000000000000000 ) ) ;
#67240 = CARTESIAN_POINT ( 'NONE',  ( 30.00000000000000000, -11.50000000000100009, 19.50000000000103739 ) ) ;
#67241 = EDGE_CURVE ( 'NONE', #67224, #64674, #18605, .T. ) ;
#67242 = CARTESIAN_POINT ( 'NONE',  ( 283.0000000000000568, -42.00000000000000000, 7.000000000000000000 ) ) ;
#67243 = CARTESIAN_POINT ( 'NONE',  ( 16.75000000000000000, -2.500000000000000000, 23.22168783648699986 ) ) ;
#67244 = PLANE ( 'NONE',  #9804 ) ;
#67245 = PRODUCT_RELATED_PRODUCT_CATEGORY ( 'part', '', ( #17722 ) ) ;
#67246 = CARTESIAN_POINT ( 'NONE',  ( 11.08848345035334404, -11.48848345035349183, 455.0000000000000568 ) ) ;
#67247 = ADVANCED_FACE ( 'NONE', ( #46848 ), #29612, .F. ) ;
#67248 = DIRECTION ( 'NONE',  ( -1.000000000000000000, 0.000000000000000000, 0.000000000000000000 ) ) ;
#67249 = ORIENTED_EDGE ( 'NONE', *, *, #32431, .T. ) ;
#67250 = CARTESIAN_POINT ( 'NONE',  ( -15.50000000000000000, -1.037157890325000054, -22.50000000000000000 ) ) ;
#67251 = EDGE_CURVE ( 'NONE', #56996, #15758, #36702, .T. ) ;
#67252 = ADVANCED_BREP_SHAPE_REPRESENTATION ( '', ( #20363, #45918 ), #825 ) ;
#67254 = ORIENTED_EDGE ( 'NONE', *, *, #25157, .F. ) ;
#67253 = DIRECTION ( 'NONE',  ( 0.000000000000000000, -1.000000000000000000, 0.000000000000000000 ) ) ;
#67255 = DIRECTION ( 'NONE',  ( -0.000000000000000000, 3.673940397442059868E-16, -1.000000000000000000 ) ) ;
#67256 = LINE ( 'NONE', #2543, #35698 ) ;
#67257 = AXIS2_PLACEMENT_3D ( 'NONE', #67597, #69609, #56966 ) ;
#67258 = CYLINDRICAL_SURFACE ( 'NONE', #16720, 0.1749999999999989342 ) ;
#67259 = DIRECTION ( 'NONE',  ( -1.000000000000000000, 0.000000000000000000, 0.000000000000000000 ) ) ;
#67260 = CARTESIAN_POINT ( 'NONE',  ( 49.00000000000000000, -0.1999999999911795112, 8.826273045769999343E-12 ) ) ;
#67261 = AXIS2_PLACEMENT_3D ( 'NONE', #28565, #57194, #23270 ) ;
#67262 = ORIENTED_EDGE ( 'NONE', *, *, #14644, .F. ) ;
#67263 = DIRECTION ( 'NONE',  ( 0.000000000000000000, 1.000000000000000000, 0.000000000000000000 ) ) ;
#67264 = ORIENTED_EDGE ( 'NONE', *, *, #16767, .F. ) ;
#67265 = VECTOR ( 'NONE', #46486, 1000.000000000000000 ) ;
#67266 = DIRECTION ( 'NONE',  ( -1.000000000000000000, 0.000000000000000000, 0.000000000000000000 ) ) ;
#67267 = DIRECTION ( 'NONE',  ( 0.000000000000000000, 0.000000000000000000, 1.000000000000000000 ) ) ;
#67268 = VECTOR ( 'NONE', #17060, 1000.000000000000000 ) ;
#67269 = AXIS2_PLACEMENT_3D ( 'NONE', #34109, #44370, #55355 ) ;
#67270 = PLANE ( 'NONE',  #19475 ) ;
#67271 = ORIENTED_EDGE ( 'NONE', *, *, #43223, .F. ) ;
#67272 = CARTESIAN_POINT ( 'NONE',  ( 7.000000000000000000, -38.15000000000000568, -13.19999999999999929 ) ) ;
#67273 = EDGE_LOOP ( 'NONE', ( #68736, #5410, #11558, #19952 ) ) ;
#67274 = VERTEX_POINT ( 'NONE', #55800 ) ;
#67275 = DIRECTION ( 'NONE',  ( -0.000000000000000000, -0.000000000000000000, 1.000000000000000000 ) ) ;
#67276 = FACE_BOUND ( 'NONE', #23063, .T. ) ;
#67277 = AXIS2_PLACEMENT_3D ( 'NONE', #59978, #65640, #48342 ) ;
#67278 = CIRCLE ( 'NONE', #65020, 0.1749999999999993783 ) ;
#67279 = ORIENTED_EDGE ( 'NONE', *, *, #8612, .F. ) ;
#67280 = CARTESIAN_POINT ( 'NONE',  ( 13.00000000000000178, -17.50000000000000000, 15.70500000000000007 ) ) ;
#67281 = CIRCLE ( 'NONE', #15309, 1.000000000000000000 ) ;
#67282 = DIRECTION ( 'NONE',  ( 0.7142857142857395036, 0.000000000000000000, 0.6998542122237394469 ) ) ;
#67283 = CARTESIAN_POINT ( 'NONE',  ( 25.50000000000000355, 0.000000000000000000, 22.50000000000000000 ) ) ;
#67284 = ORIENTED_EDGE ( 'NONE', *, *, #42578, .F. ) ;
#67285 = ORIENTED_EDGE ( 'NONE', *, *, #30136, .F. ) ;
#67287 = EDGE_LOOP ( 'NONE', ( #66190, #48528, #42015, #54437 ) ) ;
#67286 = PLANE ( 'NONE',  #45252 ) ;
#67288 = ORIENTED_EDGE ( 'NONE', *, *, #62428, .T. ) ;
#67289 = PRODUCT ( 'LINEAR ACTUATOR', 'LINEAR ACTUATOR', '', ( #57916 ) ) ;
#67290 = VECTOR ( 'NONE', #34730, 1000.000000000000000 ) ;
#67291 = DIRECTION ( 'NONE',  ( 0.000000000000000000, -0.1111111111108836896, 0.9938079899999319178 ) ) ;
#67292 = DIRECTION ( 'NONE',  ( 1.836970198721029934E-16, 1.836970198721010706E-16, -1.000000000000000000 ) ) ;
#67293 = DIRECTION ( 'NONE',  ( 0.000000000000000000, 0.000000000000000000, -1.000000000000000000 ) ) ;
#67294 = CARTESIAN_POINT ( 'NONE',  ( 7.261609891743268541, -8.000000000000000000, -1.000000000000000000 ) ) ;
#67295 = AXIS2_PLACEMENT_3D ( 'NONE', #69625, #22564, #12965 ) ;
#67296 = EDGE_CURVE ( 'NONE', #29966, #28048, #2743, .T. ) ;
#67297 = DIRECTION ( 'NONE',  ( -1.000000000000000000, 0.000000000000000000, 0.000000000000000000 ) ) ;
#67298 = ORIENTED_EDGE ( 'NONE', *, *, #4315, .T. ) ;
#67299 = VERTEX_POINT ( 'NONE', #33873 ) ;
#67300 = ORIENTED_EDGE ( 'NONE', *, *, #50200, .F. ) ;
#67301 = ORIENTED_EDGE ( 'NONE', *, *, #39131, .T. ) ;
#67302 = ADVANCED_FACE ( 'NONE', ( #28921 ), #50495, .T. ) ;
#67303 = CARTESIAN_POINT ( 'NONE',  ( -8.250000000000000000, 7.250000000000001776, -22.00000000000000000 ) ) ;
#67304 = DIRECTION ( 'NONE',  ( -1.000000000000000000, 0.000000000000000000, 0.000000000000000000 ) ) ;
#67305 = DIRECTION ( 'NONE',  ( -1.000000000000000000, 0.000000000000000000, 0.000000000000000000 ) ) ;
#67306 = VERTEX_POINT ( 'NONE', #18302 ) ;
#67308 = ADVANCED_FACE ( 'NONE', ( #25291 ), #68425, .F. ) ;
#67307 = EDGE_LOOP ( 'NONE', ( #37802, #9324, #64016, #30406 ) ) ;
#67309 = VECTOR ( 'NONE', #28449, 1000.000000000000000 ) ;
#67310 = VERTEX_POINT ( 'NONE', #10427 ) ;
#67311 = FACE_OUTER_BOUND ( 'NONE', #55570, .T. ) ;
#67312 = VERTEX_POINT ( 'NONE', #47561 ) ;
#67313 = VECTOR ( 'NONE', #17186, 1000.000000000000000 ) ;
#67314 = VERTEX_POINT ( 'NONE', #15736 ) ;
#67315 = FACE_OUTER_BOUND ( 'NONE', #39458, .T. ) ;
#67316 = EDGE_CURVE ( 'NONE', #10256, #6549, #29917, .T. ) ;
#67317 = ORIENTED_EDGE ( 'NONE', *, *, #57807, .F. ) ;
#67318 = EDGE_LOOP ( 'NONE', ( #29019, #32665, #9714, #3045 ) ) ;
#67319 = AXIS2_PLACEMENT_3D ( 'NONE', #5691, #47414, #15612 ) ;
#67320 = LINE ( 'NONE', #3667, #41788 ) ;
#67322 = ORIENTED_EDGE ( 'NONE', *, *, #27268, .T. ) ;
#67321 = DIRECTION ( 'NONE',  ( -1.000000000000000000, 1.813998472013049822E-14, -1.836970198720996654E-16 ) ) ;
#67323 = VERTEX_POINT ( 'NONE', #20677 ) ;
#67324 = DIRECTION ( 'NONE',  ( 0.000000000000000000, 0.000000000000000000, -1.000000000000000000 ) ) ;
#67325 = VECTOR ( 'NONE', #51769, 1000.000000000000114 ) ;
#67326 = CIRCLE ( 'NONE', #5258, 0.8128000000000145109 ) ;
#67327 = AXIS2_PLACEMENT_3D ( 'NONE', #46610, #62517, #57579 ) ;
#67328 = CYLINDRICAL_SURFACE ( 'NONE', #3607, 0.8128000000000145109 ) ;
#67329 = ADVANCED_FACE ( 'NONE', ( #58878 ), #48266, .F. ) ;
#67330 = CARTESIAN_POINT ( 'NONE',  ( 7.000000000000000000, -20.40000000000000213, -12.40000000000000213 ) ) ;
#67332 = VERTEX_POINT ( 'NONE', #38003 ) ;
#67331 = CARTESIAN_POINT ( 'NONE',  ( 10.31452373788281562, -6.657023737882825642, 54.00000000000000711 ) ) ;
#67333 = ORIENTED_EDGE ( 'NONE', *, *, #55542, .F. ) ;
#67334 = AXIS2_PLACEMENT_3D ( 'NONE', #25926, #58793, #26963 ) ;
#67335 = AXIS2_PLACEMENT_3D ( 'NONE', #65735, #48440, #60415 ) ;
#67336 = DIRECTION ( 'NONE',  ( 0.000000000000000000, -0.000000000000000000, -1.000000000000000000 ) ) ;
#67337 = CARTESIAN_POINT ( 'NONE',  ( -7.250000000000000888, 7.450000000000003730, -15.00000000000000000 ) ) ;
#67338 = CARTESIAN_POINT ( 'NONE',  ( 283.0000000000000568, -26.06132420600899735, 10.13999572156699891 ) ) ;
#67339 = AXIS2_PLACEMENT_3D ( 'NONE', #48289, #21408, #32029 ) ;
#67340 = EDGE_CURVE ( 'NONE', #40849, #49649, #31660, .T. ) ;
#67341 = VERTEX_POINT ( 'NONE', #4780 ) ;
#67342 = CARTESIAN_POINT ( 'NONE',  ( -7.250000000000000888, 7.250000000000001776, -13.50000000000000178 ) ) ;
#67343 = ADVANCED_FACE ( 'NONE', ( #32005 ), #177, .T. ) ;
#67344 = AXIS2_PLACEMENT_3D ( 'NONE', #62464, #46213, #57183 ) ;
#67345 = DIRECTION ( 'NONE',  ( 1.570596175624152290E-15, -1.000000000000000000, 0.000000000000000000 ) ) ;
#67346 = CARTESIAN_POINT ( 'NONE',  ( -7.250000000000000888, -8.249999999999998224, -7.500000000000000000 ) ) ;
#67347 = MANIFOLD_SOLID_BREP ( 'Fillet1', #63445 ) ;
#67348 = VERTEX_POINT ( 'NONE', #36592 ) ;
#67349 = CARTESIAN_POINT ( 'NONE',  ( 4.149127210878725158, -3.677663764522648648, 54.00000000000000711 ) ) ;
#67350 = CARTESIAN_POINT ( 'NONE',  ( 6.619341603356837744, -7.265214908726146170, 195.0000000000000284 ) ) ;
#67351 = DIRECTION ( 'NONE',  ( 0.000000000000000000, 0.000000000000000000, -1.000000000000000000 ) ) ;
#67352 = VERTEX_POINT ( 'NONE', #20336 ) ;
#67353 = CARTESIAN_POINT ( 'NONE',  ( -7.955476262117259445, 9.547976262117179758, 54.00000000000000711 ) ) ;
#67354 = CARTESIAN_POINT ( 'NONE',  ( 49.00000000000000000, 0.000000000000000000, 0.000000000000000000 ) ) ;
#67355 = EDGE_LOOP ( 'NONE', ( #55373, #37798, #16247, #51554, #14340, #7787, #50178, #23399, #57263, #23969, #45445, #45045, #55408, #45680, #42741, #61242, #35894, #27124 ) ) ;
#67356 = DIRECTION ( 'NONE',  ( 0.000000000000000000, 0.000000000000000000, -1.000000000000000000 ) ) ;
#67357 = CARTESIAN_POINT ( 'NONE',  ( 13.00000000000000178, -15.50000000000000000, -20.05051025721700242 ) ) ;
#67358 = LINE ( 'NONE', #45780, #40972 ) ;
#67359 = DIRECTION ( 'NONE',  ( 1.000000000000000000, -0.000000000000000000, -0.000000000000000000 ) ) ;
#67360 = LINE ( 'NONE', #56392, #62389 ) ;
#67361 = VERTEX_POINT ( 'NONE', #41900 ) ;
#67362 = DIRECTION ( 'NONE',  ( 1.000000000000000000, -1.828336019306068379E-14, 0.000000000000000000 ) ) ;
#67363 = LINE ( 'NONE', #62040, #49696 ) ;
#67364 = VECTOR ( 'NONE', #40841, 1000.000000000000000 ) ;
#67365 = CARTESIAN_POINT ( 'NONE',  ( -11.18999999999999950, 12.00000000000000000, -4.250000000000000000 ) ) ;
#67366 = EDGE_CURVE ( 'NONE', #41078, #37589, #4442, .T. ) ;
#67367 = AXIS2_PLACEMENT_3D ( 'NONE', #65762, #50188, #55161 ) ;
#67368 = VECTOR ( 'NONE', #46708, 1000.000000000000000 ) ;
#67369 = DIRECTION ( 'NONE',  ( -1.000000000000000000, 0.000000000000000000, 0.000000000000000000 ) ) ;
#67370 = LINE ( 'NONE', #12556, #44097 ) ;
#67371 = EDGE_LOOP ( 'NONE', ( #40587, #5185, #38433, #6177, #12153, #45067, #64386, #28307 ) ) ;
#67373 = ORIENTED_EDGE ( 'NONE', *, *, #20675, .F. ) ;
#67372 = DIRECTION ( 'NONE',  ( -1.000000000000000000, 0.000000000000000000, 0.000000000000000000 ) ) ;
#67374 = ADVANCED_FACE ( 'NONE', ( #42946 ), #58169, .T. ) ;
#67375 = VECTOR ( 'NONE', #23169, 1000.000000000000000 ) ;
#67376 = CIRCLE ( 'NONE', #43488, 0.2000000000000005107 ) ;
#67377 = AXIS2_PLACEMENT_3D ( 'NONE', #43060, #69931, #26118 ) ;
#67378 = CARTESIAN_POINT ( 'NONE',  ( 49.00000000000000000, -0.2000000000089119934, 8.909539772616881237E-12 ) ) ;
#67379 = LINE ( 'NONE', #35176, #59401 ) ;
#67380 = ORIENTED_EDGE ( 'NONE', *, *, #28786, .F. ) ;
#67381 = EDGE_CURVE ( 'NONE', #47223, #37085, #59216, .T. ) ;
#67382 = AXIS2_PLACEMENT_3D ( 'NONE', #43506, #21608, #60458 ) ;
#67383 = DIRECTION ( 'NONE',  ( -1.000000000000000000, 0.000000000000000000, 0.000000000000000000 ) ) ;
#67384 = ADVANCED_FACE ( 'NONE', ( #36971 ), #53926, .F. ) ;
#67385 = ORIENTED_EDGE ( 'NONE', *, *, #19477, .F. ) ;
#67386 = CIRCLE ( 'NONE', #50420, 0.2000000000000005107 ) ;
#67387 = CARTESIAN_POINT ( 'NONE',  ( -14.25000000000000000, -0.3156864504677185379, -22.25638000318209109 ) ) ;
#67388 = ORIENTED_EDGE ( 'NONE', *, *, #11560, .T. ) ;
#67389 = EDGE_CURVE ( 'NONE', #46286, #30523, #1702, .T. ) ;
#67390 = ORIENTED_EDGE ( 'NONE', *, *, #54552, .F. ) ;
#67391 = LINE ( 'NONE', #18945, #18332 ) ;
#67392 = LINE ( 'NONE', #7628, #15092 ) ;
#67393 = FACE_OUTER_BOUND ( 'NONE', #36005, .T. ) ;
#67394 = CARTESIAN_POINT ( 'NONE',  ( 10.50702373788281996, -3.664523737882826815, 54.00000000000000711 ) ) ;
#67395 = AXIS2_PLACEMENT_3D ( 'NONE', #61217, #45660, #13492 ) ;
#67396 = ORIENTED_EDGE ( 'NONE', *, *, #56721, .F. ) ;
#67397 = EDGE_CURVE ( 'NONE', #59771, #54084, #21030, .T. ) ;
#67398 = EDGE_LOOP ( 'NONE', ( #50769, #4545, #31677, #50113, #57690 ) ) ;
#67399 = DIRECTION ( 'NONE',  ( 0.000000000000000000, -1.000000000000000000, 0.000000000000000000 ) ) ;
#67400 = EDGE_CURVE ( 'NONE', #44075, #12124, #23547, .T. ) ;
#67401 = LINE ( 'NONE', #28846, #53135 ) ;
#67402 = VERTEX_POINT ( 'NONE', #44318 ) ;
#67403 = EDGE_CURVE ( 'NONE', #55252, #36470, #59903, .T. ) ;
#67404 = ORIENTED_EDGE ( 'NONE', *, *, #2676, .T. ) ;
#67405 = ADVANCED_FACE ( 'NONE', ( #33033 ), #27387, .T. ) ;
#67406 = EDGE_CURVE ( 'NONE', #26198, #32897, #64971, .T. ) ;
#67407 = ORIENTED_EDGE ( 'NONE', *, *, #26984, .F. ) ;
#67408 = DIRECTION ( 'NONE',  ( -1.836970198721029934E-16, -1.836970198721010706E-16, 1.000000000000000000 ) ) ;
#67410 = ORIENTED_EDGE ( 'NONE', *, *, #20304, .F. ) ;
#67409 = CARTESIAN_POINT ( 'NONE',  ( -7.393516549646776070, -6.006483450353401921, 455.0000000000000568 ) ) ;
#67411 = ADVANCED_FACE ( 'NONE', ( #48957 ), #50328, .F. ) ;
#67412 = LINE ( 'NONE', #2002, #51433 ) ;
#67413 = DIRECTION ( 'NONE',  ( 0.000000000000000000, -1.000000000000000000, 0.000000000000000000 ) ) ;
#67414 = VERTEX_POINT ( 'NONE', #17811 ) ;
#67415 = EDGE_LOOP ( 'NONE', ( #47405, #54146 ) ) ;
#67416 = CIRCLE ( 'NONE', #53862, 0.3499999999999996447 ) ;
#67417 = DIRECTION ( 'NONE',  ( 1.000000000000000000, 0.000000000000000000, 0.000000000000000000 ) ) ;
#67418 = DIRECTION ( 'NONE',  ( 0.8660254037844510311, 0.4999999999999786282, 0.000000000000000000 ) ) ;
#67419 = VECTOR ( 'NONE', #15871, 1000.000000000000000 ) ;
#67420 = CIRCLE ( 'NONE', #15499, 4.000000000000000888 ) ;
#67421 = ADVANCED_FACE ( 'NONE', ( #12150, #28753 ), #44662, .F. ) ;
#67422 = DIRECTION ( 'NONE',  ( -1.836970198721029934E-16, -1.836970198721010706E-16, 1.000000000000000000 ) ) ;
#67423 = ADVANCED_FACE ( 'NONE', ( #33718 ), #55300, .F. ) ;
#67424 = AXIS2_PLACEMENT_3D ( 'NONE', #2564, #66572, #46054 ) ;
#67425 = VECTOR ( 'NONE', #4807, 1000.000000000000000 ) ;
#67426 = CARTESIAN_POINT ( 'NONE',  ( 7.000000000000000000, -30.80000000000000071, -8.900000000000000355 ) ) ;
#67427 = CARTESIAN_POINT ( 'NONE',  ( 7.357023737882817827, -4.961189459950053227, 26.00000000000000711 ) ) ;
#67429 = VERTEX_POINT ( 'NONE', #54614 ) ;
#67428 = PRESENTATION_STYLE_ASSIGNMENT (( #41592 ) ) ;
#67430 = VERTEX_POINT ( 'NONE', #517 ) ;
#67431 = FACE_OUTER_BOUND ( 'NONE', #11535, .T. ) ;
#67432 = CARTESIAN_POINT ( 'NONE',  ( -4.727349090213552429, -4.201500623656063915, 455.0000000000000568 ) ) ;
#67433 = AXIS2_PLACEMENT_3D ( 'NONE', #16122, #27078, #47260 ) ;
#67434 = DIRECTION ( 'NONE',  ( -0.000000000000000000, -0.000000000000000000, -1.000000000000000000 ) ) ;
#67435 = FACE_OUTER_BOUND ( 'NONE', #26946, .T. ) ;
#67436 = CARTESIAN_POINT ( 'NONE',  ( -8.250000000000001776, -7.249999999999998224, -19.50000000000000000 ) ) ;
#67437 = VERTEX_POINT ( 'NONE', #49974 ) ;
#67438 = FACE_OUTER_BOUND ( 'NONE', #60497, .T. ) ;
#67439 = CARTESIAN_POINT ( 'NONE',  ( -9.750000000000001776, 9.690000000000001279, -4.250000000000000000 ) ) ;
#67440 = DIRECTION ( 'NONE',  ( 0.7071067811865464625, -0.7071067811865486830, -2.597868168706483555E-16 ) ) ;
#67441 = DIRECTION ( 'NONE',  ( 3.491481338843133355E-15, 1.000000000000000000, 1.836970198721029934E-16 ) ) ;
#67442 = CIRCLE ( 'NONE', #66329, 0.1999999999999996503 ) ;
#67443 = ADVANCED_FACE ( 'NONE', ( #6523 ), #6161, .F. ) ;
#67444 = FACE_BOUND ( 'NONE', #65627, .T. ) ;
#67445 = CARTESIAN_POINT ( 'NONE',  ( 8.144523737882817471, -9.562023737882809016, 26.00000000000000000 ) ) ;
#67446 = DIRECTION ( 'NONE',  ( 1.836970198721029934E-16, 1.836970198721010706E-16, -1.000000000000000000 ) ) ;
#67447 = ORIENTED_EDGE ( 'NONE', *, *, #41913, .F. ) ;
#67448 = CARTESIAN_POINT ( 'NONE',  ( 283.0000000000000568, -26.06128899128900045, -10.14003097807800025 ) ) ;
#67449 = CARTESIAN_POINT ( 'NONE',  ( 39.00000000000000000, -21.00000000000000000, -14.57806571531351914 ) ) ;
#67450 = ORIENTED_EDGE ( 'NONE', *, *, #32686, .T. ) ;
#67451 = DIRECTION ( 'NONE',  ( 0.000000000000000000, 0.000000000000000000, 1.000000000000000000 ) ) ;
#67452 = LINE ( 'NONE', #46912, #15292 ) ;
#67453 = DIRECTION ( 'NONE',  ( -1.000000000000000000, 0.000000000000000000, 0.000000000000000000 ) ) ;
#67454 = DIRECTION ( 'NONE',  ( -1.000000000000000000, 0.000000000000000000, 0.000000000000000000 ) ) ;
#67455 = FACE_OUTER_BOUND ( 'NONE', #65310, .T. ) ;
#67456 = ORIENTED_EDGE ( 'NONE', *, *, #55111, .F. ) ;
#67457 = ADVANCED_FACE ( 'NONE', ( #27731 ), #22085, .T. ) ;
#67458 = CYLINDRICAL_SURFACE ( 'NONE', #45405, 0.4000000000000010214 ) ;
#67459 = ORIENTED_EDGE ( 'NONE', *, *, #22037, .F. ) ;
#67460 = LINE ( 'NONE', #67799, #35381 ) ;
#67461 = DIRECTION ( 'NONE',  ( 0.000000000000000000, 0.000000000000000000, -1.000000000000000000 ) ) ;
#67462 = AXIS2_PLACEMENT_3D ( 'NONE', #36039, #47350, #53024 ) ;
#67463 = VERTEX_POINT ( 'NONE', #43648 ) ;
#67464 = EDGE_CURVE ( 'NONE', #48929, #65032, #43502, .T. ) ;
#67465 = CARTESIAN_POINT ( 'NONE',  ( 7.250000000000005329, -7.249999999999998224, -10.00000000000000000 ) ) ;
#67466 = EDGE_CURVE ( 'NONE', #31830, #23630, #65230, .T. ) ;
#67467 = VERTEX_POINT ( 'NONE', #43980 ) ;
#67468 = CIRCLE ( 'NONE', #18908, 0.2999999999994937827 ) ;
#67469 = AXIS2_PLACEMENT_3D ( 'NONE', #8719, #46888, #41944 ) ;
#67470 = FACE_OUTER_BOUND ( 'NONE', #33320, .T. ) ;
#67471 = EDGE_LOOP ( 'NONE', ( #29422, #9046, #19532, #1474 ) ) ;
#67472 = EDGE_CURVE ( 'NONE', #4926, #19062, #65559, .T. ) ;
#67473 = ORIENTED_EDGE ( 'NONE', *, *, #22320, .T. ) ;
#67474 = FACE_OUTER_BOUND ( 'NONE', #15751, .T. ) ;
#67475 = ORIENTED_EDGE ( 'NONE', *, *, #60274, .T. ) ;
#67476 = ORIENTED_EDGE ( 'NONE', *, *, #46646, .F. ) ;
#67477 = VECTOR ( 'NONE', #2480, 1000.000000000000000 ) ;
#67478 = CIRCLE ( 'NONE', #59606, 1.000000000000003553 ) ;
#67479 = CARTESIAN_POINT ( 'NONE',  ( 49.00000000000000000, 13.66939075806899950, 20.80000000000000426 ) ) ;
#67480 = CARTESIAN_POINT ( 'NONE',  ( 41.09999999999999432, -14.06939075806901940, -20.80000000000000426 ) ) ;
#67481 = DIRECTION ( 'NONE',  ( -1.000000000000000000, 0.000000000000000000, 0.000000000000000000 ) ) ;
#67482 = LINE ( 'NONE', #43099, #53120 ) ;
#67483 = ORIENTED_EDGE ( 'NONE', *, *, #32813, .T. ) ;
#67484 = CARTESIAN_POINT ( 'NONE',  ( 283.0000000000000568, -32.95000000000000284, -14.50000000000000000 ) ) ;
#67485 = VECTOR ( 'NONE', #58839, 1000.000000000000000 ) ;
#67486 = VECTOR ( 'NONE', #65978, 1000.000000000000000 ) ;
#67488 = DIRECTION ( 'NONE',  ( -1.000000000000000000, 1.261617073437657577E-14, 4.635105932205237132E-30 ) ) ;
#67487 = DIRECTION ( 'NONE',  ( 0.000000000000000000, 0.000000000000000000, 1.000000000000000000 ) ) ;
#67489 = ORIENTED_EDGE ( 'NONE', *, *, #27486, .F. ) ;
#67491 = EDGE_LOOP ( 'NONE', ( #6466, #4987, #11053, #93 ) ) ;
#67490 = LINE ( 'NONE', #3821, #20676 ) ;
#67492 = ORIENTED_EDGE ( 'NONE', *, *, #67046, .T. ) ;
#67493 = EDGE_CURVE ( 'NONE', #61430, #12238, #60241, .T. ) ;
#67494 = APPLICATION_PROTOCOL_DEFINITION ( 'draft international standard', 'automotive_design', 1998, #38180 ) ;
#67495 = FACE_OUTER_BOUND ( 'NONE', #10690, .T. ) ;
#67496 = ORIENTED_EDGE ( 'NONE', *, *, #34059, .F. ) ;
#67497 = AXIS2_PLACEMENT_3D ( 'NONE', #2370, #23932, #46192 ) ;
#67498 = LINE ( 'NONE', #62881, #18968 ) ;
#67499 = CARTESIAN_POINT ( 'NONE',  ( 7.000000000000000000, -32.46196062927499781, -8.091291340630698770 ) ) ;
#67500 = ORIENTED_EDGE ( 'NONE', *, *, #23563, .F. ) ;
#67501 = ORIENTED_EDGE ( 'NONE', *, *, #16929, .F. ) ;
#67502 = CARTESIAN_POINT ( 'NONE',  ( -7.750000000000001776, -7.348062532927999158, -5.000000000000000000 ) ) ;
#67503 = DIRECTION ( 'NONE',  ( -0.000000000000000000, -0.000000000000000000, -1.000000000000000000 ) ) ;
#67504 = ORIENTED_EDGE ( 'NONE', *, *, #13507, .F. ) ;
#67505 = DIRECTION ( 'NONE',  ( -0.7071067811865500152, -0.7071067811865451302, 4.683861624749757595E-31 ) ) ;
#67506 = LINE ( 'NONE', #68191, #28961 ) ;
#67507 = CARTESIAN_POINT ( 'NONE',  ( 6.657023737882818537, -10.31452373788282095, 54.00000000000000711 ) ) ;
#67508 = EDGE_CURVE ( 'NONE', #58770, #4599, #1210, .T. ) ;
#67509 = EDGE_LOOP ( 'NONE', ( #45823, #35921, #9843, #31835 ) ) ;
#67510 = ADVANCED_FACE ( 'NONE', ( #24155 ), #39710, .T. ) ;
#67511 = CARTESIAN_POINT ( 'NONE',  ( 7.450000000000006395, 7.250000000000000888, -10.00000000000000000 ) ) ;
#67512 = CARTESIAN_POINT ( 'NONE',  ( -8.693516549646711056, 11.11351654964659730, 455.0000000000000568 ) ) ;
#67513 = AXIS2_PLACEMENT_3D ( 'NONE', #54239, #49611, #11429 ) ;
#67516 = ORIENTED_EDGE ( 'NONE', *, *, #58265, .T. ) ;
#67515 = EDGE_CURVE ( 'NONE', #19689, #43731, #14175, .T. ) ;
#67514 = DIRECTION ( 'NONE',  ( 0.000000000000000000, 0.000000000000000000, 1.000000000000000000 ) ) ;
#67518 = ORIENTED_EDGE ( 'NONE', *, *, #19800, .F. ) ;
#67517 = CARTESIAN_POINT ( 'NONE',  ( -24.00000000000000000, -16.64230188589299786, 14.64519951917100116 ) ) ;
#67519 = CARTESIAN_POINT ( 'NONE',  ( -9.791916549646712653, 10.19191654964664018, 455.0000000000000568 ) ) ;
#67520 = FACE_OUTER_BOUND ( 'NONE', #1765, .T. ) ;
#67521 = DIRECTION ( 'NONE',  ( 0.000000000000000000, 0.000000000000000000, -1.000000000000000000 ) ) ;
#67522 = DIRECTION ( 'NONE',  ( 1.000000000000000000, -0.000000000000000000, 0.000000000000000000 ) ) ;
#67523 = CARTESIAN_POINT ( 'NONE',  ( -4.393516549646835578, -11.78648345035344214, 455.0000000000000568 ) ) ;
#67524 = ORIENTED_EDGE ( 'NONE', *, *, #25253, .T. ) ;
#67525 = DIRECTION ( 'NONE',  ( 1.000000000000000000, -1.356437060717834379E-15, -1.836970198721032646E-16 ) ) ;
#67526 = DIRECTION ( 'NONE',  ( 3.016910393003147986E-15, 1.000000000000000000, -0.000000000000000000 ) ) ;
#67527 = CARTESIAN_POINT ( 'NONE',  ( -11.99351654964671354, 7.813516549646603693, 455.0000000000000568 ) ) ;
#67528 = VECTOR ( 'NONE', #43808, 1000.000000000000000 ) ;
#67530 = ORIENTED_EDGE ( 'NONE', *, *, #43445, .F. ) ;
#67529 = CARTESIAN_POINT ( 'NONE',  ( 2.706483450353371900, 10.91351654964663354, 195.0000000000000284 ) ) ;
#67531 = DIRECTION ( 'NONE',  ( -1.000000000000000000, 0.000000000000000000, 0.000000000000000000 ) ) ;
#67532 = DIRECTION ( 'NONE',  ( 0.000000000000000000, 0.7071067811865474617, 0.7071067811865474617 ) ) ;
#67533 = VECTOR ( 'NONE', #18703, 1000.000000000000000 ) ;
#67534 = CIRCLE ( 'NONE', #66410, 0.7112000000000124889 ) ;
#67535 = VERTEX_POINT ( 'NONE', #50672 ) ;
#67536 = ORIENTED_EDGE ( 'NONE', *, *, #17978, .T. ) ;
#67537 = CARTESIAN_POINT ( 'NONE',  ( 8.900000000000005684, -0.2000000000000000111, 0.000000000000000000 ) ) ;
#67538 = DIRECTION ( 'NONE',  ( -0.000000000000000000, 3.673940397442059868E-16, -1.000000000000000000 ) ) ;
#67539 = ORIENTED_EDGE ( 'NONE', *, *, #41847, .F. ) ;
#67540 = DIRECTION ( 'NONE',  ( -0.000000000000000000, 3.673940397442059868E-16, -1.000000000000000000 ) ) ;
#67541 = CARTESIAN_POINT ( 'NONE',  ( 27.90000000000000213, 13.66939075806899240, 20.79999999999999361 ) ) ;
#67542 = EDGE_CURVE ( 'NONE', #30661, #22096, #66106, .T. ) ;
#67543 = CARTESIAN_POINT ( 'NONE',  ( 11.78648345035340839, 7.813516549646560172, 455.0000000000000568 ) ) ;
#67544 = ORIENTED_EDGE ( 'NONE', *, *, #12131, .T. ) ;
#67545 = PLANE ( 'NONE',  #22472 ) ;
#67546 = DIRECTION ( 'NONE',  ( 0.000000000000000000, -0.7057491738665938596, 0.7084617869628679898 ) ) ;
#67547 = VERTEX_POINT ( 'NONE', #18848 ) ;
#67548 = DIRECTION ( 'NONE',  ( -0.5773502691896230665, -0.5773502691896271743, 0.5773502691896271743 ) ) ;
#67549 = EDGE_CURVE ( 'NONE', #54840, #13233, #45709, .T. ) ;
#67550 = EDGE_CURVE ( 'NONE', #57368, #13785, #46762, .T. ) ;
#67551 = FILL_AREA_STYLE ('',( #28660 ) ) ;
#67552 = CARTESIAN_POINT ( 'NONE',  ( 2.420780051175148273, -8.711985858128677762, 54.00000000000000711 ) ) ;
#67553 = VERTEX_POINT ( 'NONE', #8933 ) ;
#67554 = EDGE_CURVE ( 'NONE', #27638, #57404, #3287, .T. ) ;
#67555 = ORIENTED_EDGE ( 'NONE', *, *, #24124, .F. ) ;
#67556 = EDGE_CURVE ( 'NONE', #28277, #1362, #2237, .T. ) ;
#67557 = LINE ( 'NONE', #36422, #58956 ) ;
#67558 = ORIENTED_EDGE ( 'NONE', *, *, #57429, .T. ) ;
#67559 = ORIENTED_EDGE ( 'NONE', *, *, #67858, .F. ) ;
#67560 = DIRECTION ( 'NONE',  ( 0.000000000000000000, 0.000000000000000000, 1.000000000000000000 ) ) ;
#67561 = DIRECTION ( 'NONE',  ( -1.794541526872559352E-16, -1.000000000000000000, 0.000000000000000000 ) ) ;
#67562 = CARTESIAN_POINT ( 'NONE',  ( 12.00648345035341968, 11.18071654964654726, 455.0000000000000568 ) ) ;
#67563 = EDGE_CURVE ( 'NONE', #3872, #41995, #12993, .T. ) ;
#67564 = DIRECTION ( 'NONE',  ( -0.7671651518152998728, 0.6414496315691574635, 0.000000000000000000 ) ) ;
#67565 = VERTEX_POINT ( 'NONE', #34757 ) ;
#67566 = CARTESIAN_POINT ( 'NONE',  ( 39.00000000000000000, 0.000000000000000000, 0.000000000000000000 ) ) ;
#67568 = CARTESIAN_POINT ( 'NONE',  ( -11.50000000000000000, -11.50000000000000000, -11.00000000000000000 ) ) ;
#67567 = DIRECTION ( 'NONE',  ( -1.000000000000000000, 1.794541526872559352E-16, 0.000000000000000000 ) ) ;
#67569 = VERTEX_POINT ( 'NONE', #19542 ) ;
#67571 = ORIENTED_EDGE ( 'NONE', *, *, #50032, .F. ) ;
#67570 = DIRECTION ( 'NONE',  ( 0.000000000000000000, 1.000000000000000000, 0.000000000000000000 ) ) ;
#67572 = ORIENTED_EDGE ( 'NONE', *, *, #19402, .T. ) ;
#67573 = ORIENTED_EDGE ( 'NONE', *, *, #2170, .T. ) ;
#67574 = DIRECTION ( 'NONE',  ( 0.7071067811865474617, -0.7071067811865474617, -2.597868168706479611E-16 ) ) ;
#67575 = AXIS2_PLACEMENT_3D ( 'NONE', #35612, #31395, #57196 ) ;
#67576 = LINE ( 'NONE', #56947, #42014 ) ;
#67577 = MANIFOLD_SOLID_BREP ( 'LPattern1[23]', #16012 ) ;
#67578 = VERTEX_POINT ( 'NONE', #51371 ) ;
#67579 = ORIENTED_EDGE ( 'NONE', *, *, #53672, .F. ) ;
#67580 = VECTOR ( 'NONE', #17152, 1000.000000000000000 ) ;
#67581 = LINE ( 'NONE', #20184, #17358 ) ;
#67582 = FACE_OUTER_BOUND ( 'NONE', #55216, .T. ) ;
#67583 = ORIENTED_EDGE ( 'NONE', *, *, #7818, .T. ) ;
#67584 = ORIENTED_EDGE ( 'NONE', *, *, #67095, .F. ) ;
#67585 = DIRECTION ( 'NONE',  ( 0.000000000000000000, 0.000000000000000000, -1.000000000000000000 ) ) ;
#67586 = DIRECTION ( 'NONE',  ( 0.000000000000000000, -0.1111111111108840643, -0.9938079899999319178 ) ) ;
#67587 = ORIENTED_EDGE ( 'NONE', *, *, #69644, .T. ) ;
#67588 = AXIS2_PLACEMENT_3D ( 'NONE', #67612, #35414, #61944 ) ;
#67589 = DIRECTION ( 'NONE',  ( -3.491481338843133355E-15, -1.000000000000000000, -1.836970198721029934E-16 ) ) ;
#67590 = DIRECTION ( 'NONE',  ( 1.000000000000000000, -0.000000000000000000, 0.000000000000000000 ) ) ;
#67593 = ORIENTED_EDGE ( 'NONE', *, *, #10328, .F. ) ;
#67592 = ADVANCED_FACE ( 'NONE', ( #24510 ), #68342, .F. ) ;
#67591 = CARTESIAN_POINT ( 'NONE',  ( -10.03972626211722918, 9.689726262117183353, 54.00000000000000711 ) ) ;
#67594 = ORIENTED_EDGE ( 'NONE', *, *, #25331, .T. ) ;
#67595 = EDGE_CURVE ( 'NONE', #26444, #59688, #57025, .T. ) ;
#67596 = FACE_OUTER_BOUND ( 'NONE', #48625, .T. ) ;
#67597 = CARTESIAN_POINT ( 'NONE',  ( -10.30047626211729295, -6.657023737882751924, 54.00000000000000711 ) ) ;
#67598 = CARTESIAN_POINT ( 'NONE',  ( 15.00000000000000000, -26.28355339059299922, 9.766446609406699508 ) ) ;
#67599 = CARTESIAN_POINT ( 'NONE',  ( 8.711985858128681315, 8.079219948824839292, 26.00000000000000711 ) ) ;
#67600 = DIRECTION ( 'NONE',  ( -1.000000000000000000, 0.000000000000000000, 0.000000000000000000 ) ) ;
#67601 = ADVANCED_FACE ( 'NONE', ( #67995 ), #62676, .T. ) ;
#67602 = DIRECTION ( 'NONE',  ( 0.000000000000000000, 0.000000000000000000, -1.000000000000000000 ) ) ;
#67603 = CARTESIAN_POINT ( 'NONE',  ( 23.90000000000000213, -0.2000000000089119934, 8.909539772616881237E-12 ) ) ;
#67604 = ORIENTED_EDGE ( 'NONE', *, *, #64402, .F. ) ;
#67605 = DIRECTION ( 'NONE',  ( 1.000000000000000000, 0.000000000000000000, 0.000000000000000000 ) ) ;
#67607 = ORIENTED_EDGE ( 'NONE', *, *, #66890, .F. ) ;
#67606 = FACE_OUTER_BOUND ( 'NONE', #46622, .T. ) ;
#67608 = DIRECTION ( 'NONE',  ( 0.000000000000000000, 0.000000000000000000, -1.000000000000000000 ) ) ;
#67609 = DIRECTION ( 'NONE',  ( 0.7071067811865411334, -0.7071067811865539010, -2.597868168706484541E-16 ) ) ;
#67610 = DIRECTION ( 'NONE',  ( 1.000000000000000000, 0.000000000000000000, 0.000000000000000000 ) ) ;
#67611 = CARTESIAN_POINT ( 'NONE',  ( -11.75000000000000000, -5.000000000000000000, 26.25000000000000000 ) ) ;
#67612 = CARTESIAN_POINT ( 'NONE',  ( -11.75000000000000000, -5.000000000000000000, 60.00000000000000000 ) ) ;
#67613 = ORIENTED_EDGE ( 'NONE', *, *, #57437, .T. ) ;
#67614 = CARTESIAN_POINT ( 'NONE',  ( -7.250000000000000888, 7.250000000000001776, -10.50000000000000000 ) ) ;
#67615 = CARTESIAN_POINT ( 'NONE',  ( 47.00000000000000000, 0.000000000000000000, 0.000000000000000000 ) ) ;
#67616 = ORIENTED_EDGE ( 'NONE', *, *, #10163, .T. ) ;
#67617 = LINE ( 'NONE', #46047, #29090 ) ;
#67618 = AXIS2_PLACEMENT_3D ( 'NONE', #31228, #31915, #64103 ) ;
#67619 = LINE ( 'NONE', #24131, #55768 ) ;
#67620 = ORIENTED_EDGE ( 'NONE', *, *, #30980, .T. ) ;
#67621 = CARTESIAN_POINT ( 'NONE',  ( 23.48000000000000043, -15.50000000000000000, 26.00000000000000355 ) ) ;
#67622 = EDGE_LOOP ( 'NONE', ( #51213, #47293, #57044, #12709 ) ) ;
#67623 = VERTEX_POINT ( 'NONE', #36884 ) ;
#67624 = AXIS2_PLACEMENT_3D ( 'NONE', #19944, #41512, #63080 ) ;
#67625 = LINE ( 'NONE', #29092, #17752 ) ;
#67626 = CYLINDRICAL_SURFACE ( 'NONE', #11610, 0.2000000000000005107 ) ;
#67627 = DIRECTION ( 'NONE',  ( 1.836970198721029934E-16, 1.836970198721010706E-16, -1.000000000000000000 ) ) ;
#67628 = VECTOR ( 'NONE', #53469, 1000.000000000000000 ) ;
#67629 = DIRECTION ( 'NONE',  ( 0.000000000000000000, 0.000000000000000000, 1.000000000000000000 ) ) ;
#67630 = DIRECTION ( 'NONE',  ( 1.000000000000000000, -0.000000000000000000, -0.000000000000000000 ) ) ;
#67631 = ORIENTED_EDGE ( 'NONE', *, *, #11575, .F. ) ;
#67632 = ORIENTED_EDGE ( 'NONE', *, *, #31079, .T. ) ;
#67633 = EDGE_CURVE ( 'NONE', #38190, #48101, #36156, .T. ) ;
#67635 = VERTEX_POINT ( 'NONE', #41472 ) ;
#67634 = DIRECTION ( 'NONE',  ( -1.000000000000000000, 0.000000000000000000, 0.000000000000000000 ) ) ;
#67636 = VERTEX_POINT ( 'NONE', #26261 ) ;
#67637 = VECTOR ( 'NONE', #13684, 1000.000000000000000 ) ;
#67638 = FACE_OUTER_BOUND ( 'NONE', #8693, .T. ) ;
#67639 = FACE_OUTER_BOUND ( 'NONE', #47743, .T. ) ;
#67640 = EDGE_CURVE ( 'NONE', #37912, #5159, #36758, .T. ) ;
#67641 = DIRECTION ( 'NONE',  ( -1.000000000000000000, 0.000000000000000000, 0.000000000000000000 ) ) ;
#67642 = DIRECTION ( 'NONE',  ( 1.000000000000000000, -3.016910393003147986E-15, 0.000000000000000000 ) ) ;
#67643 = EDGE_CURVE ( 'NONE', #37614, #9113, #41813, .T. ) ;
#67644 = DIRECTION ( 'NONE',  ( 1.000000000000000000, 0.000000000000000000, 0.000000000000000000 ) ) ;
#67645 = DIRECTION ( 'NONE',  ( 0.000000000000000000, 0.000000000000000000, 1.000000000000000000 ) ) ;
#67646 = EDGE_LOOP ( 'NONE', ( #65931, #55652, #13797, #20355 ) ) ;
#67647 = ORIENTED_EDGE ( 'NONE', *, *, #21207, .T. ) ;
#67648 = ORIENTED_EDGE ( 'NONE', *, *, #15597, .T. ) ;
#67649 = ORIENTED_EDGE ( 'NONE', *, *, #53545, .T. ) ;
#67650 = DIRECTION ( 'NONE',  ( -2.990116172375847553E-15, -1.000000000000000000, -1.836970198721030920E-16 ) ) ;
#67651 = CARTESIAN_POINT ( 'NONE',  ( 15.00000000000000000, -25.60000000000000142, 17.60000000000000142 ) ) ;
#67652 = EDGE_CURVE ( 'NONE', #34600, #50090, #37573, .T. ) ;
#67653 = CARTESIAN_POINT ( 'NONE',  ( 1.000000000000000000, -21.00000000000000000, 4.000000000000000000 ) ) ;
#67654 = VERTEX_POINT ( 'NONE', #63040 ) ;
#67655 = EDGE_LOOP ( 'NONE', ( #3726, #37021, #43173, #41356 ) ) ;
#67656 = ORIENTED_EDGE ( 'NONE', *, *, #54155, .T. ) ;
#67657 = DIRECTION ( 'NONE',  ( 0.3479852726768751237, 0.000000000000000000, -0.9375000000000004441 ) ) ;
#67658 = ORIENTED_EDGE ( 'NONE', *, *, #62383, .T. ) ;
#67659 = EDGE_LOOP ( 'NONE', ( #34484, #19203, #42711, #18320 ) ) ;
#67660 = CARTESIAN_POINT ( 'NONE',  ( -6.817976262117261044, 9.722976262117182245, 26.00000000000000711 ) ) ;
#67661 = ORIENTED_EDGE ( 'NONE', *, *, #36016, .F. ) ;
#67662 = CIRCLE ( 'NONE', #10088, 1.000000000000000000 ) ;
#67663 = ORIENTED_EDGE ( 'NONE', *, *, #2709, .T. ) ;
#67664 = DIRECTION ( 'NONE',  ( 1.836970198721029934E-16, 1.836970198721010706E-16, -1.000000000000000000 ) ) ;
#67666 = ORIENTED_EDGE ( 'NONE', *, *, #60901, .F. ) ;
#67665 = LINE ( 'NONE', #19569, #27756 ) ;
#67667 = VERTEX_POINT ( 'NONE', #48522 ) ;
#67668 = AXIS2_PLACEMENT_3D ( 'NONE', #31488, #9562, #63660 ) ;
#67669 = DIRECTION ( 'NONE',  ( 0.000000000000000000, 0.000000000000000000, -1.000000000000000000 ) ) ;
#67670 = CARTESIAN_POINT ( 'NONE',  ( -2.693516549646675529, 10.91351654964657314, 195.0000000000000284 ) ) ;
#67671 = CARTESIAN_POINT ( 'NONE',  ( 289.5000000000000000, 0.000000000000000000, 26.50000000000000000 ) ) ;
#67673 = ORIENTED_EDGE ( 'NONE', *, *, #19604, .F. ) ;
#67672 = CARTESIAN_POINT ( 'NONE',  ( -7.259684009079930611, 7.798499376343971612, 455.0000000000000568 ) ) ;
#67674 = ORIENTED_EDGE ( 'NONE', *, *, #55280, .F. ) ;
#67675 = AXIS2_PLACEMENT_3D ( 'NONE', #62284, #46722, #13852 ) ;
#67676 = CARTESIAN_POINT ( 'NONE',  ( 7.250000000000005329, 7.250000000000000888, -9.000000000000001776 ) ) ;
#67677 = FACE_OUTER_BOUND ( 'NONE', #49762, .T. ) ;
#67678 = EDGE_CURVE ( 'NONE', #33741, #6284, #47131, .T. ) ;
#67679 = AXIS2_PLACEMENT_3D ( 'NONE', #41586, #63156, #36285 ) ;
#67680 = DIRECTION ( 'NONE',  ( 0.000000000000000000, 1.000000000000000000, 0.000000000000000000 ) ) ;
#67681 = VERTEX_POINT ( 'NONE', #42860 ) ;
#67682 = LINE ( 'NONE', #62017, #65365 ) ;
#67683 = AXIS2_PLACEMENT_3D ( 'NONE', #54665, #6221, #49373 ) ;
#67684 = CARTESIAN_POINT ( 'NONE',  ( 6.836383711243005479, -4.149127210878733152, 26.00000000000000711 ) ) ;
#67685 = DIRECTION ( 'NONE',  ( 0.000000000000000000, -1.000000000000000000, 0.000000000000000000 ) ) ;
#67686 = VERTEX_POINT ( 'NONE', #57726 ) ;
#67687 = DIRECTION ( 'NONE',  ( 0.7671651518153028704, 0.6414496315691539108, -2.309356642088818463E-17 ) ) ;
#67688 = LINE ( 'NONE', #19248, #55478 ) ;
#67689 = EDGE_CURVE ( 'NONE', #62156, #62419, #57078, .T. ) ;
#67690 = CARTESIAN_POINT ( 'NONE',  ( -6.642976262117334940, -10.31452373788278898, 54.00000000000000711 ) ) ;
#67691 = ORIENTED_EDGE ( 'NONE', *, *, #28188, .F. ) ;
#67692 = ADVANCED_FACE ( 'NONE', ( #63391 ), #64108, .F. ) ;
#67693 = DIRECTION ( 'NONE',  ( 0.000000000000000000, 0.000000000000000000, -1.000000000000000000 ) ) ;
#67694 = DIRECTION ( 'NONE',  ( -1.000000000000000000, 0.000000000000000000, 0.000000000000000000 ) ) ;
#67695 = VERTEX_POINT ( 'NONE', #20248 ) ;
#67696 = FACE_BOUND ( 'NONE', #13427, .T. ) ;
#67697 = DIRECTION ( 'NONE',  ( 1.000000000000000000, 0.000000000000000000, 0.000000000000000000 ) ) ;
#67698 = LINE ( 'NONE', #24918, #29661 ) ;
#67699 = FACE_OUTER_BOUND ( 'NONE', #2161, .T. ) ;
#67700 = DIRECTION ( 'NONE',  ( 0.000000000000000000, 0.000000000000000000, -1.000000000000000000 ) ) ;
#67701 = ORIENTED_EDGE ( 'NONE', *, *, #20696, .T. ) ;
#67702 = FACE_OUTER_BOUND ( 'NONE', #29074, .T. ) ;
#67703 = DIRECTION ( 'NONE',  ( 0.000000000000000000, 1.000000000000000000, 0.000000000000000000 ) ) ;
#67704 = DIRECTION ( 'NONE',  ( -1.000000000000000000, 0.000000000000000000, 0.000000000000000000 ) ) ;
#67705 = CARTESIAN_POINT ( 'NONE',  ( 8.711985858128693749, -2.420780051175180692, 54.00000000000000711 ) ) ;
#67706 = DIRECTION ( 'NONE',  ( -1.000000000000000000, 0.000000000000000000, 0.000000000000000000 ) ) ;
#67707 = ORIENTED_EDGE ( 'NONE', *, *, #49236, .F. ) ;
#67708 = AXIS2_PLACEMENT_3D ( 'NONE', #41626, #20756, #69894 ) ;
#67710 = VERTEX_POINT ( 'NONE', #31919 ) ;
#67709 = DIRECTION ( 'NONE',  ( -1.000000000000000000, 0.000000000000000000, 0.000000000000000000 ) ) ;
#67711 = VECTOR ( 'NONE', #27128, 1000.000000000000000 ) ;
#67712 = ADVANCED_FACE ( 'NONE', ( #14953 ), #37225, .F. ) ;
#67713 = DIRECTION ( 'NONE',  ( -1.000000000000000000, 0.000000000000000000, 0.000000000000000000 ) ) ;
#67714 = EDGE_CURVE ( 'NONE', #2702, #60441, #31231, .T. ) ;
#67715 = DIRECTION ( 'NONE',  ( -1.000000000000000000, 0.000000000000000000, 0.000000000000000000 ) ) ;
#67716 = CARTESIAN_POINT ( 'NONE',  ( 0.000000000000000000, -17.79289321881347163, 20.50000000000002487 ) ) ;
#67717 = VERTEX_POINT ( 'NONE', #10005 ) ;
#67718 = ADVANCED_FACE ( 'NONE', ( #47470 ), #58449, .F. ) ;
#67719 = CIRCLE ( 'NONE', #64307, 0.1999999999999987899 ) ;
#67720 = DIRECTION ( 'NONE',  ( 1.836970198721029934E-16, 1.836970198721010706E-16, -1.000000000000000000 ) ) ;
#67721 = EDGE_CURVE ( 'NONE', #19218, #25597, #4694, .T. ) ;
#67722 = ORIENTED_EDGE ( 'NONE', *, *, #5221, .F. ) ;
#67723 = CONICAL_SURFACE ( 'NONE', #24830, 2.000000000000001776, 0.7853981633974503884 ) ;
#67724 = ORIENTED_EDGE ( 'NONE', *, *, #50520, .F. ) ;
#67725 = EDGE_LOOP ( 'NONE', ( #17333, #52456 ) ) ;
#67727 = EDGE_CURVE ( 'NONE', #13864, #35273, #42161, .T. ) ;
#67726 = CARTESIAN_POINT ( 'NONE',  ( -25.50000000000000355, -15.50000000000000000, 22.50000000000000000 ) ) ;
#67728 = CARTESIAN_POINT ( 'NONE',  ( 7.450000000000006395, 7.250000000000000888, -22.50000000000000000 ) ) ;
#67729 = ADVANCED_FACE ( 'NONE', ( #48180 ), #15302, .F. ) ;
#67730 = VECTOR ( 'NONE', #47449, 1000.000000000000114 ) ;
#67731 = CARTESIAN_POINT ( 'NONE',  ( -7.250000000000001776, -7.249999999999998224, -10.50000000000000000 ) ) ;
#67732 = DIRECTION ( 'NONE',  ( 0.000000000000000000, 0.000000000000000000, 1.000000000000000000 ) ) ;
#67733 = ORIENTED_EDGE ( 'NONE', *, *, #57477, .T. ) ;
#67734 = ORIENTED_EDGE ( 'NONE', *, *, #49956, .T. ) ;
#67735 = CARTESIAN_POINT ( 'NONE',  ( 7.450000000000003730, -7.249999999999997335, -22.50000000000000000 ) ) ;
#67737 = FACE_OUTER_BOUND ( 'NONE', #17720, .T. ) ;
#67736 = AXIS2_PLACEMENT_3D ( 'NONE', #40457, #41510, #62015 ) ;
#67738 = EDGE_LOOP ( 'NONE', ( #2433, #18573, #47730, #63416 ) ) ;
#67739 = ORIENTED_EDGE ( 'NONE', *, *, #42789, .F. ) ;
#67740 = ORIENTED_EDGE ( 'NONE', *, *, #53278, .F. ) ;
#67741 = DIRECTION ( 'NONE',  ( 0.000000000000000000, 0.000000000000000000, -1.000000000000000000 ) ) ;
#67743 = ORIENTED_EDGE ( 'NONE', *, *, #17771, .T. ) ;
#67742 = DIRECTION ( 'NONE',  ( -0.000000000000000000, 3.673940397442059868E-16, -1.000000000000000000 ) ) ;
#67744 = CARTESIAN_POINT ( 'NONE',  ( 275.0000000000000000, -38.09999999999885034, 7.900000000002049383 ) ) ;
#67745 = CARTESIAN_POINT ( 'NONE',  ( 106.4257688009193998, 0.000000000000000000, 285.9830310981789125 ) ) ;
#67746 = AXIS2_PLACEMENT_3D ( 'NONE', #53252, #16802, #9762 ) ;
#67747 = EDGE_CURVE ( 'NONE', #9246, #56820, #64442, .T. ) ;
#67748 = ORIENTED_EDGE ( 'NONE', *, *, #43942, .F. ) ;
#67749 = ORIENTED_EDGE ( 'NONE', *, *, #45257, .F. ) ;
#67750 = ADVANCED_FACE ( 'NONE', ( #32256 ), #5407, .F. ) ;
#67751 = CARTESIAN_POINT ( 'NONE',  ( -9.781776262117247711, 9.781776262117171328, 26.00000000000000711 ) ) ;
#67752 = DIRECTION ( 'NONE',  ( -4.956352788505168198E-15, -1.000000000000000000, 0.000000000000000000 ) ) ;
#67753 = CIRCLE ( 'NONE', #9060, 0.6000000000000006439 ) ;
#67754 = CARTESIAN_POINT ( 'NONE',  ( 39.00000000000000000, 0.000000000000000000, 0.000000000000000000 ) ) ;
#67755 = AXIS2_PLACEMENT_3D ( 'NONE', #46067, #34047, #23458 ) ;
#67756 = EDGE_CURVE ( 'NONE', #53390, #51374, #5744, .T. ) ;
#67757 = VECTOR ( 'NONE', #9001, 1000.000000000000000 ) ;
#67758 = FACE_OUTER_BOUND ( 'NONE', #63797, .T. ) ;
#67759 = CARTESIAN_POINT ( 'NONE',  ( 290.0000000000000000, -0.5000000000000000000, -26.50000000000000000 ) ) ;
#67760 = ORIENTED_EDGE ( 'NONE', *, *, #27585, .F. ) ;
#67761 = ORIENTED_EDGE ( 'NONE', *, *, #43069, .F. ) ;
#67762 = CARTESIAN_POINT ( 'NONE',  ( 0.2499999999999975020, -42.25000000000000000, 26.75000000000000000 ) ) ;
#67764 = DIRECTION ( 'NONE',  ( 0.000000000000000000, -0.000000000000000000, 1.000000000000000000 ) ) ;
#67763 = CIRCLE ( 'NONE', #11288, 2.215251240775983899 ) ;
#67765 = CARTESIAN_POINT ( 'NONE',  ( -2.355476262117319308, -8.835729544836356197, 54.00000000000000711 ) ) ;
#67766 = LINE ( 'NONE', #35948, #58484 ) ;
#67767 = VECTOR ( 'NONE', #59020, 1000.000000000000000 ) ;
#67768 = EDGE_CURVE ( 'NONE', #25046, #46850, #21995, .T. ) ;
#67769 = DIRECTION ( 'NONE',  ( 1.000000000000000000, -1.254221251785257574E-14, 0.000000000000000000 ) ) ;
#67770 = ORIENTED_EDGE ( 'NONE', *, *, #14065, .T. ) ;
#67771 = CARTESIAN_POINT ( 'NONE',  ( -8.697938382363179954, -8.093267424590409931, 26.00000000000000000 ) ) ;
#67773 = AXIS2_PLACEMENT_3D ( 'NONE', #54990, #17137, #44004 ) ;
#67772 = PLANE ( 'NONE',  #33835 ) ;
#67774 = FACE_OUTER_BOUND ( 'NONE', #55738, .T. ) ;
#67775 = AXIS2_PLACEMENT_3D ( 'NONE', #23007, #2476, #50227 ) ;
#67776 = DIRECTION ( 'NONE',  ( -0.000000000000000000, 1.000000000000000000, -0.000000000000000000 ) ) ;
#67777 = CARTESIAN_POINT ( 'NONE',  ( -8.697938382363135545, 8.079219948824830411, 54.00000000000000711 ) ) ;
#67778 = ADVANCED_FACE ( 'NONE', ( #17037 ), #17727, .T. ) ;
#67779 = CARTESIAN_POINT ( 'NONE',  ( 33.89999999999999858, -14.06939075806900874, 20.80000000000001137 ) ) ;
#67780 = EDGE_CURVE ( 'NONE', #39731, #24136, #90, .T. ) ;
#67781 = AXIS2_PLACEMENT_3D ( 'NONE', #7752, #29314, #50886 ) ;
#67782 = CYLINDRICAL_SURFACE ( 'NONE', #35222, 1.000000000000000000 ) ;
#67783 = ORIENTED_EDGE ( 'NONE', *, *, #43642, .F. ) ;
#67784 = DIRECTION ( 'NONE',  ( 1.000000000000000000, -8.903847840905249551E-15, 1.836970198721013664E-16 ) ) ;
#67785 = FACE_OUTER_BOUND ( 'NONE', #54227, .T. ) ;
#67786 = EDGE_CURVE ( 'NONE', #20416, #43624, #67278, .T. ) ;
#67787 = ORIENTED_EDGE ( 'NONE', *, *, #52638, .F. ) ;
#67788 = CARTESIAN_POINT ( 'NONE',  ( 13.90000000000000213, 20.60000000000000142, -13.86939075806900057 ) ) ;
#67789 = EDGE_CURVE ( 'NONE', #30559, #27705, #6433, .T. ) ;
#67790 = ADVANCED_FACE ( 'NONE', ( #6757 ), #48875, .F. ) ;
#67791 = DIRECTION ( 'NONE',  ( 1.000000000000000000, 3.016910393003147986E-15, 0.000000000000000000 ) ) ;
#67792 = CARTESIAN_POINT ( 'NONE',  ( 8.689999999999999503, 8.750000000000000000, -5.000000000000000000 ) ) ;
#67793 = CARTESIAN_POINT ( 'NONE',  ( -3.663616288757091333, -4.149127210878728711, 54.00000000000000711 ) ) ;
#67794 = CARTESIAN_POINT ( 'NONE',  ( 7.000000000000000000, -38.15000000000000568, 14.50000000000000000 ) ) ;
#67795 = ORIENTED_EDGE ( 'NONE', *, *, #35850, .T. ) ;
#67796 = EDGE_CURVE ( 'NONE', #44324, #30449, #27996, .T. ) ;
#67797 = LINE ( 'NONE', #29604, #415 ) ;
#67798 = ORIENTED_EDGE ( 'NONE', *, *, #47052, .F. ) ;
#67799 = CARTESIAN_POINT ( 'NONE',  ( -4.188533722949417282, -4.740315990920197287, 455.0000000000000568 ) ) ;
#67800 = MANIFOLD_SOLID_BREP ( 'LPattern1[21]', #14891 ) ;
#67801 = AXIS2_PLACEMENT_3D ( 'NONE', #14271, #42178, #3660 ) ;
#67802 = EDGE_CURVE ( 'NONE', #18238, #56714, #66159, .T. ) ;
#67803 = DIRECTION ( 'NONE',  ( -0.7071067811865486830, -0.7071067811865464625, 0.000000000000000000 ) ) ;
#67804 = ORIENTED_EDGE ( 'NONE', *, *, #58509, .F. ) ;
#67805 = CARTESIAN_POINT ( 'NONE',  ( -8.250000000000001776, 0.000000000000000000, -8.500000000000000000 ) ) ;
#67806 = ADVANCED_FACE ( 'NONE', ( #7096, #28675, #11037, #37919, #27645 ), #43900, .T. ) ;
#67807 = VERTEX_POINT ( 'NONE', #65478 ) ;
#67808 = CIRCLE ( 'NONE', #64451, 4.000000000000000888 ) ;
#67809 = CARTESIAN_POINT ( 'NONE',  ( -5.993516549646776603, -6.006483450353426790, 455.0000000000000568 ) ) ;
#67810 = ORIENTED_EDGE ( 'NONE', *, *, #7984, .F. ) ;
#67811 = VERTEX_POINT ( 'NONE', #32615 ) ;
#67813 = ADVANCED_FACE ( 'NONE', ( #54185, #60159 ), #50936, .F. ) ;
#67812 = CARTESIAN_POINT ( 'NONE',  ( 275.0000000000000000, -42.50000000000000000, 7.500000000000000000 ) ) ;
#67814 = AXIS2_PLACEMENT_3D ( 'NONE', #55237, #60532, #60870 ) ;
#67815 = ORIENTED_EDGE ( 'NONE', *, *, #60490, .F. ) ;
#67816 = VERTEX_POINT ( 'NONE', #39963 ) ;
#67817 = ADVANCED_FACE ( 'NONE', ( #23378 ), #14155, .F. ) ;
#67818 = DIRECTION ( 'NONE',  ( -0.000000000000000000, -0.000000000000000000, -1.000000000000000000 ) ) ;
#67819 = DIRECTION ( 'NONE',  ( 0.000000000000000000, 0.000000000000000000, -1.000000000000000000 ) ) ;
#67821 = DIRECTION ( 'NONE',  ( 0.000000000000000000, 0.7096009616570518874, -0.7046037717862339012 ) ) ;
#67820 = VECTOR ( 'NONE', #18425, 1000.000000000000000 ) ;
#67822 = ORIENTED_EDGE ( 'NONE', *, *, #57799, .F. ) ;
#67823 = CIRCLE ( 'NONE', #64462, 2.458500000000000796 ) ;
#67824 = CARTESIAN_POINT ( 'NONE',  ( -8.198316549646712303, 5.993516549646603409, 455.0000000000000568 ) ) ;
#67826 = DIRECTION ( 'NONE',  ( -0.000000000000000000, 3.673940397442059868E-16, -1.000000000000000000 ) ) ;
#67825 = DIRECTION ( 'NONE',  ( 0.000000000000000000, 0.7046037717862339012, 0.7096009616570518874 ) ) ;
#67827 = ORIENTED_EDGE ( 'NONE', *, *, #55981, .F. ) ;
#67829 = EDGE_LOOP ( 'NONE', ( #55256, #13962, #31554, #12502 ) ) ;
#67828 = CARTESIAN_POINT ( 'NONE',  ( 33.89999999999999858, 0.000000000000000000, 0.000000000000000000 ) ) ;
#67830 = VERTEX_POINT ( 'NONE', #57297 ) ;
#67831 = APPLICATION_PROTOCOL_DEFINITION ( 'draft international standard', 'automotive_design', 1998, #30935 ) ;
#67832 = CARTESIAN_POINT ( 'NONE',  ( -7.250000000000000888, 7.250000000000001776, -23.50000000000000000 ) ) ;
#67834 = ORIENTED_EDGE ( 'NONE', *, *, #3015, .T. ) ;
#67833 = CARTESIAN_POINT ( 'NONE',  ( 0.000000000000000000, 20.50000000000000000, -17.79289321881345032 ) ) ;
#67835 = AXIS2_PLACEMENT_3D ( 'NONE', #44309, #38340, #877 ) ;
#67836 = DIRECTION ( 'NONE',  ( 0.000000000000000000, 0.000000000000000000, -1.000000000000000000 ) ) ;
#67837 = DIRECTION ( 'NONE',  ( 0.000000000000000000, 0.000000000000000000, -1.000000000000000000 ) ) ;
#67838 = ORIENTED_EDGE ( 'NONE', *, *, #20237, .T. ) ;
#67839 = ORIENTED_EDGE ( 'NONE', *, *, #19092, .F. ) ;
#67840 = CIRCLE ( 'NONE', #28313, 1.620999999999997332 ) ;
#67841 = CARTESIAN_POINT ( 'NONE',  ( -3.663616288757090000, -6.364920264886882784, 26.00000000000000711 ) ) ;
#67842 = EDGE_LOOP ( 'NONE', ( #22443, #22244, #62330, #42764 ) ) ;
#67843 = EDGE_CURVE ( 'NONE', #36514, #22100, #55966, .T. ) ;
#67844 = CARTESIAN_POINT ( 'NONE',  ( -29.50000000000000355, -12.00000000000000000, -10.69999999999999929 ) ) ;
#67845 = LINE ( 'NONE', #46613, #39111 ) ;
#67846 = CARTESIAN_POINT ( 'NONE',  ( 7.250000000000005329, 7.250000000000000888, -16.50000000000000000 ) ) ;
#67847 = ORIENTED_EDGE ( 'NONE', *, *, #18195, .F. ) ;
#67848 = EDGE_CURVE ( 'NONE', #36598, #44196, #1752, .T. ) ;
#67849 = CARTESIAN_POINT ( 'NONE',  ( 0.000000000000000000, 20.50000000000000000, -17.79289321881345032 ) ) ;
#67850 = DIRECTION ( 'NONE',  ( -0.000000000000000000, 3.673940397442059868E-16, -1.000000000000000000 ) ) ;
#67852 = ORIENTED_EDGE ( 'NONE', *, *, #34646, .T. ) ;
#67851 = LINE ( 'NONE', #19403, #68143 ) ;
#67854 = ORIENTED_EDGE ( 'NONE', *, *, #28508, .F. ) ;
#67853 = DIRECTION ( 'NONE',  ( 0.000000000000000000, 1.000000000000000000, 0.000000000000000000 ) ) ;
#67855 = EDGE_CURVE ( 'NONE', #26901, #30052, #66846, .T. ) ;
#67856 = DIRECTION ( 'NONE',  ( -0.000000000000000000, 1.000000000000000000, -0.000000000000000000 ) ) ;
#67857 = CARTESIAN_POINT ( 'NONE',  ( -8.697938382363135545, 2.406732575409538111, 26.00000000000000711 ) ) ;
#67858 = EDGE_CURVE ( 'NONE', #49899, #66965, #44695, .T. ) ;
#67859 = FACE_OUTER_BOUND ( 'NONE', #21507, .T. ) ;
#67860 = CARTESIAN_POINT ( 'NONE',  ( 8.250000000000005329, 7.250000000000000888, -12.50000000000000000 ) ) ;
#67861 = EDGE_CURVE ( 'NONE', #21718, #35045, #62242, .T. ) ;
#67862 = LINE ( 'NONE', #36030, #321 ) ;
#67863 = ORIENTED_EDGE ( 'NONE', *, *, #30269, .T. ) ;
#67864 = CARTESIAN_POINT ( 'NONE',  ( 0.5000000000000000000, 0.000000000000000000, 26.50000000000000000 ) ) ;
#67865 = DIRECTION ( 'NONE',  ( 0.000000000000000000, -1.000000000000000000, 0.000000000000000000 ) ) ;
#67866 = CIRCLE ( 'NONE', #36213, 3.499999999999040323 ) ;
#67867 = DIRECTION ( 'NONE',  ( 0.000000000000000000, -1.000000000000000000, -3.673940397442059868E-16 ) ) ;
#67869 = ORIENTED_EDGE ( 'NONE', *, *, #35385, .T. ) ;
#67868 = CARTESIAN_POINT ( 'NONE',  ( 7.450000000000003730, -7.249999999999997335, -16.50000000000000000 ) ) ;
#67870 = PRODUCT_DEFINITION_SHAPE ( 'NONE', 'NONE',  #18371 ) ;
#67871 = AXIS2_PLACEMENT_3D ( 'NONE', #24455, #23751, #61562 ) ;
#67872 = LINE ( 'NONE', #19425, #66295 ) ;
#67873 = DIRECTION ( 'NONE',  ( -1.000000000000000000, 0.000000000000000000, 0.000000000000000000 ) ) ;
#67874 = VECTOR ( 'NONE', #16223, 1000.000000000000000 ) ;
#67875 = VERTEX_POINT ( 'NONE', #34310 ) ;
#67876 = EDGE_LOOP ( 'NONE', ( #7282, #60615, #248, #789 ) ) ;
#67877 = DIRECTION ( 'NONE',  ( 1.000000000000000000, -0.000000000000000000, 0.000000000000000000 ) ) ;
#67878 = CARTESIAN_POINT ( 'NONE',  ( 283.0000000000000568, -37.14999999999894698, -8.200000000002349410 ) ) ;
#67879 = VERTEX_POINT ( 'NONE', #13103 ) ;
#67880 = VECTOR ( 'NONE', #61255, 1000.000000000000000 ) ;
#67881 = EDGE_CURVE ( 'NONE', #51768, #65806, #29363, .T. ) ;
#67882 = AXIS2_PLACEMENT_3D ( 'NONE', #22853, #44400, #65975 ) ;
#67883 = FACE_OUTER_BOUND ( 'NONE', #12861, .T. ) ;
#67884 = DIRECTION ( 'NONE',  ( 0.000000000000000000, -0.7071067811865455743, 0.7071067811865495711 ) ) ;
#67885 = CARTESIAN_POINT ( 'NONE',  ( -7.250000000000000888, -8.249999999999998224, -26.00000000000001066 ) ) ;
#67886 = CONICAL_SURFACE ( 'NONE', #3539, 2.458500000000000796, 1.047019301333029784 ) ;
#67887 = CARTESIAN_POINT ( 'NONE',  ( 10.92648345035337343, -2.706483450353395437, 195.0000000000000284 ) ) ;
#67888 = ORIENTED_EDGE ( 'NONE', *, *, #43364, .T. ) ;
#67889 = CARTESIAN_POINT ( 'NONE',  ( -7.172176262117278434, -5.257023737882785319, 54.00000000000000711 ) ) ;
#67890 = VERTEX_POINT ( 'NONE', #18764 ) ;
#67891 = ORIENTED_EDGE ( 'NONE', *, *, #67727, .T. ) ;
#67892 = VERTEX_POINT ( 'NONE', #39623 ) ;
#67893 = CARTESIAN_POINT ( 'NONE',  ( 10.92648345035337343, -9.306483450353395526, 195.0000000000000284 ) ) ;
#67894 = VECTOR ( 'NONE', #25623, 1000.000000000000000 ) ;
#67895 = CARTESIAN_POINT ( 'NONE',  ( 29.50000000000000355, -11.50000000000100009, 15.00000000000084910 ) ) ;
#67896 = CYLINDRICAL_SURFACE ( 'NONE', #25370, 0.5000000000001374456 ) ;
#67897 = VERTEX_POINT ( 'NONE', #55897 ) ;
#67898 = EDGE_LOOP ( 'NONE', ( #50735, #23412, #33997, #42228 ) ) ;
#67900 = EDGE_CURVE ( 'NONE', #20521, #23324, #50313, .T. ) ;
#67899 = FACE_OUTER_BOUND ( 'NONE', #32956, .T. ) ;
#67901 = VERTEX_POINT ( 'NONE', #61182 ) ;
#67902 = VERTEX_POINT ( 'NONE', #35357 ) ;
#67903 = EDGE_CURVE ( 'NONE', #32604, #28065, #13807, .T. ) ;
#67904 = LINE ( 'NONE', #2148, #30420 ) ;
#67905 = FACE_OUTER_BOUND ( 'NONE', #67898, .T. ) ;
#67906 = DIRECTION ( 'NONE',  ( -1.000000000000000000, 0.000000000000000000, 0.000000000000000000 ) ) ;
#67907 = AXIS2_PLACEMENT_3D ( 'NONE', #64555, #52548, #42625 ) ;
#67908 = LINE ( 'NONE', #14153, #39891 ) ;
#67909 = ORIENTED_EDGE ( 'NONE', *, *, #43239, .F. ) ;
#67910 = CARTESIAN_POINT ( 'NONE',  ( 9.562023737882812569, -8.144523737882824577, 54.00000000000000711 ) ) ;
#67912 = DIRECTION ( 'NONE',  ( -1.000000000000000000, 0.000000000000000000, 0.000000000000000000 ) ) ;
#67911 = CARTESIAN_POINT ( 'NONE',  ( 75.42576880091934299, 0.000000000000000000, 330.9830310981789694 ) ) ;
#67913 = ORIENTED_EDGE ( 'NONE', *, *, #36667, .T. ) ;
#67915 = VERTEX_POINT ( 'NONE', #67910 ) ;
#67914 = DIRECTION ( 'NONE',  ( -1.000000000000000000, 0.000000000000000000, 0.000000000000000000 ) ) ;
#67916 = ORIENTED_EDGE ( 'NONE', *, *, #49236, .T. ) ;
#67917 = VERTEX_POINT ( 'NONE', #7450 ) ;
#67918 = DIRECTION ( 'NONE',  ( 0.000000000000000000, 0.000000000000000000, -1.000000000000000000 ) ) ;
#67919 = VECTOR ( 'NONE', #20286, 1000.000000000000000 ) ;
#67920 = CARTESIAN_POINT ( 'NONE',  ( -10.19191654964671301, 9.791916549646639822, 455.0000000000000568 ) ) ;
#67921 = CIRCLE ( 'NONE', #37448, 0.1999999999999987899 ) ;
#67922 = EDGE_LOOP ( 'NONE', ( #51282, #9860, #31234, #7551 ) ) ;
#67923 = VERTEX_POINT ( 'NONE', #1803 ) ;
#67924 = CARTESIAN_POINT ( 'NONE',  ( 25.57999999999999829, 0.000000000000000000, 0.000000000000000000 ) ) ;
#67925 = DIRECTION ( 'NONE',  ( 0.000000000000000000, 0.7057491738665938596, 0.7084617869628679898 ) ) ;
#67926 = ORIENTED_EDGE ( 'NONE', *, *, #34412, .F. ) ;
#67927 = VECTOR ( 'NONE', #11367, 1000.000000000000000 ) ;
#67928 = VECTOR ( 'NONE', #31821, 1000.000000000000000 ) ;
#67929 = EDGE_LOOP ( 'NONE', ( #53723, #3481, #12055, #3707 ) ) ;
#67930 = CARTESIAN_POINT ( 'NONE',  ( -7.750000000000001776, -7.348062532927999158, -5.000000000000000000 ) ) ;
#67931 = LINE ( 'NONE', #58019, #66640 ) ;
#67932 = ORIENTED_EDGE ( 'NONE', *, *, #37497, .T. ) ;
#67933 = AXIS2_PLACEMENT_3D ( 'NONE', #17362, #66151, #1792 ) ;
#67934 = EDGE_CURVE ( 'NONE', #17842, #16692, #2153, .T. ) ;
#67935 = DIRECTION ( 'NONE',  ( -0.000000000000000000, 3.673940397442059868E-16, -1.000000000000000000 ) ) ;
#67936 = LINE ( 'NONE', #34700, #42984 ) ;
#67938 = VERTEX_POINT ( 'NONE', #23717 ) ;
#67937 =( NAMED_UNIT ( * ) PLANE_ANGLE_UNIT ( ) SI_UNIT ( $, .RADIAN. ) );
#67939 = EDGE_LOOP ( 'NONE', ( #65557, #37309, #62378, #53084 ) ) ;
#67940 = ADVANCED_FACE ( 'NONE', ( #45273 ), #35015, .F. ) ;
#67942 = LINE ( 'NONE', #7826, #29388 ) ;
#67941 = VECTOR ( 'NONE', #17690, 1000.000000000000000 ) ;
#67943 = FILL_AREA_STYLE ('',( #10202 ) ) ;
#67944 = DIRECTION ( 'NONE',  ( -0.000000000000000000, 0.000000000000000000, 1.000000000000000000 ) ) ;
#67945 = EDGE_CURVE ( 'NONE', #39379, #35639, #57130, .T. ) ;
#67946 = CARTESIAN_POINT ( 'NONE',  ( 41.09999999999999432, 13.66939075806899950, -20.80000000000000426 ) ) ;
#67947 = EDGE_CURVE ( 'NONE', #38194, #51551, #8495, .T. ) ;
#67948 = DIRECTION ( 'NONE',  ( -1.000000000000000000, 0.000000000000000000, 0.000000000000000000 ) ) ;
#67949 = CARTESIAN_POINT ( 'NONE',  ( 30.00000000000000000, -9.487228132326899654, 12.50000000000000000 ) ) ;
#67950 = EDGE_CURVE ( 'NONE', #14058, #48542, #24777, .T. ) ;
#67951 = EDGE_CURVE ( 'NONE', #25681, #8234, #62588, .T. ) ;
#67952 = LINE ( 'NONE', #61572, #46010 ) ;
#67953 = EDGE_LOOP ( 'NONE', ( #59493, #44851, #65562, #34562 ) ) ;
#67954 = LINE ( 'NONE', #14201, #65415 ) ;
#67956 = ORIENTED_EDGE ( 'NONE', *, *, #40224, .F. ) ;
#67955 = DIRECTION ( 'NONE',  ( 1.000000000000000000, 0.000000000000000000, 0.000000000000000000 ) ) ;
#67957 = DIRECTION ( 'NONE',  ( 0.000000000000000000, 0.000000000000000000, 1.000000000000000000 ) ) ;
#67958 = CARTESIAN_POINT ( 'NONE',  ( 6.006483450353379716, -6.006483450353490738, 455.0000000000000568 ) ) ;
#67959 = EDGE_CURVE ( 'NONE', #18593, #21803, #47737, .T. ) ;
#67960 = VECTOR ( 'NONE', #15686, 1000.000000000000000 ) ;
#67961 = DIRECTION ( 'NONE',  ( 1.000000000000000000, 0.000000000000000000, 0.000000000000000000 ) ) ;
#67962 = CARTESIAN_POINT ( 'NONE',  ( -10.08346604330788132, -2.706483450353354581, 455.0000000000000568 ) ) ;
#67963 = ORIENTED_EDGE ( 'NONE', *, *, #31422, .F. ) ;
#67964 = FACE_OUTER_BOUND ( 'NONE', #69284, .T. ) ;
#67965 = DIRECTION ( 'NONE',  ( 0.000000000000000000, 0.000000000000000000, 1.000000000000000000 ) ) ;
#67966 = ORIENTED_EDGE ( 'NONE', *, *, #6899, .T. ) ;
#67967 = CYLINDRICAL_SURFACE ( 'NONE', #51663, 0.2000000000000005107 ) ;
#67968 = AXIS2_PLACEMENT_3D ( 'NONE', #50883, #6381, #60456 ) ;
#67969 = FACE_OUTER_BOUND ( 'NONE', #68797, .T. ) ;
#67970 = EDGE_LOOP ( 'NONE', ( #28639, #20972, #53386, #63915 ) ) ;
#67971 = DIRECTION ( 'NONE',  ( -1.000000000000000000, 0.000000000000000000, 0.000000000000000000 ) ) ;
#67972 = ORIENTED_EDGE ( 'NONE', *, *, #59637, .T. ) ;
#67973 = ORIENTED_EDGE ( 'NONE', *, *, #49660, .T. ) ;
#67974 = PLANE ( 'NONE',  #51624 ) ;
#67975 = DIRECTION ( 'NONE',  ( 1.000000000000000000, -1.883404846338789915E-14, 1.836970198720995421E-16 ) ) ;
#67976 = DIRECTION ( 'NONE',  ( 0.000000000000000000, 0.000000000000000000, -1.000000000000000000 ) ) ;
#67977 = CIRCLE ( 'NONE', #14939, 0.7499999999999997780 ) ;
#67978 = VECTOR ( 'NONE', #11606, 1000.000000000000114 ) ;
#67979 = DIRECTION ( 'NONE',  ( 0.000000000000000000, 0.000000000000000000, -1.000000000000000000 ) ) ;
#67980 = CARTESIAN_POINT ( 'NONE',  ( -6.749999999999998224, 7.750000000000001776, -5.000000000000000000 ) ) ;
#67981 = ORIENTED_EDGE ( 'NONE', *, *, #50109, .F. ) ;
#67982 = ORIENTED_EDGE ( 'NONE', *, *, #22610, .T. ) ;
#67984 = VERTEX_POINT ( 'NONE', #31140 ) ;
#67983 = DIRECTION ( 'NONE',  ( 0.000000000000000000, 0.000000000000000000, -1.000000000000000000 ) ) ;
#67985 = AXIS2_PLACEMENT_3D ( 'NONE', #51643, #14146, #15216 ) ;
#67986 = VERTEX_POINT ( 'NONE', #4619 ) ;
#67987 = EDGE_CURVE ( 'NONE', #26595, #35004, #31160, .T. ) ;
#67988 = CYLINDRICAL_SURFACE ( 'NONE', #10093, 0.5000000000000000000 ) ;
#67989 = CARTESIAN_POINT ( 'NONE',  ( 41.09999999999999432, -21.00000000000000000, -13.86939075806900057 ) ) ;
#67990 = DIRECTION ( 'NONE',  ( -1.000000000000000000, 0.000000000000000000, 0.000000000000000000 ) ) ;
#67991 = FACE_BOUND ( 'NONE', #19466, .T. ) ;
#67992 = EDGE_CURVE ( 'NONE', #68319, #63525, #662, .T. ) ;
#67993 = EDGE_CURVE ( 'NONE', #68976, #29522, #57646, .T. ) ;
#67994 = VECTOR ( 'NONE', #56559, 1000.000000000000000 ) ;
#67995 = FACE_OUTER_BOUND ( 'NONE', #60795, .T. ) ;
#67996 = DIRECTION ( 'NONE',  ( 0.000000000000000000, 0.7084617869628681008, -0.7057491738665939707 ) ) ;
#67997 = ORIENTED_EDGE ( 'NONE', *, *, #10358, .T. ) ;
#67998 = ORIENTED_EDGE ( 'NONE', *, *, #55873, .F. ) ;
#67999 = EDGE_CURVE ( 'NONE', #1121, #13935, #40156, .T. ) ;
#68000 = EDGE_LOOP ( 'NONE', ( #7867, #22020, #45678, #27540 ) ) ;
#68001 = VERTEX_POINT ( 'NONE', #9217 ) ;
#68002 = DIRECTION ( 'NONE',  ( 0.000000000000000000, 0.000000000000000000, -1.000000000000000000 ) ) ;
#68003 = DIRECTION ( 'NONE',  ( 0.6414496315691367023, -0.7671651518153173033, -2.309356642089295169E-17 ) ) ;
#68004 = CARTESIAN_POINT ( 'NONE',  ( 15.50000000000000000, -0.2000000000000000111, 25.80000000297970075 ) ) ;
#68005 = ORIENTED_EDGE ( 'NONE', *, *, #63689, .T. ) ;
#68006 = VERTEX_POINT ( 'NONE', #4276 ) ;
#68007 = ORIENTED_EDGE ( 'NONE', *, *, #38153, .T. ) ;
#68008 = DIRECTION ( 'NONE',  ( 0.000000000000000000, -0.9239212585478484563, -0.3825826812642726948 ) ) ;
#68009 = ORIENTED_EDGE ( 'NONE', *, *, #58543, .T. ) ;
#68010 = ORIENTED_EDGE ( 'NONE', *, *, #33394, .F. ) ;
#68011 = CARTESIAN_POINT ( 'NONE',  ( 9.690000000000001279, -9.750000000000001776, -7.000000000000000000 ) ) ;
#68012 = AXIS2_PLACEMENT_3D ( 'NONE', #12622, #56132, #7676 ) ;
#68013 = ORIENTED_EDGE ( 'NONE', *, *, #44666, .F. ) ;
#68014 = ORIENTED_EDGE ( 'NONE', *, *, #40090, .F. ) ;
#68015 = CARTESIAN_POINT ( 'NONE',  ( 41.09999999999999432, -14.06939075806900163, 20.80000000000000426 ) ) ;
#68016 = VECTOR ( 'NONE', #28200, 1000.000000000000000 ) ;
#68018 = ORIENTED_EDGE ( 'NONE', *, *, #55150, .T. ) ;
#68017 = DIRECTION ( 'NONE',  ( 0.000000000000000000, 0.000000000000000000, -1.000000000000000000 ) ) ;
#68019 = ORIENTED_EDGE ( 'NONE', *, *, #11342, .T. ) ;
#68020 = FACE_OUTER_BOUND ( 'NONE', #28345, .T. ) ;
#68021 = EDGE_CURVE ( 'NONE', #2849, #67686, #59359, .T. ) ;
#68022 = DIRECTION ( 'NONE',  ( 0.000000000000000000, 1.000000000000000000, 0.000000000000000000 ) ) ;
#68023 = FACE_OUTER_BOUND ( 'NONE', #15922, .T. ) ;
#68025 = ORIENTED_EDGE ( 'NONE', *, *, #2560, .F. ) ;
#68024 = DIRECTION ( 'NONE',  ( -0.000000000000000000, -0.000000000000000000, -1.000000000000000000 ) ) ;
#68026 = ORIENTED_EDGE ( 'NONE', *, *, #4014, .T. ) ;
#68027 = CARTESIAN_POINT ( 'NONE',  ( -1.853252480934882707, -9.417013320880883498, 455.0000000000000568 ) ) ;
#68028 = FACE_OUTER_BOUND ( 'NONE', #32583, .T. ) ;
#68029 = VECTOR ( 'NONE', #54267, 1000.000000000000000 ) ;
#68030 = DIRECTION ( 'NONE',  ( 0.000000000000000000, 0.000000000000000000, 1.000000000000000000 ) ) ;
#68031 = PLANE ( 'NONE',  #31625 ) ;
#68032 = EDGE_CURVE ( 'NONE', #47318, #31506, #25477, .T. ) ;
#68033 = ORIENTED_EDGE ( 'NONE', *, *, #29934, .F. ) ;
#68034 = DIRECTION ( 'NONE',  ( 1.000000000000000000, -0.000000000000000000, -0.000000000000000000 ) ) ;
#68035 = CARTESIAN_POINT ( 'NONE',  ( -4.173516549646839380, -12.00648345035344811, 455.0000000000000568 ) ) ;
#68036 = VECTOR ( 'NONE', #4778, 1000.000000000000000 ) ;
#68037 = CARTESIAN_POINT ( 'NONE',  ( -11.75000000000000000, -5.200000000000001066, -11.75000000000000000 ) ) ;
#68038 = EDGE_CURVE ( 'NONE', #66121, #26706, #20868, .T. ) ;
#68039 = EDGE_LOOP ( 'NONE', ( #55059, #68726, #3976, #13440 ) ) ;
#68040 = DIRECTION ( 'NONE',  ( -1.836970198721029934E-16, 1.836970198721036590E-16, -1.000000000000000000 ) ) ;
#68042 = DIRECTION ( 'NONE',  ( 0.000000000000000000, 0.000000000000000000, -1.000000000000000000 ) ) ;
#68041 = AXIS2_PLACEMENT_3D ( 'NONE', #66029, #17597, #2036 ) ;
#68043 = VECTOR ( 'NONE', #7854, 1000.000000000000000 ) ;
#68044 = DIRECTION ( 'NONE',  ( -1.836970198721029934E-16, 1.836970198721036590E-16, -1.000000000000000000 ) ) ;
#68045 = VERTEX_POINT ( 'NONE', #48094 ) ;
#68046 = CARTESIAN_POINT ( 'NONE',  ( -3.834182069070765309, 7.342976262117171693, 26.00000000000000711 ) ) ;
#68047 = VECTOR ( 'NONE', #27516, 1000.000000000000114 ) ;
#68048 = DIRECTION ( 'NONE',  ( -1.047444401652939849E-14, -1.000000000000000000, -1.836970198721029934E-16 ) ) ;
#68049 = VECTOR ( 'NONE', #13124, 1000.000000000000000 ) ;
#68050 = CARTESIAN_POINT ( 'NONE',  ( 7.250000000000005329, 7.250000000000000888, -17.50000000000000000 ) ) ;
#68051 = ORIENTED_EDGE ( 'NONE', *, *, #39684, .F. ) ;
#68052 = CARTESIAN_POINT ( 'NONE',  ( -11.50000000000000000, -11.50000000000000000, -19.00000000000000000 ) ) ;
#68053 = FACE_OUTER_BOUND ( 'NONE', #19521, .T. ) ;
#68054 = FACE_OUTER_BOUND ( 'NONE', #36985, .T. ) ;
#68055 = CYLINDRICAL_SURFACE ( 'NONE', #44779, 0.3000000000005393908 ) ;
#68056 = LINE ( 'NONE', #41174, #17272 ) ;
#68057 = ORIENTED_EDGE ( 'NONE', *, *, #42758, .F. ) ;
#68058 = DIRECTION ( 'NONE',  ( 0.000000000000000000, -1.000000000000000000, 0.000000000000000000 ) ) ;
#68059 = DIRECTION ( 'NONE',  ( 0.000000000000000000, 0.000000000000000000, -1.000000000000000000 ) ) ;
#68060 = AXIS2_PLACEMENT_3D ( 'NONE', #57094, #2645, #34816 ) ;
#68061 = CARTESIAN_POINT ( 'NONE',  ( 12.00648345035338238, 4.173516549646515195, 455.0000000000000568 ) ) ;
#68062 = CYLINDRICAL_SURFACE ( 'NONE', #28604, 1.399999999999998579 ) ;
#68063 = CARTESIAN_POINT ( 'NONE',  ( -30.00000000000000000, -14.04000000000000092, 14.80000000000000071 ) ) ;
#68064 = VECTOR ( 'NONE', #41240, 1000.000000000000000 ) ;
#68065 = VERTEX_POINT ( 'NONE', #37488 ) ;
#68067 = ORIENTED_EDGE ( 'NONE', *, *, #36331, .T. ) ;
#68066 = CARTESIAN_POINT ( 'NONE',  ( -15.50000000000000000, -5.000000000000000000, -22.50000000000000000 ) ) ;
#68068 = CARTESIAN_POINT ( 'NONE',  ( 0.000000000000000000, -8.249999999999998224, -16.00000000000000000 ) ) ;
#68069 = CARTESIAN_POINT ( 'NONE',  ( 7.250000000000005329, -7.249999999999998224, -26.00000000000001066 ) ) ;
#68070 = DIRECTION ( 'NONE',  ( -0.000000000000000000, 3.673940397442059868E-16, -1.000000000000000000 ) ) ;
#68071 = ORIENTED_EDGE ( 'NONE', *, *, #62743, .T. ) ;
#68072 = ADVANCED_FACE ( 'NONE', ( #57996 ), #20516, .F. ) ;
#68073 = CARTESIAN_POINT ( 'NONE',  ( 7.250000000000005329, -7.249999999999998224, -16.50000000000000000 ) ) ;
#68074 = ORIENTED_EDGE ( 'NONE', *, *, #45765, .T. ) ;
#68075 = ADVANCED_FACE ( 'NONE', ( #47043 ), #25125, .T. ) ;
#68076 = ORIENTED_EDGE ( 'NONE', *, *, #19413, .F. ) ;
#68077 = ORIENTED_EDGE ( 'NONE', *, *, #7997, .T. ) ;
#68078 = CARTESIAN_POINT ( 'NONE',  ( 7.250000000000005329, -7.249999999999998224, -26.00000000000001066 ) ) ;
#68079 = DIRECTION ( 'NONE',  ( 1.000000000000000000, -1.185108578570163560E-14, 0.000000000000000000 ) ) ;
#68080 = CARTESIAN_POINT ( 'NONE',  ( -7.250000000000001776, -7.249999999999998224, -26.00000000000001066 ) ) ;
#68081 = FACE_OUTER_BOUND ( 'NONE', #8947, .T. ) ;
#68082 = CIRCLE ( 'NONE', #33101, 2.204799999999999205 ) ;
#68083 = ORIENTED_EDGE ( 'NONE', *, *, #62615, .T. ) ;
#68084 = VERTEX_POINT ( 'NONE', #63307 ) ;
#68085 = CARTESIAN_POINT ( 'NONE',  ( -8.452095193409387974, -4.255011587777191906, 195.0000000000000284 ) ) ;
#68086 = VECTOR ( 'NONE', #55026, 1000.000000000000000 ) ;
#68087 = CARTESIAN_POINT ( 'NONE',  ( -8.452095193409402185, 7.744988412222746810, 195.0000000000000284 ) ) ;
#68088 = ORIENTED_EDGE ( 'NONE', *, *, #3877, .T. ) ;
#68089 = STYLED_ITEM ( 'NONE', ( #31388 ), #65930 ) ;
#68090 = EDGE_LOOP ( 'NONE', ( #21150, #59250, #10244, #54477 ) ) ;
#68091 = ORIENTED_EDGE ( 'NONE', *, *, #7230, .F. ) ;
#68092 = ORIENTED_EDGE ( 'NONE', *, *, #64860, .T. ) ;
#68093 = EDGE_CURVE ( 'NONE', #63685, #13194, #24428, .T. ) ;
#68094 = DIRECTION ( 'NONE',  ( 0.000000000000000000, 1.000000000000000000, 0.000000000000000000 ) ) ;
#68095 = VECTOR ( 'NONE', #57508, 1000.000000000000000 ) ;
#68097 = ORIENTED_EDGE ( 'NONE', *, *, #17853, .F. ) ;
#68096 = DIRECTION ( 'NONE',  ( 2.135044278125301343E-15, -1.000000000000000000, -3.673940397442059868E-16 ) ) ;
#68098 = CARTESIAN_POINT ( 'NONE',  ( 4.747751991980625696, -5.393625297349947445, 195.0000000000000284 ) ) ;
#68099 = VECTOR ( 'NONE', #28267, 1000.000000000000000 ) ;
#68100 = CARTESIAN_POINT ( 'NONE',  ( 4.206483450353373676, 11.11351654964663282, 195.0000000000000284 ) ) ;
#68101 = EDGE_LOOP ( 'NONE', ( #33307, #46279, #30632, #63079 ) ) ;
#68102 = EDGE_LOOP ( 'NONE', ( #28486, #30752, #7254, #20606 ) ) ;
#68103 = VECTOR ( 'NONE', #16412, 1000.000000000000000 ) ;
#68104 = DIRECTION ( 'NONE',  ( -1.000000000000000000, 0.000000000000000000, 0.000000000000000000 ) ) ;
#68105 = CIRCLE ( 'NONE', #34212, 0.5000000000009320322 ) ;
#68106 = CARTESIAN_POINT ( 'NONE',  ( 283.0000000000000568, -26.06132420600899735, 10.13999572156699891 ) ) ;
#68107 = EDGE_CURVE ( 'NONE', #26429, #3987, #9568, .T. ) ;
#68108 = DIRECTION ( 'NONE',  ( 0.000000000000000000, 0.000000000000000000, 1.000000000000000000 ) ) ;
#68109 = CARTESIAN_POINT ( 'NONE',  ( 39.00000000000000000, -21.00000000000000000, -14.57806571531351914 ) ) ;
#68110 = EDGE_CURVE ( 'NONE', #65403, #4106, #26182, .T. ) ;
#68111 = EDGE_CURVE ( 'NONE', #24412, #44389, #33461, .T. ) ;
#68112 = ORIENTED_EDGE ( 'NONE', *, *, #55194, .T. ) ;
#68113 = AXIS2_PLACEMENT_3D ( 'NONE', #21915, #44163, #59746 ) ;
#68114 = CARTESIAN_POINT ( 'NONE',  ( 7.450000000000004619, -1.336933437520057563E-15, -22.50000000000000000 ) ) ;
#68115 = CARTESIAN_POINT ( 'NONE',  ( 0.000000000000000000, -8.249999999999998224, -25.00000000000000000 ) ) ;
#68116 = CARTESIAN_POINT ( 'NONE',  ( -11.00000000000000000, -8.959999999999999076, 17.04524521594300523 ) ) ;
#68117 = ADVANCED_FACE ( 'NONE', ( #59047 ), #53064, .T. ) ;
#68118 = CARTESIAN_POINT ( 'NONE',  ( 5.393625297349900372, -7.265214908726231435, 455.0000000000000568 ) ) ;
#68119 = ADVANCED_FACE ( 'NONE', ( #19803 ), #4959, .T. ) ;
#68120 = EDGE_CURVE ( 'NONE', #35525, #11608, #43470, .T. ) ;
#68121 = DIRECTION ( 'NONE',  ( -1.794541526872559352E-16, -1.000000000000000000, 0.000000000000000000 ) ) ;
#68122 = EDGE_CURVE ( 'NONE', #21711, #33281, #54443, .T. ) ;
#68123 = ORIENTED_EDGE ( 'NONE', *, *, #43503, .F. ) ;
#68124 = CARTESIAN_POINT ( 'NONE',  ( -4.193516549646782998, -11.12648345035339581, 195.0000000000000284 ) ) ;
#68125 = CARTESIAN_POINT ( 'NONE',  ( -3.650476262117329007, -10.31452373788281385, 26.00000000000000000 ) ) ;
#68126 = EDGE_CURVE ( 'NONE', #24168, #57618, #52663, .T. ) ;
#68127 = CARTESIAN_POINT ( 'NONE',  ( 6.344579767990823349, -8.406483450353396947, 195.0000000000000284 ) ) ;
#68128 = VECTOR ( 'NONE', #19861, 1000.000000000000000 ) ;
#68129 = AXIS2_PLACEMENT_3D ( 'NONE', #46330, #10510, #13455 ) ;
#68130 = LINE ( 'NONE', #14399, #66517 ) ;
#68131 = DIRECTION ( 'NONE',  ( 0.7671651518153065341, -0.6414496315691495809, 0.000000000000000000 ) ) ;
#68132 = CYLINDRICAL_SURFACE ( 'NONE', #5316, 0.2000000000000000944 ) ;
#68133 = FACE_OUTER_BOUND ( 'NONE', #13091, .T. ) ;
#68134 = CIRCLE ( 'NONE', #7147, 0.2000000000005226763 ) ;
#68135 = EDGE_LOOP ( 'NONE', ( #14162, #8751, #65179, #41146 ) ) ;
#68136 = CIRCLE ( 'NONE', #39898, 0.5000000000009302559 ) ;
#68137 = CARTESIAN_POINT ( 'NONE',  ( 15.29633693294940500, -0.2717122460100945269, 23.82579074638835692 ) ) ;
#68138 = CARTESIAN_POINT ( 'NONE',  ( 275.0000000000000000, -41.99999999999906208, 14.49999999999903899 ) ) ;
#68139 = ORIENTED_EDGE ( 'NONE', *, *, #67689, .F. ) ;
#68140 = CARTESIAN_POINT ( 'NONE',  ( 22.14589803375000088, -17.50000000000000000, -21.50000000000000000 ) ) ;
#68141 = DIRECTION ( 'NONE',  ( 3.016910393003147986E-15, -1.000000000000000000, 0.000000000000000000 ) ) ;
#68142 = DIRECTION ( 'NONE',  ( -1.000000000000000000, 0.000000000000000000, 0.000000000000000000 ) ) ;
#68143 = VECTOR ( 'NONE', #62901, 1000.000000000000000 ) ;
#68145 = VECTOR ( 'NONE', #55016, 1000.000000000000000 ) ;
#68144 = DIRECTION ( 'NONE',  ( -0.8660254037844482555, 0.000000000000000000, 0.4999999999999831801 ) ) ;
#68146 = CYLINDRICAL_SURFACE ( 'NONE', #21498, 1.399999999999998579 ) ;
#68147 = ORIENTED_EDGE ( 'NONE', *, *, #27213, .F. ) ;
#68148 = CARTESIAN_POINT ( 'NONE',  ( 8.249999999999996447, 8.250000000000001776, 0.000000000000000000 ) ) ;
#68149 = ORIENTED_EDGE ( 'NONE', *, *, #34652, .T. ) ;
#68150 = CARTESIAN_POINT ( 'NONE',  ( -3.842976262117221875, 10.30047626211716860, 26.00000000000000711 ) ) ;
#68151 = DIRECTION ( 'NONE',  ( -1.000000000000000000, 0.000000000000000000, 0.000000000000000000 ) ) ;
#68152 = ORIENTED_EDGE ( 'NONE', *, *, #62598, .F. ) ;
#68153 = CARTESIAN_POINT ( 'NONE',  ( 10.09643294401453240, 9.293516549646613001, 195.0000000000000284 ) ) ;
#68154 = EDGE_LOOP ( 'NONE', ( #5042, #36607, #58505, #17995 ) ) ;
#68155 = DIRECTION ( 'NONE',  ( 1.000000000000000000, -1.671920889371702854E-15, 0.000000000000000000 ) ) ;
#68156 = ORIENTED_EDGE ( 'NONE', *, *, #9189, .T. ) ;
#68157 = ORIENTED_EDGE ( 'NONE', *, *, #65064, .T. ) ;
#68158 = CARTESIAN_POINT ( 'NONE',  ( -8.916576262117258622, 9.689726262117185129, 26.00000000000000711 ) ) ;
#68159 = ORIENTED_EDGE ( 'NONE', *, *, #67403, .T. ) ;
#68160 = EDGE_LOOP ( 'NONE', ( #14628, #46339, #69678, #6436 ) ) ;
#68161 = CARTESIAN_POINT ( 'NONE',  ( -7.342976262117259623, 4.947141984184421304, 54.00000000000000711 ) ) ;
#68162 = CARTESIAN_POINT ( 'NONE',  ( 16.75000000000000000, -0.2038245569916320166, 23.22168783648699986 ) ) ;
#68163 = LINE ( 'NONE', #3814, #45664 ) ;
#68164 = ORIENTED_EDGE ( 'NONE', *, *, #19176, .T. ) ;
#68165 = AXIS2_PLACEMENT_3D ( 'NONE', #13605, #50036, #51082 ) ;
#68166 = DIRECTION ( 'NONE',  ( -0.000000000000000000, 3.673940397442059868E-16, -1.000000000000000000 ) ) ;
#68168 = DIRECTION ( 'NONE',  ( 0.000000000000000000, 0.000000000000000000, 1.000000000000000000 ) ) ;
#68167 = CARTESIAN_POINT ( 'NONE',  ( 0.000000000000000000, 0.000000000000000000, -18.00000000000000000 ) ) ;
#68169 = EDGE_CURVE ( 'NONE', #3391, #24260, #22269, .T. ) ;
#68170 = VERTEX_POINT ( 'NONE', #5324 ) ;
#68172 = ORIENTED_EDGE ( 'NONE', *, *, #26533, .T. ) ;
#68171 = PLANE ( 'NONE',  #60187 ) ;
#68173 = EDGE_LOOP ( 'NONE', ( #29378, #38089, #64759, #6026 ) ) ;
#68174 = APPLICATION_PROTOCOL_DEFINITION ( 'draft international standard', 'automotive_design', 1998, #27335 ) ;
#68175 = EDGE_CURVE ( 'NONE', #414, #36899, #1380, .T. ) ;
#68176 = DIRECTION ( 'NONE',  ( 1.000000000000000000, -0.000000000000000000, 0.000000000000000000 ) ) ;
#68178 = EDGE_LOOP ( 'NONE', ( #11400, #63306, #59668, #34724 ) ) ;
#68177 = CARTESIAN_POINT ( 'NONE',  ( 16.75000000000000000, -0.2714405302574892098, -22.98746066354537376 ) ) ;
#68179 = DIRECTION ( 'NONE',  ( 1.000000000000000000, 0.000000000000000000, 0.000000000000000000 ) ) ;
#68180 = VECTOR ( 'NONE', #20050, 1000.000000000000000 ) ;
#68181 = CARTESIAN_POINT ( 'NONE',  ( -11.00000000000000000, -11.50000000000000000, -15.00000000000000000 ) ) ;
#68182 = ORIENTED_EDGE ( 'NONE', *, *, #7316, .T. ) ;
#68183 = EDGE_CURVE ( 'NONE', #42852, #28114, #62831, .T. ) ;
#68184 = ORIENTED_EDGE ( 'NONE', *, *, #50087, .F. ) ;
#68185 = VECTOR ( 'NONE', #48944, 1000.000000000000000 ) ;
#68186 = VECTOR ( 'NONE', #67148, 1000.000000000000000 ) ;
#68187 = DIRECTION ( 'NONE',  ( -0.7671651518153065341, -0.6414496315691495809, -2.356647714346224881E-16 ) ) ;
#68188 = EDGE_CURVE ( 'NONE', #48595, #68798, #49816, .T. ) ;
#68189 = EDGE_LOOP ( 'NONE', ( #83, #57925, #68076, #43029, #37504, #10154, #23434, #39120 ) ) ;
#68190 = CARTESIAN_POINT ( 'NONE',  ( 11.00000000000000000, -5.599999999999999645, -9.000000000000001776 ) ) ;
#68191 = CARTESIAN_POINT ( 'NONE',  ( 283.0000000000000568, -20.40000000000000213, 12.40000000000000213 ) ) ;
#68192 = AXIS2_PLACEMENT_3D ( 'NONE', #53355, #296, #49764 ) ;
#68193 = VECTOR ( 'NONE', #35804, 1000.000000000000000 ) ;
#68194 = VECTOR ( 'NONE', #47791, 1000.000000000000000 ) ;
#68195 = CARTESIAN_POINT ( 'NONE',  ( 30.00000000000000000, -8.959999999999999076, -17.04524521594300523 ) ) ;
#68196 = VERTEX_POINT ( 'NONE', #5661 ) ;
#68197 = DIRECTION ( 'NONE',  ( -1.000000000000000000, 0.000000000000000000, 0.000000000000000000 ) ) ;
#68198 = EDGE_CURVE ( 'NONE', #68881, #48598, #32177, .T. ) ;
#68199 = LINE ( 'NONE', #55840, #67533 ) ;
#68201 = ORIENTED_EDGE ( 'NONE', *, *, #45345, .F. ) ;
#68200 = CARTESIAN_POINT ( 'NONE',  ( -29.50000000000000355, -11.50000000000100009, 19.50000000000103739 ) ) ;
#68203 = ORIENTED_EDGE ( 'NONE', *, *, #34361, .T. ) ;
#68202 = DIRECTION ( 'NONE',  ( -1.836970198721029934E-16, 1.836970198721036590E-16, -1.000000000000000000 ) ) ;
#68204 = VECTOR ( 'NONE', #32260, 1000.000000000000000 ) ;
#68205 = CARTESIAN_POINT ( 'NONE',  ( 13.00000000000000178, -15.50000000000000000, 14.50000000000000000 ) ) ;
#68206 = DIRECTION ( 'NONE',  ( 5.626525616968433120E-15, 1.000000000000000000, 1.836970198721025990E-16 ) ) ;
#68207 = DIRECTION ( 'NONE',  ( 0.000000000000000000, 0.000000000000000000, 1.000000000000000000 ) ) ;
#68208 = FACE_OUTER_BOUND ( 'NONE', #3114, .T. ) ;
#68209 = CARTESIAN_POINT ( 'NONE',  ( -11.00000000000000000, -8.959999999999999076, -17.04524521594300523 ) ) ;
#68210 = EDGE_CURVE ( 'NONE', #56785, #53395, #38191, .T. ) ;
#68211 = VERTEX_POINT ( 'NONE', #37833 ) ;
#68212 = CARTESIAN_POINT ( 'NONE',  ( 9.562023737882812569, -8.144523737882824577, 54.00000000000000711 ) ) ;
#68213 = DIRECTION ( 'NONE',  ( -1.000000000000000000, 0.000000000000000000, 0.000000000000000000 ) ) ;
#68215 = EDGE_CURVE ( 'NONE', #30328, #43890, #22941, .T. ) ;
#68214 = CYLINDRICAL_SURFACE ( 'NONE', #60351, 0.3999999999999993006 ) ;
#68217 = ORIENTED_EDGE ( 'NONE', *, *, #29728, .F. ) ;
#68216 = LINE ( 'NONE', #46642, #607 ) ;
#68218 = CARTESIAN_POINT ( 'NONE',  ( 40.90000000000000568, 0.000000000000000000, 0.000000000000000000 ) ) ;
#68219 = CYLINDRICAL_SURFACE ( 'NONE', #10410, 0.5000000000023396840 ) ;
#68220 = EDGE_LOOP ( 'NONE', ( #28001, #34677, #2838, #5105 ) ) ;
#68221 = LINE ( 'NONE', #69637, #28647 ) ;
#68222 = DIRECTION ( 'NONE',  ( -0.000000000000000000, -0.000000000000000000, -1.000000000000000000 ) ) ;
#68223 = ADVANCED_FACE ( 'NONE', ( #65397 ), #5997, .T. ) ;
#68224 = AXIS2_PLACEMENT_3D ( 'NONE', #671, #22240, #60053 ) ;
#68225 = ORIENTED_EDGE ( 'NONE', *, *, #43282, .T. ) ;
#68226 = DIRECTION ( 'NONE',  ( 0.000000000000000000, 0.000000000000000000, 1.000000000000000000 ) ) ;
#68227 = DIRECTION ( 'NONE',  ( 0.000000000000000000, -0.7071067811865495711, -0.7071067811865455743 ) ) ;
#68228 = DIRECTION ( 'NONE',  ( 0.5000000000000068834, 0.8660254037844345998, 6.723777587268309839E-17 ) ) ;
#68229 = DIRECTION ( 'NONE',  ( -1.000000000000000000, 0.000000000000000000, 0.000000000000000000 ) ) ;
#68230 = AXIS2_PLACEMENT_3D ( 'NONE', #67080, #40206, #34891 ) ;
#68231 = VECTOR ( 'NONE', #22006, 1000.000000000000000 ) ;
#68232 = ORIENTED_EDGE ( 'NONE', *, *, #10773, .F. ) ;
#68233 = CARTESIAN_POINT ( 'NONE',  ( 0.000000000000000000, -7.449999999999998401, -22.50000000000000000 ) ) ;
#68234 = VERTEX_POINT ( 'NONE', #60077 ) ;
#68235 = ORIENTED_EDGE ( 'NONE', *, *, #35033, .F. ) ;
#68236 = VERTEX_POINT ( 'NONE', #11624 ) ;
#68237 = DIRECTION ( 'NONE',  ( 1.000000000000000000, -5.981805089575194965E-17, 0.000000000000000000 ) ) ;
#68238 = AXIS2_PLACEMENT_3D ( 'NONE', #38595, #53829, #21982 ) ;
#68239 = AXIS2_PLACEMENT_3D ( 'NONE', #42211, #9700, #25618 ) ;
#68240 = EDGE_CURVE ( 'NONE', #9842, #20615, #27559, .T. ) ;
#68241 = CARTESIAN_POINT ( 'NONE',  ( 10.09643294401454661, -9.306483450353395526, 195.0000000000000284 ) ) ;
#68242 = VECTOR ( 'NONE', #60412, 1000.000000000000000 ) ;
#68243 = CARTESIAN_POINT ( 'NONE',  ( 15.00000000000000000, -21.00000000000000000, 8.000000000000000000 ) ) ;
#68244 = ORIENTED_EDGE ( 'NONE', *, *, #20427, .T. ) ;
#68245 = VERTEX_POINT ( 'NONE', #27913 ) ;
#68246 = CARTESIAN_POINT ( 'NONE',  ( -7.250000000000000888, 7.250000000000001776, -26.00000000000001066 ) ) ;
#68247 = VERTEX_POINT ( 'NONE', #10956 ) ;
#68248 = EDGE_CURVE ( 'NONE', #12315, #44134, #49482, .T. ) ;
#68249 = ORIENTED_EDGE ( 'NONE', *, *, #57163, .F. ) ;
#68250 = FACE_OUTER_BOUND ( 'NONE', #32266, .T. ) ;
#68251 = CYLINDRICAL_SURFACE ( 'NONE', #50513, 0.3499999999999996447 ) ;
#68252 = CARTESIAN_POINT ( 'NONE',  ( 0.000000000000000000, 8.250000000000001776, -25.50000000000000355 ) ) ;
#68253 = DIRECTION ( 'NONE',  ( 0.000000000000000000, 0.000000000000000000, -1.000000000000000000 ) ) ;
#68254 = ORIENTED_EDGE ( 'NONE', *, *, #17890, .T. ) ;
#68255 = EDGE_CURVE ( 'NONE', #56239, #39495, #21565, .T. ) ;
#68256 = VECTOR ( 'NONE', #38853, 1000.000000000000000 ) ;
#68257 = DIRECTION ( 'NONE',  ( -1.000000000000000000, 0.000000000000000000, 0.000000000000000000 ) ) ;
#68259 = DIRECTION ( 'NONE',  ( -0.8660254037844400399, -0.4999999999999973910, 6.723777587268495961E-17 ) ) ;
#68258 = CARTESIAN_POINT ( 'NONE',  ( 7.450000000000004619, -1.336933437520057563E-15, -7.500000000000000000 ) ) ;
#68260 = ORIENTED_EDGE ( 'NONE', *, *, #41042, .T. ) ;
#68261 = EDGE_CURVE ( 'NONE', #53834, #68001, #51527, .T. ) ;
#68263 = ORIENTED_EDGE ( 'NONE', *, *, #2425, .T. ) ;
#68262 = CARTESIAN_POINT ( 'NONE',  ( -10.91351654964675610, -9.306483450353326248, 195.0000000000000284 ) ) ;
#68264 = ORIENTED_EDGE ( 'NONE', *, *, #38289, .T. ) ;
#68265 = EDGE_CURVE ( 'NONE', #903, #28244, #60561, .T. ) ;
#68266 = CARTESIAN_POINT ( 'NONE',  ( -7.342976262117248965, -3.848229544836283100, 26.00000000000000711 ) ) ;
#68267 = CARTESIAN_POINT ( 'NONE',  ( -1.620245201994301665, 8.227189898828640935, 54.00000000000000711 ) ) ;
#68268 = VERTEX_POINT ( 'NONE', #64696 ) ;
#68269 = EDGE_LOOP ( 'NONE', ( #5497, #34413, #58482, #68506, #45085, #57628, #63496, #11371 ) ) ;
#68270 = ADVANCED_FACE ( 'NONE', ( #17633 ), #6676, .F. ) ;
#68271 = AXIS2_PLACEMENT_3D ( 'NONE', #14859, #47028, #69292 ) ;
#68272 = EDGE_CURVE ( 'NONE', #53780, #17018, #46989, .T. ) ;
#68273 = DIRECTION ( 'NONE',  ( 0.000000000000000000, 0.000000000000000000, 1.000000000000000000 ) ) ;
#68274 = PLANE ( 'NONE',  #20993 ) ;
#68275 = CIRCLE ( 'NONE', #12928, 1.000000000000000000 ) ;
#68276 = VERTEX_POINT ( 'NONE', #45188 ) ;
#68277 = ADVANCED_FACE ( 'NONE', ( #61443 ), #13375, .T. ) ;
#68278 = EDGE_CURVE ( 'NONE', #58489, #1811, #60767, .T. ) ;
#68279 = ORIENTED_EDGE ( 'NONE', *, *, #25082, .F. ) ;
#68280 = LINE ( 'NONE', #62611, #34159 ) ;
#68281 = LINE ( 'NONE', #19484, #56497 ) ;
#68282 = VERTEX_POINT ( 'NONE', #33889 ) ;
#68283 = EDGE_CURVE ( 'NONE', #21280, #14789, #7361, .T. ) ;
#68284 = AXIS2_PLACEMENT_3D ( 'NONE', #22829, #40118, #34118 ) ;
#68285 = AXIS2_PLACEMENT_3D ( 'NONE', #34235, #28947, #50521 ) ;
#68286 = CYLINDRICAL_SURFACE ( 'NONE', #44776, 1.000000000000000000 ) ;
#68287 = CARTESIAN_POINT ( 'NONE',  ( 39.90000000000000568, -0.2000000000000000111, 0.000000000000000000 ) ) ;
#68289 = ORIENTED_EDGE ( 'NONE', *, *, #67128, .T. ) ;
#68288 = CARTESIAN_POINT ( 'NONE',  ( 18.89999999999999858, -0.1999999999911795112, 8.826273045769999343E-12 ) ) ;
#68290 = EDGE_LOOP ( 'NONE', ( #38800, #23117, #16415, #16561 ) ) ;
#68291 = LINE ( 'NONE', #50974, #68934 ) ;
#68292 = EDGE_CURVE ( 'NONE', #40989, #10852, #3127, .T. ) ;
#68293 = CYLINDRICAL_SURFACE ( 'NONE', #11476, 1.929199999999998916 ) ;
#68294 = LINE ( 'NONE', #57333, #18825 ) ;
#68295 = CARTESIAN_POINT ( 'NONE',  ( 105.8309041053263257, 61.65740854044500452, 0.000000000000000000 ) ) ;
#68296 = CARTESIAN_POINT ( 'NONE',  ( 3.664523737882778853, -10.50702373788280219, 26.00000000000000000 ) ) ;
#68297 = CIRCLE ( 'NONE', #58109, 3.499999999999054534 ) ;
#68298 = CARTESIAN_POINT ( 'NONE',  ( 30.00000000000000000, -12.00000000000000000, 10.20500000000000007 ) ) ;
#68299 = EDGE_CURVE ( 'NONE', #16950, #2504, #48165, .T. ) ;
#68300 = VERTEX_POINT ( 'NONE', #19372 ) ;
#68301 = DIRECTION ( 'NONE',  ( -1.836970198721029934E-16, 1.836970198721036344E-16, -1.000000000000000000 ) ) ;
#68304 = ORIENTED_EDGE ( 'NONE', *, *, #22177, .F. ) ;
#68303 = ADVANCED_FACE ( 'NONE', ( #39879 ), #55477, .F. ) ;
#68302 = DIRECTION ( 'NONE',  ( -1.836970198721029934E-16, 1.836970198721036590E-16, -1.000000000000000000 ) ) ;
#68305 = CARTESIAN_POINT ( 'NONE',  ( 30.00000000000000000, -11.50000000000082068, 10.20500000000000007 ) ) ;
#68306 = COLOUR_RGB ( '', 0.66274510, 0.83137255, 0.94901961) ;
#68307 = DIRECTION ( 'NONE',  ( 1.000000000000000000, 0.000000000000000000, 0.000000000000000000 ) ) ;
#68308 = AXIS2_PLACEMENT_3D ( 'NONE', #42287, #6799, #36636 ) ;
#68309 = LINE ( 'NONE', #30826, #28452 ) ;
#68310 = ORIENTED_EDGE ( 'NONE', *, *, #30198, .T. ) ;
#68311 = DIRECTION ( 'NONE',  ( -1.000000000000000000, 0.000000000000000000, 0.000000000000000000 ) ) ;
#68312 = CARTESIAN_POINT ( 'NONE',  ( 9.703773737882814387, 8.916576262117184015, 54.00000000000000711 ) ) ;
#68313 = VERTEX_POINT ( 'NONE', #67824 ) ;
#68314 = CARTESIAN_POINT ( 'NONE',  ( -6.822336235477489019, -6.364920264886855250, 54.00000000000000711 ) ) ;
#68315 = CARTESIAN_POINT ( 'NONE',  ( -10.49297626211725110, -3.664523737882711352, 54.00000000000000711 ) ) ;
#68316 = CARTESIAN_POINT ( 'NONE',  ( -28.00000000000000000, -16.64230188589299786, -14.64519951917100116 ) ) ;
#68317 = EDGE_LOOP ( 'NONE', ( #36554, #50972, #18401, #735, #1519, #44977, #38132, #20408, #43511, #21142, #58909, #69822, #61106, #59687 ) ) ;
#68318 = LINE ( 'NONE', #58432, #37269 ) ;
#68319 = VERTEX_POINT ( 'NONE', #2416 ) ;
#68320 = ORIENTED_EDGE ( 'NONE', *, *, #1899, .T. ) ;
#68321 = DIRECTION ( 'NONE',  ( -3.596772705736696467E-15, -1.000000000000000000, 0.000000000000000000 ) ) ;
#68322 = CARTESIAN_POINT ( 'NONE',  ( 275.0000000000000000, -30.45000000000000639, 15.00000000000000000 ) ) ;
#68323 = DIRECTION ( 'NONE',  ( -1.671920889371702657E-15, -1.000000000000000000, -3.673940397442059868E-16 ) ) ;
#68324 = EDGE_CURVE ( 'NONE', #12404, #4257, #45864, .T. ) ;
#68325 = CIRCLE ( 'NONE', #69442, 1.000000000000000888 ) ;
#68326 = CARTESIAN_POINT ( 'NONE',  ( -6.642976262117260333, 10.30047626211718104, 54.00000000000000711 ) ) ;
#68327 = CARTESIAN_POINT ( 'NONE',  ( 13.00000000000000178, -16.28999999999710369, 14.50000000000000000 ) ) ;
#68328 = ORIENTED_EDGE ( 'NONE', *, *, #30627, .T. ) ;
#68329 = EDGE_LOOP ( 'NONE', ( #52834, #37657, #28701, #29354 ) ) ;
#68331 = ORIENTED_EDGE ( 'NONE', *, *, #53384, .F. ) ;
#68330 = FACE_OUTER_BOUND ( 'NONE', #36200, .T. ) ;
#68332 = ORIENTED_EDGE ( 'NONE', *, *, #60971, .T. ) ;
#68333 = ADVANCED_FACE ( 'NONE', ( #1718 ), #23285, .F. ) ;
#68334 = AXIS2_PLACEMENT_3D ( 'NONE', #20209, #41773, #14915 ) ;
#68335 = VECTOR ( 'NONE', #5922, 1000.000000000000000 ) ;
#68336 = DIRECTION ( 'NONE',  ( 9.050731179009442381E-15, 1.000000000000000000, 3.673940397442060361E-16 ) ) ;
#68337 = DIRECTION ( 'NONE',  ( 0.000000000000000000, 0.000000000000000000, 1.000000000000000000 ) ) ;
#68338 = LINE ( 'NONE', #40764, #64006 ) ;
#68339 = CIRCLE ( 'NONE', #60392, 0.7499999999999997780 ) ;
#68340 = CARTESIAN_POINT ( 'NONE',  ( -8.593516549646711411, 4.383466043307770121, 195.0000000000000284 ) ) ;
#68341 = EDGE_CURVE ( 'NONE', #41718, #19639, #50363, .T. ) ;
#68342 = CYLINDRICAL_SURFACE ( 'NONE', #19768, 0.1749999999999998224 ) ;
#68343 = VECTOR ( 'NONE', #17901, 1000.000000000000000 ) ;
#68344 = AXIS2_PLACEMENT_3D ( 'NONE', #25570, #42518, #15656 ) ;
#68345 = DIRECTION ( 'NONE',  ( -1.836970198721029934E-16, 1.836970198721036344E-16, -1.000000000000000000 ) ) ;
#68346 = EDGE_CURVE ( 'NONE', #61284, #45166, #17655, .T. ) ;
#68347 = ORIENTED_EDGE ( 'NONE', *, *, #32449, .T. ) ;
#68348 = ORIENTED_EDGE ( 'NONE', *, *, #30627, .F. ) ;
#68349 = EDGE_CURVE ( 'NONE', #47484, #31270, #35268, .T. ) ;
#68350 = EDGE_LOOP ( 'NONE', ( #43170, #60237, #25733, #69721 ) ) ;
#68352 = EDGE_LOOP ( 'NONE', ( #66571, #42413, #18345, #52685 ) ) ;
#68351 = AXIS2_PLACEMENT_3D ( 'NONE', #3878, #41697, #36393 ) ;
#68353 = CARTESIAN_POINT ( 'NONE',  ( -3.667976262117328190, -9.737023737882820384, 54.00000000000000711 ) ) ;
#68354 = ADVANCED_FACE ( 'NONE', ( #44846 ), #66425, .F. ) ;
#68355 = ADVANCED_FACE ( 'NONE', ( #17973 ), #13010, .F. ) ;
#68356 = DIRECTION ( 'NONE',  ( -0.000000000000000000, -0.000000000000000000, 1.000000000000000000 ) ) ;
#68357 = CIRCLE ( 'NONE', #37880, 0.5000000000009302559 ) ;
#68358 = FACE_OUTER_BOUND ( 'NONE', #9222, .T. ) ;
#68359 = ORIENTED_EDGE ( 'NONE', *, *, #7113, .T. ) ;
#68360 = VERTEX_POINT ( 'NONE', #2758 ) ;
#68361 = VERTEX_POINT ( 'NONE', #67484 ) ;
#68362 = AXIS2_PLACEMENT_3D ( 'NONE', #27275, #748, #21275 ) ;
#68363 = DIRECTION ( 'NONE',  ( -1.000000000000000000, 0.000000000000000000, 0.000000000000000000 ) ) ;
#68364 = VERTEX_POINT ( 'NONE', #19032 ) ;
#68365 = ORIENTED_EDGE ( 'NONE', *, *, #61914, .F. ) ;
#68366 = CARTESIAN_POINT ( 'NONE',  ( 4.456444791733522252E-16, 7.450000000000002842, -13.50000000000000178 ) ) ;
#68367 = ORIENTED_EDGE ( 'NONE', *, *, #22046, .T. ) ;
#68368 = ORIENTED_EDGE ( 'NONE', *, *, #42323, .T. ) ;
#68369 = DIRECTION ( 'NONE',  ( 0.000000000000000000, 0.000000000000000000, 1.000000000000000000 ) ) ;
#68371 = ORIENTED_EDGE ( 'NONE', *, *, #52133, .T. ) ;
#68370 = DIRECTION ( 'NONE',  ( 0.000000000000000000, -1.000000000000000000, 0.000000000000000000 ) ) ;
#68372 = ORIENTED_EDGE ( 'NONE', *, *, #43616, .F. ) ;
#68373 = DIRECTION ( 'NONE',  ( 0.000000000000000000, 0.000000000000000000, 1.000000000000000000 ) ) ;
#68374 = DIRECTION ( 'NONE',  ( -0.000000000000000000, -0.000000000000000000, 1.000000000000000000 ) ) ;
#68376 = EDGE_LOOP ( 'NONE', ( #54693, #43591, #45046, #50756 ) ) ;
#68375 = DIRECTION ( 'NONE',  ( 0.000000000000000000, -0.7066873191084664940, 0.7075259945834416753 ) ) ;
#68377 = ORIENTED_EDGE ( 'NONE', *, *, #5404, .F. ) ;
#68378 = CARTESIAN_POINT ( 'NONE',  ( -11.18071654964669825, 11.99351654964660341, 455.0000000000000568 ) ) ;
#68379 = VECTOR ( 'NONE', #14047, 1000.000000000000000 ) ;
#68380 = CARTESIAN_POINT ( 'NONE',  ( -8.393516549646779623, -6.344579767990844665, 455.0000000000000568 ) ) ;
#68381 = DIRECTION ( 'NONE',  ( -0.7071067811865446862, 0.7071067811865503483, 0.000000000000000000 ) ) ;
#68382 = LINE ( 'NONE', #47174, #22623 ) ;
#68383 = ORIENTED_EDGE ( 'NONE', *, *, #2181, .T. ) ;
#68384 = CARTESIAN_POINT ( 'NONE',  ( -7.750000000000001776, -7.348062532927999158, 0.000000000000000000 ) ) ;
#68385 = EDGE_CURVE ( 'NONE', #7056, #23202, #40594, .T. ) ;
#68386 = AXIS2_PLACEMENT_3D ( 'NONE', #22457, #37677, #53595 ) ;
#68387 = CIRCLE ( 'NONE', #9645, 0.06000000000000102474 ) ;
#68389 = CARTESIAN_POINT ( 'NONE',  ( -15.50000000000000000, -15.50000000000000000, -22.50000000000000000 ) ) ;
#68388 = CIRCLE ( 'NONE', #38017, 0.7500000000000006661 ) ;
#68390 = CARTESIAN_POINT ( 'NONE',  ( 70.47321854994621049, 47.95351654967443977, 39.00000000000000000 ) ) ;
#68391 = ORIENTED_EDGE ( 'NONE', *, *, #25503, .T. ) ;
#68392 = ADVANCED_FACE ( 'NONE', ( #51561 ), #35991, .T. ) ;
#68393 = DIRECTION ( 'NONE',  ( 1.000000000000000000, 0.000000000000000000, 0.000000000000000000 ) ) ;
#68394 = LINE ( 'NONE', #47182, #58877 ) ;
#68395 = AXIS2_PLACEMENT_3D ( 'NONE', #45837, #29919, #51499 ) ;
#68396 = AXIS2_PLACEMENT_3D ( 'NONE', #7698, #29259, #2058 ) ;
#68397 = AXIS2_PLACEMENT_3D ( 'NONE', #42082, #52352, #68960 ) ;
#68398 = DIRECTION ( 'NONE',  ( 2.135044278125299371E-15, 1.000000000000000000, 0.000000000000000000 ) ) ;
#68399 = ORIENTED_EDGE ( 'NONE', *, *, #40001, .T. ) ;
#68400 = AXIS2_PLACEMENT_3D ( 'NONE', #23561, #3058, #50439 ) ;
#68401 = DIRECTION ( 'NONE',  ( 0.000000000000000000, 0.000000000000000000, -1.000000000000000000 ) ) ;
#68402 = VECTOR ( 'NONE', #32502, 1000.000000000000000 ) ;
#68403 = LINE ( 'NONE', #4416, #7848 ) ;
#68404 = ORIENTED_EDGE ( 'NONE', *, *, #27642, .T. ) ;
#68405 = CARTESIAN_POINT ( 'NONE',  ( 0.000000000000000000, -0.5000000000000000000, 26.50000000000000000 ) ) ;
#68406 = CARTESIAN_POINT ( 'NONE',  ( 11.00000000000000000, -5.599999999999999645, -27.00000000000000000 ) ) ;
#68407 = CARTESIAN_POINT ( 'NONE',  ( 2.369523737882810455, 8.821682069070735821, 26.00000000000000711 ) ) ;
#68408 = AXIS2_PLACEMENT_3D ( 'NONE', #44538, #18017, #61489 ) ;
#68409 = FACE_OUTER_BOUND ( 'NONE', #66048, .T. ) ;
#68410 = CARTESIAN_POINT ( 'NONE',  ( 7.750000000000001776, 7.750000000000000000, -5.000000000000000000 ) ) ;
#68411 = VERTEX_POINT ( 'NONE', #36699 ) ;
#68412 = CARTESIAN_POINT ( 'NONE',  ( 24.00000000000000000, -16.28999999999710369, 15.00000000000794920 ) ) ;
#68413 = CARTESIAN_POINT ( 'NONE',  ( -15.50000000000000000, -1.037157890325000054, -22.50000000000000000 ) ) ;
#68414 = DIRECTION ( 'NONE',  ( -1.000000000000000000, 0.000000000000000000, 0.000000000000000000 ) ) ;
#68415 = DIRECTION ( 'NONE',  ( -1.000000000000000000, 0.000000000000000000, 0.000000000000000000 ) ) ;
#68416 = DIRECTION ( 'NONE',  ( -0.8660254037844383745, -0.5000000000000005551, -1.836970198721031660E-16 ) ) ;
#68417 = VERTEX_POINT ( 'NONE', #63577 ) ;
#68419 = ORIENTED_EDGE ( 'NONE', *, *, #53802, .T. ) ;
#68418 = CARTESIAN_POINT ( 'NONE',  ( -7.450000000000001954, 7.250000000000000000, -22.50000000000000000 ) ) ;
#68420 = EDGE_CURVE ( 'NONE', #62704, #36865, #4528, .T. ) ;
#68421 = DIRECTION ( 'NONE',  ( 0.000000000000000000, -1.000000000000000000, 0.000000000000000000 ) ) ;
#68422 = DIRECTION ( 'NONE',  ( 1.000000000000000000, -0.000000000000000000, -0.000000000000000000 ) ) ;
#68423 = CARTESIAN_POINT ( 'NONE',  ( 7.000000000000000000, -23.29603921945599865, 12.50000000000000000 ) ) ;
#68424 = VERTEX_POINT ( 'NONE', #20430 ) ;
#68425 = CYLINDRICAL_SURFACE ( 'NONE', #8458, 0.3499999999999996447 ) ;
#68426 = LINE ( 'NONE', #25659, #35194 ) ;
#68427 = CIRCLE ( 'NONE', #49258, 0.2000000000000005107 ) ;
#68428 = EDGE_CURVE ( 'NONE', #8452, #43101, #26097, .T. ) ;
#68429 = ORIENTED_EDGE ( 'NONE', *, *, #53604, .F. ) ;
#68430 = ORIENTED_EDGE ( 'NONE', *, *, #43364, .F. ) ;
#68431 = EDGE_CURVE ( 'NONE', #16805, #33051, #58268, .T. ) ;
#68432 = AXIS2_PLACEMENT_3D ( 'NONE', #18926, #13959, #35518 ) ;
#68433 = ORIENTED_EDGE ( 'NONE', *, *, #13542, .T. ) ;
#68434 = DIRECTION ( 'NONE',  ( 0.000000000000000000, 0.000000000000000000, 1.000000000000000000 ) ) ;
#68435 = EDGE_CURVE ( 'NONE', #60745, #51045, #43613, .T. ) ;
#68436 = ADVANCED_FACE ( 'NONE', ( #42347 ), #9126, .F. ) ;
#68437 = CARTESIAN_POINT ( 'NONE',  ( 0.000000000000000000, 0.000000000000000000, -5.000000000000000000 ) ) ;
#68438 = DIRECTION ( 'NONE',  ( -1.000000000000000000, 0.000000000000000000, 0.000000000000000000 ) ) ;
#68439 = LINE ( 'NONE', #9389, #21263 ) ;
#68440 = AXIS2_PLACEMENT_3D ( 'NONE', #17750, #18422, #1827 ) ;
#68441 = AXIS2_PLACEMENT_3D ( 'NONE', #26059, #68837, #20391 ) ;
#68442 = CIRCLE ( 'NONE', #4045, 2.458500000000000796 ) ;
#68443 = EDGE_CURVE ( 'NONE', #57359, #9842, #52261, .T. ) ;
#68444 = ORIENTED_EDGE ( 'NONE', *, *, #66660, .T. ) ;
#68445 = VERTEX_POINT ( 'NONE', #41290 ) ;
#68446 = DIRECTION ( 'NONE',  ( 1.000000000000000000, -1.047444401652940007E-14, 1.836970198721010706E-16 ) ) ;
#68447 = CARTESIAN_POINT ( 'NONE',  ( 7.250000000000005329, -7.449999999999998401, -8.000000000000000000 ) ) ;
#68448 = VECTOR ( 'NONE', #34090, 1000.000000000000000 ) ;
#68449 = VECTOR ( 'NONE', #9219, 1000.000000000000000 ) ;
#68450 = VECTOR ( 'NONE', #4183, 1000.000000000000000 ) ;
#68451 = ORIENTED_EDGE ( 'NONE', *, *, #68110, .T. ) ;
#68452 = ORIENTED_EDGE ( 'NONE', *, *, #31777, .F. ) ;
#68453 = ORIENTED_EDGE ( 'NONE', *, *, #24806, .F. ) ;
#68454 = VERTEX_POINT ( 'NONE', #57210 ) ;
#68455 = CIRCLE ( 'NONE', #37977, 1.224999999999998757 ) ;
#68456 = CARTESIAN_POINT ( 'NONE',  ( 7.450000000000004619, -1.336933437520057563E-15, -10.50000000000000000 ) ) ;
#68457 = UNCERTAINTY_MEASURE_WITH_UNIT (LENGTH_MEASURE( 1.000000000000000082E-05 ), #62185, 'distance_accuracy_value', 'NONE');
#68459 = ORIENTED_EDGE ( 'NONE', *, *, #15952, .T. ) ;
#68458 = DIRECTION ( 'NONE',  ( 0.000000000000000000, 0.000000000000000000, 1.000000000000000000 ) ) ;
#68460 = DIRECTION ( 'NONE',  ( 1.000000000000000000, -0.000000000000000000, 0.000000000000000000 ) ) ;
#68461 = AXIS2_PLACEMENT_3D ( 'NONE', #20976, #24888, #4393 ) ;
#68462 = CARTESIAN_POINT ( 'NONE',  ( 25.50000000000000355, 0.000000000000000000, 22.50000000000000000 ) ) ;
#68463 = ORIENTED_EDGE ( 'NONE', *, *, #54907, .T. ) ;
#68464 = ORIENTED_EDGE ( 'NONE', *, *, #23973, .T. ) ;
#68465 = CARTESIAN_POINT ( 'NONE',  ( 7.250000000000005329, -7.249999999999998224, -20.50000000000000000 ) ) ;
#68466 = CARTESIAN_POINT ( 'NONE',  ( -7.250000000000000000, -7.449999999999998401, -10.50000000000000000 ) ) ;
#68467 = ORIENTED_EDGE ( 'NONE', *, *, #44828, .F. ) ;
#68468 = SURFACE_STYLE_FILL_AREA ( #10462 ) ;
#68469 = FACE_OUTER_BOUND ( 'NONE', #45900, .T. ) ;
#68470 = CARTESIAN_POINT ( 'NONE',  ( -6.331612867284154511, 8.393516549646601987, 455.0000000000000568 ) ) ;
#68471 = ORIENTED_EDGE ( 'NONE', *, *, #62518, .T. ) ;
#68472 = EDGE_CURVE ( 'NONE', #39516, #40478, #63927, .T. ) ;
#68473 = CARTESIAN_POINT ( 'NONE',  ( 6.665817930929283541, 7.342976262117200115, 26.00000000000000711 ) ) ;
#68474 = DIRECTION ( 'NONE',  ( 0.000000000000000000, 0.000000000000000000, -1.000000000000000000 ) ) ;
#68475 = EDGE_CURVE ( 'NONE', #20196, #40849, #25753, .T. ) ;
#68476 = EDGE_CURVE ( 'NONE', #47021, #7002, #46947, .T. ) ;
#68477 = CARTESIAN_POINT ( 'NONE',  ( 18.85410196625000268, -15.50000000000000000, 21.50000000000000000 ) ) ;
#68478 = VECTOR ( 'NONE', #42241, 1000.000000000000000 ) ;
#68479 = LINE ( 'NONE', #58577, #48317 ) ;
#68480 = EDGE_CURVE ( 'NONE', #21570, #54832, #56067, .T. ) ;
#68481 = CONICAL_SURFACE ( 'NONE', #40250, 4.000000000000000000, 0.7853981633974476129 ) ;
#68482 = CARTESIAN_POINT ( 'NONE',  ( -10.30047626211724854, -3.664523737882715348, 54.00000000000000711 ) ) ;
#68483 = ORIENTED_EDGE ( 'NONE', *, *, #42725, .F. ) ;
#68484 = LINE ( 'NONE', #30997, #62926 ) ;
#68485 = CARTESIAN_POINT ( 'NONE',  ( -8.000000000000000000, -6.879816696376141572, 5.000000000000000000 ) ) ;
#68486 = CARTESIAN_POINT ( 'NONE',  ( 4.396432944014576627, 8.393516549646587777, 455.0000000000000568 ) ) ;
#68487 = CARTESIAN_POINT ( 'NONE',  ( -7.250000000000001776, -7.249999999999998224, -14.50000000000000000 ) ) ;
#68488 = AXIS2_PLACEMENT_3D ( 'NONE', #38977, #55245, #23416 ) ;
#68489 = AXIS2_PLACEMENT_3D ( 'NONE', #1950, #23513, #63366 ) ;
#68490 = VECTOR ( 'NONE', #51220, 1000.000000000000000 ) ;
#68491 = CYLINDRICAL_SURFACE ( 'NONE', #17952, 0.2000000000000005107 ) ;
#68492 = CARTESIAN_POINT ( 'NONE',  ( 39.90000000000000568, -0.000000000000000000, -20.80000000000000071 ) ) ;
#68493 = AXIS2_PLACEMENT_3D ( 'NONE', #25249, #8973, #42559 ) ;
#68494 = DIRECTION ( 'NONE',  ( 0.000000000000000000, 1.000000000000000000, 0.000000000000000000 ) ) ;
#68495 = AXIS2_PLACEMENT_3D ( 'NONE', #62866, #57557, #26796 ) ;
#68496 = CARTESIAN_POINT ( 'NONE',  ( -7.250000000000000888, -8.249999999999998224, -18.50000000000000000 ) ) ;
#68497 = ORIENTED_EDGE ( 'NONE', *, *, #16812, .F. ) ;
#68498 = DIRECTION ( 'NONE',  ( -1.000000000000000000, 0.000000000000000000, 0.000000000000000000 ) ) ;
#68499 = LINE ( 'NONE', #63182, #24868 ) ;
#68500 = ORIENTED_EDGE ( 'NONE', *, *, #38950, .F. ) ;
#68501 = DIRECTION ( 'NONE',  ( 0.000000000000000000, 1.000000000000000000, 0.000000000000000000 ) ) ;
#68502 = FACE_OUTER_BOUND ( 'NONE', #43639, .T. ) ;
#68503 = CIRCLE ( 'NONE', #7509, 1.399999999999999245 ) ;
#68504 = DIRECTION ( 'NONE',  ( 0.5000000000000068834, 0.8660254037844345998, 6.723777587268309839E-17 ) ) ;
#68505 = DIRECTION ( 'NONE',  ( 0.000000000000000000, 0.000000000000000000, 1.000000000000000000 ) ) ;
#68506 = ORIENTED_EDGE ( 'NONE', *, *, #53998, .T. ) ;
#68507 = VECTOR ( 'NONE', #36189, 1000.000000000000000 ) ;
#68508 = ORIENTED_EDGE ( 'NONE', *, *, #36414, .F. ) ;
#68509 = LINE ( 'NONE', #20063, #6734 ) ;
#68510 = CARTESIAN_POINT ( 'NONE',  ( -29.50000000000000355, -12.00000000000000000, -10.52786404500095863 ) ) ;
#68511 = ORIENTED_EDGE ( 'NONE', *, *, #7773, .T. ) ;
#68512 = DIRECTION ( 'NONE',  ( -3.491481338843132961E-15, -1.000000000000000000, -1.836970198721029934E-16 ) ) ;
#68513 = DIRECTION ( 'NONE',  ( 0.000000000000000000, 1.000000000000000000, 0.000000000000000000 ) ) ;
#68514 = VERTEX_POINT ( 'NONE', #19713 ) ;
#68515 = PLANE ( 'NONE',  #14174 ) ;
#68516 = VERTEX_POINT ( 'NONE', #41646 ) ;
#68517 = ORIENTED_EDGE ( 'NONE', *, *, #27802, .F. ) ;
#68518 = CARTESIAN_POINT ( 'NONE',  ( -4.609516549646713202, 3.593516549646603941, 455.0000000000000568 ) ) ;
#68519 = ORIENTED_EDGE ( 'NONE', *, *, #60892, .F. ) ;
#68520 = VERTEX_POINT ( 'NONE', #68875 ) ;
#68521 = EDGE_CURVE ( 'NONE', #66328, #42153, #31754, .T. ) ;
#68522 = CARTESIAN_POINT ( 'NONE',  ( 49.00000000000000000, -0.2000000000089119934, 8.909539772616881237E-12 ) ) ;
#68523 = CARTESIAN_POINT ( 'NONE',  ( 11.78648345035337819, -7.826483450353491023, 455.0000000000000568 ) ) ;
#68524 = CARTESIAN_POINT ( 'NONE',  ( 46.39999999999999858, 21.00000000000000000, -1.250000000000000000 ) ) ;
#68525 = EDGE_CURVE ( 'NONE', #2503, #46841, #53324, .T. ) ;
#68526 = ADVANCED_FACE ( 'NONE', ( #62494 ), #8773, .F. ) ;
#68527 = VECTOR ( 'NONE', #67609, 1000.000000000000000 ) ;
#68528 = VERTEX_POINT ( 'NONE', #31042 ) ;
#68529 = CARTESIAN_POINT ( 'NONE',  ( -6.486996718459913325, -3.157023737882783454, 54.00000000000000711 ) ) ;
#68531 = DIRECTION ( 'NONE',  ( -0.8660254037844510311, -0.4999999999999785727, 0.000000000000000000 ) ) ;
#68530 = PLANE ( 'NONE',  #24791 ) ;
#68532 = EDGE_LOOP ( 'NONE', ( #30450, #8044, #11461, #7972 ) ) ;
#68535 = ORIENTED_EDGE ( 'NONE', *, *, #37772, .T. ) ;
#68534 = EDGE_CURVE ( 'NONE', #4520, #22003, #4873, .T. ) ;
#68533 = LINE ( 'NONE', #57561, #12771 ) ;
#68536 = AXIS2_PLACEMENT_3D ( 'NONE', #16897, #290, #27504 ) ;
#68537 = ORIENTED_EDGE ( 'NONE', *, *, #60827, .F. ) ;
#68538 = SHAPE_DEFINITION_REPRESENTATION ( #46409, #64796 ) ;
#68539 = AXIS2_PLACEMENT_3D ( 'NONE', #16201, #59336, #38470 ) ;
#68540 = EDGE_CURVE ( 'NONE', #39563, #67875, #26438, .T. ) ;
#68541 = PLANE ( 'NONE',  #32252 ) ;
#68542 = EDGE_CURVE ( 'NONE', #31770, #36169, #27861, .T. ) ;
#68544 = EDGE_LOOP ( 'NONE', ( #53938, #55201, #5899, #50690 ) ) ;
#68543 = LINE ( 'NONE', #69590, #39870 ) ;
#68545 = AXIS2_PLACEMENT_3D ( 'NONE', #34943, #55492, #17993 ) ;
#68546 = DIRECTION ( 'NONE',  ( -0.000000000000000000, -0.000000000000000000, 1.000000000000000000 ) ) ;
#68547 = CARTESIAN_POINT ( 'NONE',  ( 11.78648345035333378, 4.393516549646564684, 195.0000000000000284 ) ) ;
#68548 = VERTEX_POINT ( 'NONE', #11888 ) ;
#68549 = ORIENTED_EDGE ( 'NONE', *, *, #44214, .T. ) ;
#68550 = VECTOR ( 'NONE', #3764, 1000.000000000000000 ) ;
#68551 = AXIS2_PLACEMENT_3D ( 'NONE', #20512, #64690, #37826 ) ;
#68552 = CARTESIAN_POINT ( 'NONE',  ( 0.000000000000000000, 8.250000000000001776, -8.000000000000000000 ) ) ;
#68553 = ORIENTED_EDGE ( 'NONE', *, *, #15900, .T. ) ;
#68554 = DIRECTION ( 'NONE',  ( 0.000000000000000000, 1.000000000000000000, 0.000000000000000000 ) ) ;
#68556 = CARTESIAN_POINT ( 'NONE',  ( 26.90000000000000213, -21.00000000000000000, 13.86939075806900057 ) ) ;
#68555 = VECTOR ( 'NONE', #37083, 1000.000000000000000 ) ;
#68557 = CARTESIAN_POINT ( 'NONE',  ( 7.532023737882783898, 3.834182069070696031, 54.00000000000000711 ) ) ;
#68558 = ORIENTED_EDGE ( 'NONE', *, *, #56429, .T. ) ;
#68559 = CIRCLE ( 'NONE', #65241, 0.1999999999999987899 ) ;
#68560 = LINE ( 'NONE', #46274, #62875 ) ;
#68561 = DIRECTION ( 'NONE',  ( 0.000000000000000000, 0.000000000000000000, -1.000000000000000000 ) ) ;
#68562 = EDGE_LOOP ( 'NONE', ( #66072, #21039, #29443, #23870 ) ) ;
#68564 = VERTEX_POINT ( 'NONE', #11210 ) ;
#68563 = DIRECTION ( 'NONE',  ( 0.000000000000000000, -0.7071067811865475727, -0.7071067811865475727 ) ) ;
#68565 = DIRECTION ( 'NONE',  ( 1.000000000000000000, 0.000000000000000000, 0.000000000000000000 ) ) ;
#68566 = DIRECTION ( 'NONE',  ( 0.000000000000000000, 0.7071067811865474617, -0.7071067811865474617 ) ) ;
#68567 = CARTESIAN_POINT ( 'NONE',  ( -7.813516549646711162, 11.99351654964660341, 455.0000000000000568 ) ) ;
#68568 = DIRECTION ( 'NONE',  ( 0.000000000000000000, 1.000000000000000000, 0.000000000000000000 ) ) ;
#68569 = EDGE_CURVE ( 'NONE', #69196, #56572, #44078, .T. ) ;
#68570 = FACE_OUTER_BOUND ( 'NONE', #62647, .T. ) ;
#68571 = ORIENTED_EDGE ( 'NONE', *, *, #44387, .T. ) ;
#68572 = DIRECTION ( 'NONE',  ( -1.836970198721029934E-16, 1.836970198721036344E-16, -1.000000000000000000 ) ) ;
#68573 = DIRECTION ( 'NONE',  ( -1.000000000000000000, 0.000000000000000000, 0.000000000000000000 ) ) ;
#68574 = CYLINDRICAL_SURFACE ( 'NONE', #8584, 0.3999999999999993006 ) ;
#68576 = VERTEX_POINT ( 'NONE', #65654 ) ;
#68575 = DIRECTION ( 'NONE',  ( 0.000000000000000000, 0.000000000000000000, 1.000000000000000000 ) ) ;
#68577 = CARTESIAN_POINT ( 'NONE',  ( -9.689726262117227762, 10.03972626211718300, 54.00000000000000711 ) ) ;
#68578 = AXIS2_PLACEMENT_3D ( 'NONE', #47001, #24737, #52310 ) ;
#68579 = FACE_OUTER_BOUND ( 'NONE', #55601, .T. ) ;
#68580 = ADVANCED_FACE ( 'NONE', ( #33122 ), #43742, .F. ) ;
#68581 = LINE ( 'NONE', #21528, #44648 ) ;
#68582 = ORIENTED_EDGE ( 'NONE', *, *, #14016, .T. ) ;
#68583 = CARTESIAN_POINT ( 'NONE',  ( 8.250000000000005329, -7.249999999999998224, -26.00000000000001066 ) ) ;
#68584 = DIRECTION ( 'NONE',  ( 1.000000000000000000, -0.000000000000000000, -0.000000000000000000 ) ) ;
#68585 = EDGE_LOOP ( 'NONE', ( #33624, #34663, #45843, #1086 ) ) ;
#68586 = FACE_OUTER_BOUND ( 'NONE', #56796, .T. ) ;
#68587 = CYLINDRICAL_SURFACE ( 'NONE', #45858, 25.39999999999999858 ) ;
#68588 = AXIS2_PLACEMENT_3D ( 'NONE', #20454, #47326, #69934 ) ;
#68589 = AXIS2_PLACEMENT_3D ( 'NONE', #69868, #42995, #27433 ) ;
#68590 = DIRECTION ( 'NONE',  ( -0.000000000000000000, -0.000000000000000000, -1.000000000000000000 ) ) ;
#68591 = EDGE_CURVE ( 'NONE', #40253, #19785, #69915, .T. ) ;
#68592 = DIRECTION ( 'NONE',  ( 0.000000000000000000, 0.000000000000000000, 1.000000000000000000 ) ) ;
#68593 = CIRCLE ( 'NONE', #31313, 0.1749999999999989342 ) ;
#68594 = CARTESIAN_POINT ( 'NONE',  ( 41.09999999999999432, -14.06939075806901940, -20.80000000000000426 ) ) ;
#68595 = VERTEX_POINT ( 'NONE', #21824 ) ;
#68596 = DIRECTION ( 'NONE',  ( -0.000000000000000000, -0.7071067811865474617, 0.7071067811865474617 ) ) ;
#68597 = VERTEX_POINT ( 'NONE', #16174 ) ;
#68598 = FACE_OUTER_BOUND ( 'NONE', #27344, .T. ) ;
#68599 = ORIENTED_EDGE ( 'NONE', *, *, #65490, .F. ) ;
#68600 = ORIENTED_EDGE ( 'NONE', *, *, #67046, .F. ) ;
#68601 = FACE_OUTER_BOUND ( 'NONE', #46669, .T. ) ;
#68602 = AXIS2_PLACEMENT_3D ( 'NONE', #30215, #8277, #57074 ) ;
#68603 = VECTOR ( 'NONE', #38772, 1000.000000000000000 ) ;
#68604 = EDGE_CURVE ( 'NONE', #39010, #13815, #970, .T. ) ;
#68605 = CARTESIAN_POINT ( 'NONE',  ( -7.250000000000000888, 7.250000000000001776, -17.50000000000000000 ) ) ;
#68606 = CARTESIAN_POINT ( 'NONE',  ( 29.89999999999999858, 0.000000000000000000, 0.000000000000000000 ) ) ;
#68607 = EDGE_LOOP ( 'NONE', ( #14506, #60674, #63481, #43084, #2749, #13741, #44665, #18578 ) ) ;
#68608 = ORIENTED_EDGE ( 'NONE', *, *, #7751, .F. ) ;
#68609 = FACE_OUTER_BOUND ( 'NONE', #23648, .T. ) ;
#68610 = ORIENTED_EDGE ( 'NONE', *, *, #38901, .F. ) ;
#68611 = ORIENTED_EDGE ( 'NONE', *, *, #18123, .T. ) ;
#68612 = CIRCLE ( 'NONE', #38133, 4.500000000000191847 ) ;
#68613 = CARTESIAN_POINT ( 'NONE',  ( 7.450000000000004619, -1.336933437520057563E-15, -25.00000000000000000 ) ) ;
#68614 = DIRECTION ( 'NONE',  ( 0.000000000000000000, 1.000000000000000000, 0.000000000000000000 ) ) ;
#68615 = LINE ( 'NONE', #68252, #55824 ) ;
#68616 = EDGE_CURVE ( 'NONE', #18784, #10363, #16565, .T. ) ;
#68617 = VERTEX_POINT ( 'NONE', #5570 ) ;
#68618 = DIRECTION ( 'NONE',  ( -0.000000000000000000, -0.000000000000000000, -1.000000000000000000 ) ) ;
#68620 = CARTESIAN_POINT ( 'NONE',  ( -7.250000000000000888, -8.249999999999998224, -20.50000000000000000 ) ) ;
#68619 = CARTESIAN_POINT ( 'NONE',  ( -7.450000000000001954, -7.249999999999998224, -18.50000000000000000 ) ) ;
#68621 = ORIENTED_EDGE ( 'NONE', *, *, #15718, .F. ) ;
#68624 = ORIENTED_EDGE ( 'NONE', *, *, #59511, .T. ) ;
#68623 = EDGE_CURVE ( 'NONE', #44169, #26101, #27134, .T. ) ;
#68622 = CARTESIAN_POINT ( 'NONE',  ( 105.8309041053263257, 3.657408540445008960, 10.00000000000000000 ) ) ;
#68625 = ORIENTED_EDGE ( 'NONE', *, *, #38423, .F. ) ;
#68626 = ADVANCED_FACE ( 'NONE', ( #64614 ), #27476, .F. ) ;
#68627 = FACE_OUTER_BOUND ( 'NONE', #2460, .T. ) ;
#68628 = ADVANCED_FACE ( 'NONE', ( #37746 ), #33477, .T. ) ;
#68629 = DIRECTION ( 'NONE',  ( 0.000000000000000000, 1.000000000000000000, 0.000000000000000000 ) ) ;
#68630 = ORIENTED_EDGE ( 'NONE', *, *, #59380, .F. ) ;
#68631 = AXIS2_PLACEMENT_3D ( 'NONE', #50646, #12457, #7849 ) ;
#68632 = ORIENTED_EDGE ( 'NONE', *, *, #32340, .T. ) ;
#68633 = LINE ( 'NONE', #9230, #26414 ) ;
#68634 = CARTESIAN_POINT ( 'NONE',  ( 49.00000000000000000, 20.60000000000000142, -13.86939075806900057 ) ) ;
#68635 = ORIENTED_EDGE ( 'NONE', *, *, #65583, .T. ) ;
#68636 = ORIENTED_EDGE ( 'NONE', *, *, #65106, .T. ) ;
#68637 = CIRCLE ( 'NONE', #20070, 1.224999999999999423 ) ;
#68638 = LINE ( 'NONE', #37168, #51131 ) ;
#68639 = PLANE ( 'NONE',  #15890 ) ;
#68640 = ORIENTED_EDGE ( 'NONE', *, *, #33110, .T. ) ;
#68641 = VECTOR ( 'NONE', #49883, 1000.000000000000000 ) ;
#68642 = VECTOR ( 'NONE', #21332, 1000.000000000000000 ) ;
#68643 = CARTESIAN_POINT ( 'NONE',  ( 9.912023737882815766, -3.682023737882826886, 54.00000000000000711 ) ) ;
#68644 = EDGE_CURVE ( 'NONE', #32305, #15923, #10868, .T. ) ;
#68645 = CARTESIAN_POINT ( 'NONE',  ( 283.0000000000000568, -27.13000000000000611, 13.50000000000000000 ) ) ;
#68646 = CIRCLE ( 'NONE', #56217, 4.000000000000000000 ) ;
#68648 = ORIENTED_EDGE ( 'NONE', *, *, #67881, .F. ) ;
#68647 = CARTESIAN_POINT ( 'NONE',  ( -6.835476262117260227, 10.30047626211718104, 54.00000000000000711 ) ) ;
#68649 = EDGE_LOOP ( 'NONE', ( #44063, #69742, #28955, #50081 ) ) ;
#68650 = CARTESIAN_POINT ( 'NONE',  ( 6.665817930929288870, 7.342976262117195674, 54.00000000000000711 ) ) ;
#68651 = VECTOR ( 'NONE', #4744, 1000.000000000000114 ) ;
#68652 = VECTOR ( 'NONE', #61817, 1000.000000000000000 ) ;
#68653 = CARTESIAN_POINT ( 'NONE',  ( 25.57999999999999829, 0.000000000000000000, 0.000000000000000000 ) ) ;
#68654 = FACE_OUTER_BOUND ( 'NONE', #17360, .T. ) ;
#68655 = CARTESIAN_POINT ( 'NONE',  ( -7.250000000000000888, 7.450000000000003730, -15.50000000000000000 ) ) ;
#68656 = EDGE_CURVE ( 'NONE', #43571, #27271, #6417, .T. ) ;
#68657 = LINE ( 'NONE', #3244, #38474 ) ;
#68658 = CYLINDRICAL_SURFACE ( 'NONE', #11212, 1.000000000000000000 ) ;
#68659 = ORIENTED_EDGE ( 'NONE', *, *, #39218, .F. ) ;
#68660 = CARTESIAN_POINT ( 'NONE',  ( 12.90000000000000213, -14.06939075806900163, -20.80000000000000426 ) ) ;
#68661 = ADVANCED_FACE ( 'NONE', ( #38444 ), #59991, .F. ) ;
#68663 = ORIENTED_EDGE ( 'NONE', *, *, #39762, .T. ) ;
#68662 = FACE_OUTER_BOUND ( 'NONE', #47936, .T. ) ;
#68664 = AXIS2_PLACEMENT_3D ( 'NONE', #29505, #23153, #55348 ) ;
#68665 = PLANE ( 'NONE',  #68334 ) ;
#68666 = DIRECTION ( 'NONE',  ( 1.000000000000000000, -0.000000000000000000, 0.000000000000000000 ) ) ;
#68667 = DIRECTION ( 'NONE',  ( -1.000000000000000000, 1.221996412923863792E-14, 1.836970198721052367E-16 ) ) ;
#68668 = EDGE_CURVE ( 'NONE', #55879, #37116, #40262, .T. ) ;
#68669 = CARTESIAN_POINT ( 'NONE',  ( 3.857023737882813386, 10.30047626211720768, 26.00000000000000711 ) ) ;
#68670 = EDGE_CURVE ( 'NONE', #26198, #7905, #54701, .T. ) ;
#68671 = VERTEX_POINT ( 'NONE', #49406 ) ;
#68672 = CARTESIAN_POINT ( 'NONE',  ( 30.00000000000000000, -12.00000000000000000, -10.20500000000000007 ) ) ;
#68673 = FACE_OUTER_BOUND ( 'NONE', #40831, .T. ) ;
#68674 = EDGE_LOOP ( 'NONE', ( #54213, #7983, #60523, #39568 ) ) ;
#68675 = DIRECTION ( 'NONE',  ( 0.7671651518152939886, -0.6414496315691645689, 2.309356642088622481E-17 ) ) ;
#68676 = CARTESIAN_POINT ( 'NONE',  ( -4.031976262117261456, 3.142976262117183506, 54.00000000000000711 ) ) ;
#68677 = EDGE_CURVE ( 'NONE', #6775, #52725, #64967, .T. ) ;
#68678 = DIRECTION ( 'NONE',  ( 1.000000000000000000, -0.000000000000000000, 0.000000000000000000 ) ) ;
#68679 = VERTEX_POINT ( 'NONE', #59659 ) ;
#68680 = CARTESIAN_POINT ( 'NONE',  ( -9.093516549646826874, -10.92648345035338941, 455.0000000000000568 ) ) ;
#68681 = ORIENTED_EDGE ( 'NONE', *, *, #31878, .T. ) ;
#68682 = EDGE_CURVE ( 'NONE', #14586, #23311, #49733, .T. ) ;
#68683 = ORIENTED_EDGE ( 'NONE', *, *, #48082, .T. ) ;
#68684 = ADVANCED_FACE ( 'NONE', ( #37402 ), #32090, .T. ) ;
#68685 = CARTESIAN_POINT ( 'NONE',  ( 5.257023737882819070, -5.257023737882825287, 54.00000000000000711 ) ) ;
#68686 = CYLINDRICAL_SURFACE ( 'NONE', #54599, 0.1749999999999980738 ) ;
#68687 = DIRECTION ( 'NONE',  ( -0.000000000000000000, -0.000000000000000000, -1.000000000000000000 ) ) ;
#68688 = ADVANCED_FACE ( 'NONE', ( #50764 ), #35190, .F. ) ;
#68689 = ADVANCED_FACE ( 'NONE', ( #1299 ), #39122, .F. ) ;
#68690 = ADVANCED_FACE ( 'NONE', ( #13291 ), #34496, .F. ) ;
#68691 = CARTESIAN_POINT ( 'NONE',  ( -7.250000000000000888, 7.250000000000001776, -8.000000000000000000 ) ) ;
#68692 = CARTESIAN_POINT ( 'NONE',  ( 11.00000000000000000, -17.50000000000000000, 26.64999999999999858 ) ) ;
#68693 = ORIENTED_EDGE ( 'NONE', *, *, #7498, .T. ) ;
#68694 = VERTEX_POINT ( 'NONE', #55393 ) ;
#68696 = ORIENTED_EDGE ( 'NONE', *, *, #62333, .F. ) ;
#68695 = DIRECTION ( 'NONE',  ( 0.000000000000000000, 0.000000000000000000, 1.000000000000000000 ) ) ;
#68697 = EDGE_CURVE ( 'NONE', #41134, #14927, #62069, .T. ) ;
#68698 = ORIENTED_EDGE ( 'NONE', *, *, #21646, .T. ) ;
#68699 = VECTOR ( 'NONE', #20500, 1000.000000000000000 ) ;
#68700 = FACE_OUTER_BOUND ( 'NONE', #12166, .T. ) ;
#68701 = CARTESIAN_POINT ( 'NONE',  ( -4.727349090213504468, -4.201500623656015065, 195.0000000000000284 ) ) ;
#68702 = ADVANCED_FACE ( 'NONE', ( #50076 ), #66344, .F. ) ;
#68703 = DIRECTION ( 'NONE',  ( -0.000000000000000000, -0.000000000000000000, 1.000000000000000000 ) ) ;
#68704 = ADVANCED_FACE ( 'NONE', ( #60689 ), #12924, .F. ) ;
#68705 = VECTOR ( 'NONE', #30357, 1000.000000000000000 ) ;
#68706 = DIRECTION ( 'NONE',  ( 0.8660254037844311581, -0.5000000000000129896, 6.723777587268175486E-17 ) ) ;
#68708 = CARTESIAN_POINT ( 'NONE',  ( -7.250000000000000000, -7.449999999999998401, -25.50000000000000355 ) ) ;
#68707 = FACE_OUTER_BOUND ( 'NONE', #58612, .T. ) ;
#68709 = ORIENTED_EDGE ( 'NONE', *, *, #22090, .F. ) ;
#68710 = ORIENTED_EDGE ( 'NONE', *, *, #54639, .F. ) ;
#68711 = ORIENTED_EDGE ( 'NONE', *, *, #28258, .T. ) ;
#68712 = VERTEX_POINT ( 'NONE', #40151 ) ;
#68713 = FACE_OUTER_BOUND ( 'NONE', #38211, .T. ) ;
#68714 = EDGE_CURVE ( 'NONE', #21845, #23827, #7974, .T. ) ;
#68715 = DIRECTION ( 'NONE',  ( 0.000000000000000000, -0.000000000000000000, -1.000000000000000000 ) ) ;
#68716 = ADVANCED_FACE ( 'NONE', ( #13638, #8327 ), #28501, .F. ) ;
#68717 = AXIS2_PLACEMENT_3D ( 'NONE', #51338, #4923, #8545 ) ;
#68718 = DIRECTION ( 'NONE',  ( -0.000000000000000000, -0.000000000000000000, -1.000000000000000000 ) ) ;
#68719 = ORIENTED_EDGE ( 'NONE', *, *, #29508, .T. ) ;
#68720 = VERTEX_POINT ( 'NONE', #51119 ) ;
#68721 = ORIENTED_EDGE ( 'NONE', *, *, #66313, .T. ) ;
#68722 = CARTESIAN_POINT ( 'NONE',  ( 7.811466277050736373, -4.740315990920159983, 195.0000000000000284 ) ) ;
#68723 = ORIENTED_EDGE ( 'NONE', *, *, #27842, .F. ) ;
#68724 = ORIENTED_EDGE ( 'NONE', *, *, #32425, .F. ) ;
#68725 = LINE ( 'NONE', #63767, #46873 ) ;
#68726 = ORIENTED_EDGE ( 'NONE', *, *, #7123, .F. ) ;
#68727 = ORIENTED_EDGE ( 'NONE', *, *, #64781, .F. ) ;
#68728 = LINE ( 'NONE', #13218, #57585 ) ;
#68730 = ORIENTED_EDGE ( 'NONE', *, *, #42717, .T. ) ;
#68729 = LINE ( 'NONE', #30888, #17593 ) ;
#68731 = ORIENTED_EDGE ( 'NONE', *, *, #69873, .T. ) ;
#68732 = CARTESIAN_POINT ( 'NONE',  ( 9.562023737882812569, -2.369523737882815784, 26.00000000000000711 ) ) ;
#68733 = DIRECTION ( 'NONE',  ( -1.000000000000000000, 0.000000000000000000, 0.000000000000000000 ) ) ;
#68735 = ORIENTED_EDGE ( 'NONE', *, *, #28125, .F. ) ;
#68734 = CARTESIAN_POINT ( 'NONE',  ( 11.50000000000000000, -12.00000000000000000, 10.69999999999999929 ) ) ;
#68736 = ORIENTED_EDGE ( 'NONE', *, *, #55111, .T. ) ;
#68737 = DIRECTION ( 'NONE',  ( -1.836970198721029934E-16, -1.836970198721010706E-16, 1.000000000000000000 ) ) ;
#68738 = LINE ( 'NONE', #4733, #67919 ) ;
#68739 = CARTESIAN_POINT ( 'NONE',  ( -5.380658396643315022, -4.747751991980679875, 455.0000000000000568 ) ) ;
#68740 = DIRECTION ( 'NONE',  ( -1.000000000000000000, 1.115702204244422993E-14, 0.000000000000000000 ) ) ;
#68741 = ORIENTED_EDGE ( 'NONE', *, *, #40898, .F. ) ;
#68742 = DIRECTION ( 'NONE',  ( 0.000000000000000000, -1.000000000000000000, 0.000000000000000000 ) ) ;
#68743 = AXIS2_PLACEMENT_3D ( 'NONE', #35803, #45704, #46066 ) ;
#68744 = EDGE_CURVE ( 'NONE', #1475, #69663, #45922, .T. ) ;
#68745 = DIRECTION ( 'NONE',  ( 0.7671651518153006499, 0.6414496315691565753, 0.000000000000000000 ) ) ;
#68746 = ORIENTED_EDGE ( 'NONE', *, *, #8208, .T. ) ;
#68748 = ADVANCED_FACE ( 'NONE', ( #6933 ), #7634, .T. ) ;
#68747 = DIRECTION ( 'NONE',  ( -1.000000000000000000, 0.000000000000000000, 0.000000000000000000 ) ) ;
#68749 = DIRECTION ( 'NONE',  ( -0.000000000000000000, 3.673940397442059868E-16, -1.000000000000000000 ) ) ;
#68750 = AXIS2_PLACEMENT_3D ( 'NONE', #50712, #1575, #23142 ) ;
#68751 = DIRECTION ( 'NONE',  ( -0.000000000000000000, 3.673940397442059868E-16, -1.000000000000000000 ) ) ;
#68752 = ADVANCED_FACE ( 'NONE', ( #67032 ), #7278, .T. ) ;
#68753 = ORIENTED_EDGE ( 'NONE', *, *, #25290, .T. ) ;
#68754 = CARTESIAN_POINT ( 'NONE',  ( 11.75000000000000000, -5.200000000000001066, -11.75000000000000000 ) ) ;
#68755 = EDGE_CURVE ( 'NONE', #58374, #20073, #45111, .T. ) ;
#68756 = CARTESIAN_POINT ( 'NONE',  ( 0.000000000000000000, -7.449999999999998401, -22.50000000000000000 ) ) ;
#68757 = CIRCLE ( 'NONE', #38280, 2.000000000000001776 ) ;
#68758 = DIRECTION ( 'NONE',  ( 0.000000000000000000, -1.000000000000000000, 0.000000000000000000 ) ) ;
#68759 = ORIENTED_EDGE ( 'NONE', *, *, #3509, .F. ) ;
#68760 = CARTESIAN_POINT ( 'NONE',  ( -7.450000000000001954, -7.249999999999998224, -20.00000000000000000 ) ) ;
#68761 = DIRECTION ( 'NONE',  ( -1.000000000000000000, 0.000000000000000000, 0.000000000000000000 ) ) ;
#68762 = PLANE ( 'NONE',  #51163 ) ;
#68763 = FACE_OUTER_BOUND ( 'NONE', #34585, .T. ) ;
#68764 = CARTESIAN_POINT ( 'NONE',  ( 11.50000000000000000, -11.50000000000000000, -15.00000000000000000 ) ) ;
#68765 = ORIENTED_EDGE ( 'NONE', *, *, #17177, .T. ) ;
#68766 = DIRECTION ( 'NONE',  ( 1.224646799147353207E-16, 1.000000000000000000, -0.000000000000000000 ) ) ;
#68767 = DIRECTION ( 'NONE',  ( 0.000000000000000000, 0.000000000000000000, -1.000000000000000000 ) ) ;
#68768 = DIRECTION ( 'NONE',  ( -0.000000000000000000, -0.000000000000000000, -1.000000000000000000 ) ) ;
#68769 = ADVANCED_FACE ( 'NONE', ( #61730 ), #39797, .F. ) ;
#68770 = DIRECTION ( 'NONE',  ( -0.000000000000000000, -0.000000000000000000, -1.000000000000000000 ) ) ;
#68771 = DIRECTION ( 'NONE',  ( -0.7071067811865474617, -0.7071067811865474617, -0.000000000000000000 ) ) ;
#68772 = ORIENTED_EDGE ( 'NONE', *, *, #51588, .F. ) ;
#68774 = ORIENTED_EDGE ( 'NONE', *, *, #44317, .T. ) ;
#68773 = DIRECTION ( 'NONE',  ( 0.000000000000000000, 0.000000000000000000, 1.000000000000000000 ) ) ;
#68775 = DIRECTION ( 'NONE',  ( 1.000000000000000000, -0.000000000000000000, -0.000000000000000000 ) ) ;
#68776 = LINE ( 'NONE', #41189, #69654 ) ;
#68777 = CARTESIAN_POINT ( 'NONE',  ( 6.665817930929285318, 7.517976262117199937, 26.00000000000000711 ) ) ;
#68778 = EDGE_LOOP ( 'NONE', ( #67489, #64990, #21399, #30142 ) ) ;
#68779 =( NAMED_UNIT ( * ) SI_UNIT ( $, .STERADIAN. ) SOLID_ANGLE_UNIT ( ) );
#68780 = DIRECTION ( 'NONE',  ( 0.000000000000000000, 0.000000000000000000, 1.000000000000000000 ) ) ;
#68781 = ORIENTED_EDGE ( 'NONE', *, *, #5823, .F. ) ;
#68782 = ORIENTED_EDGE ( 'NONE', *, *, #10877, .F. ) ;
#68783 = CIRCLE ( 'NONE', #15696, 0.6000000000000006439 ) ;
#68784 = EDGE_LOOP ( 'NONE', ( #46440, #35768 ) ) ;
#68785 = EDGE_CURVE ( 'NONE', #37150, #38571, #47106, .T. ) ;
#68786 = CARTESIAN_POINT ( 'NONE',  ( -8.513516549646713116, 11.29351654964659701, 194.9999952000000292 ) ) ;
#68787 = AXIS2_PLACEMENT_3D ( 'NONE', #15299, #25918, #47466 ) ;
#68788 = CARTESIAN_POINT ( 'NONE',  ( 78.77321854994620765, 47.95351654967443977, 43.00000000000000000 ) ) ;
#68790 = EDGE_CURVE ( 'NONE', #53780, #8234, #24612, .T. ) ;
#68789 = DIRECTION ( 'NONE',  ( -0.000000000000000000, 3.673940397442059868E-16, -1.000000000000000000 ) ) ;
#68791 = EDGE_LOOP ( 'NONE', ( #57639, #45994, #11957, #51283 ) ) ;
#68793 = ADVANCED_FACE ( 'NONE', ( #46509 ), #9035, .F. ) ;
#68792 = ORIENTED_EDGE ( 'NONE', *, *, #17125, .T. ) ;
#68794 = PLANE ( 'NONE',  #18816 ) ;
#68795 = CIRCLE ( 'NONE', #1061, 24.99999999998784972 ) ;
#68796 = DIRECTION ( 'NONE',  ( 0.000000000000000000, -0.8206518066484758123, -0.5714285714283042772 ) ) ;
#68797 = EDGE_LOOP ( 'NONE', ( #62512, #42944, #5029, #179 ) ) ;
#68798 = VERTEX_POINT ( 'NONE', #41207 ) ;
#68799 = ORIENTED_EDGE ( 'NONE', *, *, #33302, .T. ) ;
#68800 = VECTOR ( 'NONE', #49757, 1000.000000000000114 ) ;
#68801 = VERTEX_POINT ( 'NONE', #57824 ) ;
#68802 = DIRECTION ( 'NONE',  ( -0.000000000000000000, 3.673940397442059868E-16, -1.000000000000000000 ) ) ;
#68804 = VERTEX_POINT ( 'NONE', #68085 ) ;
#68803 = DIRECTION ( 'NONE',  ( -1.047444401652940007E-14, -1.000000000000000000, -1.836970198721029934E-16 ) ) ;
#68806 = CIRCLE ( 'NONE', #39407, 2.204799999999997429 ) ;
#68805 = VECTOR ( 'NONE', #20738, 1000.000000000000000 ) ;
#68807 = DIRECTION ( 'NONE',  ( 0.000000000000000000, -0.7071067811865475727, 0.7071067811865475727 ) ) ;
#68808 = FACE_OUTER_BOUND ( 'NONE', #15335, .T. ) ;
#68809 = CARTESIAN_POINT ( 'NONE',  ( 275.0000000000000000, -28.94999999999999929, -13.50000000000000000 ) ) ;
#68810 = VERTEX_POINT ( 'NONE', #40858 ) ;
#68811 = ORIENTED_EDGE ( 'NONE', *, *, #24048, .T. ) ;
#68812 = CIRCLE ( 'NONE', #25924, 1.000000000000002665 ) ;
#68813 = CARTESIAN_POINT ( 'NONE',  ( -11.07551654964682797, -11.08848345035333693, 455.0000000000000568 ) ) ;
#68814 = CARTESIAN_POINT ( 'NONE',  ( 4.740315990920129785, -4.201500623656049704, 195.0000000000000284 ) ) ;
#68815 = ORIENTED_EDGE ( 'NONE', *, *, #19789, .F. ) ;
#68816 = ADVANCED_FACE ( 'NONE', ( #62413 ), #4101, .F. ) ;
#68817 = DIRECTION ( 'NONE',  ( -0.000000000000000000, -0.000000000000000000, -1.000000000000000000 ) ) ;
#68818 = CARTESIAN_POINT ( 'NONE',  ( 29.25000000000000000, -5.000000000000000000, 26.25000000000000000 ) ) ;
#68819 = FACE_OUTER_BOUND ( 'NONE', #58271, .T. ) ;
#68820 = ORIENTED_EDGE ( 'NONE', *, *, #19159, .F. ) ;
#68821 = CARTESIAN_POINT ( 'NONE',  ( 8.250000000000005329, -8.249999999999998224, -26.00000000000001066 ) ) ;
#68823 = EDGE_CURVE ( 'NONE', #43477, #523, #25676, .T. ) ;
#68822 = DIRECTION ( 'NONE',  ( 0.000000000000000000, 1.000000000000000000, -0.000000000000000000 ) ) ;
#68824 = DIRECTION ( 'NONE',  ( -1.000000000000000000, 0.000000000000000000, 0.000000000000000000 ) ) ;
#68825 = DIRECTION ( 'NONE',  ( -0.000000000000000000, -0.000000000000000000, -1.000000000000000000 ) ) ;
#68826 = ADVANCED_FACE ( 'NONE', ( #9393 ), #13989, .F. ) ;
#68827 = ADVANCED_FACE ( 'NONE', ( #63132 ), #68794, .F. ) ;
#68828 = CARTESIAN_POINT ( 'NONE',  ( 106.4257688009193430, 0.000000000000000000, 330.9830310981789694 ) ) ;
#68830 = ORIENTED_EDGE ( 'NONE', *, *, #50884, .F. ) ;
#68829 = ADVANCED_FACE ( 'NONE', ( #3389 ), #57127, .T. ) ;
#68831 = CYLINDRICAL_SURFACE ( 'NONE', #4246, 4.000000000000000000 ) ;
#68832 = ADVANCED_FACE ( 'NONE', ( #51827 ), #52177, .F. ) ;
#68833 = LINE ( 'NONE', #69527, #46363 ) ;
#68834 = AXIS2_PLACEMENT_3D ( 'NONE', #4852, #53304, #25367 ) ;
#68835 =( NAMED_UNIT ( * ) PLANE_ANGLE_UNIT ( ) SI_UNIT ( $, .RADIAN. ) );
#68836 = VECTOR ( 'NONE', #41724, 1000.000000000000000 ) ;
#68837 = DIRECTION ( 'NONE',  ( 0.000000000000000000, -1.000000000000000000, 0.000000000000000000 ) ) ;
#68838 = ADVANCED_FACE ( 'NONE', ( #30266 ), #36258, .T. ) ;
#68839 = LINE ( 'NONE', #63175, #48463 ) ;
#68840 = DIRECTION ( 'NONE',  ( 0.000000000000000000, -3.673940397442059868E-16, 1.000000000000000000 ) ) ;
#68841 = AXIS2_PLACEMENT_3D ( 'NONE', #38566, #18016, #60119 ) ;
#68842 = CARTESIAN_POINT ( 'NONE',  ( -2.752095193409373586, 9.942044687070435316, 455.0000000000000568 ) ) ;
#68843 = LINE ( 'NONE', #52945, #30766 ) ;
#68844 = ORIENTED_EDGE ( 'NONE', *, *, #42707, .F. ) ;
#68845 = CARTESIAN_POINT ( 'NONE',  ( -9.897976262117291313, -6.657023737882756365, 54.00000000000000711 ) ) ;
#68846 = FACE_OUTER_BOUND ( 'NONE', #9310, .T. ) ;
#68847 = DIRECTION ( 'NONE',  ( 1.000000000000000000, -5.981805089575194965E-17, 0.000000000000000000 ) ) ;
#68848 = CARTESIAN_POINT ( 'NONE',  ( 8.250000000000005329, 7.250000000000000888, -26.00000000000001066 ) ) ;
#68849 = AXIS2_PLACEMENT_3D ( 'NONE', #51790, #24914, #46474 ) ;
#68850 = CARTESIAN_POINT ( 'NONE',  ( 39.00000000000000000, 0.000000000000000000, 5.000000000000000000 ) ) ;
#68851 = LINE ( 'NONE', #43012, #33107 ) ;
#68852 = CARTESIAN_POINT ( 'NONE',  ( 4.149127210878741145, 3.663616288756999406, 54.00000000000000711 ) ) ;
#68853 = VERTEX_POINT ( 'NONE', #62780 ) ;
#68854 = CIRCLE ( 'NONE', #33802, 0.5249999999999994671 ) ;
#68855 = ORIENTED_EDGE ( 'NONE', *, *, #52727, .F. ) ;
#68856 = LINE ( 'NONE', #14760, #56400 ) ;
#68857 = DIRECTION ( 'NONE',  ( 0.000000000000000000, 0.000000000000000000, 1.000000000000000000 ) ) ;
#68858 = ORIENTED_EDGE ( 'NONE', *, *, #4360, .T. ) ;
#68859 = CARTESIAN_POINT ( 'NONE',  ( 8.930623737882843471, 8.566576262117187923, 54.00000000000000711 ) ) ;
#68860 = AXIS2_PLACEMENT_3D ( 'NONE', #51064, #41856, #36198 ) ;
#68861 = DIRECTION ( 'NONE',  ( 0.000000000000000000, 0.7071067811865470176, -0.7071067811865480168 ) ) ;
#68862 = ORIENTED_EDGE ( 'NONE', *, *, #48380, .T. ) ;
#68863 = DIRECTION ( 'NONE',  ( -4.956352788505180820E-15, -1.000000000000000000, 0.000000000000000000 ) ) ;
#68864 = ORIENTED_EDGE ( 'NONE', *, *, #36056, .F. ) ;
#68865 = VERTEX_POINT ( 'NONE', #14357 ) ;
#68866 = DIRECTION ( 'NONE',  ( 0.000000000000000000, -0.7071067811865474617, -0.7071067811865474617 ) ) ;
#68867 = ORIENTED_EDGE ( 'NONE', *, *, #36418, .F. ) ;
#68868 = DIRECTION ( 'NONE',  ( 5.626525616968433120E-15, 1.000000000000000000, 1.836970198721026236E-16 ) ) ;
#68870 = ADVANCED_FACE ( 'NONE', ( #25307 ), #8852, .F. ) ;
#68869 = LINE ( 'NONE', #63573, #7604 ) ;
#68871 = LINE ( 'NONE', #62150, #14078 ) ;
#68872 = AXIS2_PLACEMENT_3D ( 'NONE', #42621, #194, #58552 ) ;
#68873 = ORIENTED_EDGE ( 'NONE', *, *, #37129, .T. ) ;
#68874 = EDGE_CURVE ( 'NONE', #39378, #58511, #61895, .T. ) ;
#68875 = CARTESIAN_POINT ( 'NONE',  ( 283.0000000000000568, -28.94999999999999929, -13.50000000000000000 ) ) ;
#68876 = EDGE_CURVE ( 'NONE', #37589, #14927, #51997, .T. ) ;
#68878 = CARTESIAN_POINT ( 'NONE',  ( -10.30047626211728939, -6.849523737882745600, 26.00000000000000000 ) ) ;
#68877 = FACE_OUTER_BOUND ( 'NONE', #19875, .T. ) ;
#68879 = ORIENTED_EDGE ( 'NONE', *, *, #58976, .F. ) ;
#68880 = ORIENTED_EDGE ( 'NONE', *, *, #42312, .F. ) ;
#68881 = VERTEX_POINT ( 'NONE', #8491 ) ;
#68882 = EDGE_CURVE ( 'NONE', #59231, #54124, #3206, .T. ) ;
#68884 = ORIENTED_EDGE ( 'NONE', *, *, #5151, .T. ) ;
#68883 = ITEM_DEFINED_TRANSFORMATION ( 'NONE', 'NONE', #3072,  #45918 ) ;
#68885 = CARTESIAN_POINT ( 'NONE',  ( 9.690000000000001279, -9.690000000000001279, 0.000000000000000000 ) ) ;
#68886 = CIRCLE ( 'NONE', #38395, 0.1999999999999987899 ) ;
#68887 = VECTOR ( 'NONE', #69910, 1000.000000000000000 ) ;
#68889 = ORIENTED_EDGE ( 'NONE', *, *, #20759, .F. ) ;
#68888 = LINE ( 'NONE', #64285, #19550 ) ;
#68890 = DIRECTION ( 'NONE',  ( -0.000000000000000000, -0.000000000000000000, 1.000000000000000000 ) ) ;
#68891 = AXIS2_PLACEMENT_3D ( 'NONE', #43092, #5625, #27194 ) ;
#68892 = LINE ( 'NONE', #20790, #11375 ) ;
#68893 = ORIENTED_EDGE ( 'NONE', *, *, #33929, .T. ) ;
#68894 = EDGE_LOOP ( 'NONE', ( #62738, #55534, #2430, #36966, #63125, #50503, #11505, #62953 ) ) ;
#68895 = VECTOR ( 'NONE', #51869, 1000.000000000000000 ) ;
#68896 = CARTESIAN_POINT ( 'NONE',  ( -7.250000000000000888, 7.250000000000001776, -21.50000000000000000 ) ) ;
#68897 = ORIENTED_EDGE ( 'NONE', *, *, #7185, .T. ) ;
#68898 = VECTOR ( 'NONE', #29246, 1000.000000000000000 ) ;
#68899 = CARTESIAN_POINT ( 'NONE',  ( -5.242976262117299946, -7.186223737882804663, 54.00000000000000711 ) ) ;
#68900 = LINE ( 'NONE', #284, #37920 ) ;
#68901 = DIRECTION ( 'NONE',  ( -0.000000000000000000, 3.673940397442059868E-16, -1.000000000000000000 ) ) ;
#68902 = ORIENTED_EDGE ( 'NONE', *, *, #1244, .F. ) ;
#68903 = CIRCLE ( 'NONE', #41790, 2.000000000000001776 ) ;
#68904 = DIRECTION ( 'NONE',  ( -1.047444401652940007E-14, -1.000000000000000000, -1.836970198721029934E-16 ) ) ;
#68906 = EDGE_LOOP ( 'NONE', ( #33799, #29483 ) ) ;
#68905 = DIRECTION ( 'NONE',  ( -1.000000000000000000, 0.000000000000000000, -0.000000000000000000 ) ) ;
#68908 = ORIENTED_EDGE ( 'NONE', *, *, #40706, .T. ) ;
#68907 = DIRECTION ( 'NONE',  ( 0.000000000000000000, -1.000000000000000000, 0.000000000000000000 ) ) ;
#68909 = DIRECTION ( 'NONE',  ( 0.000000000000000000, 1.000000000000000000, 0.000000000000000000 ) ) ;
#68910 = VECTOR ( 'NONE', #14198, 1000.000000000000000 ) ;
#68911 = VECTOR ( 'NONE', #69138, 1000.000000000000000 ) ;
#68912 = CARTESIAN_POINT ( 'NONE',  ( 7.408280051175172076, -6.789561617636940660, 26.00000000000000000 ) ) ;
#68913 = LINE ( 'NONE', #68567, #8735 ) ;
#68914 = FACE_OUTER_BOUND ( 'NONE', #63408, .T. ) ;
#68915 = LINE ( 'NONE', #14110, #2573 ) ;
#68916 = ORIENTED_EDGE ( 'NONE', *, *, #8343, .F. ) ;
#68917 = CARTESIAN_POINT ( 'NONE',  ( 10.50702373788281996, -6.849523737882814878, 26.00000000000000000 ) ) ;
#68918 = ADVANCED_FACE ( 'NONE', ( #67905 ), #17762, .F. ) ;
#68919 = CARTESIAN_POINT ( 'NONE',  ( 1.690483450353344352, -10.74648345035345720, 455.0000000000000568 ) ) ;
#68921 = ORIENTED_EDGE ( 'NONE', *, *, #51496, .F. ) ;
#68920 = DIRECTION ( 'NONE',  ( -0.000000000000000000, 3.673940397442059868E-16, -1.000000000000000000 ) ) ;
#68922 = FACE_OUTER_BOUND ( 'NONE', #46001, .T. ) ;
#68923 = ADVANCED_FACE ( 'NONE', ( #46328 ), #45985, .F. ) ;
#68924 = AXIS2_PLACEMENT_3D ( 'NONE', #8789, #40607, #62167 ) ;
#68925 = CARTESIAN_POINT ( 'NONE',  ( 3.157023737882819425, -4.046023737882825877, 54.00000000000000711 ) ) ;
#68926 = FACE_OUTER_BOUND ( 'NONE', #16661, .T. ) ;
#68927 = EDGE_LOOP ( 'NONE', ( #58063, #27137, #40409, #7859 ) ) ;
#68928 = DIRECTION ( 'NONE',  ( -1.000000000000000000, 0.000000000000000000, 0.000000000000000000 ) ) ;
#68929 = CARTESIAN_POINT ( 'NONE',  ( -7.250000000000001776, -7.249999999999998224, -16.50000000000000000 ) ) ;
#68930 = VERTEX_POINT ( 'NONE', #45618 ) ;
#68931 = FACE_OUTER_BOUND ( 'NONE', #21416, .T. ) ;
#68932 = DIRECTION ( 'NONE',  ( 0.000000000000000000, 0.000000000000000000, -1.000000000000000000 ) ) ;
#68933 = CARTESIAN_POINT ( 'NONE',  ( -11.00000000000000000, -16.28999999999710369, 15.00000000000794920 ) ) ;
#68934 = VECTOR ( 'NONE', #45654, 1000.000000000000000 ) ;
#68935 = LINE ( 'NONE', #41705, #28253 ) ;
#68936 = CIRCLE ( 'NONE', #28288, 0.2000000000000005107 ) ;
#68938 = EDGE_CURVE ( 'NONE', #52946, #55726, #35719, .T. ) ;
#68937 = LINE ( 'NONE', #14496, #42143 ) ;
#68939 = VECTOR ( 'NONE', #4843, 1000.000000000000000 ) ;
#68940 = VERTEX_POINT ( 'NONE', #19797 ) ;
#68941 = ORIENTED_EDGE ( 'NONE', *, *, #23393, .T. ) ;
#68942 = ORIENTED_EDGE ( 'NONE', *, *, #45904, .T. ) ;
#68943 = ORIENTED_EDGE ( 'NONE', *, *, #65382, .F. ) ;
#68944 = ORIENTED_EDGE ( 'NONE', *, *, #2016, .T. ) ;
#68945 = AXIS2_PLACEMENT_3D ( 'NONE', #56991, #12542, #8549 ) ;
#68946 = LINE ( 'NONE', #4603, #22410 ) ;
#68947 = AXIS2_PLACEMENT_3D ( 'NONE', #64179, #9005, #14331 ) ;
#68948 = CARTESIAN_POINT ( 'NONE',  ( 0.000000000000000000, -42.00000000000000000, 26.50000000000000000 ) ) ;
#68949 = DIRECTION ( 'NONE',  ( 0.000000000000000000, 0.000000000000000000, 1.000000000000000000 ) ) ;
#68950 = ORIENTED_EDGE ( 'NONE', *, *, #32697, .T. ) ;
#68951 = ORIENTED_EDGE ( 'NONE', *, *, #52267, .F. ) ;
#68952 = DIRECTION ( 'NONE',  ( -1.836970198721029934E-16, 1.836970198721036590E-16, -1.000000000000000000 ) ) ;
#68953 = VERTEX_POINT ( 'NONE', #13801 ) ;
#68954 = EDGE_LOOP ( 'NONE', ( #58289, #32834, #58094, #64265 ) ) ;
#68955 = DIRECTION ( 'NONE',  ( -0.000000000000000000, 3.673940397442059868E-16, -1.000000000000000000 ) ) ;
#68956 = CARTESIAN_POINT ( 'NONE',  ( 290.0000000000000000, -21.00000000000000000, 0.000000000000000000 ) ) ;
#68957 = LINE ( 'NONE', #31490, #9499 ) ;
#68958 = VERTEX_POINT ( 'NONE', #40678 ) ;
#68959 = EDGE_CURVE ( 'NONE', #59745, #54092, #69720, .T. ) ;
#68960 = DIRECTION ( 'NONE',  ( 0.000000000000000000, 0.000000000000000000, -1.000000000000000000 ) ) ;
#68961 = AXIS2_PLACEMENT_3D ( 'NONE', #62995, #18800, #35760 ) ;
#68962 = AXIS2_PLACEMENT_3D ( 'NONE', #23121, #40065, #39721 ) ;
#68964 = DIRECTION ( 'NONE',  ( -1.000000000000000000, 0.000000000000000000, 0.000000000000000000 ) ) ;
#68963 = DIRECTION ( 'NONE',  ( 0.000000000000000000, 0.000000000000000000, 1.000000000000000000 ) ) ;
#68965 = VERTEX_POINT ( 'NONE', #47038 ) ;
#68967 = EDGE_LOOP ( 'NONE', ( #64133, #23992, #12848, #51990 ) ) ;
#68966 = CARTESIAN_POINT ( 'NONE',  ( 29.25000000000000000, -5.200000000000001066, 26.25000000000000000 ) ) ;
#68968 = ORIENTED_EDGE ( 'NONE', *, *, #44947, .T. ) ;
#68969 = EDGE_CURVE ( 'NONE', #15601, #54166, #56587, .T. ) ;
#68970 = DIRECTION ( 'NONE',  ( 0.000000000000000000, 0.000000000000000000, 1.000000000000000000 ) ) ;
#68971 = DIRECTION ( 'NONE',  ( 0.000000000000000000, -1.000000000000000000, -0.000000000000000000 ) ) ;
#68972 = VERTEX_POINT ( 'NONE', #19110 ) ;
#68973 = CARTESIAN_POINT ( 'NONE',  ( 8.250000000000005329, -7.249999999999998224, -26.00000000000001066 ) ) ;
#68974 = CARTESIAN_POINT ( 'NONE',  ( 15.00000000000000000, -21.00000000000000000, -8.000000000000000000 ) ) ;
#68975 = VERTEX_POINT ( 'NONE', #9212 ) ;
#68976 = VERTEX_POINT ( 'NONE', #29707 ) ;
#68977 = FACE_OUTER_BOUND ( 'NONE', #41623, .T. ) ;
#68978 = EDGE_CURVE ( 'NONE', #58887, #20965, #19455, .T. ) ;
#68979 = CARTESIAN_POINT ( 'NONE',  ( 16.89999999999999858, -0.1999999999911430404, -8.864436962241481021E-12 ) ) ;
#68980 = VECTOR ( 'NONE', #48027, 1000.000000000000000 ) ;
#68981 = ORIENTED_EDGE ( 'NONE', *, *, #44533, .T. ) ;
#68982 = AXIS2_PLACEMENT_3D ( 'NONE', #11318, #32895, #5688 ) ;
#68983 = CARTESIAN_POINT ( 'NONE',  ( 8.835729544836285143, 2.530476262117165920, 26.00000000000000711 ) ) ;
#68984 = FACE_OUTER_BOUND ( 'NONE', #42061, .T. ) ;
#68986 = ORIENTED_EDGE ( 'NONE', *, *, #15122, .F. ) ;
#68985 = CARTESIAN_POINT ( 'NONE',  ( -11.00000000000000000, -11.85423089348099879, -9.852125413066602277 ) ) ;
#68988 = ORIENTED_EDGE ( 'NONE', *, *, #20451, .F. ) ;
#68987 = FACE_OUTER_BOUND ( 'NONE', #37205, .T. ) ;
#68989 = AXIS2_PLACEMENT_3D ( 'NONE', #29682, #51253, #30043 ) ;
#68990 = DIRECTION ( 'NONE',  ( 0.000000000000000000, 0.000000000000000000, 1.000000000000000000 ) ) ;
#68991 = LINE ( 'NONE', #41760, #3620 ) ;
#68992 = FACE_OUTER_BOUND ( 'NONE', #54277, .T. ) ;
#68993 = PLANE ( 'NONE',  #65181 ) ;
#68994 = AXIS2_PLACEMENT_3D ( 'NONE', #55468, #39871, #7701 ) ;
#68995 = FACE_OUTER_BOUND ( 'NONE', #64598, .T. ) ;
#68996 = CARTESIAN_POINT ( 'NONE',  ( -3.834182069070817711, -7.357023737882814274, 26.00000000000000711 ) ) ;
#68997 = ORIENTED_EDGE ( 'NONE', *, *, #26721, .F. ) ;
#68998 = CARTESIAN_POINT ( 'NONE',  ( -12.00000000000000178, -11.18999999999999950, -4.250000000000000000 ) ) ;
#68999 = EDGE_CURVE ( 'NONE', #9824, #32145, #13453, .T. ) ;
#69001 = ORIENTED_EDGE ( 'NONE', *, *, #15266, .F. ) ;
#69000 = CARTESIAN_POINT ( 'NONE',  ( 75.42576880091934299, 0.000000000000000000, 330.9830310981789694 ) ) ;
#69002 = DIRECTION ( 'NONE',  ( 0.000000000000000000, 0.000000000000000000, -1.000000000000000000 ) ) ;
#69003 = CARTESIAN_POINT ( 'NONE',  ( 15.50000000000000000, -0.4000000000005274892, -22.50000000000000000 ) ) ;
#69004 = ADVANCED_FACE ( 'NONE', ( #50929 ), #14867, .T. ) ;
#69005 = CARTESIAN_POINT ( 'NONE',  ( 21.90000000000000213, 13.66939075806899240, 20.79999999999999361 ) ) ;
#69006 = EDGE_CURVE ( 'NONE', #24136, #13736, #46675, .T. ) ;
#69007 = LINE ( 'NONE', #55179, #16021 ) ;
#69008 = EDGE_CURVE ( 'NONE', #9016, #16443, #27915, .T. ) ;
#69009 = ORIENTED_EDGE ( 'NONE', *, *, #64367, .T. ) ;
#69010 = DIRECTION ( 'NONE',  ( 1.000000000000000000, -0.000000000000000000, 0.000000000000000000 ) ) ;
#69011 = CYLINDRICAL_SURFACE ( 'NONE', #28295, 3.499999999999999556 ) ;
#69012 = ORIENTED_EDGE ( 'NONE', *, *, #27655, .F. ) ;
#69013 = CARTESIAN_POINT ( 'NONE',  ( -7.250000000000000888, 7.250000000000001776, -20.50000000000000000 ) ) ;
#69014 = ADVANCED_FACE ( 'NONE', ( #14150 ), #68251, .F. ) ;
#69015 = EDGE_CURVE ( 'NONE', #61156, #35196, #18760, .T. ) ;
#69016 = DIRECTION ( 'NONE',  ( -1.000000000000000000, 0.000000000000000000, 0.000000000000000000 ) ) ;
#69017 = ORIENTED_EDGE ( 'NONE', *, *, #56592, .T. ) ;
#69018 = AXIS2_PLACEMENT_3D ( 'NONE', #67745, #18602, #34858 ) ;
#69019 = DIRECTION ( 'NONE',  ( -1.000000000000000000, 0.000000000000000000, 0.000000000000000000 ) ) ;
#69020 = VERTEX_POINT ( 'NONE', #64353 ) ;
#69021 = ORIENTED_EDGE ( 'NONE', *, *, #43061, .T. ) ;
#69022 = CYLINDRICAL_SURFACE ( 'NONE', #69762, 1.224999999999999423 ) ;
#69023 = FACE_OUTER_BOUND ( 'NONE', #55759, .T. ) ;
#69024 = LINE ( 'NONE', #19354, #48037 ) ;
#69025 = DIRECTION ( 'NONE',  ( 0.000000000000000000, 0.000000000000000000, -1.000000000000000000 ) ) ;
#69026 = FACE_OUTER_BOUND ( 'NONE', #4527, .T. ) ;
#69027 = EDGE_LOOP ( 'NONE', ( #23624, #11120, #11679, #59294 ) ) ;
#69028 = ORIENTED_EDGE ( 'NONE', *, *, #18459, .F. ) ;
#69029 = CIRCLE ( 'NONE', #66737, 0.8100000000000017186 ) ;
#69031 = VERTEX_POINT ( 'NONE', #42776 ) ;
#69030 = CARTESIAN_POINT ( 'NONE',  ( 0.9555237378827827754, -9.929523737882790968, 54.00000000000000711 ) ) ;
#69032 = ORIENTED_EDGE ( 'NONE', *, *, #50299, .T. ) ;
#69033 = VECTOR ( 'NONE', #59514, 1000.000000000000000 ) ;
#69034 = CARTESIAN_POINT ( 'NONE',  ( -30.00000000000000000, -14.04000000000000092, 17.04524521594300523 ) ) ;
#69035 = PLANE ( 'NONE',  #51226 ) ;
#69036 = EDGE_CURVE ( 'NONE', #330, #66569, #21901, .T. ) ;
#69037 = DIRECTION ( 'NONE',  ( -1.079558018506126625E-14, -1.000000000000000000, 0.000000000000000000 ) ) ;
#69038 = DIRECTION ( 'NONE',  ( 0.000000000000000000, -1.000000000000000000, -0.000000000000000000 ) ) ;
#69040 = DIRECTION ( 'NONE',  ( 0.000000000000000000, 0.000000000000000000, 1.000000000000000000 ) ) ;
#69039 = DIRECTION ( 'NONE',  ( 0.000000000000000000, 0.000000000000000000, 1.000000000000000000 ) ) ;
#69041 = ORIENTED_EDGE ( 'NONE', *, *, #14926, .T. ) ;
#69042 = VERTEX_POINT ( 'NONE', #4954 ) ;
#69043 = ORIENTED_EDGE ( 'NONE', *, *, #59324, .T. ) ;
#69044 = VECTOR ( 'NONE', #31907, 1000.000000000000000 ) ;
#69045 = CIRCLE ( 'NONE', #59997, 0.5000000000023507862 ) ;
#69046 = EDGE_CURVE ( 'NONE', #32181, #43574, #57283, .T. ) ;
#69047 = CARTESIAN_POINT ( 'NONE',  ( 15.50000000000000000, -15.50000000000000000, 22.50000000000000000 ) ) ;
#69048 = DIRECTION ( 'NONE',  ( -0.000000000000000000, 3.673940397442059868E-16, -1.000000000000000000 ) ) ;
#69049 = VECTOR ( 'NONE', #2929, 1000.000000000000000 ) ;
#69050 = DIRECTION ( 'NONE',  ( 1.836970198721029934E-16, 1.836970198721010706E-16, -1.000000000000000000 ) ) ;
#69051 = VERTEX_POINT ( 'NONE', #4271 ) ;
#69052 = ORIENTED_EDGE ( 'NONE', *, *, #65547, .T. ) ;
#69053 = ORIENTED_EDGE ( 'NONE', *, *, #46098, .F. ) ;
#69055 = DIRECTION ( 'NONE',  ( 0.000000000000000000, 0.000000000000000000, 1.000000000000000000 ) ) ;
#69054 = VECTOR ( 'NONE', #29765, 1000.000000000000000 ) ;
#69056 = ORIENTED_EDGE ( 'NONE', *, *, #62946, .T. ) ;
#69057 = ORIENTED_EDGE ( 'NONE', *, *, #62654, .F. ) ;
#69058 = LINE ( 'NONE', #46438, #19819 ) ;
#69059 = ORIENTED_EDGE ( 'NONE', *, *, #52975, .T. ) ;
#69060 = ORIENTED_EDGE ( 'NONE', *, *, #52163, .T. ) ;
#69061 = LINE ( 'NONE', #41837, #20389 ) ;
#69062 = EDGE_CURVE ( 'NONE', #23669, #59475, #9563, .T. ) ;
#69064 = VERTEX_POINT ( 'NONE', #43466 ) ;
#69063 = PLANE ( 'NONE',  #26654 ) ;
#69065 = ORIENTED_EDGE ( 'NONE', *, *, #25074, .T. ) ;
#69066 = CARTESIAN_POINT ( 'NONE',  ( 0.000000000000000000, 0.000000000000000000, -13.00000000000000178 ) ) ;
#69067 = CIRCLE ( 'NONE', #9263, 0.2500000000000002220 ) ;
#69068 = CARTESIAN_POINT ( 'NONE',  ( -5.993516549646776603, -6.006483450353426790, 455.0000000000000568 ) ) ;
#69069 = ADVANCED_FACE ( 'NONE', ( #65048 ), #54095, .F. ) ;
#69071 = EDGE_LOOP ( 'NONE', ( #33502, #22340, #4687, #38630 ) ) ;
#69070 = DIRECTION ( 'NONE',  ( 0.000000000000000000, 1.000000000000000000, 0.000000000000000000 ) ) ;
#69072 = ORIENTED_EDGE ( 'NONE', *, *, #7188, .T. ) ;
#69073 = DIRECTION ( 'NONE',  ( 0.000000000000000000, 0.000000000000000000, 1.000000000000000000 ) ) ;
#69074 = CARTESIAN_POINT ( 'NONE',  ( 10.31452373788278187, 3.842976262117144159, 54.00000000000000711 ) ) ;
#69075 = EDGE_CURVE ( 'NONE', #6765, #62987, #42429, .T. ) ;
#69076 = CARTESIAN_POINT ( 'NONE',  ( 83.77321854994620765, 47.95351654967443977, 25.00000000000000000 ) ) ;
#69077 = EDGE_CURVE ( 'NONE', #27404, #4441, #40316, .T. ) ;
#69078 = DIRECTION ( 'NONE',  ( 1.836970198721029934E-16, 1.836970198721010706E-16, -1.000000000000000000 ) ) ;
#69079 = CARTESIAN_POINT ( 'NONE',  ( -7.342976262117259623, 5.538810540049946773, 54.00000000000000711 ) ) ;
#69080 = VECTOR ( 'NONE', #740, 1000.000000000000000 ) ;
#69081 = ORIENTED_EDGE ( 'NONE', *, *, #34961, .T. ) ;
#69082 = CARTESIAN_POINT ( 'NONE',  ( -6.835476262117334834, -10.50702373788278798, 54.00000000000000711 ) ) ;
#69083 = EDGE_CURVE ( 'NONE', #28648, #43815, #25830, .T. ) ;
#69084 = ORIENTED_EDGE ( 'NONE', *, *, #26533, .F. ) ;
#69085 = FACE_OUTER_BOUND ( 'NONE', #51398, .T. ) ;
#69086 = VECTOR ( 'NONE', #61476, 1000.000000000000000 ) ;
#69087 = DIRECTION ( 'NONE',  ( 0.7071067811865486830, 0.7071067811865464625, 0.000000000000000000 ) ) ;
#69088 = EDGE_CURVE ( 'NONE', #34803, #49703, #343, .T. ) ;
#69089 = PLANE ( 'NONE',  #46023 ) ;
#69090 = EDGE_CURVE ( 'NONE', #4292, #61558, #5656, .T. ) ;
#69091 = CARTESIAN_POINT ( 'NONE',  ( 39.90000000000000568, 13.66939075806899240, 20.79999999999999361 ) ) ;
#69092 = LINE ( 'NONE', #36209, #50623 ) ;
#69093 = AXIS2_PLACEMENT_3D ( 'NONE', #8313, #29887, #24598 ) ;
#69094 = CLOSED_SHELL ( 'NONE', ( #31359, #11048, #36766, #18095, #8122, #56685, #43023, #21618, #18682, #49205, #26060, #53319, #53579, #21173, #66276, #53239, #44707, #69953, #59552, #34144, #26050 ) ) ;
#69095 = ORIENTED_EDGE ( 'NONE', *, *, #32749, .T. ) ;
#69096 = DIRECTION ( 'NONE',  ( 1.836970198721029934E-16, -1.836970198721036344E-16, 1.000000000000000000 ) ) ;
#69097 = EDGE_CURVE ( 'NONE', #22061, #46013, #47385, .T. ) ;
#69098 = DIRECTION ( 'NONE',  ( -0.000000000000000000, -0.000000000000000000, 1.000000000000000000 ) ) ;
#69099 = CIRCLE ( 'NONE', #67933, 1.000000000000000000 ) ;
#69100 = EDGE_CURVE ( 'NONE', #43188, #23628, #53058, .T. ) ;
#69101 = PLANE ( 'NONE',  #68849 ) ;
#69102 = ORIENTED_EDGE ( 'NONE', *, *, #3400, .F. ) ;
#69103 = DIRECTION ( 'NONE',  ( 0.000000000000000000, 0.000000000000000000, 1.000000000000000000 ) ) ;
#69104 = CARTESIAN_POINT ( 'NONE',  ( -7.250000000000000888, 8.250000000000001776, -10.50000000000000000 ) ) ;
#69105 = DIRECTION ( 'NONE',  ( -0.000000000000000000, 3.673940397442059868E-16, -1.000000000000000000 ) ) ;
#69106 = VECTOR ( 'NONE', #32919, 1000.000000000000000 ) ;
#69107 = LINE ( 'NONE', #58147, #42595 ) ;
#69108 = LINE ( 'NONE', #41881, #22927 ) ;
#69109 = ORIENTED_EDGE ( 'NONE', *, *, #30980, .F. ) ;
#69110 = DIRECTION ( 'NONE',  ( 0.000000000000000000, 0.000000000000000000, -1.000000000000000000 ) ) ;
#69111 = LINE ( 'NONE', #42585, #17003 ) ;
#69112 = EDGE_CURVE ( 'NONE', #7825, #50090, #32171, .T. ) ;
#69113 = CARTESIAN_POINT ( 'NONE',  ( 7.250000000000005329, 8.250000000000001776, -26.00000000000001066 ) ) ;
#69114 = DIRECTION ( 'NONE',  ( 0.000000000000000000, 0.000000000000000000, 1.000000000000000000 ) ) ;
#69115 = DIRECTION ( 'NONE',  ( -1.000000000000000000, 0.000000000000000000, 0.000000000000000000 ) ) ;
#69116 = VERTEX_POINT ( 'NONE', #52712 ) ;
#69118 = EDGE_LOOP ( 'NONE', ( #1094, #39040, #37673, #13822 ) ) ;
#69117 = DIRECTION ( 'NONE',  ( -1.000000000000000000, 0.000000000000000000, 0.000000000000000000 ) ) ;
#69119 = CARTESIAN_POINT ( 'NONE',  ( -6.858227778582867806, 2.989207322240119868, 54.00000000000000711 ) ) ;
#69120 = CARTESIAN_POINT ( 'NONE',  ( -25.50000000000000355, -5.200000000000001066, -24.50000000000000000 ) ) ;
#69121 = PLANE ( 'NONE',  #56767 ) ;
#69122 = VERTEX_POINT ( 'NONE', #53747 ) ;
#69123 = DIRECTION ( 'NONE',  ( 0.000000000000000000, 0.000000000000000000, -1.000000000000000000 ) ) ;
#69124 = DIRECTION ( 'NONE',  ( 0.000000000000000000, 0.000000000000000000, 1.000000000000000000 ) ) ;
#69125 = VECTOR ( 'NONE', #61410, 1000.000000000000000 ) ;
#69126 = ORIENTED_EDGE ( 'NONE', *, *, #33846, .T. ) ;
#69127 = ORIENTED_EDGE ( 'NONE', *, *, #64919, .F. ) ;
#69128 = EDGE_CURVE ( 'NONE', #49901, #30525, #5319, .T. ) ;
#69129 = ORIENTED_EDGE ( 'NONE', *, *, #32382, .T. ) ;
#69130 = AXIS2_PLACEMENT_3D ( 'NONE', #51236, #2794, #24374 ) ;
#69131 = DIRECTION ( 'NONE',  ( 1.000000000000000000, -3.903627567395476653E-15, 0.000000000000000000 ) ) ;
#69132 = EDGE_CURVE ( 'NONE', #53553, #61056, #60661, .T. ) ;
#69133 = CARTESIAN_POINT ( 'NONE',  ( 78.77321854994620765, 47.95351654967443977, 40.00000000000000000 ) ) ;
#69134 = CARTESIAN_POINT ( 'NONE',  ( 0.2500000000000105471, -42.24999999999999289, 26.74999999999999289 ) ) ;
#69135 = EDGE_LOOP ( 'NONE', ( #12324, #4779, #29016, #24596 ) ) ;
#69136 = ORIENTED_EDGE ( 'NONE', *, *, #8887, .F. ) ;
#69137 = EDGE_CURVE ( 'NONE', #5466, #13881, #29010, .T. ) ;
#69138 = DIRECTION ( 'NONE',  ( 0.000000000000000000, -1.000000000000000000, 0.000000000000000000 ) ) ;
#69139 = VERTEX_POINT ( 'NONE', #20862 ) ;
#69140 = ADVANCED_FACE ( 'NONE', ( #43118 ), #16250, .T. ) ;
#69141 = VERTEX_POINT ( 'NONE', #48784 ) ;
#69142 = VECTOR ( 'NONE', #50329, 1000.000000000000000 ) ;
#69143 = ORIENTED_EDGE ( 'NONE', *, *, #46134, .T. ) ;
#69144 = ORIENTED_EDGE ( 'NONE', *, *, #32827, .F. ) ;
#69145 = CARTESIAN_POINT ( 'NONE',  ( -15.50000000000000000, -1.037157890325000054, 22.50000000000000000 ) ) ;
#69146 = UNCERTAINTY_MEASURE_WITH_UNIT (LENGTH_MEASURE( 1.000000000000000082E-05 ), #23113, 'distance_accuracy_value', 'NONE');
#69147 = EDGE_CURVE ( 'NONE', #38091, #62476, #64021, .T. ) ;
#69149 = ORIENTED_EDGE ( 'NONE', *, *, #18686, .T. ) ;
#69148 = CARTESIAN_POINT ( 'NONE',  ( -10.49297626211732215, -9.795823737882733084, 26.00000000000000000 ) ) ;
#69150 = DIRECTION ( 'NONE',  ( 1.836970198721029934E-16, 1.836970198721010706E-16, -1.000000000000000000 ) ) ;
#69152 = DIRECTION ( 'NONE',  ( 0.000000000000000000, 0.000000000000000000, 1.000000000000000000 ) ) ;
#69151 = AXIS2_PLACEMENT_3D ( 'NONE', #50135, #23605, #23957 ) ;
#69153 = DIRECTION ( 'NONE',  ( -1.000000000000000000, 0.000000000000000000, 0.000000000000000000 ) ) ;
#69154 = ORIENTED_EDGE ( 'NONE', *, *, #39438, .F. ) ;
#69155 = EDGE_CURVE ( 'NONE', #57399, #44650, #1377, .T. ) ;
#69156 = ORIENTED_EDGE ( 'NONE', *, *, #27261, .T. ) ;
#69157 = ADVANCED_FACE ( 'NONE', ( #27553 ), #43821, .T. ) ;
#69158 = AXIS2_PLACEMENT_3D ( 'NONE', #34887, #34541, #35956 ) ;
#69159 = EDGE_CURVE ( 'NONE', #29848, #64676, #19989, .T. ) ;
#69160 = EDGE_CURVE ( 'NONE', #144, #41828, #44489, .T. ) ;
#69161 = CARTESIAN_POINT ( 'NONE',  ( 8.930623737882848800, 9.689726262117154931, 54.00000000000000711 ) ) ;
#69162 = LINE ( 'NONE', #37000, #6696 ) ;
#69163 = ORIENTED_EDGE ( 'NONE', *, *, #54319, .F. ) ;
#69164 = EDGE_CURVE ( 'NONE', #1040, #22191, #49812, .T. ) ;
#69165 = CARTESIAN_POINT ( 'NONE',  ( 10.50702373788277910, 3.650476262117147375, 26.00000000000000711 ) ) ;
#69166 = DIRECTION ( 'NONE',  ( 1.836970198721029934E-16, 1.836970198721010706E-16, -1.000000000000000000 ) ) ;
#69167 = PRESENTATION_STYLE_ASSIGNMENT (( #41945 ) ) ;
#69168 = ORIENTED_EDGE ( 'NONE', *, *, #59021, .T. ) ;
#69169 = CARTESIAN_POINT ( 'NONE',  ( -30.00000000000000000, -9.199999999999999289, -12.69999999999986073 ) ) ;
#69170 = LINE ( 'NONE', #37692, #35828 ) ;
#69171 = DIRECTION ( 'NONE',  ( 0.000000000000000000, 0.000000000000000000, 1.000000000000000000 ) ) ;
#69172 = DIRECTION ( 'NONE',  ( 0.000000000000000000, 0.5000000000000199840, 0.8660254037844271613 ) ) ;
#69173 = AXIS2_PLACEMENT_3D ( 'NONE', #22827, #6225, #11171 ) ;
#69174 = CARTESIAN_POINT ( 'NONE',  ( 176.4833316329832940, -10.00000000000000178, 278.4149360882130395 ) ) ;
#69175 = ORIENTED_EDGE ( 'NONE', *, *, #24696, .F. ) ;
#69176 = LINE ( 'NONE', #57510, #38113 ) ;
#69177 = DIRECTION ( 'NONE',  ( 0.7071067811865474617, 0.000000000000000000, -0.7071067811865474617 ) ) ;
#69178 = VECTOR ( 'NONE', #28798, 1000.000000000000000 ) ;
#69179 = EDGE_CURVE ( 'NONE', #4835, #65138, #28583, .T. ) ;
#69180 = DIRECTION ( 'NONE',  ( 0.000000000000000000, 1.000000000000000000, 0.000000000000000000 ) ) ;
#69181 = CARTESIAN_POINT ( 'NONE',  ( 8.406483450353359643, 7.603567055985454459, 195.0000000000000284 ) ) ;
#69182 = EDGE_CURVE ( 'NONE', #1141, #22560, #11285, .T. ) ;
#69183 = ORIENTED_EDGE ( 'NONE', *, *, #29444, .T. ) ;
#69184 = CARTESIAN_POINT ( 'NONE',  ( -11.07551654964667520, 10.19191654964664018, 455.0000000000000568 ) ) ;
#69185 = DIRECTION ( 'NONE',  ( -0.7671651518152963201, -0.6414496315691619044, 0.000000000000000000 ) ) ;
#69186 = VECTOR ( 'NONE', #30784, 1000.000000000000000 ) ;
#69187 = PLANE ( 'NONE',  #45913 ) ;
#69188 = CARTESIAN_POINT ( 'NONE',  ( 11.12648345035337982, 4.193516549646526315, 455.0000000000000568 ) ) ;
#69189 = ORIENTED_EDGE ( 'NONE', *, *, #14629, .F. ) ;
#69190 = DIRECTION ( 'NONE',  ( -0.000000000000000000, 3.673940397442059868E-16, -1.000000000000000000 ) ) ;
#69191 = DIRECTION ( 'NONE',  ( 0.000000000000000000, 0.000000000000000000, -1.000000000000000000 ) ) ;
#69192 = DIRECTION ( 'NONE',  ( 0.000000000000000000, 0.000000000000000000, 1.000000000000000000 ) ) ;
#69193 = DIRECTION ( 'NONE',  ( -1.000000000000000000, 0.000000000000000000, 0.000000000000000000 ) ) ;
#69194 = PLANE ( 'NONE',  #42147 ) ;
#69195 = CARTESIAN_POINT ( 'NONE',  ( -7.250000000000001776, -7.249999999999998224, -21.50000000000000000 ) ) ;
#69196 = VERTEX_POINT ( 'NONE', #22263 ) ;
#69197 = VECTOR ( 'NONE', #53567, 1000.000000000000000 ) ;
#69198 = ORIENTED_EDGE ( 'NONE', *, *, #62600, .F. ) ;
#69199 = CARTESIAN_POINT ( 'NONE',  ( 7.000000000000000000, -25.60000000000000142, 16.03137303340311348 ) ) ;
#69200 = CARTESIAN_POINT ( 'NONE',  ( 39.00000000000000000, -21.00000000000000000, 14.57806571531351914 ) ) ;
#69201 = ORIENTED_EDGE ( 'NONE', *, *, #47286, .F. ) ;
#69202 = FACE_OUTER_BOUND ( 'NONE', #7466, .T. ) ;
#69203 = VECTOR ( 'NONE', #50730, 1000.000000000000000 ) ;
#69204 = AXIS2_PLACEMENT_3D ( 'NONE', #57356, #57704, #30837 ) ;
#69205 = LINE ( 'NONE', #4517, #9280 ) ;
#69206 = ORIENTED_EDGE ( 'NONE', *, *, #29069, .F. ) ;
#69207 = CARTESIAN_POINT ( 'NONE',  ( 30.00000000000000000, -11.85423089348099879, 9.852125413066602277 ) ) ;
#69208 = ORIENTED_EDGE ( 'NONE', *, *, #69547, .T. ) ;
#69209 = CIRCLE ( 'NONE', #17263, 0.9999999999999991118 ) ;
#69210 = ORIENTED_EDGE ( 'NONE', *, *, #30353, .F. ) ;
#69211 = DIRECTION ( 'NONE',  ( -1.000000000000000000, 0.000000000000000000, 0.000000000000000000 ) ) ;
#69212 = ORIENTED_EDGE ( 'NONE', *, *, #21743, .T. ) ;
#69213 = EDGE_CURVE ( 'NONE', #33597, #10103, #39202, .T. ) ;
#69214 = LINE ( 'NONE', #9472, #66598 ) ;
#69215 = CARTESIAN_POINT ( 'NONE',  ( -30.00000000000000000, -11.85423089348099879, 9.852125413066602277 ) ) ;
#69216 = DIRECTION ( 'NONE',  ( 3.717264591378875951E-15, 1.000000000000000000, 0.000000000000000000 ) ) ;
#69217 = VERTEX_POINT ( 'NONE', #17629 ) ;
#69218 = ORIENTED_EDGE ( 'NONE', *, *, #3664, .F. ) ;
#69219 = EDGE_CURVE ( 'NONE', #7880, #9481, #22599, .T. ) ;
#69220 = DIRECTION ( 'NONE',  ( 1.000000000000000000, 0.000000000000000000, 0.000000000000000000 ) ) ;
#69222 = CARTESIAN_POINT ( 'NONE',  ( 0.5000000000000000000, -18.00000000000000355, -21.00000000000000000 ) ) ;
#69221 = CARTESIAN_POINT ( 'NONE',  ( 276.8775010008008053, -25.00000000000000000, -17.50000000000000000 ) ) ;
#69223 = ORIENTED_EDGE ( 'NONE', *, *, #63334, .F. ) ;
#69224 = ADVANCED_FACE ( 'NONE', ( #33882 ), #39534, .F. ) ;
#69225 = AXIS2_PLACEMENT_3D ( 'NONE', #20657, #35884, #42226 ) ;
#69226 = ORIENTED_EDGE ( 'NONE', *, *, #46389, .T. ) ;
#69227 = EDGE_CURVE ( 'NONE', #10176, #28585, #54779, .T. ) ;
#69229 = ORIENTED_EDGE ( 'NONE', *, *, #40090, .T. ) ;
#69228 = ITEM_DEFINED_TRANSFORMATION ( 'NONE', 'NONE', #51628,  #45918 ) ;
#69230 = EDGE_CURVE ( 'NONE', #40458, #67314, #12653, .T. ) ;
#69231 = EDGE_CURVE ( 'NONE', #60253, #6765, #49477, .T. ) ;
#69232 = LINE ( 'NONE', #69588, #43493 ) ;
#69233 = VECTOR ( 'NONE', #47661, 1000.000000000000000 ) ;
#69235 = VERTEX_POINT ( 'NONE', #17284 ) ;
#69234 = DIRECTION ( 'NONE',  ( -1.000000000000000000, 0.000000000000000000, 0.000000000000000000 ) ) ;
#69236 = LINE ( 'NONE', #9486, #18715 ) ;
#69237 = DIRECTION ( 'NONE',  ( -0.7671651518153038696, 0.6414496315691526895, -2.309356642089023690E-17 ) ) ;
#69238 = ORIENTED_EDGE ( 'NONE', *, *, #43616, .T. ) ;
#69239 = ORIENTED_EDGE ( 'NONE', *, *, #14556, .F. ) ;
#69240 = AXIS2_PLACEMENT_3D ( 'NONE', #54103, #65060, #48795 ) ;
#69241 = DIRECTION ( 'NONE',  ( 0.000000000000000000, 1.000000000000000000, -0.000000000000000000 ) ) ;
#69242 = EDGE_LOOP ( 'NONE', ( #68792, #29377, #18624, #64562 ) ) ;
#69243 = PLANE ( 'NONE',  #48295 ) ;
#69244 = CARTESIAN_POINT ( 'NONE',  ( 10.31452373788281562, -6.657023737882815873, 26.00000000000000000 ) ) ;
#69245 = DIRECTION ( 'NONE',  ( 1.000000000000000000, -1.047444401652940007E-14, 1.836970198721010706E-16 ) ) ;
#69246 = VERTEX_POINT ( 'NONE', #5993 ) ;
#69247 = CIRCLE ( 'NONE', #45499, 0.5999999999999998668 ) ;
#69248 =( NAMED_UNIT ( * ) PLANE_ANGLE_UNIT ( ) SI_UNIT ( $, .RADIAN. ) );
#69249 = CARTESIAN_POINT ( 'NONE',  ( 8.835729544836338434, -2.369523737882816672, 26.00000000000000711 ) ) ;
#69251 = ORIENTED_EDGE ( 'NONE', *, *, #46307, .F. ) ;
#69250 = CARTESIAN_POINT ( 'NONE',  ( 46.39999999999999858, 33.00000000000000000, -0.7500000000000000000 ) ) ;
#69253 = VERTEX_POINT ( 'NONE', #60410 ) ;
#69252 = CARTESIAN_POINT ( 'NONE',  ( 49.00000000000000000, -0.1999999999911795112, 8.826273045769999343E-12 ) ) ;
#69255 = PLANE ( 'NONE',  #47858 ) ;
#69254 = AXIS2_PLACEMENT_3D ( 'NONE', #24397, #40999, #34993 ) ;
#69256 = AXIS2_PLACEMENT_3D ( 'NONE', #43799, #1688, #6318 ) ;
#69258 = VECTOR ( 'NONE', #58093, 1000.000000000000000 ) ;
#69257 = LINE ( 'NONE', #26475, #4786 ) ;
#69259 = CARTESIAN_POINT ( 'NONE',  ( 28.90000000000000213, -0.2000000000089119934, -8.913009219568841313E-12 ) ) ;
#69260 = DIRECTION ( 'NONE',  ( 0.000000000000000000, -0.000000000000000000, 1.000000000000000000 ) ) ;
#69261 = VECTOR ( 'NONE', #27164, 1000.000000000000000 ) ;
#69262 = VECTOR ( 'NONE', #48657, 1000.000000000000000 ) ;
#69263 = CARTESIAN_POINT ( 'NONE',  ( -25.50000000000000355, -17.50000000000000000, -22.50000000000000000 ) ) ;
#69264 = ORIENTED_EDGE ( 'NONE', *, *, #30593, .T. ) ;
#69265 = FACE_OUTER_BOUND ( 'NONE', #22702, .T. ) ;
#69266 = DIRECTION ( 'NONE',  ( 1.836970198721029934E-16, 1.836970198721010706E-16, -1.000000000000000000 ) ) ;
#69268 = ORIENTED_EDGE ( 'NONE', *, *, #45257, .T. ) ;
#69267 = LINE ( 'NONE', #54059, #59353 ) ;
#69269 = EDGE_CURVE ( 'NONE', #59980, #62873, #7010, .T. ) ;
#69270 = CYLINDRICAL_SURFACE ( 'NONE', #59545, 0.5999999999999998668 ) ;
#69271 = DIRECTION ( 'NONE',  ( 0.6785983445458472207, 0.6785983445458458885, 0.2810846377148227826 ) ) ;
#69272 = EDGE_CURVE ( 'NONE', #15959, #46021, #62943, .T. ) ;
#69273 = CARTESIAN_POINT ( 'NONE',  ( -12.00000000000000000, 11.18999999999999950, 0.000000000000000000 ) ) ;
#69274 = CARTESIAN_POINT ( 'NONE',  ( -29.50000000000000355, -11.50000000000100009, 15.00000000000084910 ) ) ;
#69275 = ORIENTED_EDGE ( 'NONE', *, *, #59592, .F. ) ;
#69276 = CARTESIAN_POINT ( 'NONE',  ( 17.51999999999999957, -15.50000000000000000, -26.00000000000000355 ) ) ;
#69277 = CARTESIAN_POINT ( 'NONE',  ( 28.00000000000000000, -15.50000000000000000, -20.05051025721700242 ) ) ;
#69278 = ORIENTED_EDGE ( 'NONE', *, *, #67251, .F. ) ;
#69279 = CARTESIAN_POINT ( 'NONE',  ( 7.000000000000000000, -28.94999999999999929, -13.50000000000000000 ) ) ;
#69280 = CARTESIAN_POINT ( 'NONE',  ( -10.49297626211726175, 6.835476262117182955, 26.00000000000000711 ) ) ;
#69281 = CARTESIAN_POINT ( 'NONE',  ( 41.09999999999999432, 13.66939075806899950, -20.80000000000000426 ) ) ;
#69282 = FACE_OUTER_BOUND ( 'NONE', #13368, .T. ) ;
#69283 = PLANE ( 'NONE',  #30742 ) ;
#69284 = EDGE_LOOP ( 'NONE', ( #32439, #33901, #57031, #66300 ) ) ;
#69285 = ORIENTED_EDGE ( 'NONE', *, *, #40878, .F. ) ;
#69286 = DIRECTION ( 'NONE',  ( 0.000000000000000000, 0.000000000000000000, -1.000000000000000000 ) ) ;
#69287 = ORIENTED_EDGE ( 'NONE', *, *, #12480, .F. ) ;
#69288 = ORIENTED_EDGE ( 'NONE', *, *, #4289, .F. ) ;
#69289 = AXIS2_PLACEMENT_3D ( 'NONE', #39765, #34454, #18555 ) ;
#69290 = LINE ( 'NONE', #20846, #13352 ) ;
#69291 = PLANE ( 'NONE',  #50159 ) ;
#69292 = DIRECTION ( 'NONE',  ( -1.000000000000000000, 0.000000000000000000, 0.000000000000000000 ) ) ;
#69293 = ORIENTED_EDGE ( 'NONE', *, *, #52385, .F. ) ;
#69294 = ORIENTED_EDGE ( 'NONE', *, *, #56131, .F. ) ;
#69295 = DIRECTION ( 'NONE',  ( -0.000000000000000000, -0.000000000000000000, 1.000000000000000000 ) ) ;
#69296 = ORIENTED_EDGE ( 'NONE', *, *, #162, .F. ) ;
#69297 = VERTEX_POINT ( 'NONE', #55132 ) ;
#69298 = EDGE_CURVE ( 'NONE', #22012, #53008, #35829, .T. ) ;
#69299 = LINE ( 'NONE', #36790, #43989 ) ;
#69300 = DIRECTION ( 'NONE',  ( 0.5773502691896230665, 0.5773502691896271743, 0.5773502691896271743 ) ) ;
#69301 = VECTOR ( 'NONE', #29423, 1000.000000000000114 ) ;
#69302 = VECTOR ( 'NONE', #46158, 1000.000000000000000 ) ;
#69303 = FACE_OUTER_BOUND ( 'NONE', #41209, .T. ) ;
#69304 = ORIENTED_EDGE ( 'NONE', *, *, #23235, .F. ) ;
#69305 = CARTESIAN_POINT ( 'NONE',  ( -5.993516549646711766, 5.993516549646603409, 195.0000000000000284 ) ) ;
#69307 = CARTESIAN_POINT ( 'NONE',  ( 4.456444791733522252E-16, 7.450000000000002842, -23.50000000000000000 ) ) ;
#69306 = CARTESIAN_POINT ( 'NONE',  ( 15.50000000000129852, -15.50000000000000000, -22.50000000000000000 ) ) ;
#69308 = VECTOR ( 'NONE', #25643, 1000.000000000000000 ) ;
#69310 = ORIENTED_EDGE ( 'NONE', *, *, #5620, .T. ) ;
#69309 = AXIS2_PLACEMENT_3D ( 'NONE', #12187, #40094, #12869 ) ;
#69312 = VERTEX_POINT ( 'NONE', #2067 ) ;
#69311 = DIRECTION ( 'NONE',  ( 1.000000000000000000, -0.000000000000000000, -0.000000000000000000 ) ) ;
#69313 = ORIENTED_EDGE ( 'NONE', *, *, #47924, .T. ) ;
#69314 = VECTOR ( 'NONE', #57722, 1000.000000000000000 ) ;
#69315 = CIRCLE ( 'NONE', #59172, 0.2000000000000005107 ) ;
#69316 = EDGE_CURVE ( 'NONE', #17091, #39038, #698, .T. ) ;
#69317 = ADVANCED_FACE ( 'NONE', ( #66760 ), #13372, .F. ) ;
#69318 = LINE ( 'NONE', #16632, #14117 ) ;
#69319 = CARTESIAN_POINT ( 'NONE',  ( 4.456444791733522252E-16, 7.450000000000002842, -7.500000000000000000 ) ) ;
#69320 = EDGE_CURVE ( 'NONE', #56954, #11793, #40933, .T. ) ;
#69321 = ORIENTED_EDGE ( 'NONE', *, *, #30201, .T. ) ;
#69322 = PLANE ( 'NONE',  #5317 ) ;
#69323 = DIRECTION ( 'NONE',  ( -1.000000000000000000, 0.000000000000000000, 0.000000000000000000 ) ) ;
#69324 = VERTEX_POINT ( 'NONE', #30338 ) ;
#69325 = ORIENTED_EDGE ( 'NONE', *, *, #35712, .F. ) ;
#69326 = CARTESIAN_POINT ( 'NONE',  ( -9.390476262117196882, -0.9555237378827262651, 26.00000000000000711 ) ) ;
#69327 = LINE ( 'NONE', #30542, #782 ) ;
#69328 = LINE ( 'NONE', #53779, #63280 ) ;
#69329 = ORIENTED_EDGE ( 'NONE', *, *, #2176, .T. ) ;
#69330 = DIRECTION ( 'NONE',  ( 0.000000000000000000, -0.000000000000000000, 1.000000000000000000 ) ) ;
#69331 = DIRECTION ( 'NONE',  ( 1.000000000000000000, -0.000000000000000000, -0.000000000000000000 ) ) ;
#69332 = VECTOR ( 'NONE', #54246, 1000.000000000000000 ) ;
#69334 = ORIENTED_EDGE ( 'NONE', *, *, #9308, .T. ) ;
#69333 = DIRECTION ( 'NONE',  ( 0.6414496315691617934, -0.7671651518152962090, -2.818519042763987834E-16 ) ) ;
#69336 = ORIENTED_EDGE ( 'NONE', *, *, #30821, .T. ) ;
#69335 = DIRECTION ( 'NONE',  ( 0.000000000000000000, 0.000000000000000000, 1.000000000000000000 ) ) ;
#69337 = CARTESIAN_POINT ( 'NONE',  ( 12.00648345035338060, -4.186483450353396307, 195.0000000000000284 ) ) ;
#69338 = PLANE ( 'NONE',  #32939 ) ;
#69339 = AXIS2_PLACEMENT_3D ( 'NONE', #57620, #68590, #20141 ) ;
#69340 = FACE_OUTER_BOUND ( 'NONE', #64166, .T. ) ;
#69341 = CARTESIAN_POINT ( 'NONE',  ( -7.259684009079916400, -4.201500623655988420, 195.0000000000000284 ) ) ;
#69342 = FACE_OUTER_BOUND ( 'NONE', #9720, .T. ) ;
#69343 = DIRECTION ( 'NONE',  ( 0.000000000000000000, -0.7278708115916149302, -0.6857142857145122061 ) ) ;
#69344 = ORIENTED_EDGE ( 'NONE', *, *, #38967, .F. ) ;
#69345 = CARTESIAN_POINT ( 'NONE',  ( 39.00000000000000000, 0.000000000000000000, 2.458500000000000796 ) ) ;
#69347 = ORIENTED_EDGE ( 'NONE', *, *, #46175, .F. ) ;
#69346 = CARTESIAN_POINT ( 'NONE',  ( 12.00648345035333620, 4.173516549646563156, 195.0000000000000284 ) ) ;
#69348 = FACE_OUTER_BOUND ( 'NONE', #21545, .T. ) ;
#69349 = VECTOR ( 'NONE', #51252, 1000.000000000000000 ) ;
#69350 = CIRCLE ( 'NONE', #8348, 0.5000000000001392220 ) ;
#69351 = LINE ( 'NONE', #20563, #24509 ) ;
#69352 = EDGE_CURVE ( 'NONE', #1336, #62698, #67109, .T. ) ;
#69353 = CARTESIAN_POINT ( 'NONE',  ( 34.89999999999999858, 3.010794155703768650E-16, -2.458500000000000796 ) ) ;
#69354 = EDGE_CURVE ( 'NONE', #50308, #3316, #56501, .T. ) ;
#69355 = ADVANCED_FACE ( 'NONE', ( #18666 ), #35264, .F. ) ;
#69356 = VECTOR ( 'NONE', #55137, 1000.000000000000000 ) ;
#69357 = VECTOR ( 'NONE', #8920, 1000.000000000000000 ) ;
#69358 = AXIS2_PLACEMENT_3D ( 'NONE', #29846, #63791, #19592 ) ;
#69359 = ORIENTED_EDGE ( 'NONE', *, *, #31436, .F. ) ;
#69360 = CARTESIAN_POINT ( 'NONE',  ( -11.75000000000000000, -5.000000000000000000, -23.89194109070750116 ) ) ;
#69361 = DIRECTION ( 'NONE',  ( 0.000000000000000000, 0.000000000000000000, 1.000000000000000000 ) ) ;
#69363 = ORIENTED_EDGE ( 'NONE', *, *, #59440, .F. ) ;
#69362 = EDGE_CURVE ( 'NONE', #27929, #51881, #8399, .T. ) ;
#69364 = DIRECTION ( 'NONE',  ( 1.836970198721029934E-16, 1.836970198721010706E-16, -1.000000000000000000 ) ) ;
#69365 = VECTOR ( 'NONE', #25831, 1000.000000000000000 ) ;
#69366 = DIRECTION ( 'NONE',  ( -1.000000000000000000, 0.000000000000000000, 0.000000000000000000 ) ) ;
#69367 = LINE ( 'NONE', #20921, #37722 ) ;
#69368 = ORIENTED_EDGE ( 'NONE', *, *, #41589, .F. ) ;
#69369 = DIRECTION ( 'NONE',  ( 0.000000000000000000, 1.000000000000000000, 0.000000000000000000 ) ) ;
#69370 = VERTEX_POINT ( 'NONE', #35624 ) ;
#69371 = EDGE_LOOP ( 'NONE', ( #16756, #28782, #69421, #610 ) ) ;
#69372 = AXIS2_PLACEMENT_3D ( 'NONE', #56594, #67567, #13459 ) ;
#69373 = CARTESIAN_POINT ( 'NONE',  ( 29.89999999999999858, -0.2000000000089119934, -8.913009219568841313E-12 ) ) ;
#69374 = LINE ( 'NONE', #21978, #11662 ) ;
#69375 = CARTESIAN_POINT ( 'NONE',  ( -8.249999999999996447, -7.848062532927998269, -5.000000000000000000 ) ) ;
#69376 = DIRECTION ( 'NONE',  ( 2.478176394252584099E-15, 1.000000000000000000, 0.000000000000000000 ) ) ;
#69377 = VERTEX_POINT ( 'NONE', #68162 ) ;
#69378 = ORIENTED_EDGE ( 'NONE', *, *, #43401, .T. ) ;
#69380 = VERTEX_POINT ( 'NONE', #46942 ) ;
#69379 = FACE_OUTER_BOUND ( 'NONE', #30189, .T. ) ;
#69381 = VERTEX_POINT ( 'NONE', #29266 ) ;
#69382 = DIRECTION ( 'NONE',  ( 0.000000000000000000, 3.989863994748342081E-13, 1.000000000000000000 ) ) ;
#69383 = CARTESIAN_POINT ( 'NONE',  ( -7.250000000000000000, -7.449999999999998401, -24.50000000000000000 ) ) ;
#69384 = DIRECTION ( 'NONE',  ( 0.000000000000000000, 0.000000000000000000, -1.000000000000000000 ) ) ;
#69385 = AXIS2_PLACEMENT_3D ( 'NONE', #51987, #62947, #2485 ) ;
#69386 = CARTESIAN_POINT ( 'NONE',  ( 9.703773737882812611, 10.03972626211715813, 26.00000000000000711 ) ) ;
#69388 = FACE_OUTER_BOUND ( 'NONE', #9257, .T. ) ;
#69387 = DIRECTION ( 'NONE',  ( -0.000000000000000000, 1.000000000000000000, -0.000000000000000000 ) ) ;
#69389 = VERTEX_POINT ( 'NONE', #29622 ) ;
#69390 = ORIENTED_EDGE ( 'NONE', *, *, #33995, .T. ) ;
#69391 = AXIS2_PLACEMENT_3D ( 'NONE', #52841, #47851, #25958 ) ;
#69392 = VERTEX_POINT ( 'NONE', #41284 ) ;
#69393 = ORIENTED_EDGE ( 'NONE', *, *, #9616, .T. ) ;
#69394 = PLANE ( 'NONE',  #31114 ) ;
#69395 = PLANE ( 'NONE',  #58092 ) ;
#69396 = EDGE_CURVE ( 'NONE', #58380, #15894, #51197, .T. ) ;
#69397 = DIRECTION ( 'NONE',  ( 1.000000000000000000, 0.000000000000000000, 0.000000000000000000 ) ) ;
#69398 = VECTOR ( 'NONE', #55365, 1000.000000000000000 ) ;
#69400 = CARTESIAN_POINT ( 'NONE',  ( 8.465062094116069247, -7.757955312929539105, 195.0000000000000284 ) ) ;
#69399 = VECTOR ( 'NONE', #3651, 1000.000000000000000 ) ;
#69401 = EDGE_CURVE ( 'NONE', #56758, #3816, #13716, .T. ) ;
#69402 = VERTEX_POINT ( 'NONE', #2411 ) ;
#69403 = ORIENTED_EDGE ( 'NONE', *, *, #57575, .T. ) ;
#69404 = EDGE_CURVE ( 'NONE', #21068, #28, #50840, .T. ) ;
#69405 = ORIENTED_EDGE ( 'NONE', *, *, #12868, .F. ) ;
#69406 = DIRECTION ( 'NONE',  ( 1.000000000000000000, 0.000000000000000000, 0.000000000000000000 ) ) ;
#69407 = ORIENTED_EDGE ( 'NONE', *, *, #64313, .F. ) ;
#69408 = AXIS2_PLACEMENT_3D ( 'NONE', #22274, #5999, #39209 ) ;
#69409 = AXIS2_PLACEMENT_3D ( 'NONE', #8480, #7781, #18385 ) ;
#69410 = AXIS2_PLACEMENT_3D ( 'NONE', #30639, #58211, #42644 ) ;
#69411 = EDGE_CURVE ( 'NONE', #56437, #34317, #57205, .T. ) ;
#69412 = CARTESIAN_POINT ( 'NONE',  ( -7.250000000000000888, 7.450000000000003730, -24.50000000000000000 ) ) ;
#69413 = ORIENTED_EDGE ( 'NONE', *, *, #16537, .T. ) ;
#69414 = ORIENTED_EDGE ( 'NONE', *, *, #40892, .F. ) ;
#69415 = DIRECTION ( 'NONE',  ( -0.5000000000000019984, -0.8660254037844375974, -0.000000000000000000 ) ) ;
#69416 = CIRCLE ( 'NONE', #16366, 0.3500000000002722600 ) ;
#69417 = EDGE_CURVE ( 'NONE', #43147, #55829, #34578, .T. ) ;
#69419 = ORIENTED_EDGE ( 'NONE', *, *, #32159, .T. ) ;
#69418 = CARTESIAN_POINT ( 'NONE',  ( -13.00000000000000178, -17.50000000000000000, 20.05051025721700242 ) ) ;
#69421 = ORIENTED_EDGE ( 'NONE', *, *, #1229, .F. ) ;
#69420 = ADVANCED_FACE ( 'NONE', ( #45533 ), #61437, .T. ) ;
#69422 = AXIS2_PLACEMENT_3D ( 'NONE', #20819, #58664, #10219 ) ;
#69423 = LINE ( 'NONE', #36539, #32978 ) ;
#69424 = CARTESIAN_POINT ( 'NONE',  ( -7.250000000000001776, -7.249999999999998224, -25.00000000000000000 ) ) ;
#69426 = VERTEX_POINT ( 'NONE', #34920 ) ;
#69425 = CARTESIAN_POINT ( 'NONE',  ( -25.50000000000000355, 0.000000000000000000, 20.24999999999999645 ) ) ;
#69427 = VECTOR ( 'NONE', #55479, 1000.000000000000000 ) ;
#69428 = VERTEX_POINT ( 'NONE', #24686 ) ;
#69429 = CARTESIAN_POINT ( 'NONE',  ( 11.75000000000000000, -5.200000000000001066, 11.75000000000000000 ) ) ;
#69430 = DIRECTION ( 'NONE',  ( 1.836970198721029934E-16, 1.836970198721010706E-16, -1.000000000000000000 ) ) ;
#69431 = CARTESIAN_POINT ( 'NONE',  ( 30.00000000000000000, -17.50000000000000000, 26.64999999999999858 ) ) ;
#69432 = CARTESIAN_POINT ( 'NONE',  ( 9.912023737882815766, -3.682023737882826886, 54.00000000000000711 ) ) ;
#69433 = CARTESIAN_POINT ( 'NONE',  ( -30.00000000000000000, -15.46862696659690073, 14.50000000000000000 ) ) ;
#69434 = EDGE_LOOP ( 'NONE', ( #17860, #60420, #29257, #6786 ) ) ;
#69435 = FACE_BOUND ( 'NONE', #29843, .T. ) ;
#69436 = ORIENTED_EDGE ( 'NONE', *, *, #23183, .F. ) ;
#69437 = LINE ( 'NONE', #26657, #34343 ) ;
#69438 = CIRCLE ( 'NONE', #20878, 3.500000000000000000 ) ;
#69439 = PLANE ( 'NONE',  #21217 ) ;
#69440 = CARTESIAN_POINT ( 'NONE',  ( 275.5000000000000000, -0.5000000000000000000, 27.00000000000000000 ) ) ;
#69441 = DIRECTION ( 'NONE',  ( 0.000000000000000000, 0.000000000000000000, -1.000000000000000000 ) ) ;
#69442 = AXIS2_PLACEMENT_3D ( 'NONE', #14324, #68766, #35887 ) ;
#69443 = VERTEX_POINT ( 'NONE', #45892 ) ;
#69444 = DIRECTION ( 'NONE',  ( -1.000000000000000000, 0.000000000000000000, 0.000000000000000000 ) ) ;
#69445 = CARTESIAN_POINT ( 'NONE',  ( 4.186483450353423841, 11.99351654964658742, 455.0000000000000568 ) ) ;
#69446 = CIRCLE ( 'NONE', #41218, 3.499999999999999556 ) ;
#69447 = VECTOR ( 'NONE', #19722, 1000.000000000000000 ) ;
#69448 = LINE ( 'NONE', #57087, #66561 ) ;
#69449 = ORIENTED_EDGE ( 'NONE', *, *, #59040, .F. ) ;
#69450 = CARTESIAN_POINT ( 'NONE',  ( 15.00000000000000000, -26.28355339059299922, -9.766446609406699508 ) ) ;
#69451 = CARTESIAN_POINT ( 'NONE',  ( 10.50702373788281996, -6.849523737882823760, 54.00000000000000711 ) ) ;
#69452 = DIRECTION ( 'NONE',  ( 1.000000000000000000, -6.508391731846281342E-15, -1.836970198721041767E-16 ) ) ;
#69453 = CYLINDRICAL_SURFACE ( 'NONE', #38120, 0.7499999999999997780 ) ;
#69454 = LINE ( 'NONE', #36224, #20661 ) ;
#69455 = AXIS2_PLACEMENT_3D ( 'NONE', #45190, #67488, #25045 ) ;
#69456 = AXIS2_PLACEMENT_3D ( 'NONE', #43294, #69123, #21384 ) ;
#69458 = ORIENTED_EDGE ( 'NONE', *, *, #7813, .T. ) ;
#69457 = ADVANCED_FACE ( 'NONE', ( #30693 ), #35988, .T. ) ;
#69459 = CARTESIAN_POINT ( 'NONE',  ( 105.8309041053263257, 63.65740854044500452, 10.00000000000000000 ) ) ;
#69460 = DIRECTION ( 'NONE',  ( -7.751221965937476285E-17, -1.000000000000000000, 0.000000000000000000 ) ) ;
#69461 = CARTESIAN_POINT ( 'NONE',  ( 7.408280051175162306, 6.775514141871318508, 54.00000000000000711 ) ) ;
#69462 = CIRCLE ( 'NONE', #38965, 0.5000000000001386669 ) ;
#69463 = EDGE_CURVE ( 'NONE', #24415, #354, #51909, .T. ) ;
#69464 = PLANE ( 'NONE',  #64513 ) ;
#69465 = ORIENTED_EDGE ( 'NONE', *, *, #13728, .T. ) ;
#69467 = ORIENTED_EDGE ( 'NONE', *, *, #23263, .T. ) ;
#69466 = CARTESIAN_POINT ( 'NONE',  ( 15.89999999999999680, 20.60000000000000142, -13.86939075806900057 ) ) ;
#69468 = COLOUR_RGB ( '', 0.09019608, 0.27058824, 0.51372549) ;
#69469 = CARTESIAN_POINT ( 'NONE',  ( 29.50000000000000355, -11.70000000000012008, -10.70000000000011831 ) ) ;
#69470 = DIRECTION ( 'NONE',  ( -1.000000000000000000, 0.000000000000000000, 0.000000000000000000 ) ) ;
#69471 = CARTESIAN_POINT ( 'NONE',  ( 7.250000000000005329, -7.449999999999998401, -10.50000000000000000 ) ) ;
#69473 = ORIENTED_EDGE ( 'NONE', *, *, #62909, .T. ) ;
#69472 = EDGE_CURVE ( 'NONE', #35639, #39379, #31367, .T. ) ;
#69474 = DIRECTION ( 'NONE',  ( 1.000000000000000000, 0.000000000000000000, 0.000000000000000000 ) ) ;
#69475 = CARTESIAN_POINT ( 'NONE',  ( 10.05377373788281581, 9.689726262117151379, 54.00000000000000711 ) ) ;
#69476 = ORIENTED_EDGE ( 'NONE', *, *, #16190, .F. ) ;
#69477 = ORIENTED_EDGE ( 'NONE', *, *, #44624, .F. ) ;
#69478 = ADVANCED_FACE ( 'NONE', ( #9121 ), #52617, .T. ) ;
#69479 = ORIENTED_EDGE ( 'NONE', *, *, #35385, .F. ) ;
#69480 = FACE_OUTER_BOUND ( 'NONE', #33038, .T. ) ;
#69481 = DIRECTION ( 'NONE',  ( -1.000000000000000000, 0.000000000000000000, 0.000000000000000000 ) ) ;
#69482 = DIRECTION ( 'NONE',  ( 0.000000000000000000, -0.000000000000000000, 1.000000000000000000 ) ) ;
#69483 = EDGE_CURVE ( 'NONE', #8538, #1200, #53318, .T. ) ;
#69484 = ORIENTED_EDGE ( 'NONE', *, *, #58778, .T. ) ;
#69485 = ORIENTED_EDGE ( 'NONE', *, *, #48259, .F. ) ;
#69486 = DIRECTION ( 'NONE',  ( 0.000000000000000000, 0.000000000000000000, 1.000000000000000000 ) ) ;
#69487 = ORIENTED_EDGE ( 'NONE', *, *, #24896, .T. ) ;
#69488 = AXIS2_PLACEMENT_3D ( 'NONE', #37381, #9820, #68151 ) ;
#69489 = ORIENTED_EDGE ( 'NONE', *, *, #25621, .F. ) ;
#69490 = ORIENTED_EDGE ( 'NONE', *, *, #2236, .F. ) ;
#69491 = EDGE_LOOP ( 'NONE', ( #42798, #65135, #39868, #25356 ) ) ;
#69492 = AXIS2_PLACEMENT_3D ( 'NONE', #56569, #18735, #40301 ) ;
#69493 = DIRECTION ( 'NONE',  ( 0.000000000000000000, -3.673940397442059868E-16, 1.000000000000000000 ) ) ;
#69494 = EDGE_CURVE ( 'NONE', #55788, #13160, #59613, .T. ) ;
#69496 = EDGE_LOOP ( 'NONE', ( #128, #68659, #25132, #27233 ) ) ;
#69495 = CYLINDRICAL_SURFACE ( 'NONE', #6251, 0.3499999999999302558 ) ;
#69497 = EDGE_CURVE ( 'NONE', #21753, #39731, #10512, .T. ) ;
#69498 = DIRECTION ( 'NONE',  ( 1.000000000000000000, -0.000000000000000000, -0.000000000000000000 ) ) ;
#69499 = AXIS2_PLACEMENT_3D ( 'NONE', #28099, #58896, #59590 ) ;
#69500 = VECTOR ( 'NONE', #60727, 1000.000000000000000 ) ;
#69501 = CIRCLE ( 'NONE', #50303, 0.8100000000000017186 ) ;
#69502 = LINE ( 'NONE', #31686, #55489 ) ;
#69503 = CARTESIAN_POINT ( 'NONE',  ( 8.250000000000005329, 0.000000000000000000, -10.00000000000000000 ) ) ;
#69504 = EDGE_LOOP ( 'NONE', ( #43524, #34362, #69906, #62488 ) ) ;
#69505 = ORIENTED_EDGE ( 'NONE', *, *, #19813, .T. ) ;
#69506 = VECTOR ( 'NONE', #19019, 1000.000000000000000 ) ;
#69507 = COLOUR_RGB ( '', 0.66274510, 0.83137255, 0.94901961) ;
#69508 = EDGE_CURVE ( 'NONE', #50527, #17133, #25747, .T. ) ;
#69509 = DIRECTION ( 'NONE',  ( -0.000000000000000000, -0.000000000000000000, -1.000000000000000000 ) ) ;
#69510 = CIRCLE ( 'NONE', #61606, 24.99999999998789946 ) ;
#69511 = FACE_OUTER_BOUND ( 'NONE', #3661, .T. ) ;
#69512 = ORIENTED_EDGE ( 'NONE', *, *, #40723, .T. ) ;
#69513 = VECTOR ( 'NONE', #11094, 1000.000000000000000 ) ;
#69514 = SURFACE_STYLE_USAGE ( .BOTH. , #4126 ) ;
#69515 = DIRECTION ( 'NONE',  ( 1.000000000000000000, 0.000000000000000000, 0.000000000000000000 ) ) ;
#69516 = LINE ( 'NONE', #4477, #27680 ) ;
#69517 = ORIENTED_EDGE ( 'NONE', *, *, #34497, .F. ) ;
#69518 = AXIS2_PLACEMENT_3D ( 'NONE', #47779, #25527, #47089 ) ;
#69519 = DIRECTION ( 'NONE',  ( 0.000000000000000000, -0.7071067811865076047, 0.7071067811865875408 ) ) ;
#69520 = CARTESIAN_POINT ( 'NONE',  ( -9.690000000000001279, 9.690000000000001279, -5.000000000000000000 ) ) ;
#69521 = LINE ( 'NONE', #4824, #1431 ) ;
#69522 = DIRECTION ( 'NONE',  ( -0.000000000000000000, -0.000000000000000000, -1.000000000000000000 ) ) ;
#69523 = ADVANCED_FACE ( 'NONE', ( #20771 ), #9911, .F. ) ;
#69524 = CYLINDRICAL_SURFACE ( 'NONE', #29725, 1.224999999999998757 ) ;
#69525 = ORIENTED_EDGE ( 'NONE', *, *, #61880, .T. ) ;
#69526 = DIRECTION ( 'NONE',  ( 0.000000000000000000, 1.000000000000000000, 3.673940397442059868E-16 ) ) ;
#69527 = CARTESIAN_POINT ( 'NONE',  ( -8.452095193409402185, 7.744988412222746810, 455.0000000000000568 ) ) ;
#69528 = CARTESIAN_POINT ( 'NONE',  ( -11.47551654964667733, 11.07551654964660237, 195.0000000000000284 ) ) ;
#69529 = EDGE_CURVE ( 'NONE', #27000, #61399, #21472, .T. ) ;
#69530 = LINE ( 'NONE', #41958, #52598 ) ;
#69531 = EDGE_LOOP ( 'NONE', ( #62604, #38518, #6591, #42628 ) ) ;
#69532 = DIRECTION ( 'NONE',  ( 0.000000000000000000, 0.000000000000000000, 1.000000000000000000 ) ) ;
#69533 = VECTOR ( 'NONE', #10810, 1000.000000000000000 ) ;
#69534 = FACE_BOUND ( 'NONE', #48611, .T. ) ;
#69535 = EDGE_CURVE ( 'NONE', #41857, #26334, #4260, .T. ) ;
#69536 = LINE ( 'NONE', #21100, #50452 ) ;
#69537 = CARTESIAN_POINT ( 'NONE',  ( 6.832023737882815695, 9.722976262117192903, 54.00000000000000711 ) ) ;
#69538 = ORIENTED_EDGE ( 'NONE', *, *, #3253, .F. ) ;
#69539 = CARTESIAN_POINT ( 'NONE',  ( -5.242976262117259978, 5.242976262117182706, 54.00000000000000711 ) ) ;
#69540 = EDGE_CURVE ( 'NONE', #36372, #34655, #68869, .T. ) ;
#69541 = CARTESIAN_POINT ( 'NONE',  ( 176.4833316329832940, 9.000000000000001776, 324.6739988703752715 ) ) ;
#69542 = VECTOR ( 'NONE', #3106, 1000.000000000000000 ) ;
#69543 = LINE ( 'NONE', #47277, #32243 ) ;
#69544 = DIRECTION ( 'NONE',  ( 0.000000000000000000, -1.000000000000000000, 0.000000000000000000 ) ) ;
#69545 = AXIS2_PLACEMENT_3D ( 'NONE', #64938, #37035, #21108 ) ;
#69546 = CARTESIAN_POINT ( 'NONE',  ( 7.450000000000004619, -1.336933437520057563E-15, -15.00000000000000000 ) ) ;
#69547 = EDGE_CURVE ( 'NONE', #2059, #25912, #15131, .T. ) ;
#69548 = LINE ( 'NONE', #4160, #65 ) ;
#69549 = ORIENTED_EDGE ( 'NONE', *, *, #28184, .F. ) ;
#69550 = VECTOR ( 'NONE', #10713, 1000.000000000000114 ) ;
#69551 = AXIS2_PLACEMENT_3D ( 'NONE', #40548, #30650, #40195 ) ;
#69552 = AXIS2_PLACEMENT_3D ( 'NONE', #33319, #22706, #44258 ) ;
#69553 = VERTEX_POINT ( 'NONE', #31747 ) ;
#69554 = DIRECTION ( 'NONE',  ( 1.836970198721029934E-16, 1.836970198721010706E-16, -1.000000000000000000 ) ) ;
#69555 = LINE ( 'NONE', #31021, #26590 ) ;
#69557 = ORIENTED_EDGE ( 'NONE', *, *, #31379, .T. ) ;
#69556 = ADVANCED_FACE ( 'NONE', ( #10167 ), #36337, .F. ) ;
#69558 = CARTESIAN_POINT ( 'NONE',  ( 29.89999999999999858, 3.010794155703768650E-16, -2.458500000000000796 ) ) ;
#69559 = EDGE_CURVE ( 'NONE', #21746, #23316, #39255, .T. ) ;
#69560 = AXIS2_PLACEMENT_3D ( 'NONE', #36629, #26729, #9413 ) ;
#69561 = VECTOR ( 'NONE', #53312, 1000.000000000000000 ) ;
#69562 = STYLED_ITEM ( 'NONE', ( #59824 ), #67800 ) ;
#69563 = DIRECTION ( 'NONE',  ( 0.000000000000000000, 1.000000000000000000, 0.000000000000000000 ) ) ;
#69564 = EDGE_CURVE ( 'NONE', #24845, #22621, #32086, .T. ) ;
#69565 = ORIENTED_EDGE ( 'NONE', *, *, #2112, .F. ) ;
#69566 = EDGE_CURVE ( 'NONE', #15881, #12520, #59300, .T. ) ;
#69567 = EDGE_CURVE ( 'NONE', #20448, #61277, #47999, .T. ) ;
#69568 = AXIS2_PLACEMENT_3D ( 'NONE', #910, #16807, #65587 ) ;
#69569 = LINE ( 'NONE', #46579, #8511 ) ;
#69570 = VERTEX_POINT ( 'NONE', #14776 ) ;
#69571 = EDGE_LOOP ( 'NONE', ( #6183, #41183, #20990, #56591 ) ) ;
#69572 = CARTESIAN_POINT ( 'NONE',  ( 12.00648345035338060, -7.826483450353491023, 455.0000000000000568 ) ) ;
#69573 = ORIENTED_EDGE ( 'NONE', *, *, #12826, .F. ) ;
#69574 = DIRECTION ( 'NONE',  ( -1.000000000000000000, 0.000000000000000000, 0.000000000000000000 ) ) ;
#69575 = EDGE_CURVE ( 'NONE', #3182, #67414, #31036, .T. ) ;
#69576 = PLANE ( 'NONE',  #4538 ) ;
#69577 = DIRECTION ( 'NONE',  ( -1.000000000000000000, 0.000000000000000000, 0.000000000000000000 ) ) ;
#69578 = DIRECTION ( 'NONE',  ( 0.000000000000000000, 0.000000000000000000, -1.000000000000000000 ) ) ;
#69579 = VERTEX_POINT ( 'NONE', #47647 ) ;
#69580 = ORIENTED_EDGE ( 'NONE', *, *, #48835, .F. ) ;
#69581 = MECHANICAL_DESIGN_GEOMETRIC_PRESENTATION_REPRESENTATION (  '', ( #29882 ), #63926 ) ;
#69582 = DIRECTION ( 'NONE',  ( 0.000000000000000000, 0.000000000000000000, -1.000000000000000000 ) ) ;
#69584 = LINE ( 'NONE', #15493, #61549 ) ;
#69583 = DIRECTION ( 'NONE',  ( -1.000000000000000000, 0.000000000000000000, 0.000000000000000000 ) ) ;
#69585 = ORIENTED_EDGE ( 'NONE', *, *, #46867, .F. ) ;
#69586 = ORIENTED_EDGE ( 'NONE', *, *, #61914, .T. ) ;
#69587 = ORIENTED_EDGE ( 'NONE', *, *, #56988, .T. ) ;
#69588 = CARTESIAN_POINT ( 'NONE',  ( 7.250000000000005329, -8.249999999999998224, -26.00000000000001066 ) ) ;
#69589 = EDGE_CURVE ( 'NONE', #1690, #46397, #26791, .T. ) ;
#69591 = EDGE_LOOP ( 'NONE', ( #19219, #35560, #37909, #62003 ) ) ;
#69590 = CARTESIAN_POINT ( 'NONE',  ( 30.00000000000000000, -16.28999999999999915, 14.50000000000000000 ) ) ;
#69592 = EDGE_CURVE ( 'NONE', #33832, #35182, #27129, .T. ) ;
#69593 = CARTESIAN_POINT ( 'NONE',  ( 6.006483450353353959, 5.993516549646629166, 195.0000000000000284 ) ) ;
#69594 = DIRECTION ( 'NONE',  ( 0.000000000000000000, 1.000000000000000000, 0.000000000000000000 ) ) ;
#69595 = EDGE_LOOP ( 'NONE', ( #68636, #68951, #68464, #45606 ) ) ;
#69596 = AXIS2_PLACEMENT_3D ( 'NONE', #5791, #16748, #27005 ) ;
#69597 = ORIENTED_EDGE ( 'NONE', *, *, #28044, .T. ) ;
#69598 = CARTESIAN_POINT ( 'NONE',  ( 47.00000000000000000, -0.7500000000000000000, -4.943429983321300014 ) ) ;
#69599 = CIRCLE ( 'NONE', #35647, 24.99999999998789946 ) ;
#69600 = ORIENTED_EDGE ( 'NONE', *, *, #26374, .F. ) ;
#69601 = DIRECTION ( 'NONE',  ( 0.000000000000000000, -0.000000000000000000, 1.000000000000000000 ) ) ;
#69602 = LINE ( 'NONE', #26121, #10967 ) ;
#69603 = AXIS2_PLACEMENT_3D ( 'NONE', #9723, #31304, #36953 ) ;
#69604 = DIRECTION ( 'NONE',  ( 0.4285714285711672566, 0.000000000000000000, 0.9035079029053751931 ) ) ;
#69605 = ORIENTED_EDGE ( 'NONE', *, *, #26313, .F. ) ;
#69606 = VECTOR ( 'NONE', #49590, 1000.000000000000000 ) ;
#69607 = AXIS2_PLACEMENT_3D ( 'NONE', #44551, #49533, #13070 ) ;
#69608 = AXIS2_PLACEMENT_3D ( 'NONE', #2088, #38874, #56186 ) ;
#69609 = DIRECTION ( 'NONE',  ( -1.047444401652940007E-14, -1.000000000000000000, -1.836970198721029934E-16 ) ) ;
#69610 = DIRECTION ( 'NONE',  ( -1.000000000000000000, 1.813998472013049822E-14, -1.836970198720996654E-16 ) ) ;
#69611 = ORIENTED_EDGE ( 'NONE', *, *, #46240, .F. ) ;
#69612 = EDGE_LOOP ( 'NONE', ( #67136, #69745, #10505, #49452, #28403, #7283, #487, #61684, #30002, #25295, #53040, #9209, #6595, #40172 ) ) ;
#69613 = DIRECTION ( 'NONE',  ( -1.836970198721029934E-16, -1.836970198721010706E-16, 1.000000000000000000 ) ) ;
#69614 = VECTOR ( 'NONE', #65518, 999.9999999999998863 ) ;
#69615 = VECTOR ( 'NONE', #60510, 1000.000000000000000 ) ;
#69616 = VECTOR ( 'NONE', #32869, 1000.000000000000000 ) ;
#69617 = CARTESIAN_POINT ( 'NONE',  ( -8.227189898828699555, -1.634292677759815904, 54.00000000000000711 ) ) ;
#69618 = CARTESIAN_POINT ( 'NONE',  ( 39.00000000000000000, 0.000000000000000000, 5.000000000000000000 ) ) ;
#69619 = DIRECTION ( 'NONE',  ( 0.000000000000000000, 0.000000000000000000, 1.000000000000000000 ) ) ;
#69620 = AXIS2_PLACEMENT_3D ( 'NONE', #2783, #51587, #51224 ) ;
#69621 = CARTESIAN_POINT ( 'NONE',  ( 283.0000000000000568, -27.13000000000000611, 13.50000000000000000 ) ) ;
#69622 = ORIENTED_EDGE ( 'NONE', *, *, #37311, .T. ) ;
#69623 = FACE_OUTER_BOUND ( 'NONE', #9997, .T. ) ;
#69624 = CARTESIAN_POINT ( 'NONE',  ( -9.880476262117236175, 7.447976262117216528, 25.99999580000000421 ) ) ;
#69625 = CARTESIAN_POINT ( 'NONE',  ( 7.250000000000005329, 7.250000000000000888, -10.00000000000000000 ) ) ;
#69626 = EDGE_CURVE ( 'NONE', #40971, #11123, #888, .T. ) ;
#69628 = VERTEX_POINT ( 'NONE', #11206 ) ;
#69627 = DIRECTION ( 'NONE',  ( 0.000000000000000000, -0.9938079899998859545, -0.1111111111112941946 ) ) ;
#69629 =( BOUNDED_CURVE ( )  B_SPLINE_CURVE ( 3, ( #34013, #841, #43941, #18439 ),
 .UNSPECIFIED., .F., .F. ) 
 B_SPLINE_CURVE_WITH_KNOTS ( ( 4, 4 ),
 ( 0.7227342478134158865, 0.8956647938578649049 ),
 .UNSPECIFIED. ) 
 CURVE ( )  GEOMETRIC_REPRESENTATION_ITEM ( )  RATIONAL_B_SPLINE_CURVE ( ( 1.000000000000000000, 0.9975094710839674805, 0.9975094710839674805, 1.000000000000000000 ) ) 
 REPRESENTATION_ITEM ( '' )  );
#69630 = CIRCLE ( 'NONE', #39119, 1.000000000000000000 ) ;
#69631 = DIRECTION ( 'NONE',  ( 0.000000000000000000, 0.000000000000000000, 1.000000000000000000 ) ) ;
#69632 = DIRECTION ( 'NONE',  ( 0.000000000000000000, 0.000000000000000000, 1.000000000000000000 ) ) ;
#69633 = DIRECTION ( 'NONE',  ( 0.000000000000000000, 0.000000000000000000, 1.000000000000000000 ) ) ;
#69634 = EDGE_CURVE ( 'NONE', #51627, #19691, #11538, .T. ) ;
#69635 = DIRECTION ( 'NONE',  ( -0.000000000000000000, 3.673940397442059868E-16, -1.000000000000000000 ) ) ;
#69636 = ORIENTED_EDGE ( 'NONE', *, *, #58924, .T. ) ;
#69637 = CARTESIAN_POINT ( 'NONE',  ( -3.593516549646790015, -7.428221114745077180, 455.0000000000000568 ) ) ;
#69638 = ADVANCED_FACE ( 'NONE', ( #33472 ), #38100, .T. ) ;
#69639 = PLANE ( 'NONE',  #30573 ) ;
#69640 = ORIENTED_EDGE ( 'NONE', *, *, #58729, .T. ) ;
#69641 = DIRECTION ( 'NONE',  ( 1.000000000000000000, -1.356437060717834379E-15, -1.836970198721032646E-16 ) ) ;
#69642 = CARTESIAN_POINT ( 'NONE',  ( 15.00000000000000000, -21.00000000000000000, 0.000000000000000000 ) ) ;
#69643 = DIRECTION ( 'NONE',  ( -1.836970198721029934E-16, 1.836970198721036590E-16, -1.000000000000000000 ) ) ;
#69644 = EDGE_CURVE ( 'NONE', #6527, #24350, #59656, .T. ) ;
#69645 = CARTESIAN_POINT ( 'NONE',  ( 14.50000000000000000, -42.00000000000000000, 27.00000000000000000 ) ) ;
#69646 = LINE ( 'NONE', #47714, #42197 ) ;
#69647 = ORIENTED_EDGE ( 'NONE', *, *, #37315, .T. ) ;
#69648 = EDGE_LOOP ( 'NONE', ( #46128, #33196, #15422, #56421, #53877 ) ) ;
#69649 = FACE_OUTER_BOUND ( 'NONE', #61522, .T. ) ;
#69650 = VERTEX_POINT ( 'NONE', #49728 ) ;
#69651 = AXIS2_PLACEMENT_3D ( 'NONE', #9262, #68307, #51703 ) ;
#69652 = ORIENTED_EDGE ( 'NONE', *, *, #65248, .T. ) ;
#69653 = DIRECTION ( 'NONE',  ( -1.000000000000000000, 0.000000000000000000, 0.000000000000000000 ) ) ;
#69654 = VECTOR ( 'NONE', #41896, 1000.000000000000000 ) ;
#69655 = EDGE_CURVE ( 'NONE', #69570, #11380, #34140, .T. ) ;
#69656 = CARTESIAN_POINT ( 'NONE',  ( -7.250000000000000888, -8.249999999999998224, -19.50000000000000000 ) ) ;
#69657 = VECTOR ( 'NONE', #34625, 1000.000000000000000 ) ;
#69658 = VECTOR ( 'NONE', #29394, 1000.000000000000000 ) ;
#69659 = FACE_OUTER_BOUND ( 'NONE', #43201, .T. ) ;
#69660 = VERTEX_POINT ( 'NONE', #17895 ) ;
#69661 = ORIENTED_EDGE ( 'NONE', *, *, #875, .T. ) ;
#69662 = CARTESIAN_POINT ( 'NONE',  ( -5.779227145995327497, -6.358413763958949083, 54.00000000000000711 ) ) ;
#69663 = VERTEX_POINT ( 'NONE', #66341 ) ;
#69664 = VERTEX_POINT ( 'NONE', #60326 ) ;
#69665 = AXIS2_PLACEMENT_3D ( 'NONE', #43345, #64933, #53291 ) ;
#69666 = CIRCLE ( 'NONE', #47036, 0.1999999999999987899 ) ;
#69667 = CARTESIAN_POINT ( 'NONE',  ( 14.45366306705349402, -0.2717122460102546766, -23.33927276307431598 ) ) ;
#69668 = DIRECTION ( 'NONE',  ( 1.836970198721029934E-16, 1.836970198721010706E-16, -1.000000000000000000 ) ) ;
#69669 = DIRECTION ( 'NONE',  ( 0.000000000000000000, 1.000000000000000000, 0.000000000000000000 ) ) ;
#69670 =( GEOMETRIC_REPRESENTATION_CONTEXT ( 3 ) GLOBAL_UNCERTAINTY_ASSIGNED_CONTEXT ( ( #48628 ) ) GLOBAL_UNIT_ASSIGNED_CONTEXT ( ( #184, #64883, #12159 ) ) REPRESENTATION_CONTEXT ( 'NONE', 'WORKASPACE' ) );
#69671 = ORIENTED_EDGE ( 'NONE', *, *, #41435, .T. ) ;
#69672 = DIRECTION ( 'NONE',  ( 0.000000000000000000, 1.000000000000000000, 0.000000000000000000 ) ) ;
#69673 = VECTOR ( 'NONE', #5699, 1000.000000000000000 ) ;
#69675 = DIRECTION ( 'NONE',  ( -1.000000000000000000, 4.745709458399858621E-16, 1.836970198721030920E-16 ) ) ;
#69674 = CARTESIAN_POINT ( 'NONE',  ( 10.14575131106465378, -25.50000000000000355, 17.00000000000000000 ) ) ;
#69676 = ORIENTED_EDGE ( 'NONE', *, *, #40530, .F. ) ;
#69678 = ORIENTED_EDGE ( 'NONE', *, *, #29330, .F. ) ;
#69677 = CARTESIAN_POINT ( 'NONE',  ( -4.947141984184539432, -7.357023737882807168, 54.00000000000000711 ) ) ;
#69679 = EDGE_LOOP ( 'NONE', ( #49711, #44089, #18923, #14947 ) ) ;
#69680 = VECTOR ( 'NONE', #57495, 1000.000000000000000 ) ;
#69681 = LINE ( 'NONE', #48449, #37809 ) ;
#69682 = EDGE_CURVE ( 'NONE', #50155, #29684, #50568, .T. ) ;
#69683 = EDGE_CURVE ( 'NONE', #56927, #53423, #11882, .T. ) ;
#69684 = AXIS2_PLACEMENT_3D ( 'NONE', #69705, #21266, #48477 ) ;
#69685 = DIRECTION ( 'NONE',  ( -0.000000000000000000, 0.000000000000000000, 1.000000000000000000 ) ) ;
#69686 = ORIENTED_EDGE ( 'NONE', *, *, #50818, .T. ) ;
#69687 = ADVANCED_FACE ( 'NONE', ( #49400 ), #50072, .F. ) ;
#69688 = DIRECTION ( 'NONE',  ( -1.000000000000000000, 0.000000000000000000, -0.000000000000000000 ) ) ;
#69689 = DIRECTION ( 'NONE',  ( -0.4999999999989361843, 0.000000000000000000, 0.8660254037850529940 ) ) ;
#69690 = ORIENTED_EDGE ( 'NONE', *, *, #9894, .T. ) ;
#69691 = ORIENTED_EDGE ( 'NONE', *, *, #21859, .F. ) ;
#69692 = DIRECTION ( 'NONE',  ( 1.000000000000000000, -0.000000000000000000, 0.000000000000000000 ) ) ;
#69693 = CARTESIAN_POINT ( 'NONE',  ( 106.4257688009193998, 0.000000000000000000, 282.4830310981789125 ) ) ;
#69694 = CARTESIAN_POINT ( 'NONE',  ( 30.00000000000000000, -5.599999999999379696, 26.60000000000059828 ) ) ;
#69695 = ORIENTED_EDGE ( 'NONE', *, *, #37875, .F. ) ;
#69696 = DIRECTION ( 'NONE',  ( 0.000000000000000000, 0.000000000000000000, 1.000000000000000000 ) ) ;
#69697 = DIRECTION ( 'NONE',  ( -0.000000000000000000, 3.673940397442059868E-16, -1.000000000000000000 ) ) ;
#69698 = AXIS2_PLACEMENT_3D ( 'NONE', #62376, #35871, #62733 ) ;
#69700 = VERTEX_POINT ( 'NONE', #7273 ) ;
#69699 = CARTESIAN_POINT ( 'NONE',  ( 10.62249899919925866, -21.00000000000000000, 17.50000000000000000 ) ) ;
#69702 = EDGE_LOOP ( 'NONE', ( #24782, #10137, #14369, #13380 ) ) ;
#69701 = DIRECTION ( 'NONE',  ( 0.000000000000000000, 1.000000000000000000, 0.000000000000000000 ) ) ;
#69703 = DIRECTION ( 'NONE',  ( -1.000000000000000000, 0.000000000000000000, 0.000000000000000000 ) ) ;
#69704 = DIRECTION ( 'NONE',  ( 0.000000000000000000, -0.7071067811865475727, -0.7071067811865475727 ) ) ;
#69705 = CARTESIAN_POINT ( 'NONE',  ( 6.006483450353401921, 5.993516549646582092, 455.0000000000000568 ) ) ;
#69706 = DIRECTION ( 'NONE',  ( 0.000000000000000000, 0.000000000000000000, 1.000000000000000000 ) ) ;
#69707 = DIRECTION ( 'NONE',  ( -0.000000000000000000, -1.000000000000000000, 0.000000000000000000 ) ) ;
#69708 = AXIS2_PLACEMENT_3D ( 'NONE', #29650, #35290, #8429 ) ;
#69709 = CIRCLE ( 'NONE', #43698, 25.39999999999999858 ) ;
#69710 = CARTESIAN_POINT ( 'NONE',  ( 7.806483450353372433, 11.11351654964662039, 195.0000000000000284 ) ) ;
#69711 = ORIENTED_EDGE ( 'NONE', *, *, #541, .T. ) ;
#69712 = CARTESIAN_POINT ( 'NONE',  ( 25.50000000000000355, -17.50000000000000000, 22.50000000000000000 ) ) ;
#69714 = ORIENTED_EDGE ( 'NONE', *, *, #65102, .T. ) ;
#69713 = DIRECTION ( 'NONE',  ( 0.7071067811865475727, -0.7071067811865475727, -2.597868168706480597E-16 ) ) ;
#69715 = AXIS2_PLACEMENT_3D ( 'NONE', #20315, #41880, #27022 ) ;
#69716 = ADVANCED_FACE ( 'NONE', ( #22857 ), #967, .F. ) ;
#69717 = CARTESIAN_POINT ( 'NONE',  ( 283.0000000000000568, -38.64999999999999858, -12.69999999999999929 ) ) ;
#69718 = CARTESIAN_POINT ( 'NONE',  ( 16.75000000000000000, -2.500000000000000000, -23.22168783648699986 ) ) ;
#69719 = DIRECTION ( 'NONE',  ( -1.000000000000000000, 1.047444401652940007E-14, -1.836970198721010706E-16 ) ) ;
#69720 = CIRCLE ( 'NONE', #20034, 24.99999999998784972 ) ;
#69721 = ORIENTED_EDGE ( 'NONE', *, *, #861, .F. ) ;
#69722 = DIRECTION ( 'NONE',  ( 1.000000000000000000, -0.000000000000000000, -0.000000000000000000 ) ) ;
#69723 = EDGE_CURVE ( 'NONE', #14509, #12, #16867, .T. ) ;
#69724 = DIRECTION ( 'NONE',  ( -0.000000000000000000, -0.000000000000000000, -1.000000000000000000 ) ) ;
#69725 = EDGE_CURVE ( 'NONE', #43188, #34214, #38439, .T. ) ;
#69726 = ORIENTED_EDGE ( 'NONE', *, *, #39753, .T. ) ;
#69727 = DIRECTION ( 'NONE',  ( 1.000000000000000000, -0.000000000000000000, -0.000000000000000000 ) ) ;
#69728 = FACE_OUTER_BOUND ( 'NONE', #61185, .T. ) ;
#69729 = EDGE_CURVE ( 'NONE', #7638, #6527, #54353, .T. ) ;
#69730 = EDGE_CURVE ( 'NONE', #33533, #49649, #37015, .T. ) ;
#69731 = AXIS2_PLACEMENT_3D ( 'NONE', #48038, #37436, #58996 ) ;
#69732 = EDGE_CURVE ( 'NONE', #66744, #54664, #53967, .T. ) ;
#69733 = EDGE_LOOP ( 'NONE', ( #31108, #13949, #10431, #41664 ) ) ;
#69734 = CARTESIAN_POINT ( 'NONE',  ( 10.31452373788277832, 3.842976262117149044, 26.00000000000000711 ) ) ;
#69735 = EDGE_LOOP ( 'NONE', ( #67123, #35962, #17672, #54053 ) ) ;
#69736 = ORIENTED_EDGE ( 'NONE', *, *, #18235, .F. ) ;
#69737 = DIRECTION ( 'NONE',  ( 0.000000000000000000, 0.000000000000000000, 1.000000000000000000 ) ) ;
#69738 = DIRECTION ( 'NONE',  ( 0.000000000000000000, -0.8206518066484758123, -0.5714285714283042772 ) ) ;
#69739 = CARTESIAN_POINT ( 'NONE',  ( 30.00000000000000000, -5.000000000000000000, 27.00000000000000000 ) ) ;
#69740 = CARTESIAN_POINT ( 'NONE',  ( 41.09999999999999432, -21.00000000000000000, 13.86939075806900057 ) ) ;
#69741 = VERTEX_POINT ( 'NONE', #49044 ) ;
#69742 = ORIENTED_EDGE ( 'NONE', *, *, #40522, .F. ) ;
#69744 = ORIENTED_EDGE ( 'NONE', *, *, #10437, .T. ) ;
#69743 = DIRECTION ( 'NONE',  ( 1.000000000000000000, 0.000000000000000000, 0.000000000000000000 ) ) ;
#69745 = ORIENTED_EDGE ( 'NONE', *, *, #62743, .F. ) ;
#69746 = CARTESIAN_POINT ( 'NONE',  ( -4.727349090213559535, -7.811466277050794993, 455.0000000000000568 ) ) ;
#69747 = DIRECTION ( 'NONE',  ( 1.000000000000000000, -0.000000000000000000, -0.000000000000000000 ) ) ;
#69748 = DIRECTION ( 'NONE',  ( -1.920292680692490463E-14, -1.000000000000000000, -1.836970198721045958E-16 ) ) ;
#69749 = VECTOR ( 'NONE', #15709, 1000.000000000000000 ) ;
#69750 = DIRECTION ( 'NONE',  ( -1.000000000000000000, 3.491481338843133355E-15, 1.836970198721036344E-16 ) ) ;
#69752 = DIRECTION ( 'NONE',  ( 0.000000000000000000, -1.000000000000000000, 0.000000000000000000 ) ) ;
#69751 = PLANE ( 'NONE',  #19637 ) ;
#69753 = ORIENTED_EDGE ( 'NONE', *, *, #50614, .T. ) ;
#69755 = EDGE_LOOP ( 'NONE', ( #13713, #50501, #11637, #64435 ) ) ;
#69754 = LINE ( 'NONE', #4092, #5897 ) ;
#69756 = VERTEX_POINT ( 'NONE', #5910 ) ;
#69757 = ORIENTED_EDGE ( 'NONE', *, *, #23521, .T. ) ;
#69758 = CIRCLE ( 'NONE', #17793, 2.204799999999997873 ) ;
#69759 = AXIS2_PLACEMENT_3D ( 'NONE', #47598, #31361, #42286 ) ;
#69760 = DIRECTION ( 'NONE',  ( -1.000000000000000000, 0.000000000000000000, 0.000000000000000000 ) ) ;
#69761 = DIRECTION ( 'NONE',  ( 1.836970198721029934E-16, 1.836970198721010706E-16, -1.000000000000000000 ) ) ;
#69762 = AXIS2_PLACEMENT_3D ( 'NONE', #68685, #4344, #20230 ) ;
#69763 = AXIS2_PLACEMENT_3D ( 'NONE', #31606, #4031, #20278 ) ;
#69764 = LINE ( 'NONE', #4375, #67019 ) ;
#69765 = EDGE_LOOP ( 'NONE', ( #42198, #42873, #43444, #17182 ) ) ;
#69766 = ORIENTED_EDGE ( 'NONE', *, *, #25215, .T. ) ;
#69767 = EDGE_LOOP ( 'NONE', ( #41625, #14817, #15230, #25224 ) ) ;
#69768 = EDGE_CURVE ( 'NONE', #30390, #55486, #22176, .T. ) ;
#69769 = EDGE_CURVE ( 'NONE', #49703, #2734, #12149, .T. ) ;
#69770 = CARTESIAN_POINT ( 'NONE',  ( 7.250000000000004441, 8.750000000000001776, -26.00000000000001066 ) ) ;
#69771 = AXIS2_PLACEMENT_3D ( 'NONE', #10051, #52853, #31623 ) ;
#69772 = VECTOR ( 'NONE', #9831, 1000.000000000000000 ) ;
#69773 = VERTEX_POINT ( 'NONE', #6250 ) ;
#69774 = DIRECTION ( 'NONE',  ( -1.000000000000000000, 0.000000000000000000, 0.000000000000000000 ) ) ;
#69775 = DIRECTION ( 'NONE',  ( -0.000000000000000000, 3.673940397442059868E-16, -1.000000000000000000 ) ) ;
#69776 = ADVANCED_FACE ( 'NONE', ( #44072 ), #55389, .F. ) ;
#69777 = EDGE_LOOP ( 'NONE', ( #62622, #8809, #35739, #51250 ) ) ;
#69778 = EDGE_LOOP ( 'NONE', ( #36844, #52539, #23123, #19449 ) ) ;
#69779 = DIRECTION ( 'NONE',  ( -1.000000000000000000, 0.000000000000000000, 0.000000000000000000 ) ) ;
#69780 =( REPRESENTATION_RELATIONSHIP ('NONE','NONE', #33057, #60228 ) REPRESENTATION_RELATIONSHIP_WITH_TRANSFORMATION ( #31417 )SHAPE_REPRESENTATION_RELATIONSHIP( ) );
#69781 = CARTESIAN_POINT ( 'NONE',  ( -7.450000000000001954, 0.000000000000000000, -19.00000000000000000 ) ) ;
#69782 = VERTEX_POINT ( 'NONE', #24607 ) ;
#69783 = AXIS2_PLACEMENT_3D ( 'NONE', #50107, #51513, #28879 ) ;
#69784 = DIRECTION ( 'NONE',  ( 0.000000000000000000, 0.000000000000000000, 1.000000000000000000 ) ) ;
#69786 = ORIENTED_EDGE ( 'NONE', *, *, #48956, .F. ) ;
#69785 = DIRECTION ( 'NONE',  ( 0.000000000000000000, 1.000000000000000000, 0.000000000000000000 ) ) ;
#69787 = EDGE_LOOP ( 'NONE', ( #53070, #65822, #23776, #20224 ) ) ;
#69788 = CARTESIAN_POINT ( 'NONE',  ( 8.250000000000005329, 7.250000000000000888, -18.50000000000000000 ) ) ;
#69789 = CARTESIAN_POINT ( 'NONE',  ( 1.090483450353372907, 11.33351654964664590, 195.0000000000000284 ) ) ;
#69790 = CARTESIAN_POINT ( 'NONE',  ( 7.000000000000000000, -25.60000000000000142, -15.10000000000000142 ) ) ;
#69791 = DIRECTION ( 'NONE',  ( -1.836970198721029934E-16, 1.836970198721036344E-16, -1.000000000000000000 ) ) ;
#69792 = CARTESIAN_POINT ( 'NONE',  ( -1.620245201994368722, -8.241237374594323484, 26.00000000000000711 ) ) ;
#69793 = EDGE_LOOP ( 'NONE', ( #2994, #14067, #27300, #38781 ) ) ;
#69794 = DIRECTION ( 'NONE',  ( -0.7071067811865398012, 0.7071067811865552333, 2.597868168706484541E-16 ) ) ;
#69795 = ORIENTED_EDGE ( 'NONE', *, *, #65542, .T. ) ;
#69796 = DIRECTION ( 'NONE',  ( 0.000000000000000000, -1.000000000000000000, 0.000000000000000000 ) ) ;
#69797 = DIRECTION ( 'NONE',  ( 0.000000000000000000, 0.000000000000000000, 1.000000000000000000 ) ) ;
#69798 = DIRECTION ( 'NONE',  ( -0.000000000000000000, -1.000000000000000000, -0.000000000000000000 ) ) ;
#69799 = CARTESIAN_POINT ( 'NONE',  ( 4.206483450353421638, 11.11351654964658486, 455.0000000000000568 ) ) ;
#69800 = DIRECTION ( 'NONE',  ( 1.000000000000000000, -0.000000000000000000, 0.000000000000000000 ) ) ;
#69801 = ORIENTED_EDGE ( 'NONE', *, *, #25759, .T. ) ;
#69802 = LINE ( 'NONE', #25626, #52851 ) ;
#69803 = EDGE_CURVE ( 'NONE', #5400, #25235, #35911, .T. ) ;
#69804 = SURFACE_STYLE_USAGE ( .BOTH. , #16400 ) ;
#69805 = VECTOR ( 'NONE', #21891, 1000.000000000000000 ) ;
#69806 = EDGE_CURVE ( 'NONE', #44389, #803, #12920, .T. ) ;
#69807 = ORIENTED_EDGE ( 'NONE', *, *, #69132, .F. ) ;
#69808 = CARTESIAN_POINT ( 'NONE',  ( 7.000000000000000000, -23.50007830495750127, 12.28007262201345995 ) ) ;
#69809 = DIRECTION ( 'NONE',  ( -1.000000000000000000, 0.000000000000000000, 0.000000000000000000 ) ) ;
#69810 = ADVANCED_FACE ( 'NONE', ( #51823 ), #35187, .F. ) ;
#69811 = ORIENTED_EDGE ( 'NONE', *, *, #13824, .T. ) ;
#69812 = AXIS2_PLACEMENT_3D ( 'NONE', #29283, #67836, #19386 ) ;
#69813 = DIRECTION ( 'NONE',  ( 0.000000000000000000, -1.000000000000000000, 0.000000000000000000 ) ) ;
#69814 = AXIS2_PLACEMENT_3D ( 'NONE', #10436, #69482, #20345 ) ;
#69815 = CARTESIAN_POINT ( 'NONE',  ( 7.750000000000001776, 7.750000000000000000, 5.000000000000000000 ) ) ;
#69816 = ORIENTED_EDGE ( 'NONE', *, *, #64350, .F. ) ;
#69817 = LINE ( 'NONE', #54598, #63842 ) ;
#69818 = CARTESIAN_POINT ( 'NONE',  ( 19.90000000000000213, 20.60000000000000142, 13.86939075806899702 ) ) ;
#69819 = LINE ( 'NONE', #17102, #3532 ) ;
#69820 = EDGE_LOOP ( 'NONE', ( #17474, #20439, #13389, #20169 ) ) ;
#69822 = ORIENTED_EDGE ( 'NONE', *, *, #38573, .F. ) ;
#69821 = FACE_OUTER_BOUND ( 'NONE', #26163, .T. ) ;
#69823 = ADVANCED_FACE ( 'NONE', ( #14351 ), #2332, .T. ) ;
#69824 = CIRCLE ( 'NONE', #23514, 8.000000000000000000 ) ;
#69825 = DIRECTION ( 'NONE',  ( 0.000000000000000000, 0.000000000000000000, 1.000000000000000000 ) ) ;
#69826 = CYLINDRICAL_SURFACE ( 'NONE', #17691, 0.3999999999993835154 ) ;
#69827 = CARTESIAN_POINT ( 'NONE',  ( -29.25000000000000000, -5.200000000000001066, -26.25000000000000000 ) ) ;
#69828 = EDGE_LOOP ( 'NONE', ( #18086, #58465, #8780, #62081 ) ) ;
#69829 = DIRECTION ( 'NONE',  ( 0.000000000000000000, 1.000000000000000000, 0.000000000000000000 ) ) ;
#69830 = ORIENTED_EDGE ( 'NONE', *, *, #34942, .T. ) ;
#69831 = ORIENTED_EDGE ( 'NONE', *, *, #26676, .T. ) ;
#69832 = VERTEX_POINT ( 'NONE', #51115 ) ;
#69833 = CARTESIAN_POINT ( 'NONE',  ( 275.0000000000000000, -31.30000000000095284, -12.19999999999906315 ) ) ;
#69834 = CARTESIAN_POINT ( 'NONE',  ( -9.828310488886039309, -1.690483450353358119, 455.0000000000000568 ) ) ;
#69835 = CARTESIAN_POINT ( 'NONE',  ( 7.250000000000005329, -8.249999999999998224, -12.00000000000000000 ) ) ;
#69836 = ORIENTED_EDGE ( 'NONE', *, *, #14716, .T. ) ;
#69837 = ORIENTED_EDGE ( 'NONE', *, *, #11347, .T. ) ;
#69838 = CARTESIAN_POINT ( 'NONE',  ( 19.90000000000000213, -0.2000000000089119934, 8.909539772616881237E-12 ) ) ;
#69839 = ORIENTED_EDGE ( 'NONE', *, *, #25580, .F. ) ;
#69840 = ORIENTED_EDGE ( 'NONE', *, *, #46233, .F. ) ;
#69841 = ADVANCED_FACE ( 'NONE', ( #40145 ), #57120, .T. ) ;
#69842 = VERTEX_POINT ( 'NONE', #7970 ) ;
#69843 = ORIENTED_EDGE ( 'NONE', *, *, #62348, .F. ) ;
#69844 = CYLINDRICAL_SURFACE ( 'NONE', #45121, 4.000000000000000000 ) ;
#69845 = UNCERTAINTY_MEASURE_WITH_UNIT (LENGTH_MEASURE( 1.000000000000000082E-05 ), #9067, 'distance_accuracy_value', 'NONE');
#69847 = ORIENTED_EDGE ( 'NONE', *, *, #66924, .F. ) ;
#69846 = FACE_OUTER_BOUND ( 'NONE', #8547, .T. ) ;
#69848 = VECTOR ( 'NONE', #2740, 999.9999999999998863 ) ;
#69849 = LINE ( 'NONE', #15063, #63912 ) ;
#69850 = CARTESIAN_POINT ( 'NONE',  ( 3.724485858128677940, -7.408280051175165859, 54.00000000000000711 ) ) ;
#69851 = LINE ( 'NONE', #21067, #52767 ) ;
#69852 = ORIENTED_EDGE ( 'NONE', *, *, #23611, .T. ) ;
#69853 = CIRCLE ( 'NONE', #41630, 1.000000000000003553 ) ;
#69854 = EDGE_CURVE ( 'NONE', #8876, #13060, #13308, .T. ) ;
#69855 = CYLINDRICAL_SURFACE ( 'NONE', #48108, 0.3499999999999996447 ) ;
#69856 = EDGE_CURVE ( 'NONE', #54625, #40050, #60750, .T. ) ;
#69857 = CARTESIAN_POINT ( 'NONE',  ( 4.206483450353421638, 11.11351654964658486, 455.0000000000000568 ) ) ;
#69858 = VERTEX_POINT ( 'NONE', #62409 ) ;
#69859 = CARTESIAN_POINT ( 'NONE',  ( -7.250000000000000888, 7.250000000000001776, -25.50000000000000355 ) ) ;
#69860 = VECTOR ( 'NONE', #42744, 1000.000000000000000 ) ;
#69861 = FACE_OUTER_BOUND ( 'NONE', #18616, .T. ) ;
#69862 = CARTESIAN_POINT ( 'NONE',  ( -7.250000000000000888, 7.450000000000003730, -18.50000000000000000 ) ) ;
#69863 = ORIENTED_EDGE ( 'NONE', *, *, #45997, .F. ) ;
#69864 = DIRECTION ( 'NONE',  ( -0.000000000000000000, -0.000000000000000000, -1.000000000000000000 ) ) ;
#69865 = FACE_OUTER_BOUND ( 'NONE', #61008, .T. ) ;
#69866 = CYLINDRICAL_SURFACE ( 'NONE', #5478, 0.1999999999999996503 ) ;
#69867 = LINE ( 'NONE', #38060, #32025 ) ;
#69868 = CARTESIAN_POINT ( 'NONE',  ( -5.993516549646711766, 5.993516549646603409, 455.0000000000000568 ) ) ;
#69869 = LINE ( 'NONE', #68485, #11341 ) ;
#69870 = CARTESIAN_POINT ( 'NONE',  ( 15.89999999999999680, 13.66939075806899240, -20.79999999999999361 ) ) ;
#69871 = CARTESIAN_POINT ( 'NONE',  ( 15.50000000000000000, -5.000000000000000000, 18.50000000000000000 ) ) ;
#69872 = ADVANCED_FACE ( 'NONE', ( #45451, #13634 ), #50427, .F. ) ;
#69873 = EDGE_CURVE ( 'NONE', #18995, #24515, #67534, .T. ) ;
#69874 = ORIENTED_EDGE ( 'NONE', *, *, #26038, .T. ) ;
#69875 = DIRECTION ( 'NONE',  ( -0.6414496315691617934, 0.7671651518152962090, 0.000000000000000000 ) ) ;
#69876 = EDGE_CURVE ( 'NONE', #44054, #3700, #33499, .T. ) ;
#69877 = DIRECTION ( 'NONE',  ( -0.000000000000000000, 3.673940397442059868E-16, -1.000000000000000000 ) ) ;
#69878 = LINE ( 'NONE', #37030, #60606 ) ;
#69879 = DIRECTION ( 'NONE',  ( 1.000000000000000000, -0.000000000000000000, -0.000000000000000000 ) ) ;
#69880 = ORIENTED_EDGE ( 'NONE', *, *, #63197, .F. ) ;
#69881 = LINE ( 'NONE', #21446, #46771 ) ;
#69882 = LINE ( 'NONE', #15795, #63282 ) ;
#69883 = EDGE_CURVE ( 'NONE', #67695, #6090, #46506, .T. ) ;
#69884 = CARTESIAN_POINT ( 'NONE',  ( 7.250000000000005329, -7.249999999999998224, -25.00000000000000000 ) ) ;
#69885 = ADVANCED_FACE ( 'NONE', ( #68081 ), #19633, .T. ) ;
#69886 = AXIS2_PLACEMENT_3D ( 'NONE', #9030, #41562, #4788 ) ;
#69887 = CARTESIAN_POINT ( 'NONE',  ( -4.947141984184539432, -7.357023737882807168, 54.00000000000000711 ) ) ;
#69888 = CARTESIAN_POINT ( 'NONE',  ( 9.795823737882798810, 9.781776262117176657, 26.00000000000000711 ) ) ;
#69889 = ADVANCED_FACE ( 'NONE', ( #61362 ), #31411, .F. ) ;
#69890 = CARTESIAN_POINT ( 'NONE',  ( -7.250000000000000888, 7.250000000000001776, -26.00000000000001066 ) ) ;
#69891 = ORIENTED_EDGE ( 'NONE', *, *, #33623, .T. ) ;
#69892 = EDGE_CURVE ( 'NONE', #29989, #62095, #37061, .T. ) ;
#69893 = EDGE_LOOP ( 'NONE', ( #26577, #16859, #12970, #14803 ) ) ;
#69894 = DIRECTION ( 'NONE',  ( 0.000000000000000000, 0.000000000000000000, 1.000000000000000000 ) ) ;
#69895 = CARTESIAN_POINT ( 'NONE',  ( -5.779227145995327497, -6.358413763958949083, 54.00000000000000711 ) ) ;
#69896 = VERTEX_POINT ( 'NONE', #56420 ) ;
#69897 = DIRECTION ( 'NONE',  ( -0.7071067811865401342, 0.7071067811865550112, 1.355854680848613865E-30 ) ) ;
#69898 = VECTOR ( 'NONE', #26300, 1000.000000000000000 ) ;
#69899 = DIRECTION ( 'NONE',  ( 0.000000000000000000, 1.000000000000000000, 0.000000000000000000 ) ) ;
#69900 = ORIENTED_EDGE ( 'NONE', *, *, #39946, .F. ) ;
#69901 = VECTOR ( 'NONE', #23694, 1000.000000000000000 ) ;
#69902 = DIRECTION ( 'NONE',  ( 0.000000000000000000, 0.000000000000000000, -1.000000000000000000 ) ) ;
#69903 = VERTEX_POINT ( 'NONE', #2675 ) ;
#69904 = VERTEX_POINT ( 'NONE', #24248 ) ;
#69905 = CARTESIAN_POINT ( 'NONE',  ( 29.50000000000000355, -11.50000000000000000, -11.00000000000000000 ) ) ;
#69906 = ORIENTED_EDGE ( 'NONE', *, *, #16797, .T. ) ;
#69907 = DIRECTION ( 'NONE',  ( -1.000000000000000000, 0.000000000000000000, 0.000000000000000000 ) ) ;
#69909 = CIRCLE ( 'NONE', #14589, 2.250000000000001776 ) ;
#69908 = AXIS2_PLACEMENT_3D ( 'NONE', #60037, #38152, #55438 ) ;
#69910 = DIRECTION ( 'NONE',  ( 1.836970198721029934E-16, 1.836970198721010706E-16, -1.000000000000000000 ) ) ;
#69911 = DIRECTION ( 'NONE',  ( 0.000000000000000000, 0.000000000000000000, 1.000000000000000000 ) ) ;
#69912 = EDGE_CURVE ( 'NONE', #64822, #22889, #45809, .T. ) ;
#69913 = ORIENTED_EDGE ( 'NONE', *, *, #64373, .F. ) ;
#69914 = ORIENTED_EDGE ( 'NONE', *, *, #41654, .T. ) ;
#69915 = LINE ( 'NONE', #48356, #10957 ) ;
#69918 = DIRECTION ( 'NONE',  ( -0.000000000000000000, -1.000000000000000000, -0.000000000000000000 ) ) ;
#69917 = DIRECTION ( 'NONE',  ( -1.000000000000000000, 0.000000000000000000, 0.000000000000000000 ) ) ;
#69916 = VECTOR ( 'NONE', #57336, 1000.000000000000000 ) ;
#69919 = ORIENTED_EDGE ( 'NONE', *, *, #5312, .F. ) ;
#69920 = VERTEX_POINT ( 'NONE', #69835 ) ;
#69921 = EDGE_CURVE ( 'NONE', #10806, #31022, #57819, .T. ) ;
#69922 = ORIENTED_EDGE ( 'NONE', *, *, #46255, .F. ) ;
#69923 = CARTESIAN_POINT ( 'NONE',  ( -8.250000000000001776, -7.249999999999998224, -26.00000000000001066 ) ) ;
#69925 = ORIENTED_EDGE ( 'NONE', *, *, #38901, .T. ) ;
#69924 = FACE_OUTER_BOUND ( 'NONE', #27361, .T. ) ;
#69926 = ADVANCED_FACE ( 'NONE', ( #31330 ), #9031, .F. ) ;
#69927 = DIRECTION ( 'NONE',  ( 1.000000000000000000, -0.000000000000000000, -0.000000000000000000 ) ) ;
#69928 = DIRECTION ( 'NONE',  ( -1.000000000000000000, 0.000000000000000000, 0.000000000000000000 ) ) ;
#69929 = ORIENTED_EDGE ( 'NONE', *, *, #47823, .T. ) ;
#69930 = ORIENTED_EDGE ( 'NONE', *, *, #1300, .F. ) ;
#69931 = DIRECTION ( 'NONE',  ( 0.000000000000000000, 1.000000000000000000, 0.000000000000000000 ) ) ;
#69932 = VERTEX_POINT ( 'NONE', #47568 ) ;
#69933 = AXIS2_PLACEMENT_3D ( 'NONE', #53813, #17342, #5383 ) ;
#69934 = DIRECTION ( 'NONE',  ( -4.956352788505168198E-15, -1.000000000000000000, 0.000000000000000000 ) ) ;
#69935 = CARTESIAN_POINT ( 'NONE',  ( -7.250000000000000888, 7.450000000000003730, -17.00000000000000000 ) ) ;
#69936 = EDGE_CURVE ( 'NONE', #48542, #46263, #28014, .T. ) ;
#69937 = ORIENTED_EDGE ( 'NONE', *, *, #65444, .T. ) ;
#69938 = AXIS2_PLACEMENT_3D ( 'NONE', #17881, #10844, #60672 ) ;
#69939 = VECTOR ( 'NONE', #10258, 1000.000000000000000 ) ;
#69940 = DIRECTION ( 'NONE',  ( -1.000000000000000000, 0.000000000000000000, 0.000000000000000000 ) ) ;
#69941 = DIRECTION ( 'NONE',  ( 1.000000000000000000, -8.802523127157697409E-15, 1.836970198721013664E-16 ) ) ;
#69942 = EDGE_CURVE ( 'NONE', #8802, #4926, #53581, .T. ) ;
#69944 = ORIENTED_EDGE ( 'NONE', *, *, #49777, .T. ) ;
#69943 = CARTESIAN_POINT ( 'NONE',  ( 7.250000000000005329, 8.250000000000001776, -21.50000000000000000 ) ) ;
#69945 = ORIENTED_EDGE ( 'NONE', *, *, #17736, .F. ) ;
#69946 = ADVANCED_FACE ( 'NONE', ( #15043 ), #21395, .F. ) ;
#69947 = CARTESIAN_POINT ( 'NONE',  ( -7.259684009080030975, -7.811466277050769236, 455.0000000000000568 ) ) ;
#69948 = AXIS2_PLACEMENT_3D ( 'NONE', #48485, #51, #49518 ) ;
#69949 = LINE ( 'NONE', #4909, #43182 ) ;
#69950 = EDGE_CURVE ( 'NONE', #37762, #53071, #25671, .T. ) ;
#69951 = CARTESIAN_POINT ( 'NONE',  ( 7.250000000000005329, -7.249999999999998224, -15.50000000000000000 ) ) ;
#69952 = EDGE_CURVE ( 'NONE', #4860, #66079, #68439, .T. ) ;
#69953 = ADVANCED_FACE ( 'NONE', ( #41563 ), #58542, .T. ) ;
#69954 = DIRECTION ( 'NONE',  ( -4.336808689942006692E-15, -1.000000000000000000, 0.000000000000000000 ) ) ;
#69955 = CIRCLE ( 'NONE', #49610, 3.500000000000000000 ) ;
#69956 = DIRECTION ( 'NONE',  ( -1.000000000000000000, 0.000000000000000000, 0.000000000000000000 ) ) ;
#69957 = ORIENTED_EDGE ( 'NONE', *, *, #41119, .F. ) ;
#69958 = CARTESIAN_POINT ( 'NONE',  ( 283.0000000000000568, -28.94999999999999929, 13.50000000000000000 ) ) ;
#69959 = DIRECTION ( 'NONE',  ( -1.000000000000000000, 0.000000000000000000, 0.000000000000000000 ) ) ;
#69960 = EDGE_CURVE ( 'NONE', #6538, #992, #52898, .T. ) ;
#69961 = CARTESIAN_POINT ( 'NONE',  ( -3.663616288757055806, 4.135079735113128763, 26.00000000000000711 ) ) ;
#69962 = AXIS2_PLACEMENT_3D ( 'NONE', #22141, #60656, #43707 ) ;
#69964 = ORIENTED_EDGE ( 'NONE', *, *, #22420, .T. ) ;
#69963 = PLANE ( 'NONE',  #67212 ) ;
#69965 = CARTESIAN_POINT ( 'NONE',  ( -9.722976262117246193, -3.682023737882722081, 26.00000000000000000 ) ) ;
#69966 = ADVANCED_FACE ( 'NONE', ( #47911 ), #52530, .F. ) ;
#69967 = LINE ( 'NONE', #13511, #26972 ) ;
#69968 = DIRECTION ( 'NONE',  ( 9.912705577010386883E-15, 1.000000000000000000, 0.000000000000000000 ) ) ;
#69969 = ADVANCED_FACE ( 'NONE', ( #4095 ), #47228, .T. ) ;
#69970 = AXIS2_PLACEMENT_3D ( 'NONE', #47305, #57212, #46247 ) ;
#69971 = DIRECTION ( 'NONE',  ( -1.000000000000000000, 0.000000000000000000, 0.000000000000000000 ) ) ;
#69972 = EDGE_LOOP ( 'NONE', ( #66699, #15520 ) ) ;
#69973 = CARTESIAN_POINT ( 'NONE',  ( 11.50000000000000000, -11.50000000000000000, -15.00000000000000000 ) ) ;
#69974 = CYLINDRICAL_SURFACE ( 'NONE', #68891, 0.1749999999999998224 ) ;
#69975 = ORIENTED_EDGE ( 'NONE', *, *, #12286, .F. ) ;
#69976 = LINE ( 'NONE', #5288, #35625 ) ;
#69977 = DIRECTION ( 'NONE',  ( 0.7071067811865475727, -0.7071067811865475727, -2.597868168706480104E-16 ) ) ;
#69978 = DIRECTION ( 'NONE',  ( 1.000000000000000000, 0.000000000000000000, 0.000000000000000000 ) ) ;
#69979 = ADVANCED_FACE ( 'NONE', ( #53242 ), #4789, .T. ) ;
#69980 = DIRECTION ( 'NONE',  ( 0.000000000000000000, 1.000000000000000000, 0.000000000000000000 ) ) ;
#69981 = NEXT_ASSEMBLY_USAGE_OCCURRENCE ( 'NAUO1', ' ', ' ', #61644, #63345, $ ) ;
#69982 = NEXT_ASSEMBLY_USAGE_OCCURRENCE ( 'NAUO2', ' ', ' ', #61644, #63345, $ ) ;
#69983 = NEXT_ASSEMBLY_USAGE_OCCURRENCE ( 'NAUO3', ' ', ' ', #61644, #9788, $ ) ;
#69984 = NEXT_ASSEMBLY_USAGE_OCCURRENCE ( 'NAUO4', ' ', ' ', #61644, #9788, $ ) ;
#69985 = NEXT_ASSEMBLY_USAGE_OCCURRENCE ( 'NAUO5', ' ', ' ', #61644, #30933, $ ) ;
#69986 = NEXT_ASSEMBLY_USAGE_OCCURRENCE ( 'NAUO6', ' ', ' ', #61644, #30933, $ ) ;
#69987 = NEXT_ASSEMBLY_USAGE_OCCURRENCE ( 'NAUO7', ' ', ' ', #61644, #28759, $ ) ;
#69988 = NEXT_ASSEMBLY_USAGE_OCCURRENCE ( 'NAUO8', ' ', ' ', #61644, #28759, $ ) ;
#69989 = NEXT_ASSEMBLY_USAGE_OCCURRENCE ( 'NAUO9', ' ', ' ', #61644, #18371, $ ) ;
#69990 = NEXT_ASSEMBLY_USAGE_OCCURRENCE ( 'NAUO10', ' ', ' ', #61644, #1166, $ ) ;
#69991 = NEXT_ASSEMBLY_USAGE_OCCURRENCE ( 'NAUO11', ' ', ' ', #61644, #38746, $ ) ;
#69992 = NEXT_ASSEMBLY_USAGE_OCCURRENCE ( 'NAUO12', ' ', ' ', #61644, #18876, $ ) ;
#69993 = NEXT_ASSEMBLY_USAGE_OCCURRENCE ( 'NAUO13', ' ', ' ', #18371, #29636, $ ) ;
#69994 = NEXT_ASSEMBLY_USAGE_OCCURRENCE ( 'NAUO14', ' ', ' ', #18371, #34822, $ ) ;
#69995 = NEXT_ASSEMBLY_USAGE_OCCURRENCE ( 'NAUO15', ' ', ' ', #18371, #20553, $ ) ;
#69996 = NEXT_ASSEMBLY_USAGE_OCCURRENCE ( 'NAUO16', ' ', ' ', #18371, #17120, $ ) ;
#69997 = NEXT_ASSEMBLY_USAGE_OCCURRENCE ( 'NAUO17', ' ', ' ', #18371, #52984, $ ) ;
#69998 = NEXT_ASSEMBLY_USAGE_OCCURRENCE ( 'NAUO18', ' ', ' ', #18371, #11064, $ ) ;
#69999 = NEXT_ASSEMBLY_USAGE_OCCURRENCE ( 'NAUO19', ' ', ' ', #18371, #29636, $ ) ;
ENDSEC;
END-ISO-10303-21;
